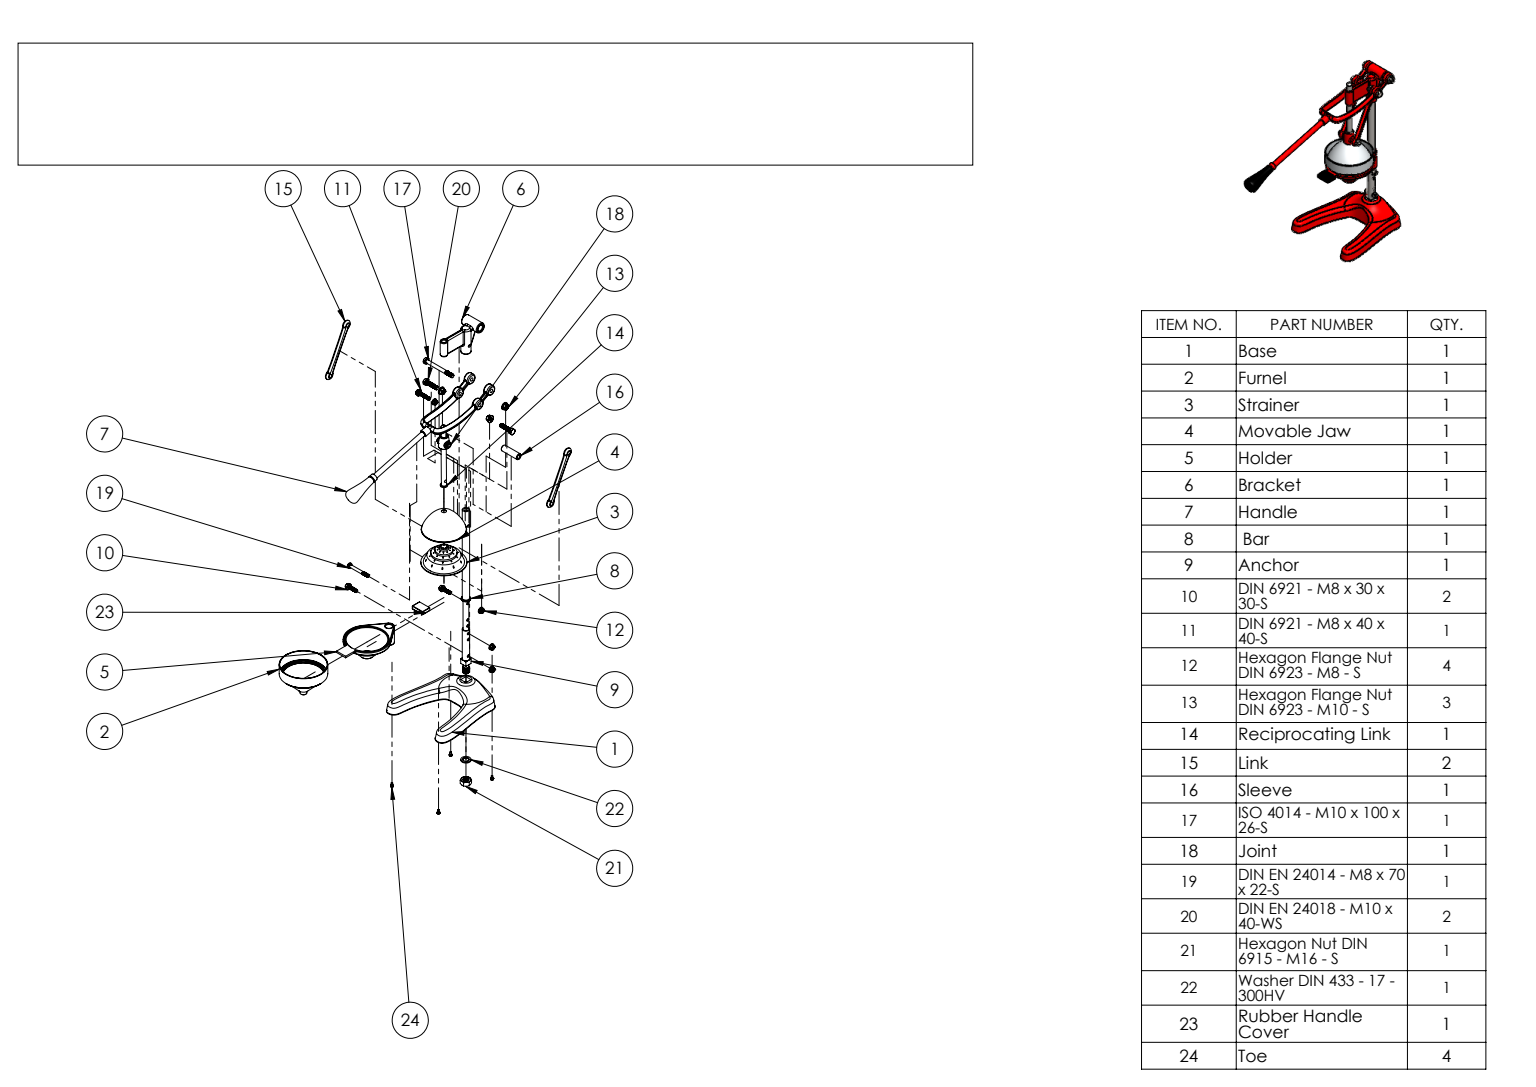
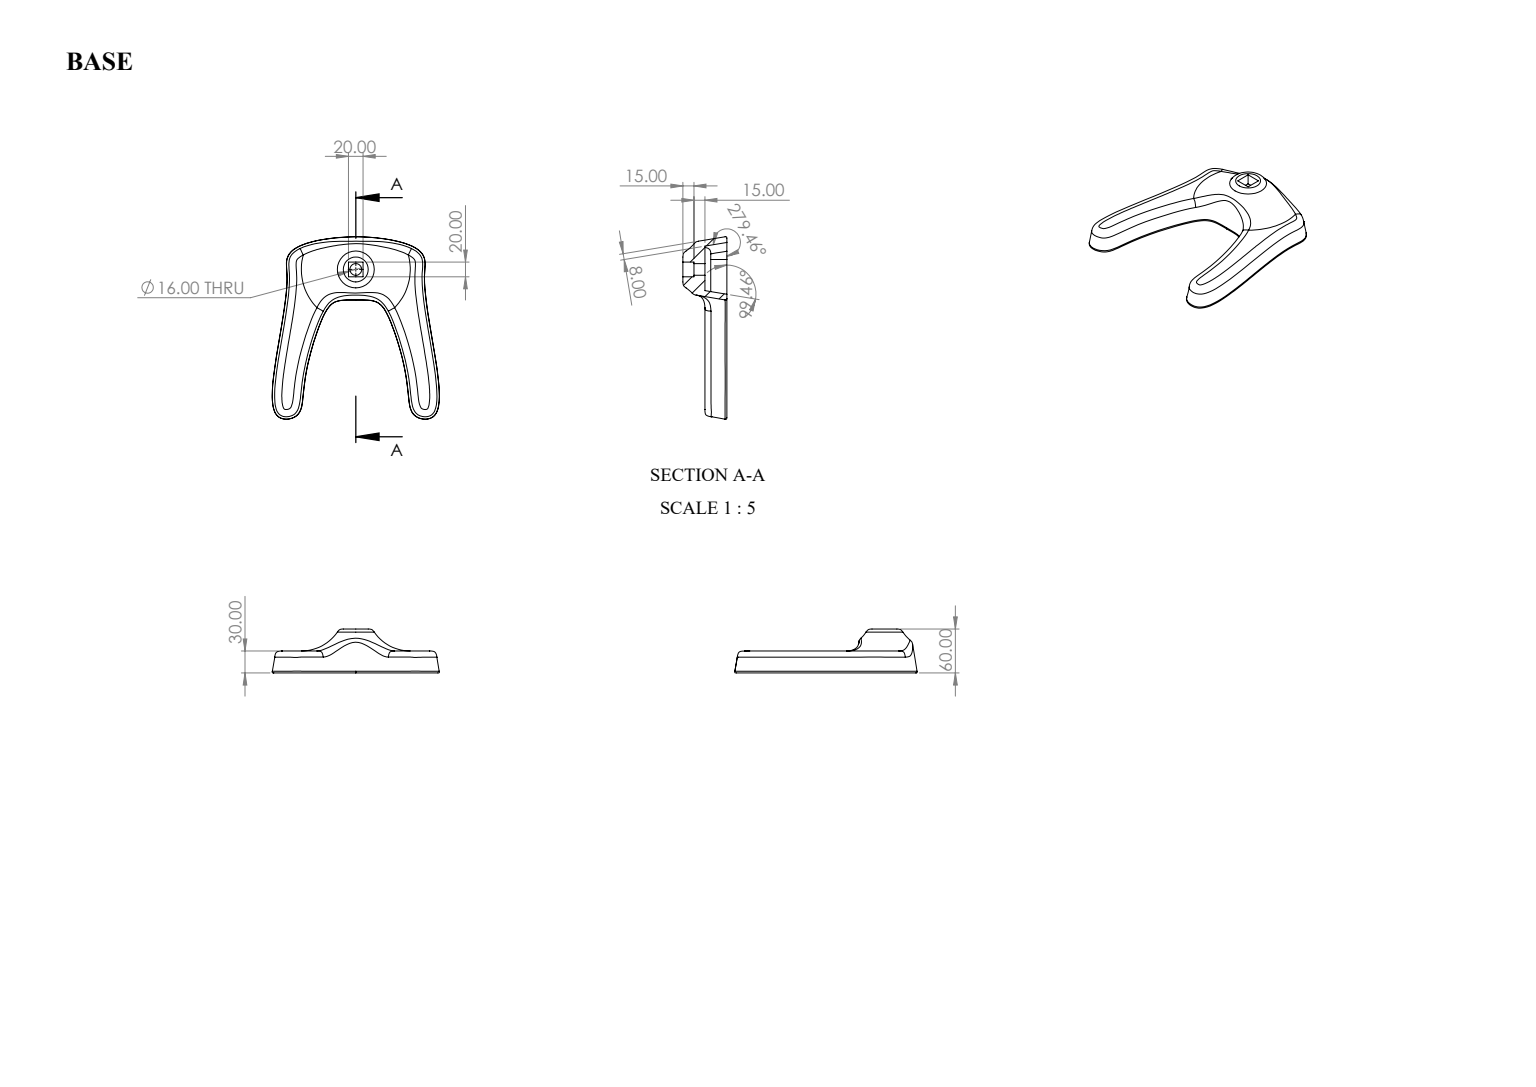
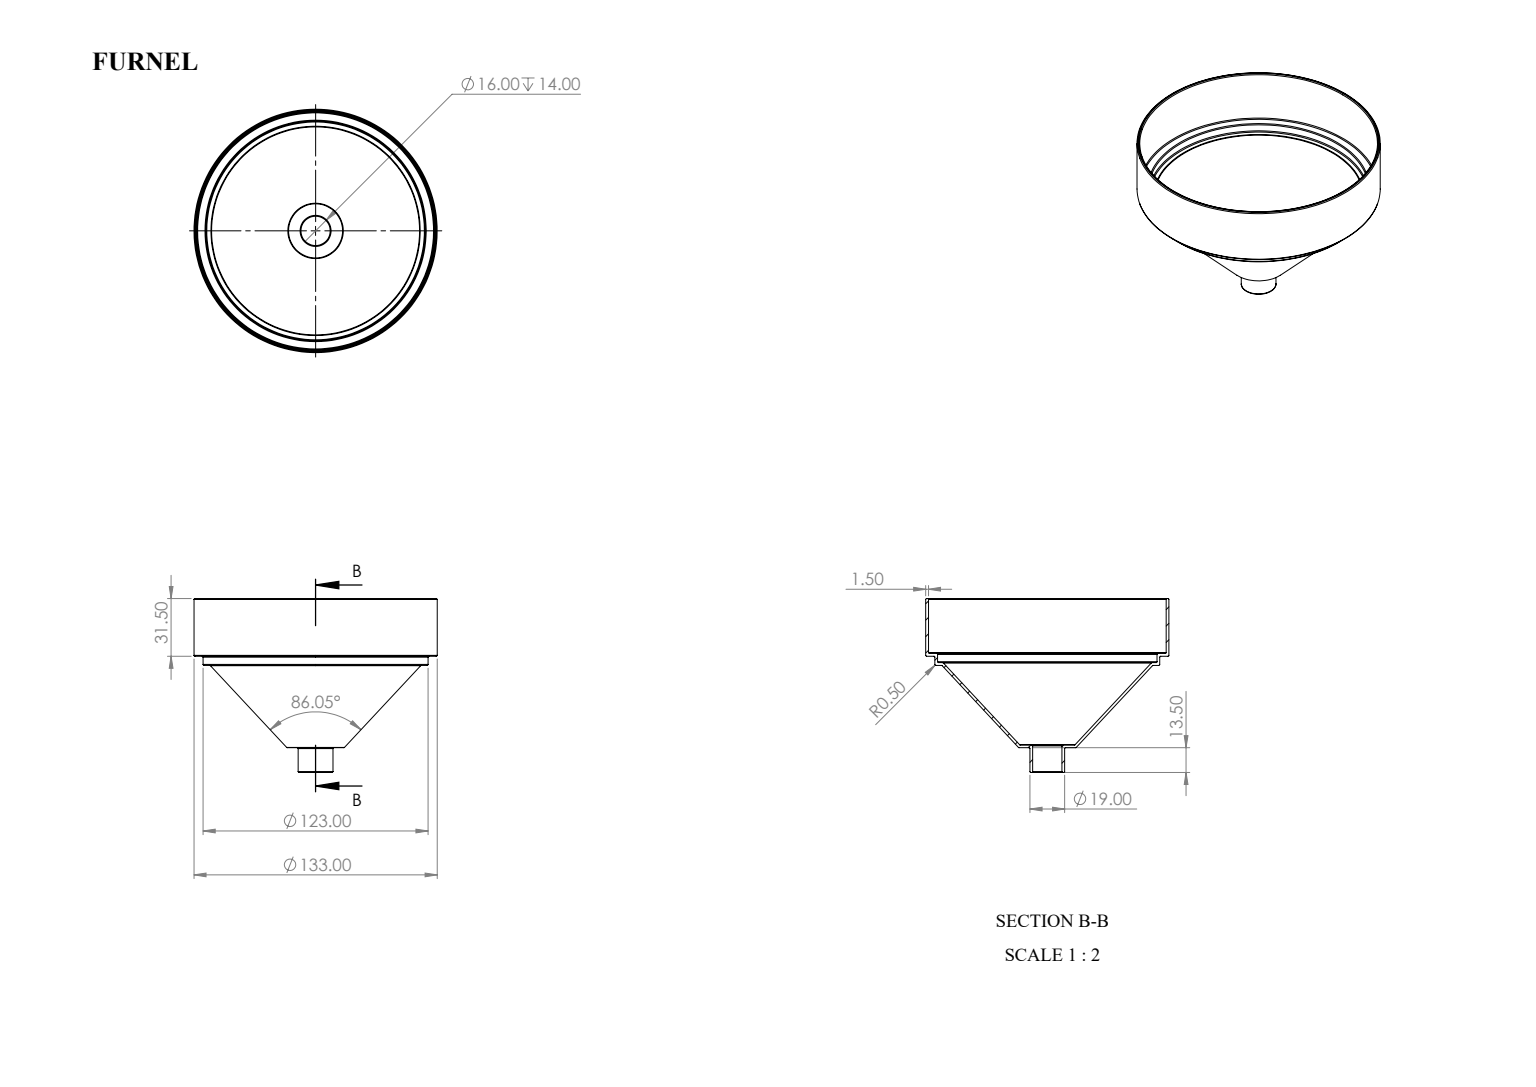
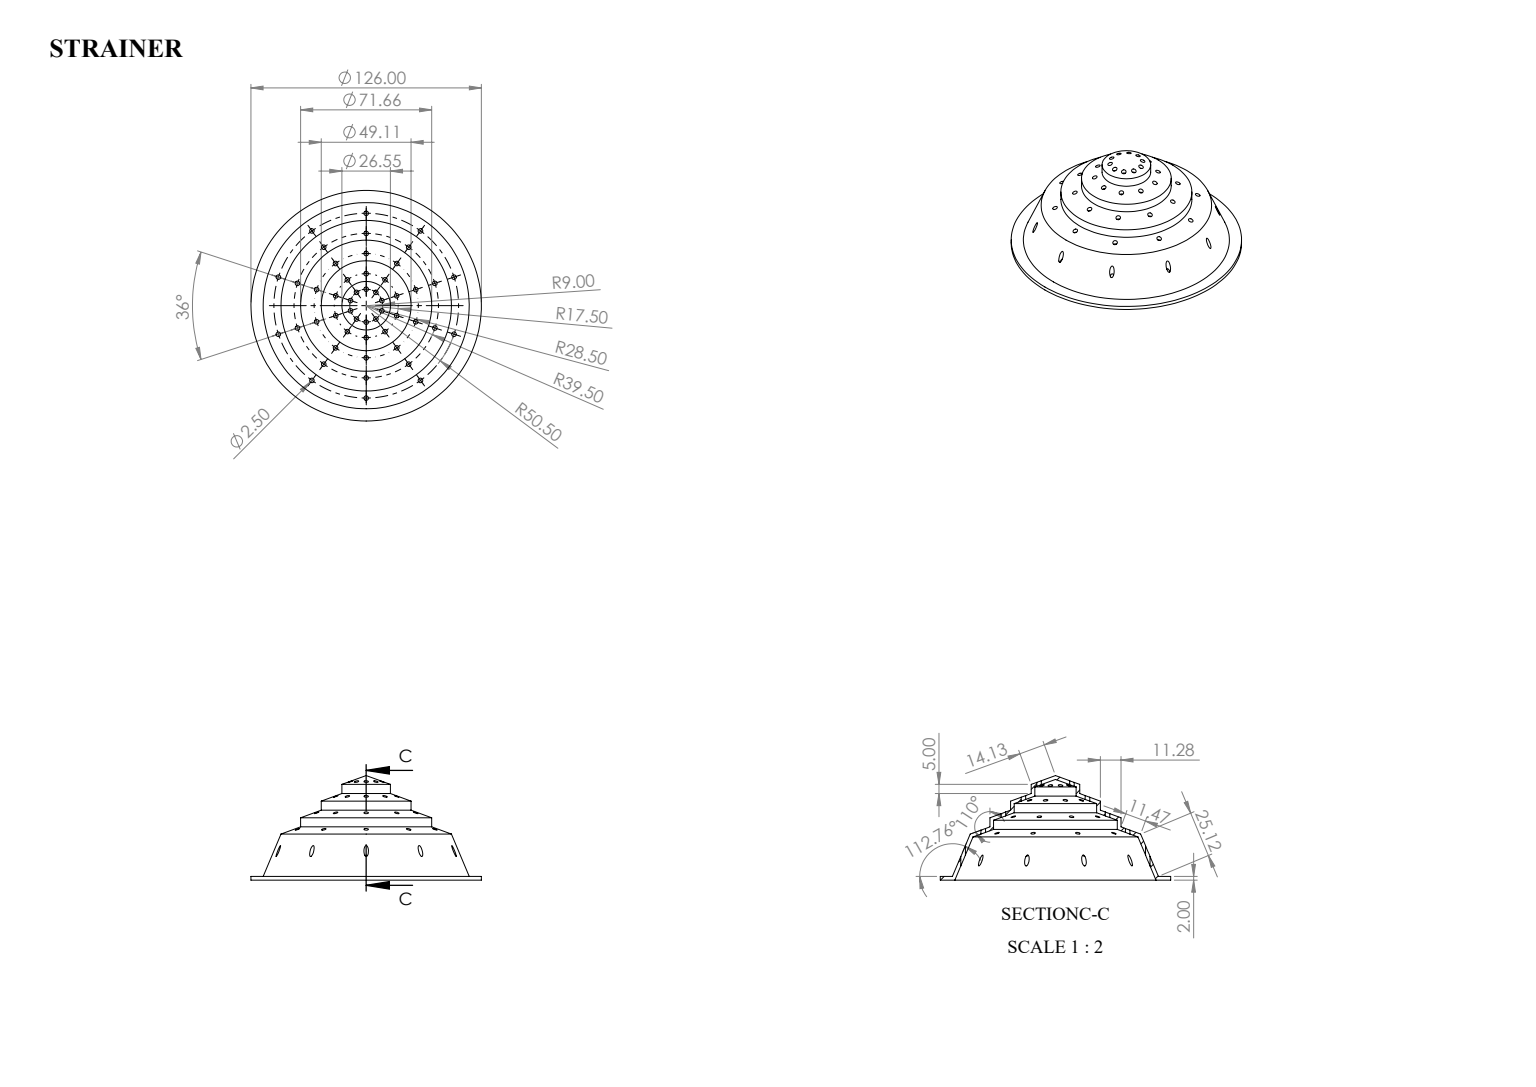
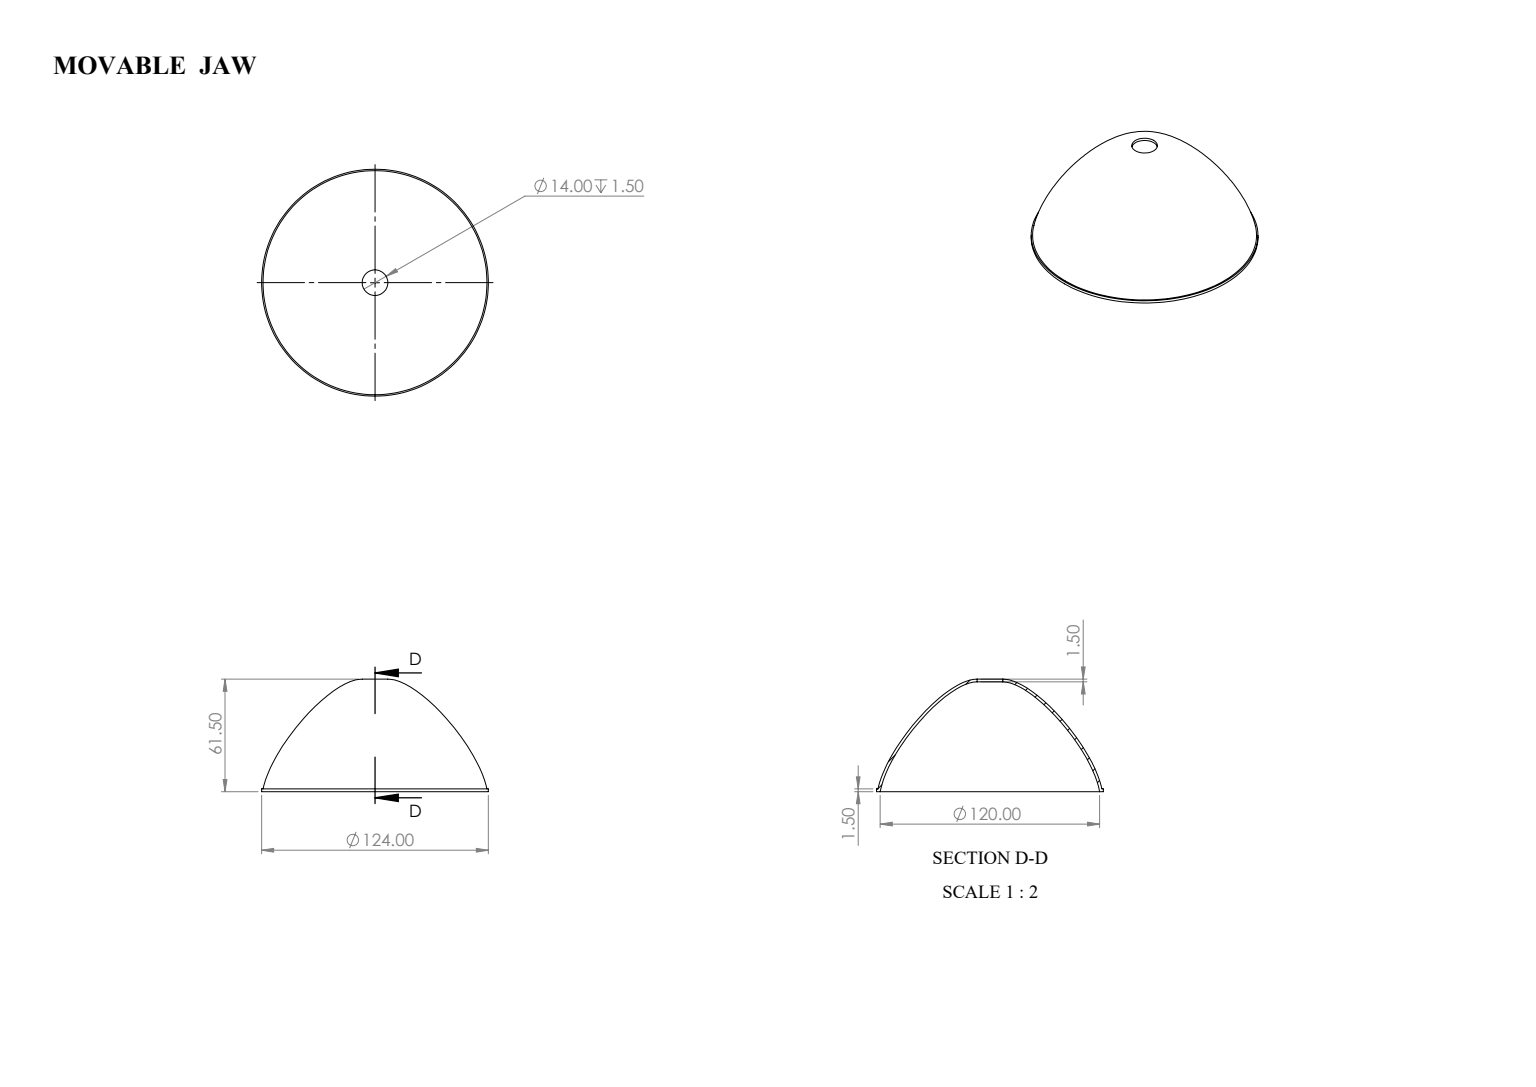
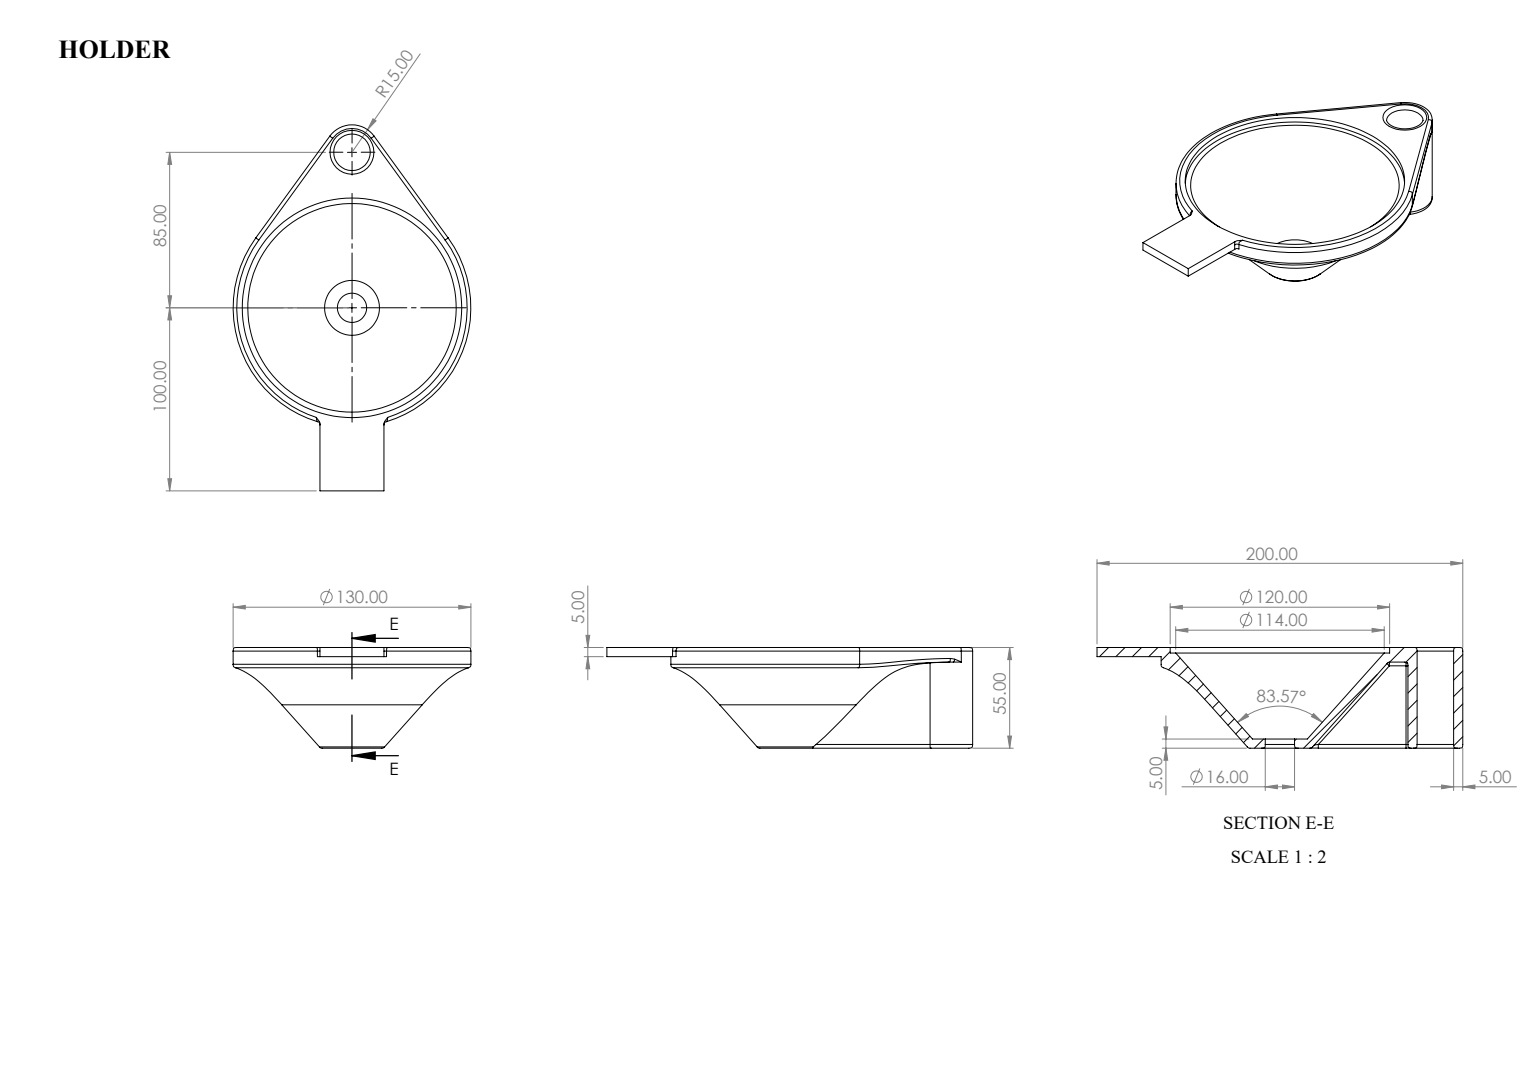
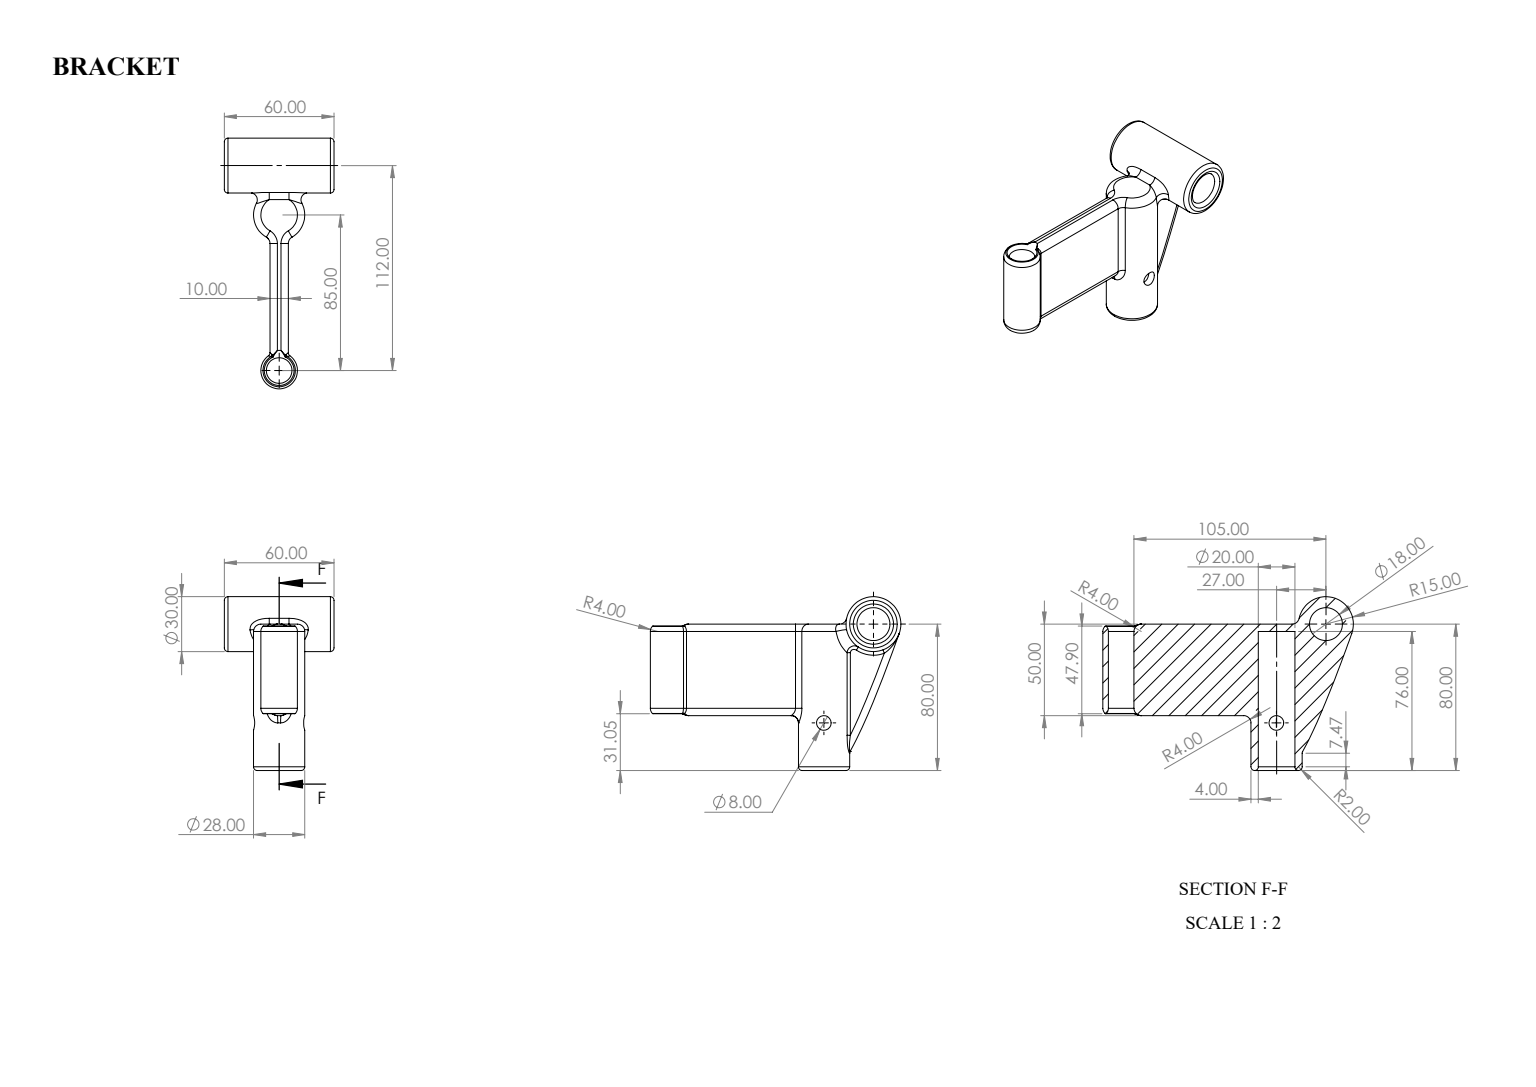
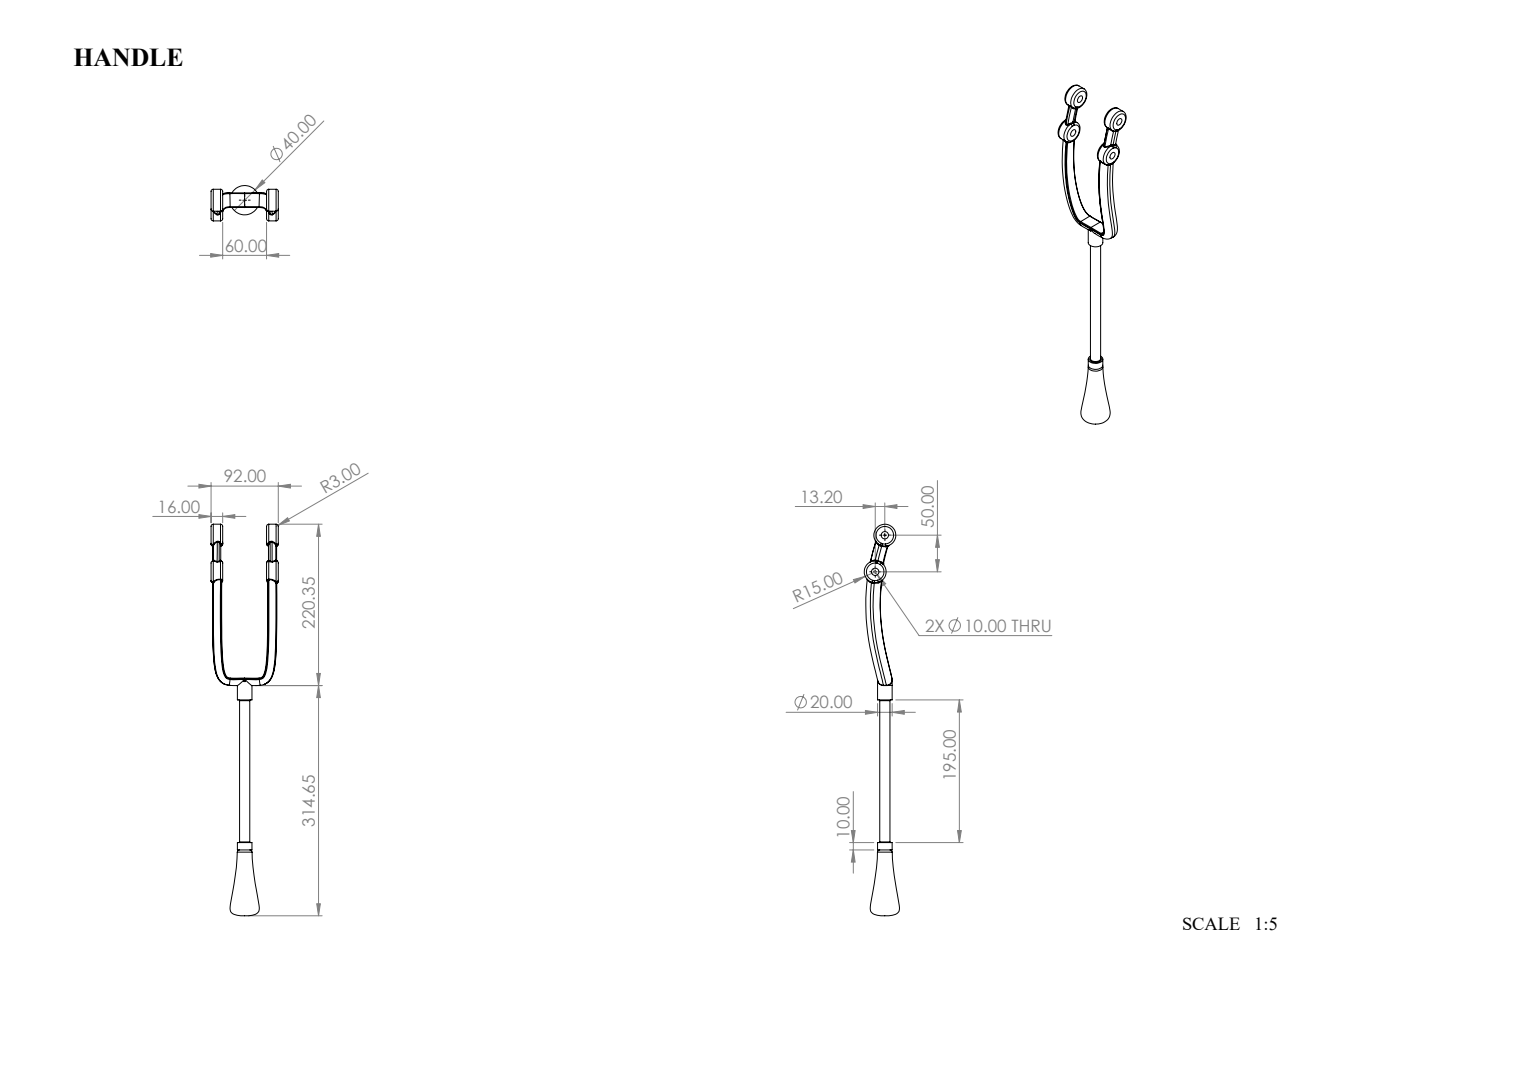
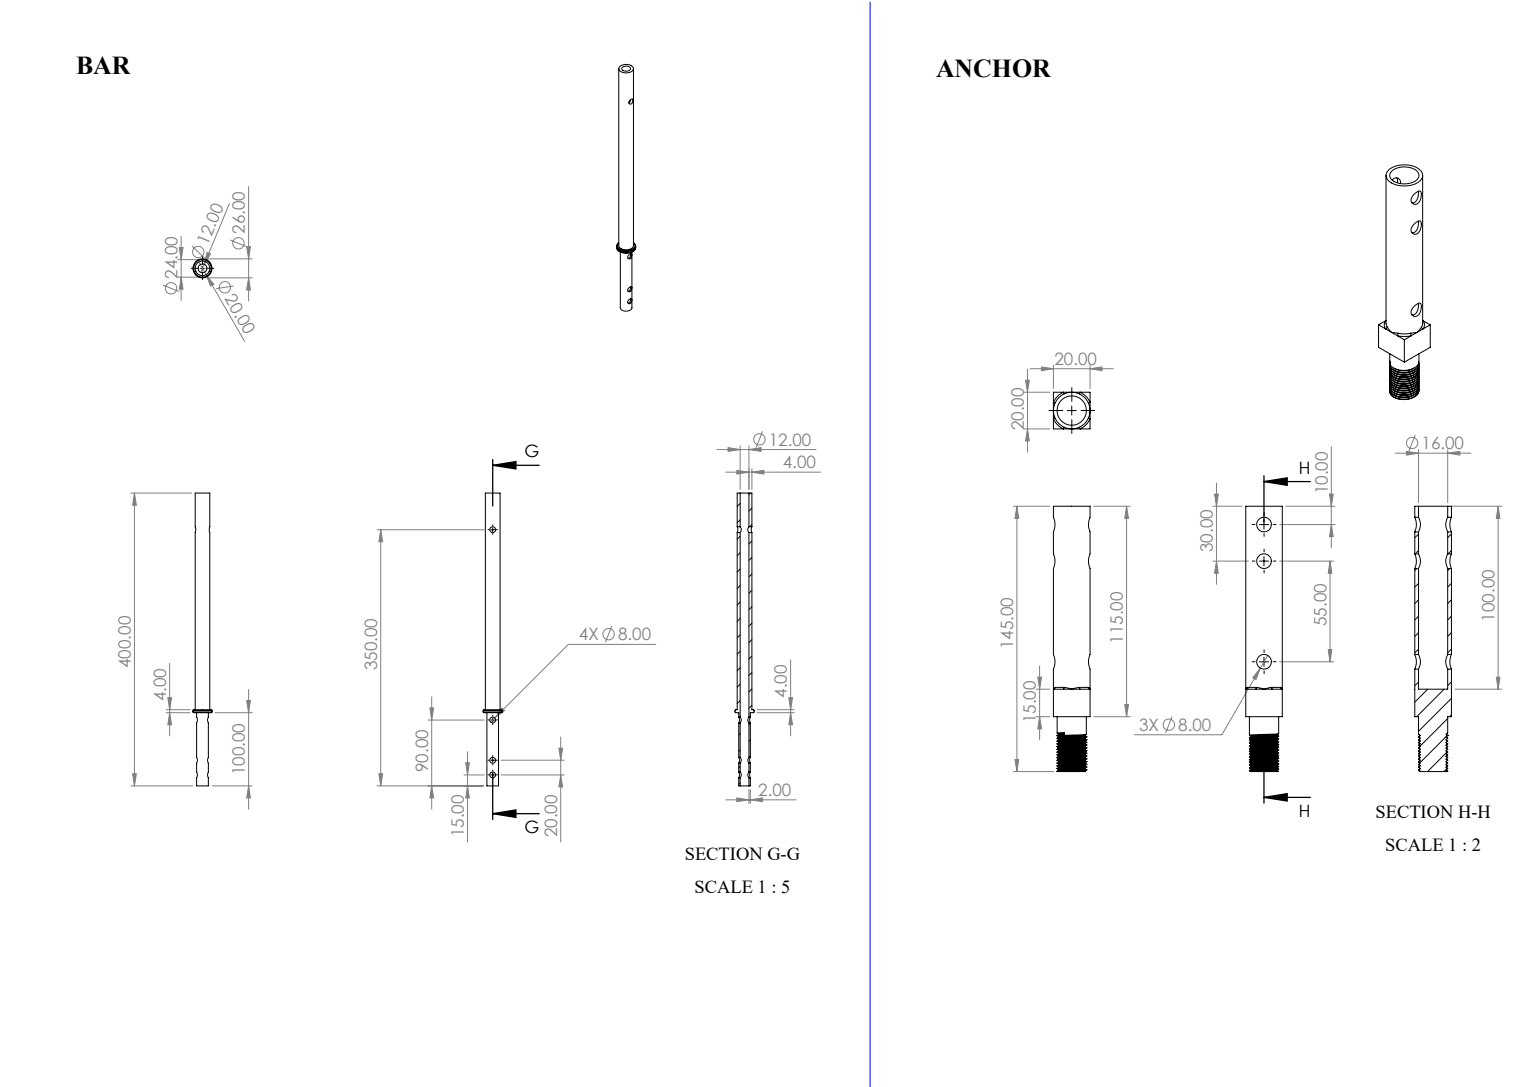
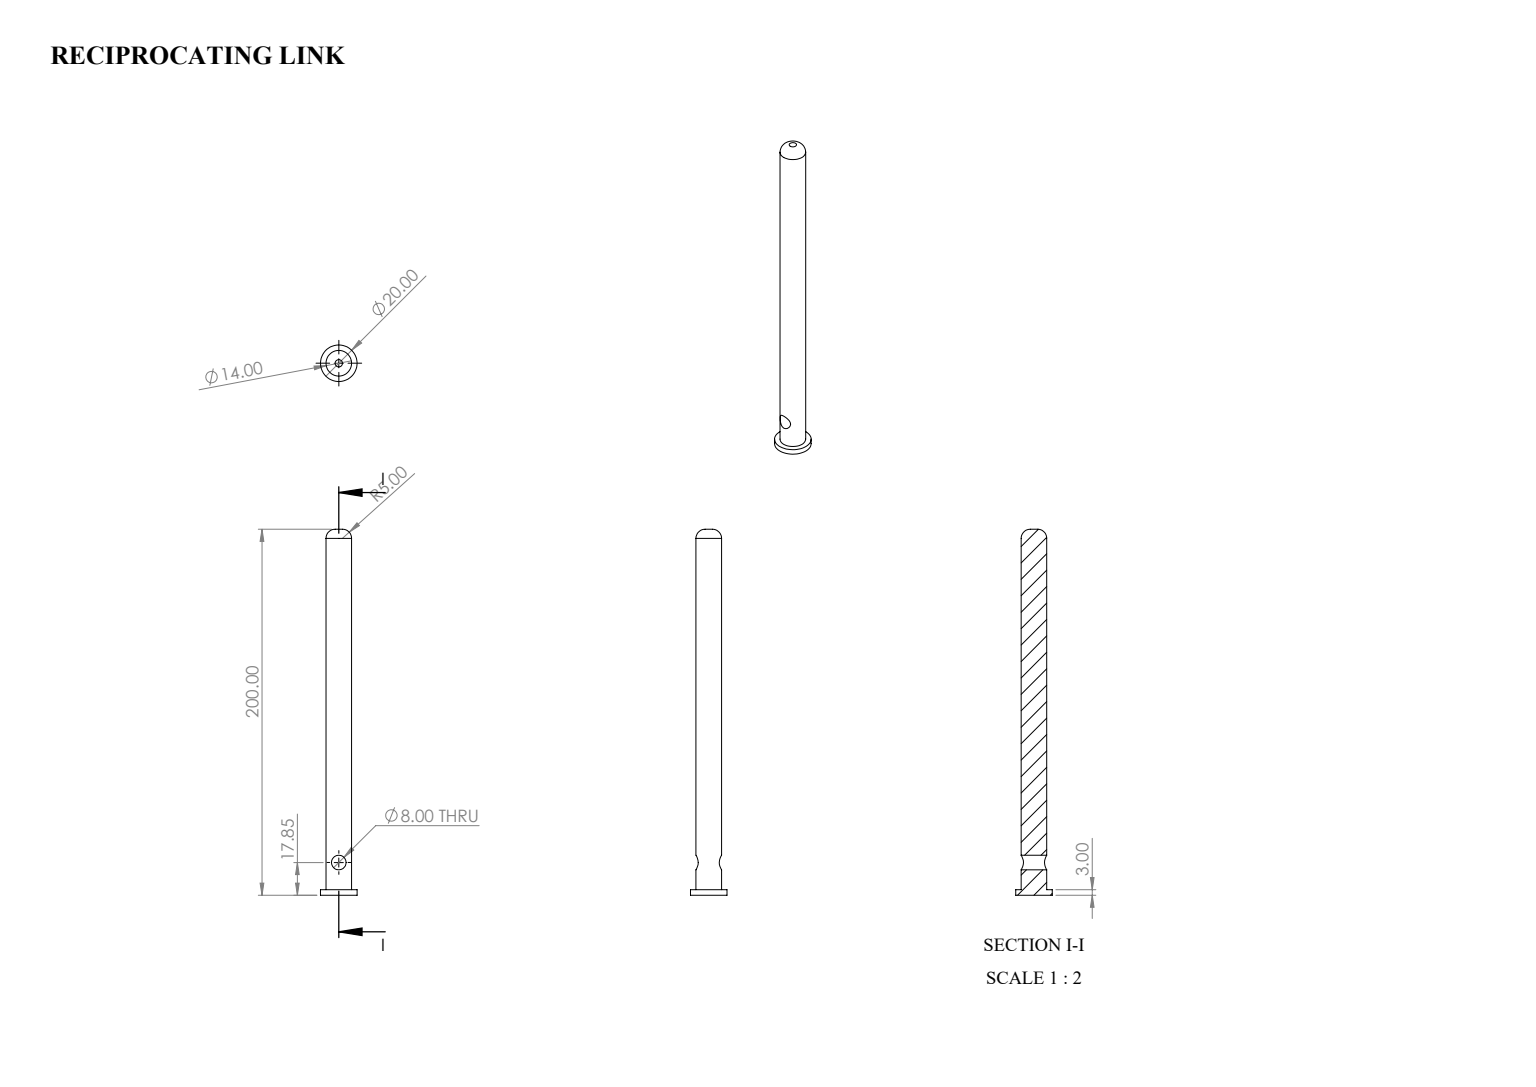
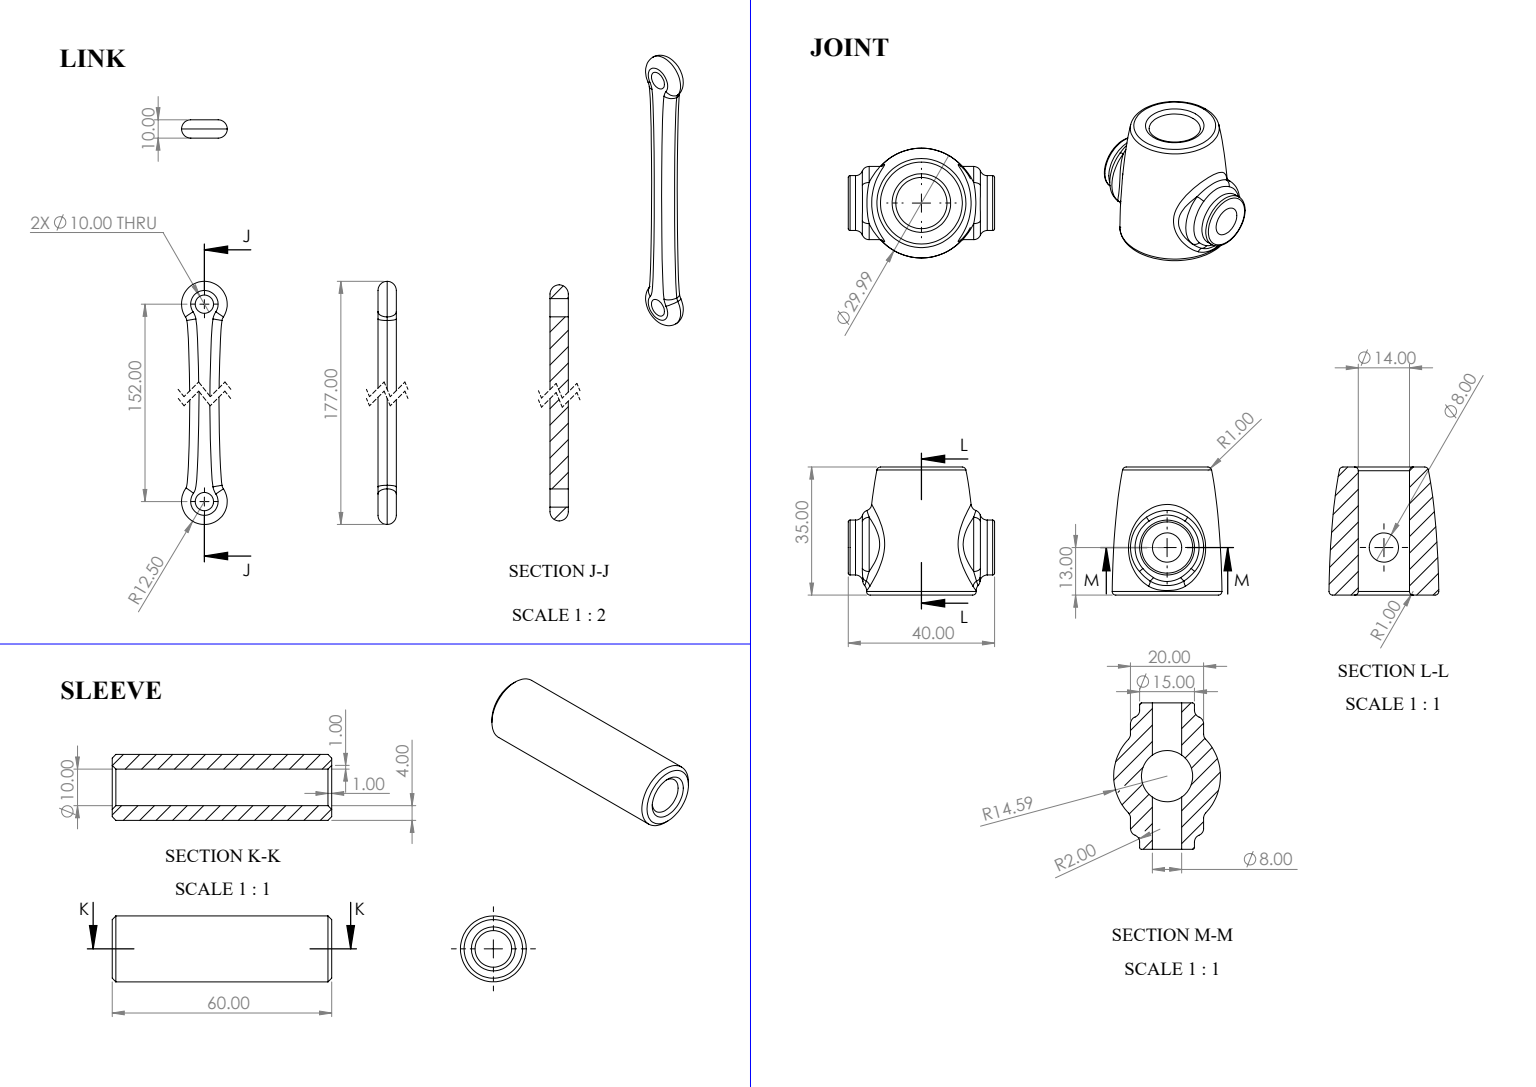
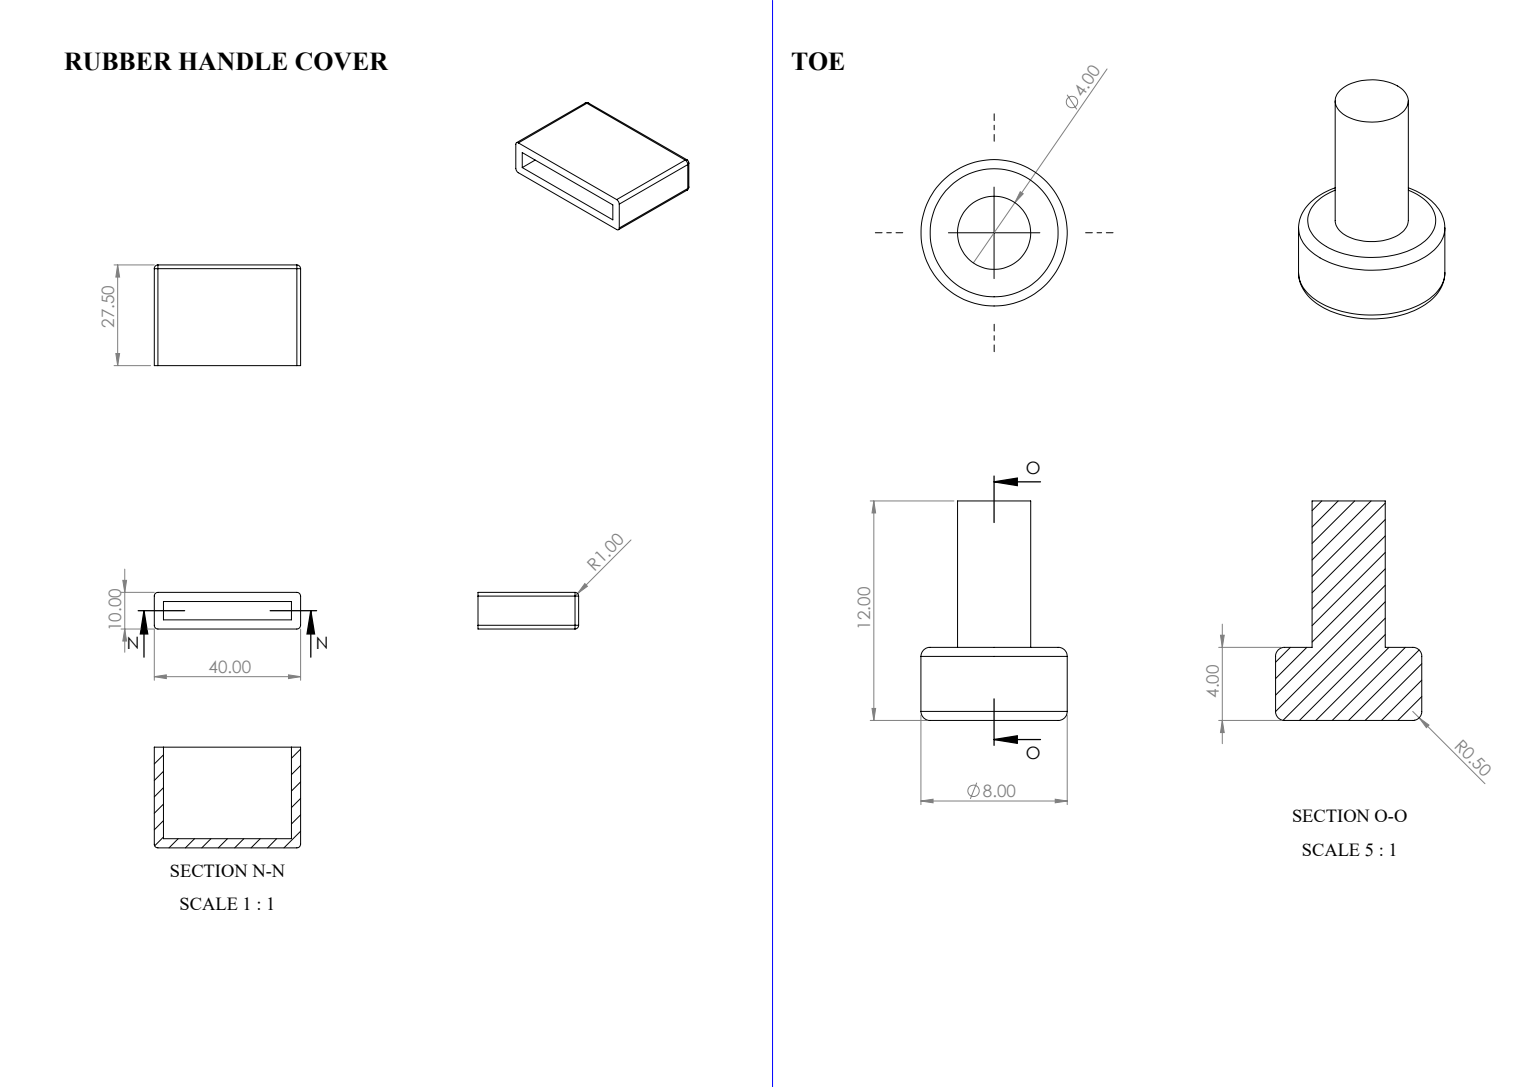
ISO-10303-21;
HEADER;
FILE_DESCRIPTION (('STEP AP214'),
    '1' );
FILE_NAME ('MAS-677',
    '2026-10-09T14:04:53',
    ( '' ),
    ( '' ),
    'SwSTEP 2.0',
    'SolidWorks 2021',
    '' );
FILE_SCHEMA (( 'AUTOMOTIVE_DESIGN' ));
ENDSEC;

DATA;
#1 = VERTEX_POINT ( 'NONE', #17992 ) ;
#2 = B_SPLINE_CURVE_WITH_KNOTS ( 'NONE', 3,
 ( #85581, #66854, #35995, #58769, #77476, #471, #16702, #68867, #91667, #3588, #33983, #17781, #27909, #60775, #99743, #44042, #16163, #93663, #90059, #52119 ),
 .UNSPECIFIED., .F., .F.,
 ( 4, 2, 2, 2, 2, 2, 2, 2, 2, 4 ),
 ( 0.007078851032209184692, 0.007582385810731511952, 0.008085920589253840080, 0.008337687978515005011, 0.008589455367776168207, 0.009092990146298498069, 0.009596524924820827931, 0.01010005970334315779, 0.01060359448186548766, 0.01110712926038781752 ),
 .UNSPECIFIED. ) ;
#3 = FACE_OUTER_BOUND ( 'NONE', #81469, .T. ) ;
#4 = CARTESIAN_POINT ( 'NONE',  ( -5.124871413311637092, 52.11721697291532251, 6.039328222380278888 ) ) ;
#5 = ORIENTED_EDGE ( 'NONE', *, *, #56749, .T. ) ;
#6 = DIRECTION ( 'NONE',  ( -1.000000000000000000, 0.000000000000000000, 0.000000000000000000 ) ) ;
#7 = CARTESIAN_POINT ( 'NONE',  ( -27.61887443722037716, 41.31835651977961987, -69.45683157427789922 ) ) ;
#8 = B_SPLINE_CURVE_WITH_KNOTS ( 'NONE', 3,
 ( #50184, #49649, #7583, #83088, #90116, #41565, #65840, #73380, #17841, #66367, #58829, #99249, #42622, #9178, #75522, #16219, #8125, #82557, #34041, #42089, #34577, #90651, #50690, #83607, #1616, #67451, #23829, #56671, #48578, #41038, #106277, #32440, #98201, #49106, #57729, #82005 ),
 .UNSPECIFIED., .F., .F.,
 ( 4, 2, 2, 2, 2, 2, 2, 2, 2, 2, 2, 2, 2, 2, 2, 2, 2, 4 ),
 ( 0.000000000000000000, 0.0008074604767267243646, 0.001614920953453448729, 0.002422381430180173094, 0.003229841906906897459, 0.004037302383633621823, 0.004844762860360346188, 0.005652223337087070552, 0.006459683813813794917, 0.007267144290540519282, 0.008074604767267243646, 0.008882065243993968878, 0.009689525720720692376, 0.01049698619744741587, 0.01130444667417414110, 0.01211190715090086634, 0.01251563738926422809, 0.01291936762762758983 ),
 .UNSPECIFIED. ) ;
#9 = CARTESIAN_POINT ( 'NONE',  ( -103.2512961873279238, -60.00000000000000711, 100.0497975478645145 ) ) ;
#10 = CARTESIAN_POINT ( 'NONE',  ( 28.43265695612079114, 17.35407036237645073, -40.99228818889015002 ) ) ;
#11 = CARTESIAN_POINT ( 'NONE',  ( 43.35354003336124151, 484.2707123563831715, -0.03226067987456286701 ) ) ;
#12 = DIRECTION ( 'NONE',  ( -1.000000000000000000, -0.000000000000000000, -0.000000000000000000 ) ) ;
#13 = CARTESIAN_POINT ( 'NONE',  ( -32.89862776688973867, 464.9311084009897854, 10.99515925127040283 ) ) ;
#15 = CARTESIAN_POINT ( 'NONE',  ( -6.817720317547426134, 41.26212449704699026, -58.42655649050038136 ) ) ;
#14 = CARTESIAN_POINT ( 'NONE',  ( -7.996668422911731078, -5.000000000000002665, -78.85453279917058467 ) ) ;
#16 = B_SPLINE_CURVE_WITH_KNOTS ( 'NONE', 3,
 ( #64877, #39563, #87576, #48148, #14717, #38505, #13662, #30413, #7160, #64366, #23384, #79992, #104270, #5579, #72952, #15794, #23929, #97239, #56222, #73482, #72438, #47616 ),
 .UNSPECIFIED., .F., .F.,
 ( 4, 2, 2, 2, 2, 2, 2, 2, 2, 2, 4 ),
 ( 0.007103997321553806935, 0.007607990259598500921, 0.008111983197643194907, 0.008363979666665547971, 0.008615976135687899301, 0.009119969073732612369, 0.009371965542754968903, 0.009623962011777323702, 0.01012795494982202810, 0.01063194788786673249, 0.01113594082591143689 ),
 .UNSPECIFIED. ) ;
#17 = CARTESIAN_POINT ( 'NONE',  ( -83.71287190118881938, -39.46305555311884916, 176.1778646026642150 ) ) ;
#18 = VERTEX_POINT ( 'NONE', #35795 ) ;
#19 = FILL_AREA_STYLE ('',( #15706 ) ) ;
#20 = VERTEX_POINT ( 'NONE', #83759 ) ;
#21 = EDGE_LOOP ( 'NONE', ( #101675, #98426, #15089, #46695 ) ) ;
#22 = CARTESIAN_POINT ( 'NONE',  ( 1.380949872273418154E-15, 45.89575828009193259, -11.27631144943088337 ) ) ;
#23 = CARTESIAN_POINT ( 'NONE',  ( 0.000000000000000000, 0.000000000000000000, -9.226681596905679683 ) ) ;
#24 = ORIENTED_EDGE ( 'NONE', *, *, #26895, .F. ) ;
#25 = VECTOR ( 'NONE', #75300, 1000.000000000000000 ) ;
#26 = CARTESIAN_POINT ( 'NONE',  ( -18.93093043102413375, 304.6959352974943158, 9.903868760122875869 ) ) ;
#27 = CARTESIAN_POINT ( 'NONE',  ( -39.15148982810983824, -57.67118160050520004, -41.75192649668374401 ) ) ;
#28 = CARTESIAN_POINT ( 'NONE',  ( 13.09999999999999787, 1.533819458162526451E-15, 0.000000000000000000 ) ) ;
#29 = CARTESIAN_POINT ( 'NONE',  ( -7.896254658894419798, -61.21070817245801976, 1.307282859663299268 ) ) ;
#30 = DIRECTION ( 'NONE',  ( 0.000000000000000000, 0.000000000000000000, 1.000000000000000000 ) ) ;
#31 = DIRECTION ( 'NONE',  ( 1.000000000000000000, 0.000000000000000000, 0.000000000000000000 ) ) ;
#32 = CARTESIAN_POINT ( 'NONE',  ( 106.8726675771063981, -14.21045842199433729, 167.8793401222494595 ) ) ;
#33 = EDGE_CURVE ( 'NONE', #89169, #22959, #61888, .T. ) ;
#34 = CARTESIAN_POINT ( 'NONE',  ( -114.2389886898993581, -60.00000000000000000, 181.3578213617837491 ) ) ;
#35 = CARTESIAN_POINT ( 'NONE',  ( -63.13573024357239660, -42.96249537661331885, 82.55452416654728154 ) ) ;
#36 = VERTEX_POINT ( 'NONE', #74603 ) ;
#37 = DIRECTION ( 'NONE',  ( -1.000000000000000000, -1.224606353822377258E-16, -0.000000000000000000 ) ) ;
#38 = CARTESIAN_POINT ( 'NONE',  ( 95.01673997733890076, -60.00000000000974865, -3.495082099215109928 ) ) ;
#39 = ORIENTED_EDGE ( 'NONE', *, *, #35413, .T. ) ;
#40 = CARTESIAN_POINT ( 'NONE',  ( 6.086195650940305374E-05, -60.35900081385168647, 33.94948342857766477 ) ) ;
#41 = CARTESIAN_POINT ( 'NONE',  ( 5.082755093536325930, -14.84375000204838457, -5.082755093536325042 ) ) ;
#42 =( LENGTH_UNIT ( ) NAMED_UNIT ( * ) SI_UNIT ( .MILLI., .METRE. ) );
#43 = VERTEX_POINT ( 'NONE', #19085 ) ;
#44 = CARTESIAN_POINT ( 'NONE',  ( 6.653282514704100592, -30.00000000000001066, 2.730950945157442966 ) ) ;
#45 = ORIENTED_EDGE ( 'NONE', *, *, #78057, .F. ) ;
#46 = CARTESIAN_POINT ( 'NONE',  ( -5.978033218201116661, -4.054134411712217556, -0.5602453477493335443 ) ) ;
#47 = CARTESIAN_POINT ( 'NONE',  ( -99.61197666665466954, -60.00000000000001421, 201.9966760002100159 ) ) ;
#48 = CARTESIAN_POINT ( 'NONE',  ( -1.320432766682874540E-15, -21.40625000204838457, 7.188101187500000044 ) ) ;
#49 =( GEOMETRIC_REPRESENTATION_CONTEXT ( 3 ) GLOBAL_UNCERTAINTY_ASSIGNED_CONTEXT ( ( #34894 ) ) GLOBAL_UNIT_ASSIGNED_CONTEXT ( ( #91410, #78925, #30403 ) ) REPRESENTATION_CONTEXT ( 'NONE', 'WORKASPACE' ) );
#50 = CARTESIAN_POINT ( 'NONE',  ( 44.26460937848495547, 463.8319445086722794, 7.881633536479285773 ) ) ;
#51 = CARTESIAN_POINT ( 'NONE',  ( 33.77559172535807619, 464.7834715296606305, 7.192701217093271815 ) ) ;
#52 =( BOUNDED_SURFACE ( )  B_SPLINE_SURFACE ( 3, 2, ( 
 ( #98850, #99925, #16904 ),
 ( #82687, #25559, #17442 ),
 ( #26100, #18510, #24494 ),
 ( #49783, #92359, #8792 ) ),
 .UNSPECIFIED., .F., .F., .F. ) 
 B_SPLINE_SURFACE_WITH_KNOTS ( ( 4, 4 ),
 ( 3, 3 ),
 ( -1.734723475976807094E-18, 0.001998086366838127629 ),
 ( 0.000000000000000000, 1.000000000000000000 ),
 .UNSPECIFIED. ) 
 GEOMETRIC_REPRESENTATION_ITEM ( )  RATIONAL_B_SPLINE_SURFACE ( (
 ( 1.000000000000000000, 0.7996726260853292967, 1.000000000000000000),
 ( 1.000000000000000000, 0.8085378326699110829, 1.000000000000000000),
 ( 1.000000000000000000, 0.8176579674344260917, 1.000000000000000000),
 ( 1.000000000000000000, 0.8258027051676627428, 1.000000000000000000) ) ) 
 REPRESENTATION_ITEM ( '' )  SURFACE ( )  );
#53 = CARTESIAN_POINT ( 'NONE',  ( -11.45206486516558009, 14.70585775886807056, 9.862607668232977076 ) ) ;
#54 = CARTESIAN_POINT ( 'NONE',  ( 1.000000000000000000, -32.16482459199326627, -4.060956965557648957 ) ) ;
#55 = AXIS2_PLACEMENT_3D ( 'NONE', #91909, #202, #25075 ) ;
#56 = CARTESIAN_POINT ( 'NONE',  ( 5.290067270632322405, 53.47475093287481940, 8.531152949374478212 ) ) ;
#57 = CARTESIAN_POINT ( 'NONE',  ( 12.30686711561308577, -4.727852861241523819, 20.32466816526829234 ) ) ;
#58 = CARTESIAN_POINT ( 'NONE',  ( -23.84378987347019674, 27.93349636785021772, 30.86234801138808947 ) ) ;
#59 = CARTESIAN_POINT ( 'NONE',  ( 0.000000000000000000, 0.000000000000000000, 8.000000000000000000 ) ) ;
#60 = CARTESIAN_POINT ( 'NONE',  ( -31.41997332126805631, -18.66943872641200741, 29.82631662943089523 ) ) ;
#61 = AXIS2_PLACEMENT_3D ( 'NONE', #48576, #41034, #67447 ) ;
#62 = CARTESIAN_POINT ( 'NONE',  ( -2.120783755322036335, -49.78473794080423431, 102.5525762030298722 ) ) ;
#63 = CARTESIAN_POINT ( 'NONE',  ( 39.22965285208312736, -18.76749908013844248, 33.52532150400537603 ) ) ;
#64 = DIRECTION ( 'NONE',  ( -1.000000000000000000, -1.224606353822377258E-16, -0.000000000000000000 ) ) ;
#65 = EDGE_LOOP ( 'NONE', ( #73939, #52655, #97069, #25713 ) ) ;
#66 = CARTESIAN_POINT ( 'NONE',  ( -7.934883677559675164, 88.86839177937550005, 1.051380792122690311 ) ) ;
#67 = EDGE_CURVE ( 'NONE', #4657, #43097, #41719, .T. ) ;
#68 = VECTOR ( 'NONE', #490, 1000.000000000000000 ) ;
#69 = CARTESIAN_POINT ( 'NONE',  ( -79.89526249746191411, -38.77347676181469183, 192.8024975868495687 ) ) ;
#70 = EDGE_LOOP ( 'NONE', ( #14398, #103627, #81786, #35183, #67385, #53899 ) ) ;
#72 = CARTESIAN_POINT ( 'NONE',  ( -42.64669454907780732, 435.7301117833579838, 8.366116403065163354 ) ) ;
#71 = DIRECTION ( 'NONE',  ( 0.000000000000000000, 1.000000000000000000, 0.000000000000000000 ) ) ;
#73 = CARTESIAN_POINT ( 'NONE',  ( -10.88549210619159346, 9.040369729539051491, -10.02153587380511190 ) ) ;
#74 = CARTESIAN_POINT ( 'NONE',  ( -49.27082696441096488, 7.795205586015203636, -15.75806003941715083 ) ) ;
#75 = CARTESIAN_POINT ( 'NONE',  ( -6.784953749642196108, 41.67963440881483450, -59.00226708758491156 ) ) ;
#76 = CARTESIAN_POINT ( 'NONE',  ( 6.804948497510390659, 41.03925918793141392, -70.91872537021917822 ) ) ;
#78 = B_SPLINE_CURVE_WITH_KNOTS ( 'NONE', 3,
 ( #67643, #99991, #99446, #58484, #91388, #59018, #76777, #77852, #37962, #2880 ),
 .UNSPECIFIED., .F., .F.,
 ( 4, 2, 2, 2, 4 ),
 ( 0.000000000000000000, 0.002305503304226490333, 0.004611006608452981534, 0.006916509912679472301, 0.009222013216905964803 ),
 .UNSPECIFIED. ) ;
#77 = CARTESIAN_POINT ( 'NONE',  ( 9.250997389131581983, 1.340359594676612611E-15, 0.000000000000000000 ) ) ;
#79 = CARTESIAN_POINT ( 'NONE',  ( 4.595881407952572495, -86.06625433201324427, -3.857520671226066789 ) ) ;
#80 = CARTESIAN_POINT ( 'NONE',  ( 60.14984002819952025, -1.232595164407830946E-29, 4.000000000000007105 ) ) ;
#81 = EDGE_CURVE ( 'NONE', #25883, #24620, #13982, .T. ) ;
#82 = CARTESIAN_POINT ( 'NONE',  ( 102.1624392737155205, -60.00000000000001421, 93.69283045337873261 ) ) ;
#83 = FACE_OUTER_BOUND ( 'NONE', #95892, .T. ) ;
#84 = CARTESIAN_POINT ( 'NONE',  ( -5.000000000000000000, 0.000000000000000000, -8.553285714285713937 ) ) ;
#85 = ORIENTED_EDGE ( 'NONE', *, *, #25518, .T. ) ;
#86 = B_SPLINE_CURVE_WITH_KNOTS ( 'NONE', 3,
 ( #103983, #94324, #70033, #102937, #94862, #53843 ),
 .UNSPECIFIED., .F., .F.,
 ( 4, 2, 4 ),
 ( 2.475503369200647279E-07, 0.002222330217055633675, 0.004444412883774348857 ),
 .UNSPECIFIED. ) ;
#87 = CARTESIAN_POINT ( 'NONE',  ( -97.97749490832038077, -30.00000000000004619, 190.5538380573200925 ) ) ;
#88 = ORIENTED_EDGE ( 'NONE', *, *, #84349, .T. ) ;
#89 = DIRECTION ( 'NONE',  ( 0.000000000000000000, 1.000000000000000000, 0.000000000000000000 ) ) ;
#90 = CARTESIAN_POINT ( 'NONE',  ( -43.00000000000000000, 450.0000000000002274, 13.20242257375370976 ) ) ;
#91 = CARTESIAN_POINT ( 'NONE',  ( 9.439578326262994423, 141.9252321839387037, 5.000000000000000000 ) ) ;
#92 = DIRECTION ( 'NONE',  ( 0.000000000000000000, -1.000000000000000000, 0.000000000000000000 ) ) ;
#93 = CARTESIAN_POINT ( 'NONE',  ( -22.66566284726399516, 27.53292244466712546, -33.08065323819745629 ) ) ;
#94 = CARTESIAN_POINT ( 'NONE',  ( -1.320432766682874540E-15, -24.40625000204838813, 7.188101187500000044 ) ) ;
#95 = AXIS2_PLACEMENT_3D ( 'NONE', #87472, #13552, #46470 ) ;
#96 = CARTESIAN_POINT ( 'NONE',  ( 7.084743714275938409, 40.92373723548720221, -70.77066346801599650 ) ) ;
#97 = ORIENTED_EDGE ( 'NONE', *, *, #94758, .T. ) ;
#98 = TOROIDAL_SURFACE ( 'NONE', #91385, 12.00000000000001066, 3.000000000000000000 ) ;
#99 = PRODUCT_RELATED_PRODUCT_CATEGORY ( 'part', '', ( #69145 ) ) ;
#101 = VERTEX_POINT ( 'NONE', #42239 ) ;
#100 = DIRECTION ( 'NONE',  ( 0.000000000000000000, -1.000000000000000000, 0.000000000000000000 ) ) ;
#102 = CARTESIAN_POINT ( 'NONE',  ( 79.44807355516962843, -49.90302049612382973, 154.1158519667677069 ) ) ;
#103 = CARTESIAN_POINT ( 'NONE',  ( -55.63518754872630012, 38.95383793071890466, 32.06611684419585373 ) ) ;
#104 =( LENGTH_UNIT ( ) NAMED_UNIT ( * ) SI_UNIT ( .MILLI., .METRE. ) );
#105 = ORIENTED_EDGE ( 'NONE', *, *, #85457, .F. ) ;
#106 = CARTESIAN_POINT ( 'NONE',  ( 2.607260012660386551E-19, 12.91535575337012354, -51.75000000000000711 ) ) ;
#107 = CARTESIAN_POINT ( 'NONE',  ( -7.188101187500002709, -10.81250000204838457, 2.977408999572647819 ) ) ;
#108 = CARTESIAN_POINT ( 'NONE',  ( 7.344505440741524005, 27.55381072701297285, -3.175463080953007999 ) ) ;
#109 = CARTESIAN_POINT ( 'NONE',  ( -49.97608103696126136, -60.00000000000002132, -32.05360424975566502 ) ) ;
#110 = CARTESIAN_POINT ( 'NONE',  ( 11.27248856952046729, 45.76231435389448876, 13.37350896801524058 ) ) ;
#111 = FILL_AREA_STYLE_COLOUR ( '', #88260 ) ;
#112 = VERTEX_POINT ( 'NONE', #1772 ) ;
#113 = AXIS2_PLACEMENT_3D ( 'NONE', #85690, #35566, #67375 ) ;
#114 =( LENGTH_UNIT ( ) NAMED_UNIT ( * ) SI_UNIT ( .MILLI., .METRE. ) );
#115 = CIRCLE ( 'NONE', #15617, 7.500000000001509015 ) ;
#116 = LINE ( 'NONE', #82122, #11300 ) ;
#117 = CARTESIAN_POINT ( 'NONE',  ( 7.341136360785455395, 41.28570779223741738, -59.23704358728311092 ) ) ;
#118 = CARTESIAN_POINT ( 'NONE',  ( 86.75557114459695640, -46.46500150678768648, 190.6000161368287138 ) ) ;
#119 = EDGE_CURVE ( 'NONE', #62895, #77549, #30853, .T. ) ;
#120 = CARTESIAN_POINT ( 'NONE',  ( 2.985641311035224431E-22, 35.08181111624585213, -27.25000000000000000 ) ) ;
#121 = CARTESIAN_POINT ( 'NONE',  ( -5.082755093536326818, -28.71875000204838813, 5.082755093536325042 ) ) ;
#122 = CARTESIAN_POINT ( 'NONE',  ( 28.31057169221128333, -31.30877727696230295, 39.66972444408808229 ) ) ;
#123 = CARTESIAN_POINT ( 'NONE',  ( -40.46354120900181073, 490.2757239658857884, 11.42275260667292791 ) ) ;
#124 = CARTESIAN_POINT ( 'NONE',  ( 4.284822031654965890, -1.092833614412281218, 104.4267991316945086 ) ) ;
#125 = CARTESIAN_POINT ( 'NONE',  ( 40.31016602574527496, 437.2133713289363754, 22.20736800721878978 ) ) ;
#126 = APPLICATION_PROTOCOL_DEFINITION ( 'draft international standard', 'automotive_design', 1998, #16230 ) ;
#127 = CARTESIAN_POINT ( 'NONE',  ( 48.59958381656775117, 10.21806572665720658, 14.48686862603841519 ) ) ;
#128 = ORIENTED_EDGE ( 'NONE', *, *, #62777, .F. ) ;
#129 = AXIS2_PLACEMENT_3D ( 'NONE', #36140, #18887, #77080 ) ;
#130 = CYLINDRICAL_SURFACE ( 'NONE', #47470, 15.00000000000000000 ) ;
#131 = EDGE_CURVE ( 'NONE', #70327, #36785, #1175, .T. ) ;
#132 = CARTESIAN_POINT ( 'NONE',  ( 16.14595037822613932, 12.99999999999999467, 8.749999999999944933 ) ) ;
#133 = AXIS2_PLACEMENT_3D ( 'NONE', #79588, #64998, #88226 ) ;
#134 = SURFACE_SIDE_STYLE ('',( #74048 ) ) ;
#135 = EDGE_CURVE ( 'NONE', #78511, #45219, #29192, .T. ) ;
#136 = PRESENTATION_STYLE_ASSIGNMENT (( #15825 ) ) ;
#137 = EDGE_LOOP ( 'NONE', ( #79684, #47625 ) ) ;
#138 = AXIS2_PLACEMENT_3D ( 'NONE', #88409, #103516, #29670 ) ;
#139 = CARTESIAN_POINT ( 'NONE',  ( -7.500000000000004441, -5.250000000000005329, -71.71180648257555390 ) ) ;
#140 = CARTESIAN_POINT ( 'NONE',  ( 107.5126338499654253, -57.67122577595705479, 113.4697314741770526 ) ) ;
#141 = COLOUR_RGB ( '', 0.09019608, 0.27058824, 0.51372549) ;
#142 = SURFACE_SIDE_STYLE ('',( #56810 ) ) ;
#143 = CARTESIAN_POINT ( 'NONE',  ( 0.5376128474930174095, 13.88012476438581544, 6.984229002090723171 ) ) ;
#144 = CARTESIAN_POINT ( 'NONE',  ( 6.999999999999995559, -46.00000000000000000, 39.12435565298213902 ) ) ;
#145 = CARTESIAN_POINT ( 'NONE',  ( 37.24841108779522614, 25.58895219176176283, 13.42546066398215210 ) ) ;
#146 = CARTESIAN_POINT ( 'NONE',  ( -77.21030068849461259, -59.99999999999998579, 191.0276050645643693 ) ) ;
#147 = CARTESIAN_POINT ( 'NONE',  ( -33.56345473223404241, 299.9083031499212666, -8.874823776838020706 ) ) ;
#148 =( LENGTH_UNIT ( ) NAMED_UNIT ( * ) SI_UNIT ( .MILLI., .METRE. ) );
#149 = CARTESIAN_POINT ( 'NONE',  ( -63.25915952246064222, 50.00000000000000000, 0.7870165385200997843 ) ) ;
#150 = CARTESIAN_POINT ( 'NONE',  ( -85.33812798373763542, -39.31465026836636412, 184.9304593203771105 ) ) ;
#151 = ORIENTED_EDGE ( 'NONE', *, *, #28634, .T. ) ;
#152 = CARTESIAN_POINT ( 'NONE',  ( 27.09085371571751466, 307.6936400730292576, -8.364846265266118408 ) ) ;
#153 = ORIENTED_EDGE ( 'NONE', *, *, #75458, .T. ) ;
#154 = CARTESIAN_POINT ( 'NONE',  ( 14.90155535905845952, 42.58002643001236720, -90.01374837836192455 ) ) ;
#155 = CARTESIAN_POINT ( 'NONE',  ( -5.308064226573042887, 41.67430808342687243, -70.56675994572434263 ) ) ;
#156 = CARTESIAN_POINT ( 'NONE',  ( -84.48871104503169249, -45.26950317026464177, -6.202404481629068655 ) ) ;
#157 = CIRCLE ( 'NONE', #101825, 3.309500000000001663 ) ;
#158 = CARTESIAN_POINT ( 'NONE',  ( 50.94745919686198476, 50.00000000000000000, -37.05882352941176094 ) ) ;
#159 = DIRECTION ( 'NONE',  ( 0.2276554125578255927, 0.04124382533949764312, 0.9728679047046888684 ) ) ;
#160 = VERTEX_POINT ( 'NONE', #69724 ) ;
#161 = AXIS2_PLACEMENT_3D ( 'NONE', #28600, #84677, #76566 ) ;
#162 = CARTESIAN_POINT ( 'NONE',  ( -32.70293721669443698, 464.5899875799652818, 16.75272535705724053 ) ) ;
#163 = CARTESIAN_POINT ( 'NONE',  ( 6.716227136310304324, 41.28548593599064986, -58.40644136812132103 ) ) ;
#164 = CARTESIAN_POINT ( 'NONE',  ( 13.60704923275002010, -1.734723475976807094E-15, -10.45706415777842935 ) ) ;
#165 = CARTESIAN_POINT ( 'NONE',  ( -34.47678062873980309, 437.1474145881088589, 5.468662283310430361 ) ) ;
#166 = EDGE_CURVE ( 'NONE', #36397, #86892, #67028, .T. ) ;
#167 = CARTESIAN_POINT ( 'NONE',  ( -49.63234380517151578, -59.99999999999993605, -40.41886796471348475 ) ) ;
#168 = CONICAL_SURFACE ( 'NONE', #3618, 4.172000000000001485, 0.9599310885968750373 ) ;
#169 = CARTESIAN_POINT ( 'NONE',  ( -79.92941718139617535, -25.61975873786342106, 131.8724341985731314 ) ) ;
#170 = VERTEX_POINT ( 'NONE', #86462 ) ;
#171 = CARTESIAN_POINT ( 'NONE',  ( 78.26152162121309175, -14.21045842199439946, 161.8191806974193696 ) ) ;
#172 = CARTESIAN_POINT ( 'NONE',  ( 84.15356149169568312, 5.000000000000023093, 6.123233995736781074E-16 ) ) ;
#173 = CARTESIAN_POINT ( 'NONE',  ( 99.06310009222487167, -57.67128884157320101, 63.13715724456057643 ) ) ;
#174 = ORIENTED_EDGE ( 'NONE', *, *, #30556, .F. ) ;
#175 = DIRECTION ( 'NONE',  ( -1.000000000000000000, -1.224606353822377258E-16, -0.000000000000000000 ) ) ;
#176 = CARTESIAN_POINT ( 'NONE',  ( -46.00000000000000000, 450.0000000000002274, 13.20242257375370976 ) ) ;
#177 = EDGE_LOOP ( 'NONE', ( #37832, #56366 ) ) ;
#178 = CARTESIAN_POINT ( 'NONE',  ( 2.022166183945757645, 14.39193082815908831, -6.705330260831378730 ) ) ;
#179 = SURFACE_STYLE_USAGE ( .BOTH. , #33144 ) ;
#180 = DIRECTION ( 'NONE',  ( 0.000000000000000000, 0.000000000000000000, 1.000000000000000000 ) ) ;
#181 = CARTESIAN_POINT ( 'NONE',  ( 7.188101187500000044, -19.15625000204838457, 0.000000000000000000 ) ) ;
#182 = CARTESIAN_POINT ( 'NONE',  ( 44.26720285007096578, 485.4142925135624296, 2.510465450173711144 ) ) ;
#183 = CARTESIAN_POINT ( 'NONE',  ( 9.333892298909262308, 83.21724268374964595, -3.590295303293451923 ) ) ;
#184 = CARTESIAN_POINT ( 'NONE',  ( 0.000000000000000000, 0.000000000000000000, 0.000000000000000000 ) ) ;
#185 = ADVANCED_FACE ( 'NONE', ( #78858 ), #30718, .T. ) ;
#186 = CARTESIAN_POINT ( 'NONE',  ( -7.500000000000000000, -3.948305025207548002, -7.349903712355482455 ) ) ;
#187 = CARTESIAN_POINT ( 'NONE',  ( -7.855360403618689702, 48.00000000000000711, -97.83275449052109707 ) ) ;
#188 = AXIS2_PLACEMENT_3D ( 'NONE', #4644, #61834, #45635 ) ;
#189 = B_SPLINE_CURVE_WITH_KNOTS ( 'NONE', 3,
 ( #47704, #5149, #104909, #71456, #31568, #72522, #105428, #62864, #30501, #97856 ),
 .UNSPECIFIED., .F., .F.,
 ( 4, 2, 2, 2, 4 ),
 ( 0.000000000000000000, 0.1250000000000000000, 0.2500000000000000000, 0.5000000000000000000, 1.000000000000000000 ),
 .UNSPECIFIED. ) ;
#190 = ORIENTED_EDGE ( 'NONE', *, *, #68395, .T. ) ;
#191 = CARTESIAN_POINT ( 'NONE',  ( -7.245482512374693762, 40.92674694571729788, -70.53853366045179030 ) ) ;
#193 = CARTESIAN_POINT ( 'NONE',  ( 30.74548990976421337, -46.43177832593983112, 34.64018936480751165 ) ) ;
#192 = CARTESIAN_POINT ( 'NONE',  ( -3.604576940039468269, -48.95215848635412215, 104.3731177596929314 ) ) ;
#194 = CARTESIAN_POINT ( 'NONE',  ( 35.45036406932566564, 436.3203772529585649, 5.179456583034234285 ) ) ;
#195 = ORIENTED_EDGE ( 'NONE', *, *, #39067, .F. ) ;
#196 = DIRECTION ( 'NONE',  ( 0.000000000000000000, 0.000000000000000000, 1.000000000000000000 ) ) ;
#197 = ORIENTED_EDGE ( 'NONE', *, *, #28937, .F. ) ;
#198 = CARTESIAN_POINT ( 'NONE',  ( 0.4988340113754564098, 3.871605243940360097, 7.999999999999996447 ) ) ;
#199 = CARTESIAN_POINT ( 'NONE',  ( 20.49977525862259142, 302.8459220885798686, -10.00124997875687427 ) ) ;
#200 = CARTESIAN_POINT ( 'NONE',  ( 37.40949999999997289, 0.000000000000000000, 0.000000000000000000 ) ) ;
#201 = CARTESIAN_POINT ( 'NONE',  ( 0.000000000000000000, 0.000000000000000000, -10.00000000000000000 ) ) ;
#202 = DIRECTION ( 'NONE',  ( -0.000000000000000000, -1.000000000000000000, -0.000000000000000000 ) ) ;
#203 = CARTESIAN_POINT ( 'NONE',  ( -37.22405814379114730, 463.3230035706858416, 20.09439497145941900 ) ) ;
#204 = ORIENTED_EDGE ( 'NONE', *, *, #17500, .T. ) ;
#205 = ADVANCED_FACE ( 'NONE', ( #45454 ), #41693, .T. ) ;
#206 = CARTESIAN_POINT ( 'NONE',  ( 92.56567127985995569, -60.00000000000000000, -10.67295280362520593 ) ) ;
#207 = CARTESIAN_POINT ( 'NONE',  ( -46.00000000000000000, 500.0000000000002274, 15.00000000000000711 ) ) ;
#208 = VECTOR ( 'NONE', #3737, 1000.000000000000000 ) ;
#209 = STYLED_ITEM ( 'NONE', ( #32664 ), #50486 ) ;
#210 = ADVANCED_FACE ( 'NONE', ( #73405 ), #48071, .F. ) ;
#211 = CARTESIAN_POINT ( 'NONE',  ( 48.02835407290503866, 11.61227450977245468, -14.35535821593549954 ) ) ;
#212 = ORIENTED_EDGE ( 'NONE', *, *, #24427, .T. ) ;
#213 = DIRECTION ( 'NONE',  ( 0.000000000000000000, 0.000000000000000000, -1.000000000000000000 ) ) ;
#214 = VERTEX_POINT ( 'NONE', #23851 ) ;
#215 = ORIENTED_EDGE ( 'NONE', *, *, #91369, .F. ) ;
#216 = CARTESIAN_POINT ( 'NONE',  ( 1.013561713383841045, 53.56087209037478658, 9.749829111538236504 ) ) ;
#217 = FACE_OUTER_BOUND ( 'NONE', #93796, .T. ) ;
#218 = CARTESIAN_POINT ( 'NONE',  ( 20.70154941269364812, 302.9148302143801175, 9.950696617737659011 ) ) ;
#219 = CARTESIAN_POINT ( 'NONE',  ( 84.37161269647305062, -45.28772981460180347, -2.916092811979204225 ) ) ;
#221 = MECHANICAL_DESIGN_GEOMETRIC_PRESENTATION_REPRESENTATION (  '', ( #3741 ), #8876 ) ;
#220 = CARTESIAN_POINT ( 'NONE',  ( -37.59043012194430844, 369.8415162678004435, 4.161255642873434191 ) ) ;
#222 = CARTESIAN_POINT ( 'NONE',  ( -3.833028914485100636, -68.60312449208545615, 13.52676978846691469 ) ) ;
#223 = CARTESIAN_POINT ( 'NONE',  ( 12.50000000000000178, 35.75035848856805387, -55.58311287890759189 ) ) ;
#224 = EDGE_LOOP ( 'NONE', ( #40162, #29975, #24462, #52322, #2837 ) ) ;
#225 = CARTESIAN_POINT ( 'NONE',  ( -9.957476778176042487, 44.05467513874048535, 12.94893335343420482 ) ) ;
#226 = AXIS2_PLACEMENT_3D ( 'NONE', #49892, #10498, #83857 ) ;
#227 = ORIENTED_EDGE ( 'NONE', *, *, #17235, .T. ) ;
#228 = DIRECTION ( 'NONE',  ( 0.000000000000000000, -1.000000000000000000, 0.000000000000000000 ) ) ;
#229 = DIRECTION ( 'NONE',  ( -1.000000000000000000, 0.000000000000000000, 0.000000000000000000 ) ) ;
#231 = VERTEX_POINT ( 'NONE', #96649 ) ;
#230 = CARTESIAN_POINT ( 'NONE',  ( -43.74360349336041054, -60.00000000000002842, 47.43859567335308469 ) ) ;
#232 = CARTESIAN_POINT ( 'NONE',  ( 64.25703057368325233, -46.43406019868007917, 87.64572675471643493 ) ) ;
#233 = EDGE_CURVE ( 'NONE', #104211, #1, #64264, .T. ) ;
#234 = VERTEX_POINT ( 'NONE', #27047 ) ;
#235 = CARTESIAN_POINT ( 'NONE',  ( 7.188101187500000933, -29.56250000204838813, -2.977408999572650483 ) ) ;
#236 = CARTESIAN_POINT ( 'NONE',  ( -101.8692865417259696, -57.67122770170253432, 80.25822756173465677 ) ) ;
#237 = EDGE_LOOP ( 'NONE', ( #11496, #69196 ) ) ;
#238 = CIRCLE ( 'NONE', #77810, 0.4000000000000001887 ) ;
#239 = CARTESIAN_POINT ( 'NONE',  ( 5.290067270632322405, -1.200000000000000030E-05, 8.531152949374478212 ) ) ;
#240 = VECTOR ( 'NONE', #96144, 1000.000000000000114 ) ;
#241 = CARTESIAN_POINT ( 'NONE',  ( 6.529018613599237852, 51.53955942784660493, -6.914392934962513948 ) ) ;
#242 = AXIS2_PLACEMENT_3D ( 'NONE', #2910, #93547, #94618 ) ;
#243 = LINE ( 'NONE', #66079, #65315 ) ;
#244 = CARTESIAN_POINT ( 'NONE',  ( -5.656854249492379694, -21.12500000409676915, -5.656854249492380582 ) ) ;
#245 = CARTESIAN_POINT ( 'NONE',  ( -4.175893272574851878, -3.000000000000000000, 7.137815226409915503 ) ) ;
#246 = CARTESIAN_POINT ( 'NONE',  ( 9.333555687487635311, 248.2189730339102027, 3.591168747312695420 ) ) ;
#247 = CARTESIAN_POINT ( 'NONE',  ( -43.43869229197126458, 464.9661605157749591, 13.42065392471462637 ) ) ;
#248 = CARTESIAN_POINT ( 'NONE',  ( -5.901355035747913647, 4.636240438707916134, 5.000000000000000000 ) ) ;
#249 = CARTESIAN_POINT ( 'NONE',  ( -13.82057366821712030, 304.5462546222179299, 9.872053150317878334 ) ) ;
#250 = ORIENTED_EDGE ( 'NONE', *, *, #71544, .T. ) ;
#251 = DIRECTION ( 'NONE',  ( 0.000000000000000000, -1.000000000000000000, 0.000000000000000000 ) ) ;
#252 = DIRECTION ( 'NONE',  ( 0.000000000000000000, -1.000000000000000000, 0.000000000000000000 ) ) ;
#253 = DIRECTION ( 'NONE',  ( 0.000000000000000000, 0.000000000000000000, -1.000000000000000000 ) ) ;
#254 = CARTESIAN_POINT ( 'NONE',  ( -98.86384284808873701, -30.00000000000000000, 189.1376879781174694 ) ) ;
#255 = EDGE_CURVE ( 'NONE', #38940, #72492, #94463, .T. ) ;
#256 = CARTESIAN_POINT ( 'NONE',  ( 0.000000000000000000, 0.000000000000000000, 0.000000000000000000 ) ) ;
#257 = CARTESIAN_POINT ( 'NONE',  ( 70.33310829152424049, -57.68251784491140199, 156.7550977623263861 ) ) ;
#258 = EDGE_CURVE ( 'NONE', #42466, #63078, #68595, .T. ) ;
#260 = CARTESIAN_POINT ( 'NONE',  ( -6.617290780772931313, 5.039644235285652307, 4.935407925509285754 ) ) ;
#259 = CARTESIAN_POINT ( 'NONE',  ( 15.95426957152705860, -2.597798534188847874, 14.77606491407465406 ) ) ;
#261 = CARTESIAN_POINT ( 'NONE',  ( 15.09152706886165340, -24.11201641507069482, -38.52986768641943627 ) ) ;
#262 = FILL_AREA_STYLE_COLOUR ( '', #16845 ) ;
#263 = CARTESIAN_POINT ( 'NONE',  ( -43.52531999574927113, -60.00000000000001421, 57.80899546987902227 ) ) ;
#264 = CARTESIAN_POINT ( 'NONE',  ( 34.83349330513379982, -4.000000000000000000, 4.898587196589415787E-16 ) ) ;
#265 = LINE ( 'NONE', #48842, #82040 ) ;
#266 = CARTESIAN_POINT ( 'NONE',  ( -86.58262807044705767, -46.48364591595048267, 190.3714820317854617 ) ) ;
#267 = VECTOR ( 'NONE', #35746, 1000.000000000000000 ) ;
#268 = EDGE_LOOP ( 'NONE', ( #80563, #62495, #21493, #73817, #21490 ) ) ;
#269 = CARTESIAN_POINT ( 'NONE',  ( 19.49736279435683173, 49.99988902982553896, 59.96655211255940543 ) ) ;
#270 = CARTESIAN_POINT ( 'NONE',  ( 30.42269336643044397, 12.90989212739758685, 41.86604079465131889 ) ) ;
#271 = CARTESIAN_POINT ( 'NONE',  ( -8.111617385471721065, -32.51280704258433474, 29.30143946630584040 ) ) ;
#272 = CARTESIAN_POINT ( 'NONE',  ( 0.2573354458087858676, -4.368923434677200568, -5.432802636760778903 ) ) ;
#274 = CARTESIAN_POINT ( 'NONE',  ( 2.923709067210019441, -69.56508743643901482, 13.30482931429384585 ) ) ;
#273 = CARTESIAN_POINT ( 'NONE',  ( 4.444974277457670375, -4.939246403834011367, -5.720331885005380812 ) ) ;
#275 = ORIENTED_EDGE ( 'NONE', *, *, #52695, .F. ) ;
#276 = CARTESIAN_POINT ( 'NONE',  ( -46.00000000000000000, 488.5496196030049418, 3.680746121982443775 ) ) ;
#277 = CARTESIAN_POINT ( 'NONE',  ( -6.615712822709019392, -4.357054607612187880, -16.81429077417682549 ) ) ;
#278 = CARTESIAN_POINT ( 'NONE',  ( -7.211357414135266986, 32.01146539934441648, 3.467230644691326802 ) ) ;
#279 = CONICAL_SURFACE ( 'NONE', #70939, 3.309500000000001663, 0.9599310885968770357 ) ;
#280 = CARTESIAN_POINT ( 'NONE',  ( 31.26362620848352947, 298.2545286346129387, -9.251380759131620835 ) ) ;
#281 = CYLINDRICAL_SURFACE ( 'NONE', #32950, 7.000000000000000000 ) ;
#282 = AXIS2_PLACEMENT_3D ( 'NONE', #75371, #11159, #84548 ) ;
#283 = CARTESIAN_POINT ( 'NONE',  ( -7.344133061198927948, -82.55505607319420847, 3.176267128233875248 ) ) ;
#284 = CARTESIAN_POINT ( 'NONE',  ( 36.08349330513379982, 1.593028355512270962E-15, 0.000000000000000000 ) ) ;
#285 = EDGE_CURVE ( 'NONE', #95564, #63670, #35892, .T. ) ;
#286 = CARTESIAN_POINT ( 'NONE',  ( 109.5675852999991662, -29.99999999999999645, 170.1819856699497961 ) ) ;
#287 = CARTESIAN_POINT ( 'NONE',  ( -35.57955382936916067, 363.3973965622570859, 2.919629247011395368 ) ) ;
#288 = VERTEX_POINT ( 'NONE', #8688 ) ;
#289 = CARTESIAN_POINT ( 'NONE',  ( 0.000000000000000000, 0.000000000000000000, -11.12471428571428689 ) ) ;
#290 = CARTESIAN_POINT ( 'NONE',  ( -9.699189539447148789, 253.1769222824670180, -2.444343703917194688 ) ) ;
#291 = SURFACE_STYLE_USAGE ( .BOTH. , #18137 ) ;
#292 = CARTESIAN_POINT ( 'NONE',  ( -3.280815508853482498, -7.221948645665456468, -7.591546097228406786 ) ) ;
#293 = CARTESIAN_POINT ( 'NONE',  ( 3.021254343616667892, 47.67943487759343668, -5.000000000000000000 ) ) ;
#294 = ADVANCED_FACE ( 'NONE', ( #51802 ), #85848, .T. ) ;
#295 = CARTESIAN_POINT ( 'NONE',  ( 0.000000000000000000, 55.00000000000000000, 0.000000000000000000 ) ) ;
#296 = ORIENTED_EDGE ( 'NONE', *, *, #75581, .T. ) ;
#297 = CARTESIAN_POINT ( 'NONE',  ( -3.313708498984817119, -22.53124999999998934, -7.999999999999941380 ) ) ;
#298 = ORIENTED_EDGE ( 'NONE', *, *, #77843, .T. ) ;
#299 = CARTESIAN_POINT ( 'NONE',  ( 38.47428897412589066, 485.7788508071993760, -4.770630528148340765 ) ) ;
#300 = CARTESIAN_POINT ( 'NONE',  ( 32.15310320217080431, 439.7024266304582056, 23.94087012106557211 ) ) ;
#301 = CARTESIAN_POINT ( 'NONE',  ( 9.045746190732545600, 45.90313006749667579, 14.51680462862703891 ) ) ;
#303 = ADVANCED_FACE ( 'NONE', ( #91748 ), #25570, .T. ) ;
#302 = EDGE_LOOP ( 'NONE', ( #4266, #95495, #92686, #39494, #82857, #4404 ) ) ;
#304 = CARTESIAN_POINT ( 'NONE',  ( -5.957442974701830707, 48.00000000000000000, 65.00000000000000000 ) ) ;
#305 = CARTESIAN_POINT ( 'NONE',  ( 5.000000000000000000, -15.25461064037142833, 12.58690023576579620 ) ) ;
#307 = CARTESIAN_POINT ( 'NONE',  ( -29.44801773522681643, -60.00000000000494538, 45.39224945972397052 ) ) ;
#306 = MECHANICAL_DESIGN_GEOMETRIC_PRESENTATION_REPRESENTATION (  '', ( #93377 ), #55528 ) ;
#308 = DIRECTION ( 'NONE',  ( -0.5735764363510512664, 0.8191520442889881348, 1.003171929053520309E-16 ) ) ;
#309 = ORIENTED_EDGE ( 'NONE', *, *, #20951, .F. ) ;
#310 = CARTESIAN_POINT ( 'NONE',  ( 107.0172663714162553, -60.00000000000002132, 197.1060892900004546 ) ) ;
#311 = CIRCLE ( 'NONE', #55388, 4.000000000000007105 ) ;
#313 = CARTESIAN_POINT ( 'NONE',  ( 18.09412890605399227, -49.91541348027277536, 32.54674071594174478 ) ) ;
#312 = CARTESIAN_POINT ( 'NONE',  ( -109.2896413415886485, -29.99999999999996092, 180.5615511752786233 ) ) ;
#314 = UNCERTAINTY_MEASURE_WITH_UNIT (LENGTH_MEASURE( 1.000000000000000082E-05 ), #86417, 'distance_accuracy_value', 'NONE');
#315 = CARTESIAN_POINT ( 'NONE',  ( 1.218045234088034112, 53.93925255856578360, -8.677002990697831208 ) ) ;
#316 = CARTESIAN_POINT ( 'NONE',  ( -41.05697111444229819, -36.06893584801743202, 38.79370462227291227 ) ) ;
#317 =( GEOMETRIC_REPRESENTATION_CONTEXT ( 3 ) GLOBAL_UNCERTAINTY_ASSIGNED_CONTEXT ( ( #48311 ) ) GLOBAL_UNIT_ASSIGNED_CONTEXT ( ( #53769, #12768, #45689 ) ) REPRESENTATION_CONTEXT ( 'NONE', 'WORKASPACE' ) );
#318 = CARTESIAN_POINT ( 'NONE',  ( -14.62309622336928783, 18.64284798593354964, -35.53993507408184627 ) ) ;
#319 = ORIENTED_EDGE ( 'NONE', *, *, #87246, .F. ) ;
#320 = PRESENTATION_STYLE_ASSIGNMENT (( #72655 ) ) ;
#321 = CARTESIAN_POINT ( 'NONE',  ( 98.59800593614012598, -5.000000000000020428, 0.000000000000000000 ) ) ;
#322 = CARTESIAN_POINT ( 'NONE',  ( 25.95507789760542039, 309.1386286255022924, 10.94030088463808070 ) ) ;
#323 = SURFACE_STYLE_FILL_AREA ( #74247 ) ;
#324 = DIRECTION ( 'NONE',  ( -1.000000000000000000, -0.000000000000000000, -0.000000000000000000 ) ) ;
#325 = CARTESIAN_POINT ( 'NONE',  ( -37.27001300466930900, 460.4716935085137948, 2.455202772530845401 ) ) ;
#326 = ORIENTED_EDGE ( 'NONE', *, *, #60102, .F. ) ;
#327 = CARTESIAN_POINT ( 'NONE',  ( 4.586789253316146286, -47.77528324151398209, 102.5764008378948091 ) ) ;
#328 = EDGE_LOOP ( 'NONE', ( #41587, #87018 ) ) ;
#329 = CARTESIAN_POINT ( 'NONE',  ( 76.44072697005394446, -30.00000000006936318, 169.7891841772097052 ) ) ;
#330 = CARTESIAN_POINT ( 'NONE',  ( -1.544427540536530316E-15, -4.285714285714290916, 25.22241582816893057 ) ) ;
#331 = DIRECTION ( 'NONE',  ( -1.000000000000000000, -1.224606353822377258E-16, -0.000000000000000000 ) ) ;
#332 = DIRECTION ( 'NONE',  ( -1.000000000000000000, -1.224606353822377258E-16, -0.000000000000000000 ) ) ;
#333 = CARTESIAN_POINT ( 'NONE',  ( 90.70948918873676803, -30.00000000000000000, 92.63632137647867637 ) ) ;
#334 = EDGE_CURVE ( 'NONE', #34125, #93985, #84713, .T. ) ;
#335 = CARTESIAN_POINT ( 'NONE',  ( 7.999912353029506207, 101.0001752939690647, -0.2691822806795024503 ) ) ;
#336 = ORIENTED_EDGE ( 'NONE', *, *, #86962, .T. ) ;
#337 = VERTEX_POINT ( 'NONE', #16789 ) ;
#338 = ORIENTED_EDGE ( 'NONE', *, *, #17693, .T. ) ;
#339 = DIRECTION ( 'NONE',  ( -1.000000000000000000, -1.224606353822377258E-16, -0.000000000000000000 ) ) ;
#340 = CARTESIAN_POINT ( 'NONE',  ( -5.413519594459913264, -11.02779875410785237, -10.18303460993699971 ) ) ;
#341 = CARTESIAN_POINT ( 'NONE',  ( -41.16035149709456675, 464.6079056639530904, 16.67014335653854218 ) ) ;
#342 = EDGE_CURVE ( 'NONE', #9727, #28736, #74562, .T. ) ;
#343 = CARTESIAN_POINT ( 'NONE',  ( -30.47452941428689144, 336.9182531266175715, 16.65730915348260410 ) ) ;
#344 = FILL_AREA_STYLE ('',( #10074 ) ) ;
#345 = ORIENTED_EDGE ( 'NONE', *, *, #51668, .F. ) ;
#346 = SURFACE_SIDE_STYLE ('',( #64603 ) ) ;
#347 = VERTEX_POINT ( 'NONE', #103552 ) ;
#348 = CARTESIAN_POINT ( 'NONE',  ( 33.16497501405928716, 438.9508968883829425, 23.91452439716892187 ) ) ;
#349 = CARTESIAN_POINT ( 'NONE',  ( 78.80651474684775337, -38.66927030591594416, 190.4702765846127477 ) ) ;
#350 = LINE ( 'NONE', #100679, #26605 ) ;
#351 = CARTESIAN_POINT ( 'NONE',  ( 30.36308363480350536, 298.1723161944738081, 2.669529410806691150 ) ) ;
#352 = FILL_AREA_STYLE ('',( #57023 ) ) ;
#353 = CARTESIAN_POINT ( 'NONE',  ( 5.581309233574441675E-23, 43.17555810750860701, -18.75000000000000355 ) ) ;
#355 = EDGE_CURVE ( 'NONE', #17308, #71961, #69604, .T. ) ;
#354 = AXIS2_PLACEMENT_3D ( 'NONE', #30290, #103624, #54514 ) ;
#356 = CARTESIAN_POINT ( 'NONE',  ( -28.08625202345140792, 34.36930134029169892, -8.015757243435880142 ) ) ;
#357 = CIRCLE ( 'NONE', #7239, 15.00000000000000711 ) ;
#358 = DIRECTION ( 'NONE',  ( 0.000000000000000000, 1.000000000000000000, 0.000000000000000000 ) ) ;
#359 = DIRECTION ( 'NONE',  ( -1.000000000000000000, 0.000000000000000000, 0.000000000000000000 ) ) ;
#360 = DIRECTION ( 'NONE',  ( -1.000000000000000000, -1.224606353822377258E-16, -0.000000000000000000 ) ) ;
#361 = EDGE_LOOP ( 'NONE', ( #69773, #97426, #67085, #73591, #21283 ) ) ;
#363 = CARTESIAN_POINT ( 'NONE',  ( -23.85731009206051567, 303.8684408157198504, 10.15848730775081599 ) ) ;
#362 = SURFACE_STYLE_USAGE ( .BOTH. , #70999 ) ;
#364 = FACE_OUTER_BOUND ( 'NONE', #54905, .T. ) ;
#365 = FILL_AREA_STYLE ('',( #52142 ) ) ;
#366 = CARTESIAN_POINT ( 'NONE',  ( -5.656854249492381470, -10.06249999999999112, 5.656854249492379694 ) ) ;
#367 = DIRECTION ( 'NONE',  ( 0.2281669654646126255, 0.2206132685146504901, 0.9482982767178022021 ) ) ;
#368 = CIRCLE ( 'NONE', #53762, 4.000000000000000888 ) ;
#369 = B_SPLINE_CURVE_WITH_KNOTS ( 'NONE', 3,
 ( #79357, #70214, #86946, #54006 ),
 .UNSPECIFIED., .F., .F.,
 ( 4, 4 ),
 ( 0.000000000000000000, 0.002179261451102595427 ),
 .UNSPECIFIED. ) ;
#370 = DIRECTION ( 'NONE',  ( 0.000000000000000000, -1.000000000000000000, 0.000000000000000000 ) ) ;
#371 = CYLINDRICAL_SURFACE ( 'NONE', #34798, 3.400000000000000355 ) ;
#372 = CARTESIAN_POINT ( 'NONE',  ( 85.94098261277883921, -35.59794438537343808, 185.2097674715711833 ) ) ;
#373 = CYLINDRICAL_SURFACE ( 'NONE', #62496, 4.000000000000000000 ) ;
#374 = ORIENTED_EDGE ( 'NONE', *, *, #93282, .F. ) ;
#375 = CARTESIAN_POINT ( 'NONE',  ( 87.67975675995961637, -57.66951933457082191, -24.82267382768696251 ) ) ;
#376 = CARTESIAN_POINT ( 'NONE',  ( 0.000000000000000000, 0.000000000000000000, 27.00000000000000000 ) ) ;
#377 = CARTESIAN_POINT ( 'NONE',  ( 30.00000000000000000, 0.000000000000000000, 15.00000000000000000 ) ) ;
#378 =( BOUNDED_CURVE ( )  B_SPLINE_CURVE ( 2, ( #76091, #61000, #11891, #101964, #28124, #35141, #100895, #50737, #44819 ),
 .UNSPECIFIED., .F., .F. ) 
 B_SPLINE_CURVE_WITH_KNOTS ( ( 3, 2, 2, 2, 3 ),
 ( 0.5735294117647058432, 0.5808823529411765163, 0.5882352941176470784, 0.5955882352941176405, 0.6029411764705882026 ),
 .UNSPECIFIED. ) 
 CURVE ( )  GEOMETRIC_REPRESENTATION_ITEM ( )  RATIONAL_B_SPLINE_CURVE ( ( 1.000000000000000000, 0.9238795325112867385, 1.000000000000000000, 0.9238795325112867385, 1.000000000000000000, 0.9238795325112867385, 1.000000000000000000, 0.9238795325112867385, 1.000000000000000000 ) ) 
 REPRESENTATION_ITEM ( '' )  );
#379 = MECHANICAL_DESIGN_GEOMETRIC_PRESENTATION_REPRESENTATION (  '', ( #26349 ), #84892 ) ;
#380 = CARTESIAN_POINT ( 'NONE',  ( -81.08062976773315711, -30.00000000000001421, 2.674856533068522779 ) ) ;
#381 = EDGE_CURVE ( 'NONE', #74067, #18, #102497, .T. ) ;
#382 = B_SPLINE_CURVE_WITH_KNOTS ( 'NONE', 3,
 ( #64122, #81847, #38263, #71124 ),
 .UNSPECIFIED., .F., .F.,
 ( 4, 4 ),
 ( 0.0009348627901856346525, 0.02189385877134459105 ),
 .UNSPECIFIED. ) ;
#383 = CARTESIAN_POINT ( 'NONE',  ( 28.58272191126957651, 16.23375075743845031, 41.45992959583530535 ) ) ;
#384 = DIRECTION ( 'NONE',  ( -1.000000000000000000, 0.000000000000000000, 0.000000000000000000 ) ) ;
#385 = CARTESIAN_POINT ( 'NONE',  ( 14.27307692307692299, -4.171999999999999709, 0.000000000000000000 ) ) ;
#386 = ADVANCED_FACE ( 'NONE', ( #53417 ), #96135, .T. ) ;
#388 = CARTESIAN_POINT ( 'NONE',  ( 23.58349330513380337, 1.593028355512270962E-15, 0.000000000000000000 ) ) ;
#387 = CARTESIAN_POINT ( 'NONE',  ( 0.5805565836007605673, 3.752776749732565253, 6.499999999999997335 ) ) ;
#389 = DIRECTION ( 'NONE',  ( 0.000000000000000000, -1.000000000000000000, 0.000000000000000000 ) ) ;
#390 = CARTESIAN_POINT ( 'NONE',  ( -29.68315524076956535, 13.47185074185901499, 42.10535821593508388 ) ) ;
#391 = SURFACE_STYLE_USAGE ( .BOTH. , #82418 ) ;
#392 = CARTESIAN_POINT ( 'NONE',  ( 4.472135954999578722, -84.72588149001676072, -4.000000000000003553 ) ) ;
#393 = CARTESIAN_POINT ( 'NONE',  ( -22.13658770490400229, 25.65638329602028733, 32.60403273639936117 ) ) ;
#394 = DIRECTION ( 'NONE',  ( 0.000000000000000000, 0.5000000000000009992, 0.8660254037844380415 ) ) ;
#395 = AXIS2_PLACEMENT_3D ( 'NONE', #92986, #43904, #76792 ) ;
#396 = CARTESIAN_POINT ( 'NONE',  ( -100.1961331157895785, -37.99999999999996447, 190.2810200694672744 ) ) ;
#397 = EDGE_LOOP ( 'NONE', ( #26477, #74616, #27189, #53326 ) ) ;
#398 = CARTESIAN_POINT ( 'NONE',  ( -6.928203230275510549, 29.99999999999999645, -4.000000000000000000 ) ) ;
#399 = DIRECTION ( 'NONE',  ( 0.000000000000000000, 1.000000000000000000, 0.000000000000000000 ) ) ;
#400 = CARTESIAN_POINT ( 'NONE',  ( 28.99999999999999645, 6.123233995736765296E-16, -4.999999999999999112 ) ) ;
#401 = CARTESIAN_POINT ( 'NONE',  ( -58.10004709386434740, -28.99893100057961703, -25.62387168749792465 ) ) ;
#403 = FACE_OUTER_BOUND ( 'NONE', #11304, .T. ) ;
#402 = CARTESIAN_POINT ( 'NONE',  ( 102.0666666666666629, 1.023464760207051730E-14, 0.000000000000000000 ) ) ;
#404 = EDGE_CURVE ( 'NONE', #3901, #1310, #12401, .T. ) ;
#405 = ORIENTED_EDGE ( 'NONE', *, *, #80496, .T. ) ;
#406 = ORIENTED_EDGE ( 'NONE', *, *, #769, .T. ) ;
#407 = CARTESIAN_POINT ( 'NONE',  ( -26.78494459259576033, 34.86751637306745977, 7.587752381711101890 ) ) ;
#408 = DIRECTION ( 'NONE',  ( 0.000000000000000000, 0.000000000000000000, -1.000000000000000000 ) ) ;
#409 =( NAMED_UNIT ( * ) PLANE_ANGLE_UNIT ( ) SI_UNIT ( $, .RADIAN. ) );
#410 = CARTESIAN_POINT ( 'NONE',  ( -90.00834054549592622, -60.00000000000000711, -18.84511867618155634 ) ) ;
#411 = ORIENTED_EDGE ( 'NONE', *, *, #79860, .T. ) ;
#412 = CARTESIAN_POINT ( 'NONE',  ( 18.45432732700360390, -25.80688170520882352, -30.46384464344198406 ) ) ;
#413 = CARTESIAN_POINT ( 'NONE',  ( 67.96666666666666856, -3.309500000000000774, 4.475777889183797681E-16 ) ) ;
#414 = CARTESIAN_POINT ( 'NONE',  ( 101.1404883722410517, -52.73811232283483008, 193.2266567730409292 ) ) ;
#416 = CARTESIAN_POINT ( 'NONE',  ( -16.80263806300990481, 45.55013935554968185, 6.657797401561873940 ) ) ;
#415 = CARTESIAN_POINT ( 'NONE',  ( 3.816988791951658744, -18.99760367465201938, 27.04954382783872546 ) ) ;
#417 = ORIENTED_EDGE ( 'NONE', *, *, #61734, .F. ) ;
#418 = MECHANICAL_DESIGN_GEOMETRIC_PRESENTATION_REPRESENTATION (  '', ( #43583 ), #41807 ) ;
#419 = EDGE_LOOP ( 'NONE', ( #2090, #86427, #72217, #95516, #41988, #25906 ) ) ;
#420 =( GEOMETRIC_REPRESENTATION_CONTEXT ( 3 ) GLOBAL_UNCERTAINTY_ASSIGNED_CONTEXT ( ( #22603 ) ) GLOBAL_UNIT_ASSIGNED_CONTEXT ( ( #87873, #23154, #22635 ) ) REPRESENTATION_CONTEXT ( 'NONE', 'WORKASPACE' ) );
#421 = ORIENTED_EDGE ( 'NONE', *, *, #82408, .T. ) ;
#422 = CARTESIAN_POINT ( 'NONE',  ( 30.61824294310940076, 339.8033301911921171, 17.27473575236878389 ) ) ;
#423 = CARTESIAN_POINT ( 'NONE',  ( -6.081241251370744116, -12.38970427209902425, 12.35256966254870115 ) ) ;
#424 = CARTESIAN_POINT ( 'NONE',  ( 9.810831326706606959, 53.41083018302243346, 2.841840335636323989 ) ) ;
#426 = EDGE_CURVE ( 'NONE', #9363, #29639, #83534, .T. ) ;
#425 = ORIENTED_EDGE ( 'NONE', *, *, #39572, .T. ) ;
#427 = CARTESIAN_POINT ( 'NONE',  ( 16.48303619537878006, 45.94111582078985379, -4.157797401561770911 ) ) ;
#428 = CARTESIAN_POINT ( 'NONE',  ( -7.125691916582565177, 41.67430808341742932, -69.26730091582949456 ) ) ;
#429 = DIRECTION ( 'NONE',  ( 1.000000000000000000, -0.000000000000000000, -0.000000000000000000 ) ) ;
#430 = CARTESIAN_POINT ( 'NONE',  ( -14.02841258157142690, -57.67128452586098319, 41.71853563109401364 ) ) ;
#431 = CARTESIAN_POINT ( 'NONE',  ( 7.188101187500001821, -34.06250000204839523, -2.977408999572650483 ) ) ;
#432 = CARTESIAN_POINT ( 'NONE',  ( -30.55667715332060297, 16.37467338430767683, 39.95293003182839442 ) ) ;
#433 = CARTESIAN_POINT ( 'NONE',  ( -21.23684446602550935, 304.9566545053270943, -9.977713076987674512 ) ) ;
#434 = FACE_OUTER_BOUND ( 'NONE', #87709, .T. ) ;
#435 = CARTESIAN_POINT ( 'NONE',  ( 8.555192725956649369, -60.00000000000006395, -44.87746236044966253 ) ) ;
#436 = CARTESIAN_POINT ( 'NONE',  ( -17.10644827616429708, -60.00000000000001421, 42.25319189086976479 ) ) ;
#437 = CARTESIAN_POINT ( 'NONE',  ( -51.13187347197568755, -25.65488839008201438, 47.91772828370423554 ) ) ;
#438 = CARTESIAN_POINT ( 'NONE',  ( 0.2708782075111812460, 21.85270131633358304, -7.000000000000008882 ) ) ;
#439 = ORIENTED_EDGE ( 'NONE', *, *, #77485, .F. ) ;
#440 = CARTESIAN_POINT ( 'NONE',  ( -99.38087883715134296, -60.32317553465453841, 196.1180290444751222 ) ) ;
#441 =( REPRESENTATION_RELATIONSHIP ('NONE','NONE', #69581, #74292 ) REPRESENTATION_RELATIONSHIP_WITH_TRANSFORMATION ( #103638 )SHAPE_REPRESENTATION_RELATIONSHIP( ) );
#442 = CARTESIAN_POINT ( 'NONE',  ( -2.295593195902894124, 298.7070635967813246, -10.00347380708980261 ) ) ;
#443 = CARTESIAN_POINT ( 'NONE',  ( 12.37144696128341792, -4.000000000000002665, 20.44658103856077602 ) ) ;
#444 = VERTEX_POINT ( 'NONE', #60986 ) ;
#445 = CARTESIAN_POINT ( 'NONE',  ( -16.96103378808793138, 43.64123910865905032, 4.188553803742784076 ) ) ;
#446 = CARTESIAN_POINT ( 'NONE',  ( 89.04072021948540794, -38.53165156231079891, 200.3084838905402592 ) ) ;
#447 = CARTESIAN_POINT ( 'NONE',  ( 29.34999999999999787, 1.533819458162526451E-15, 0.000000000000000000 ) ) ;
#448 = FACE_OUTER_BOUND ( 'NONE', #50951, .T. ) ;
#449 = CARTESIAN_POINT ( 'NONE',  ( -20.15810180139540364, 294.7575509362039838, 1.916965569035420369 ) ) ;
#450 = CARTESIAN_POINT ( 'NONE',  ( 72.41885610122542971, 42.00000000000000000, -55.65414010180089832 ) ) ;
#451 = CARTESIAN_POINT ( 'NONE',  ( 85.77043248607724024, -30.00000000000001066, 176.9767547045051685 ) ) ;
#452 = CARTESIAN_POINT ( 'NONE',  ( 37.50059943756071590, 490.7879993827834255, 12.38039871356642507 ) ) ;
#453 = FACE_OUTER_BOUND ( 'NONE', #37066, .T. ) ;
#454 = ADVANCED_FACE ( 'NONE', ( #62064 ), #49615, .T. ) ;
#455 = CARTESIAN_POINT ( 'NONE',  ( 27.33349330513380693, -4.000000000000000888, 4.898587196589416773E-16 ) ) ;
#456 = B_SPLINE_CURVE_WITH_KNOTS ( 'NONE', 3,
 ( #78501, #3568, #102254, #28404 ),
 .UNSPECIFIED., .F., .F.,
 ( 4, 4 ),
 ( 0.008938635547386365732, 0.01006686641814317357 ),
 .UNSPECIFIED. ) ;
#457 = VERTEX_POINT ( 'NONE', #94953 ) ;
#458 = ORIENTED_EDGE ( 'NONE', *, *, #93604, .T. ) ;
#459 = CARTESIAN_POINT ( 'NONE',  ( 52.85568683939615653, -25.63927253738310341, 50.79666856344920234 ) ) ;
#460 = CONICAL_SURFACE ( 'NONE', #53864, 3.309500000000007880, 0.9599310885968770357 ) ;
#461 = CARTESIAN_POINT ( 'NONE',  ( -4.691018660002292506, 301.0267645919033157, -10.01286726553616191 ) ) ;
#462 = CARTESIAN_POINT ( 'NONE',  ( 9.781067317119404692, 51.26646010159761602, 3.095465610852687899 ) ) ;
#463 = ADVANCED_FACE ( 'NONE', ( #21088 ), #52709, .F. ) ;
#464 = ORIENTED_EDGE ( 'NONE', *, *, #17873, .F. ) ;
#465 = CARTESIAN_POINT ( 'NONE',  ( -92.64914355384837563, -38.35495843336040878, 40.51828768684245574 ) ) ;
#466 = ORIENTED_EDGE ( 'NONE', *, *, #57229, .F. ) ;
#467 =( NAMED_UNIT ( * ) SI_UNIT ( $, .STERADIAN. ) SOLID_ANGLE_UNIT ( ) );
#468 = CARTESIAN_POINT ( 'NONE',  ( 98.81766897887224843, -38.35584203838750739, 81.49447246300090342 ) ) ;
#469 = CARTESIAN_POINT ( 'NONE',  ( 13.30905003209610982, 22.18330274843690475, 4.016012902930523154 ) ) ;
#470 = CARTESIAN_POINT ( 'NONE',  ( 87.19055186570717808, -60.14788264809187979, 31.77688151689448404 ) ) ;
#471 = CARTESIAN_POINT ( 'NONE',  ( -17.58486903827841275, 43.20934354716421666, -6.234446319141409454 ) ) ;
#472 = CARTESIAN_POINT ( 'NONE',  ( 4.905843853654985764, -4.999999999999999112, -16.52456679617690938 ) ) ;
#473 = CARTESIAN_POINT ( 'NONE',  ( -29.63900401201415136, 311.2735914789724916, -7.504590757657062738 ) ) ;
#474 = DIRECTION ( 'NONE',  ( 1.000000000000000000, 0.000000000000000000, 0.000000000000000000 ) ) ;
#475 = CARTESIAN_POINT ( 'NONE',  ( 75.45569487463558289, -60.00000000000000711, 184.2290690944641369 ) ) ;
#476 = EDGE_CURVE ( 'NONE', #67441, #75440, #73711, .T. ) ;
#477 = CARTESIAN_POINT ( 'NONE',  ( 18.14701115887386607, 45.00000000000001421, 62.47877254244827583 ) ) ;
#478 = VERTEX_POINT ( 'NONE', #19497 ) ;
#479 = CARTESIAN_POINT ( 'NONE',  ( 59.37731412860715352, -46.43601160270981154, 73.85368140583713625 ) ) ;
#480 = CARTESIAN_POINT ( 'NONE',  ( -28.47508235818447986, 296.9186349479344926, -1.549936504308094598 ) ) ;
#481 = CARTESIAN_POINT ( 'NONE',  ( 9.113097280746998763, -53.73680858635314905, 31.11721482942555639 ) ) ;
#482 = DIRECTION ( 'NONE',  ( -1.000000000000000000, -0.000000000000000000, -0.000000000000000000 ) ) ;
#484 = CARTESIAN_POINT ( 'NONE',  ( -33.00000000000004263, 485.0303364503728289, 0.9535057477319844876 ) ) ;
#483 = CARTESIAN_POINT ( 'NONE',  ( -66.20132703361541360, -30.00000000008030909, 112.2256356094896432 ) ) ;
#485 = CARTESIAN_POINT ( 'NONE',  ( -39.41908235148878958, 328.0183126189934342, 18.00525811984569913 ) ) ;
#486 = CARTESIAN_POINT ( 'NONE',  ( -38.18724015216890422, 25.28177589261053271, -13.30327295121670694 ) ) ;
#487 = DIRECTION ( 'NONE',  ( -0.8191520442889881348, 1.003171929053520186E-16, 0.5735764363510513775 ) ) ;
#488 = CARTESIAN_POINT ( 'NONE',  ( 8.000000000000000000, -28.90624999999999645, -3.313708498984761608 ) ) ;
#489 = CARTESIAN_POINT ( 'NONE',  ( -2.617478844990611897, -3.000000000000002665, -75.26027323389583046 ) ) ;
#490 = DIRECTION ( 'NONE',  ( -0.000000000000000000, 1.000000000000000000, -0.000000000000000000 ) ) ;
#491 = AXIS2_PLACEMENT_3D ( 'NONE', #31691, #89386, #30635 ) ;
#492 = VERTEX_POINT ( 'NONE', #52334 ) ;
#493 = CARTESIAN_POINT ( 'NONE',  ( 84.47996738200173183, -35.89428493999452030, 177.6417994544143539 ) ) ;
#494 = CARTESIAN_POINT ( 'NONE',  ( 43.50722185568069023, 484.7945611035598290, 4.126806436305178849 ) ) ;
#495 = CARTESIAN_POINT ( 'NONE',  ( -41.99101837128264236, 437.4456563656356138, 21.44456026107220126 ) ) ;
#496 = ORIENTED_EDGE ( 'NONE', *, *, #13109, .T. ) ;
#497 = AXIS2_PLACEMENT_3D ( 'NONE', #11558, #44489, #45027 ) ;
#498 = LINE ( 'NONE', #24845, #77218 ) ;
#499 = CARTESIAN_POINT ( 'NONE',  ( 4.905367688403428517, -5.000000000000055067, -16.52522736516917590 ) ) ;
#500 = CARTESIAN_POINT ( 'NONE',  ( -32.89532852795978357, 465.6911463857132389, 10.83018753746699581 ) ) ;
#501 = CARTESIAN_POINT ( 'NONE',  ( 6.162888688655347558, 7.505553499465140277, 0.000000000000000000 ) ) ;
#502 = CARTESIAN_POINT ( 'NONE',  ( -38.79245513715870430, 42.07398859163519234, -57.16919138223752839 ) ) ;
#503 = VECTOR ( 'NONE', #36456, 1000.000000000000341 ) ;
#504 = CARTESIAN_POINT ( 'NONE',  ( -12.40466434899015447, -3.812810247667897112, 20.50928832961362502 ) ) ;
#505 = ADVANCED_FACE ( 'NONE', ( #4864 ), #70658, .T. ) ;
#506 = CARTESIAN_POINT ( 'NONE',  ( 47.40960664892755005, -60.00000000000000000, 65.69262840591406416 ) ) ;
#507 = STYLED_ITEM ( 'NONE', ( #43636 ), #21377 ) ;
#508 = FACE_OUTER_BOUND ( 'NONE', #74890, .T. ) ;
#509 = CARTESIAN_POINT ( 'NONE',  ( 11.66830085788263105, -14.19238082999582851, 31.80802733702232388 ) ) ;
#510 = EDGE_CURVE ( 'NONE', #30914, #85394, #78873, .T. ) ;
#511 = EDGE_CURVE ( 'NONE', #39124, #34646, #11877, .T. ) ;
#513 = CARTESIAN_POINT ( 'NONE',  ( -15.57949638806330839, 22.99924373907892061, -0.5870217286331953499 ) ) ;
#512 = CARTESIAN_POINT ( 'NONE',  ( -6.915205664888873116, -19.09113298351051569, 35.17258881450032959 ) ) ;
#514 = CARTESIAN_POINT ( 'NONE',  ( -1.320432766682874540E-15, -16.53125000204838813, 7.188101187500000044 ) ) ;
#515 = CARTESIAN_POINT ( 'NONE',  ( 30.50814924115433158, 298.0999724620219240, -1.284670219152425297 ) ) ;
#516 = EDGE_CURVE ( 'NONE', #54910, #26965, #77693, .T. ) ;
#517 = ORIENTED_EDGE ( 'NONE', *, *, #1884, .T. ) ;
#518 = CARTESIAN_POINT ( 'NONE',  ( -17.50000000000280664, 49.91179365273242041, 61.97298340137167116 ) ) ;
#519 = COLOUR_RGB ( '', 0.72549020, 0.75294118, 0.79215686) ;
#520 = CARTESIAN_POINT ( 'NONE',  ( 24.46397269780010930, 25.31587970897912854, 32.08082341745669908 ) ) ;
#521 = FILL_AREA_STYLE ('',( #34037 ) ) ;
#522 = VECTOR ( 'NONE', #46039, 1000.000000000000341 ) ;
#524 = CARTESIAN_POINT ( 'NONE',  ( 51.46559081915259526, -60.22828912016439773, -31.80537533325271937 ) ) ;
#523 = CARTESIAN_POINT ( 'NONE',  ( 4.964745198532805048, 53.54848248096784147, 8.490843834923378353 ) ) ;
#525 = EDGE_CURVE ( 'NONE', #14360, #31711, #89207, .T. ) ;
#526 = STYLED_ITEM ( 'NONE', ( #63722 ), #78240 ) ;
#527 = ORIENTED_EDGE ( 'NONE', *, *, #13782, .T. ) ;
#528 = PRESENTATION_LAYER_ASSIGNMENT (  '', '', ( #72933 ) ) ;
#529 = CARTESIAN_POINT ( 'NONE',  ( 14.13631897826462236, 21.04363150066026478, -5.954641296519788796 ) ) ;
#530 = DIRECTION ( 'NONE',  ( -0.5735764363510512664, 0.8191520442889881348, 1.003171929053520309E-16 ) ) ;
#531 = AXIS2_PLACEMENT_3D ( 'NONE', #35055, #67923, #93265 ) ;
#532 = ORIENTED_EDGE ( 'NONE', *, *, #38834, .T. ) ;
#533 = SHAPE_REPRESENTATION ( '15. Rubber Handle Cover', ( #10728 ), #93743 ) ;
#534 = ADVANCED_FACE ( 'NONE', ( #97043 ), #23790, .T. ) ;
#535 = CARTESIAN_POINT ( 'NONE',  ( 102.0666666666666629, 4.172000000000019249, 0.000000000000000000 ) ) ;
#536 = CARTESIAN_POINT ( 'NONE',  ( -19.50262057251149983, 41.86950174827330073, -80.38433612792447036 ) ) ;
#537 = CARTESIAN_POINT ( 'NONE',  ( -101.1691898682323227, -59.99999999999998579, 87.89072118495219854 ) ) ;
#538 = CYLINDRICAL_SURFACE ( 'NONE', #78993, 7.000000000000000000 ) ;
#539 = CARTESIAN_POINT ( 'NONE',  ( -44.17836536378457168, 435.2619773020560956, 14.65562696767996087 ) ) ;
#540 = CARTESIAN_POINT ( 'NONE',  ( 31.03867016165222026, 468.3124986733989772, 18.90871194958903345 ) ) ;
#541 = CARTESIAN_POINT ( 'NONE',  ( -5.385673916453011856, 3.157894736842104866, 14.66382285868950675 ) ) ;
#543 = CARTESIAN_POINT ( 'NONE',  ( 30.00000000000000355, 488.8442721620239695, 4.433647275927809162 ) ) ;
#542 = CARTESIAN_POINT ( 'NONE',  ( -3.140974613990845210, -5.000000000000002665, -73.31232788067644890 ) ) ;
#544 = CARTESIAN_POINT ( 'NONE',  ( -81.41457456882541521, -53.45414052628666468, 177.1216105972638672 ) ) ;
#545 = ORIENTED_EDGE ( 'NONE', *, *, #45539, .T. ) ;
#546 = CARTESIAN_POINT ( 'NONE',  ( -27.10511071441183262, -1.200000000000000030E-05, 8.806984339686158236 ) ) ;
#547 = ORIENTED_EDGE ( 'NONE', *, *, #27451, .T. ) ;
#548 = ORIENTED_EDGE ( 'NONE', *, *, #97150, .F. ) ;
#549 = CARTESIAN_POINT ( 'NONE',  ( 33.58349330513379982, 4.898587196589405926E-16, -4.000000000000001776 ) ) ;
#550 = VERTEX_POINT ( 'NONE', #55500 ) ;
#551 = DIRECTION ( 'NONE',  ( 0.000000000000000000, -0.000000000000000000, 1.000000000000000000 ) ) ;
#552 = CARTESIAN_POINT ( 'NONE',  ( -21.29975379448946171, 294.8969325209483259, -1.990407376643346327 ) ) ;
#553 = CARTESIAN_POINT ( 'NONE',  ( -7.344133061198929724, -62.55505607319423689, 3.176267128233876136 ) ) ;
#554 = CARTESIAN_POINT ( 'NONE',  ( -30.00000000000000000, 488.6481008951269587, 3.890293910847615333 ) ) ;
#555 = DIRECTION ( 'NONE',  ( -1.000000000000000000, -1.224606353822377258E-16, -0.000000000000000000 ) ) ;
#556 = CARTESIAN_POINT ( 'NONE',  ( -16.75187969033554936, 36.38380281757302015, -24.30698433968596106 ) ) ;
#557 = CARTESIAN_POINT ( 'NONE',  ( 106.6845404271915925, -14.21045842199438525, 180.1433801272770836 ) ) ;
#558 = CARTESIAN_POINT ( 'NONE',  ( -106.4002951517535536, -14.21045842199431242, 159.7122570458138284 ) ) ;
#559 = B_SPLINE_CURVE_WITH_KNOTS ( 'NONE', 3,
 ( #3751, #4273, #36682, #21544, #20521 ),
 .UNSPECIFIED., .F., .F.,
 ( 4, 1, 4 ),
 ( 0.000000000000000000, 0.003752776749732568331, 0.007505553499465136662 ),
 .UNSPECIFIED. ) ;
#560 = CARTESIAN_POINT ( 'NONE',  ( -62.70045667444673398, -49.91596129396690174, 84.84719086326107629 ) ) ;
#561 = ORIENTED_EDGE ( 'NONE', *, *, #23670, .T. ) ;
#562 = CARTESIAN_POINT ( 'NONE',  ( 30.80675973667872114, 38.95360674089970132, 55.79500139137103076 ) ) ;
#563 = CARTESIAN_POINT ( 'NONE',  ( 98.58876825478586170, -59.99999999996099831, 57.54132604300040299 ) ) ;
#564 = EDGE_LOOP ( 'NONE', ( #72953, #38325, #11887, #25764 ) ) ;
#565 = CARTESIAN_POINT ( 'NONE',  ( 8.282570541373461381, -53.39685655951549847, 32.78284559411562071 ) ) ;
#566 = CARTESIAN_POINT ( 'NONE',  ( -101.9291513569354350, -37.82052686412928466, 156.3387055009734752 ) ) ;
#567 = CARTESIAN_POINT ( 'NONE',  ( -1.320432766682874540E-15, -12.40625000204838635, 7.188101187500000044 ) ) ;
#568 = VECTOR ( 'NONE', #12370, 1000.000000000000000 ) ;
#569 = CARTESIAN_POINT ( 'NONE',  ( 8.866506694866188809, -3.851859888774471706E-31, 4.000000000000000888 ) ) ;
#570 = ORIENTED_EDGE ( 'NONE', *, *, #97685, .F. ) ;
#571 = B_SPLINE_CURVE_WITH_KNOTS ( 'NONE', 3,
 ( #27752, #101054, #45501, #20192, #77850, #78371, #12039, #68714, #35290, #43357, #53047, #20734, #85965, #84350, #76242, #36896, #68159, #52494, #69762, #44423 ),
 .UNSPECIFIED., .F., .F.,
 ( 4, 2, 2, 2, 2, 2, 2, 2, 2, 4 ),
 ( 0.003055152949284218288, 0.003559479741444611378, 0.003811643137524814429, 0.004063806533605017479, 0.004568133325765439193, 0.005072460117925860039, 0.006081113702246704333, 0.006585440494407136455, 0.006837603890487358588, 0.007089767286567579853 ),
 .UNSPECIFIED. ) ;
#572 = CARTESIAN_POINT ( 'NONE',  ( 73.59428447264397732, 6.856755485862130937E-15, 0.000000000000000000 ) ) ;
#573 = ORIENTED_EDGE ( 'NONE', *, *, #17362, .F. ) ;
#574 = CARTESIAN_POINT ( 'NONE',  ( -46.00000000000000000, 488.3725375423296668, 3.127739281037489771 ) ) ;
#575 = VECTOR ( 'NONE', #68936, 1000.000000000000000 ) ;
#576 = CARTESIAN_POINT ( 'NONE',  ( -31.79882010337384912, -60.00000000000000000, 44.03261922666757044 ) ) ;
#577 = CARTESIAN_POINT ( 'NONE',  ( 7.188101187500001821, -17.93750000204838457, -2.977408999572650483 ) ) ;
#578 = CARTESIAN_POINT ( 'NONE',  ( 16.33361799548379523, 1.482358050883964840E-15, 0.000000000000000000 ) ) ;
#579 = CARTESIAN_POINT ( 'NONE',  ( 16.80323065652739345, 43.42158355246869661, -6.657797401561860617 ) ) ;
#580 = CIRCLE ( 'NONE', #72902, 8.000000000000000000 ) ;
#581 = CARTESIAN_POINT ( 'NONE',  ( -2.026673642932869779, 21.31079249973476308, -6.703948387959501432 ) ) ;
#582 = CARTESIAN_POINT ( 'NONE',  ( -10.82254083843020531, -4.995738461561603394, -12.56441722558348140 ) ) ;
#583 = CARTESIAN_POINT ( 'NONE',  ( -30.00000000000000355, 461.8887775513398992, 11.55279652844095573 ) ) ;
#584 = CYLINDRICAL_SURFACE ( 'NONE', #102404, 9.000000000000000000 ) ;
#585 = CARTESIAN_POINT ( 'NONE',  ( -26.67480708604283990, 296.1445473584531669, -1.720936451573135129 ) ) ;
#586 = EDGE_CURVE ( 'NONE', #87574, #89053, #59103, .T. ) ;
#587 = CARTESIAN_POINT ( 'NONE',  ( 87.01147726110801273, -59.99999999999995737, -6.889873257858575961 ) ) ;
#588 = CARTESIAN_POINT ( 'NONE',  ( -33.42055755381959159, -49.90302826338683673, 36.47865937243805234 ) ) ;
#589 = FACE_OUTER_BOUND ( 'NONE', #76016, .T. ) ;
#590 = CARTESIAN_POINT ( 'NONE',  ( 45.25892614766976862, -18.78593732984838738, 38.35189378481528877 ) ) ;
#591 = ORIENTED_EDGE ( 'NONE', *, *, #38683, .F. ) ;
#592 = EDGE_CURVE ( 'NONE', #102339, #9659, #46179, .T. ) ;
#593 = CARTESIAN_POINT ( 'NONE',  ( 43.42366826522432177, 435.2488004288791217, 10.12833319149042310 ) ) ;
#594 = EDGE_CURVE ( 'NONE', #99282, #59690, #88439, .T. ) ;
#595 = CARTESIAN_POINT ( 'NONE',  ( -83.62175913889684864, -38.78254028569615741, 197.4759616008079206 ) ) ;
#596 = VERTEX_POINT ( 'NONE', #87383 ) ;
#597 = CARTESIAN_POINT ( 'NONE',  ( 29.50756122520733271, 297.9063904818165724, 10.61050061783298126 ) ) ;
#598 = CARTESIAN_POINT ( 'NONE',  ( -1.727368016638141196E-09, 38.95322581935191408, 63.66965480466880223 ) ) ;
#599 = CARTESIAN_POINT ( 'NONE',  ( 15.50560966020076847, 37.05331456527881784, 22.93063681418749766 ) ) ;
#600 = CARTESIAN_POINT ( 'NONE',  ( 30.00000000000000000, 500.0000000000002274, -12.00000000000000711 ) ) ;
#601 = DIRECTION ( 'NONE',  ( 0.000000000000000000, -1.000000000000000000, 0.000000000000000000 ) ) ;
#602 = FACE_BOUND ( 'NONE', #43188, .T. ) ;
#603 = CARTESIAN_POINT ( 'NONE',  ( -31.38880089262778483, 374.5722431920488589, 22.86451044521289333 ) ) ;
#604 = CARTESIAN_POINT ( 'NONE',  ( 16.72321626032220721, 45.57697876764353140, 6.657797401561558637 ) ) ;
#605 = EDGE_CURVE ( 'NONE', #80946, #83274, #40402, .T. ) ;
#606 = CARTESIAN_POINT ( 'NONE',  ( 101.6859781841139920, -60.00000000000000711, 90.91199205705245845 ) ) ;
#607 = CARTESIAN_POINT ( 'NONE',  ( 0.000000000000000000, -6.928203230275511437, -3.999999999999997335 ) ) ;
#608 =( GEOMETRIC_REPRESENTATION_CONTEXT ( 3 ) GLOBAL_UNCERTAINTY_ASSIGNED_CONTEXT ( ( #68853 ) ) GLOBAL_UNIT_ASSIGNED_CONTEXT ( ( #72048, #79605, #57431 ) ) REPRESENTATION_CONTEXT ( 'NONE', 'WORKASPACE' ) );
#609 = EDGE_CURVE ( 'NONE', #31239, #105636, #64688, .T. ) ;
#610 = SURFACE_SIDE_STYLE ('',( #91280 ) ) ;
#611 = ORIENTED_EDGE ( 'NONE', *, *, #54631, .T. ) ;
#612 = AXIS2_PLACEMENT_3D ( 'NONE', #25378, #80380, #57689 ) ;
#613 = CARTESIAN_POINT ( 'NONE',  ( -98.40393905160468080, -30.00000000000002132, 190.0006876441828751 ) ) ;
#614 = ORIENTED_EDGE ( 'NONE', *, *, #97880, .F. ) ;
#615 = FACE_OUTER_BOUND ( 'NONE', #63502, .T. ) ;
#616 = FACE_OUTER_BOUND ( 'NONE', #76040, .T. ) ;
#617 = CARTESIAN_POINT ( 'NONE',  ( 30.00647014684152580, 322.4127042974290021, 14.51058770105004392 ) ) ;
#618 = CARTESIAN_POINT ( 'NONE',  ( 10.00005432054556920, 25.99986419862086962, 0.2621623937322681286 ) ) ;
#619 = CARTESIAN_POINT ( 'NONE',  ( 7.188101187500001821, -16.43750000204838457, -2.977408999572650483 ) ) ;
#620 =( NAMED_UNIT ( * ) SI_UNIT ( $, .STERADIAN. ) SOLID_ANGLE_UNIT ( ) );
#621 = CARTESIAN_POINT ( 'NONE',  ( 87.62222222222222001, 4.172000000000019249, 0.000000000000000000 ) ) ;
#623 = ORIENTED_EDGE ( 'NONE', *, *, #98570, .T. ) ;
#622 = FACE_OUTER_BOUND ( 'NONE', #19692, .T. ) ;
#624 = CARTESIAN_POINT ( 'NONE',  ( 84.12715833974999668, -25.58911834355439652, 158.2829670055756139 ) ) ;
#625 = CARTESIAN_POINT ( 'NONE',  ( 14.27307692307692299, 4.172000000000003261, 0.000000000000000000 ) ) ;
#626 = CARTESIAN_POINT ( 'NONE',  ( 15.17407431220850533, 1.340359594676612611E-15, 0.000000000000000000 ) ) ;
#627 = ORIENTED_EDGE ( 'NONE', *, *, #74226, .F. ) ;
#628 = SURFACE_STYLE_FILL_AREA ( #82659 ) ;
#629 = CARTESIAN_POINT ( 'NONE',  ( -46.86921974295896121, 18.15560460139520416, 16.08157171274191199 ) ) ;
#630 = CARTESIAN_POINT ( 'NONE',  ( -5.082755093536325042, -9.593750002048384573, -5.082755093536325930 ) ) ;
#631 = CARTESIAN_POINT ( 'NONE',  ( 0.000000000000000000, 0.000000000000000000, 0.000000000000000000 ) ) ;
#632 = CARTESIAN_POINT ( 'NONE',  ( -3.823683356083669160, -59.99999999999998579, -36.85499309513409116 ) ) ;
#633 = CARTESIAN_POINT ( 'NONE',  ( 75.30000000000001137, 4.052968581778165278E-16, -3.309499999999999886 ) ) ;
#634 = B_SPLINE_SURFACE_WITH_KNOTS ( 'NONE', 1, 3, ( 
 ( #106536, #66085, #83328, #9421, #249, #49896, #49357, #42341 ),
 ( #82264, #8376, #15943, #41806, #25126, #98964, #74694, #75227 ) ),
 .UNSPECIFIED., .F., .F., .F.,
 ( 2, 2 ),
 ( 4, 2, 2, 4 ),
 ( 0.000000000000000000, 1.000000000000000000 ),
 ( 0.000000000000000000, 0.04450745600790868145, 0.06676118401186306728, 0.08901491201581737678 ),
 .UNSPECIFIED. ) ;
#635 = CARTESIAN_POINT ( 'NONE',  ( 7.770228158362351145, -1.925929944387235853E-31, 5.000000000000002665 ) ) ;
#636 = ORIENTED_EDGE ( 'NONE', *, *, #30453, .T. ) ;
#637 = ADVANCED_FACE ( 'NONE', ( #97560 ), #104603, .F. ) ;
#638 = COLOUR_RGB ( '', 0.40784314, 0.44705882, 0.49803922) ;
#639 = CARTESIAN_POINT ( 'NONE',  ( -1.176549540017828299, 302.5210282605368661, 9.930800019558532199 ) ) ;
#640 = CARTESIAN_POINT ( 'NONE',  ( 7.436486958462253050, 40.68079685609215801, -59.06589984255106174 ) ) ;
#641 = CARTESIAN_POINT ( 'NONE',  ( 86.90843919687902996, -31.72564875591590905, 187.1486806339965199 ) ) ;
#642 = EDGE_CURVE ( 'NONE', #44079, #54759, #31287, .T. ) ;
#643 = CARTESIAN_POINT ( 'NONE',  ( 0.5678805982759365101, 35.03118002593645741, -27.38332561059753090 ) ) ;
#644 = CARTESIAN_POINT ( 'NONE',  ( -5.082755093536325042, -33.59375000204838813, -5.082755093536325930 ) ) ;
#645 = CARTESIAN_POINT ( 'NONE',  ( 55.00000000000000000, 2.000000000000000000, 0.000000000000000000 ) ) ;
#646 = VECTOR ( 'NONE', #4565, 1000.000000000000000 ) ;
#647 = CARTESIAN_POINT ( 'NONE',  ( -14.58934900096693354, 5.487773041254725648, 6.668063844683933539 ) ) ;
#648 = EDGE_CURVE ( 'NONE', #57839, #9002, #34683, .T. ) ;
#649 = CARTESIAN_POINT ( 'NONE',  ( -19.50000000000000000, 12.99999999999999289, 0.000000000000000000 ) ) ;
#650 = VECTOR ( 'NONE', #38589, 999.9999999999998863 ) ;
#651 = ITEM_DEFINED_TRANSFORMATION ( 'NONE', 'NONE', #50667,  #10728 ) ;
#652 = CARTESIAN_POINT ( 'NONE',  ( 49.26018567526338643, 7.766323692793287492, 15.83099189872057622 ) ) ;
#653 = VERTEX_POINT ( 'NONE', #24257 ) ;
#654 = CARTESIAN_POINT ( 'NONE',  ( 0.6456527140175527535, 44.02049913527396541, 16.41655882843762981 ) ) ;
#655 = DIRECTION ( 'NONE',  ( 0.000000000000000000, 0.000000000000000000, 1.000000000000000000 ) ) ;
#656 = FACE_OUTER_BOUND ( 'NONE', #105852, .T. ) ;
#657 = ORIENTED_EDGE ( 'NONE', *, *, #20920, .F. ) ;
#658 = FACE_OUTER_BOUND ( 'NONE', #92742, .T. ) ;
#659 = FACE_OUTER_BOUND ( 'NONE', #11091, .T. ) ;
#660 = CARTESIAN_POINT ( 'NONE',  ( 111.8874950267952499, -57.67106131057807517, 191.6777584699202635 ) ) ;
#661 = EDGE_CURVE ( 'NONE', #96379, #38000, #97654, .T. ) ;
#662 = CARTESIAN_POINT ( 'NONE',  ( 35.05476482818301776, 463.5208552852830053, 19.69826870374934558 ) ) ;
#663 = CARTESIAN_POINT ( 'NONE',  ( 2.025576785233600852, 14.39373949114980178, 6.704368252951605989 ) ) ;
#664 = DIRECTION ( 'NONE',  ( 0.000000000000000000, 1.000000000000000000, 0.000000000000000000 ) ) ;
#665 = CARTESIAN_POINT ( 'NONE',  ( 16.04675029026778788, 302.5605073873273341, 9.875078446694708134 ) ) ;
#666 = CARTESIAN_POINT ( 'NONE',  ( -85.92822421211859307, -60.00000000000001421, 200.5408493071717544 ) ) ;
#667 = FACE_OUTER_BOUND ( 'NONE', #72152, .T. ) ;
#668 = SURFACE_STYLE_USAGE ( .BOTH. , #81606 ) ;
#669 = ADVANCED_FACE ( 'NONE', ( #964 ), #72098, .T. ) ;
#670 = CARTESIAN_POINT ( 'NONE',  ( -40.77380256327629837, 468.8478597483947965, 21.13608272249925690 ) ) ;
#671 = CARTESIAN_POINT ( 'NONE',  ( -86.40833561382129346, -17.71286793965802886, 176.2748628663870250 ) ) ;
#673 = VERTEX_POINT ( 'NONE', #17212 ) ;
#672 = STYLED_ITEM ( 'NONE', ( #57049 ), #18131 ) ;
#674 = CARTESIAN_POINT ( 'NONE',  ( 25.11756370350098422, 305.1043195247783615, -9.727872587232992529 ) ) ;
#675 =( BOUNDED_CURVE ( )  B_SPLINE_CURVE ( 2, ( #7646, #83148, #8722 ),
 .UNSPECIFIED., .F., .F. ) 
 B_SPLINE_CURVE_WITH_KNOTS ( ( 3, 3 ),
 ( 0.000000000000000000, 1.000000000000000000 ),
 .UNSPECIFIED. ) 
 CURVE ( )  GEOMETRIC_REPRESENTATION_ITEM ( )  RATIONAL_B_SPLINE_CURVE ( ( 1.000000000000000000, 1.857142857142858317, 1.000000000000000000 ) ) 
 REPRESENTATION_ITEM ( '' )  );
#676 = CIRCLE ( 'NONE', #59253, 0.5000000000000004441 ) ;
#677 = ORIENTED_EDGE ( 'NONE', *, *, #91818, .T. ) ;
#678 = CARTESIAN_POINT ( 'NONE',  ( 16.05785784214672773, 4.775831776474238843, 3.710403933782425057 ) ) ;
#679 =( LENGTH_UNIT ( ) NAMED_UNIT ( * ) SI_UNIT ( .MILLI., .METRE. ) );
#680 = COLOUR_RGB ( '', 0.09019608, 0.27058824, 0.51372549) ;
#681 = MECHANICAL_DESIGN_GEOMETRIC_PRESENTATION_REPRESENTATION (  '', ( #33473 ), #83255 ) ;
#682 = CARTESIAN_POINT ( 'NONE',  ( -83.23302758787693278, -37.79703903699630985, -5.212852745124933129 ) ) ;
#683 = CARTESIAN_POINT ( 'NONE',  ( -5.169066395376114897, -13.70246774098932541, -6.130298896215165882 ) ) ;
#684 = CARTESIAN_POINT ( 'NONE',  ( -15.72023223728087693, 43.84211828279115508, 6.254247239864763941 ) ) ;
#685 = DIRECTION ( 'NONE',  ( 1.000000000000000000, 1.224606353822377258E-16, 0.000000000000000000 ) ) ;
#686 = CARTESIAN_POINT ( 'NONE',  ( -33.85195725564126690, 465.2464970902066739, 17.18122764674263081 ) ) ;
#687 = CARTESIAN_POINT ( 'NONE',  ( 7.000000000000000000, -15.93202192939576634, -5.930487099830196840 ) ) ;
#688 = CARTESIAN_POINT ( 'NONE',  ( -43.02621584241282449, 434.6128289108255558, 16.97888786059002086 ) ) ;
#689 = CARTESIAN_POINT ( 'NONE',  ( -36.64823341582351901, 437.5392299810053487, 4.281405873620243163 ) ) ;
#690 = CARTESIAN_POINT ( 'NONE',  ( -47.47011933289886088, -14.21045842199439946, -33.05967481147064291 ) ) ;
#691 = CARTESIAN_POINT ( 'NONE',  ( -75.77454316836929138, -42.96621770076318825, 126.5407752095937326 ) ) ;
#692 = EDGE_LOOP ( 'NONE', ( #73594, #52506, #89356, #104672, #50248 ) ) ;
#693 = CARTESIAN_POINT ( 'NONE',  ( 67.17255777190595722, -60.00000000000001421, 138.9727001947898941 ) ) ;
#694 = DIRECTION ( 'NONE',  ( -1.000000000000000000, -1.224606353822377258E-16, -0.000000000000000000 ) ) ;
#695 = CARTESIAN_POINT ( 'NONE',  ( 114.0253014678331596, -57.67114145616815080, 179.0545312471846557 ) ) ;
#696 = VERTEX_POINT ( 'NONE', #75960 ) ;
#697 = CARTESIAN_POINT ( 'NONE',  ( 8.181629489174529368, -12.25161225291834377, 8.655449601632003720 ) ) ;
#698 = FACE_BOUND ( 'NONE', #50405, .T. ) ;
#699 = VERTEX_POINT ( 'NONE', #90019 ) ;
#700 = CARTESIAN_POINT ( 'NONE',  ( -29.68315524076956891, -1.200000000000000030E-05, 40.85535821593508388 ) ) ;
#701 = SURFACE_STYLE_FILL_AREA ( #18011 ) ;
#702 = FACE_OUTER_BOUND ( 'NONE', #86765, .T. ) ;
#703 = CARTESIAN_POINT ( 'NONE',  ( 7.188101187499999156, -10.25000000204838813, 2.977408999572654924 ) ) ;
#704 = DIRECTION ( 'NONE',  ( -0.02876443885984900778, -0.9995862179207344322, 0.000000000000000000 ) ) ;
#705 = DIRECTION ( 'NONE',  ( 0.000000000000000000, 0.000000000000000000, 1.000000000000000000 ) ) ;
#706 = CARTESIAN_POINT ( 'NONE',  ( 6.643884894376897776, 3.901062859471661870, -6.756839076126022192 ) ) ;
#707 = LINE ( 'NONE', #50883, #95053 ) ;
#708 = CARTESIAN_POINT ( 'NONE',  ( -7.897827455343210623, -1.533134349199915647, -7.633632140068263183 ) ) ;
#709 =( LENGTH_UNIT ( ) NAMED_UNIT ( * ) SI_UNIT ( .MILLI., .METRE. ) );
#710 = EDGE_CURVE ( 'NONE', #67680, #74647, #10178, .T. ) ;
#711 = AXIS2_PLACEMENT_3D ( 'NONE', #65376, #24423, #49168 ) ;
#712 = VERTEX_POINT ( 'NONE', #58176 ) ;
#713 = CARTESIAN_POINT ( 'NONE',  ( -6.930184079356135562, 41.27136532024966442, -70.62329956115780760 ) ) ;
#715 = CARTESIAN_POINT ( 'NONE',  ( 29.11974998906863377, -25.58802340656078655, 30.36905162638436906 ) ) ;
#714 =( LENGTH_UNIT ( ) NAMED_UNIT ( * ) SI_UNIT ( .MILLI., .METRE. ) );
#716 = CARTESIAN_POINT ( 'NONE',  ( -5.290067270632269114, 51.34639538792298907, -8.531152949374520844 ) ) ;
#717 = VERTEX_POINT ( 'NONE', #24779 ) ;
#718 = EDGE_CURVE ( 'NONE', #102768, #42192, #99703, .T. ) ;
#719 = PRESENTATION_STYLE_ASSIGNMENT (( #26673 ) ) ;
#720 = EDGE_CURVE ( 'NONE', #58013, #63799, #70749, .T. ) ;
#721 = ORIENTED_EDGE ( 'NONE', *, *, #58191, .T. ) ;
#723 = CARTESIAN_POINT ( 'NONE',  ( -2.583889972062225482, -5.000000000000000000, -9.742892617411701650 ) ) ;
#722 = DIRECTION ( 'NONE',  ( 0.8191520442889881348, 0.000000000000000000, 0.5735764363510513775 ) ) ;
#724 = CARTESIAN_POINT ( 'NONE',  ( -4.871453668401689791E-08, -12.57758911513053413, 32.18678843846154081 ) ) ;
#725 = DIRECTION ( 'NONE',  ( 0.000000000000000000, 0.000000000000000000, 1.000000000000000000 ) ) ;
#726 = AXIS2_PLACEMENT_3D ( 'NONE', #94977, #36763, #4887 ) ;
#727 = CIRCLE ( 'NONE', #54110, 10.00000000000000000 ) ;
#728 = CARTESIAN_POINT ( 'NONE',  ( -5.079411765174640436, 41.99999999999998579, -70.14437560653188086 ) ) ;
#729 = CARTESIAN_POINT ( 'NONE',  ( 0.6415787021996353090, 46.14597056523812313, 16.42407206998221980 ) ) ;
#730 = CARTESIAN_POINT ( 'NONE',  ( -35.63058582597223278, 464.1921406587270553, 19.33089630041828855 ) ) ;
#731 = EDGE_LOOP ( 'NONE', ( #16688, #7338, #6417, #75018, #97240 ) ) ;
#732 = CARTESIAN_POINT ( 'NONE',  ( 92.74300446008587073, -59.99999999999999289, -7.104999719762539634 ) ) ;
#733 = CARTESIAN_POINT ( 'NONE',  ( -11.54075930460758670, 45.44590361214168439, -14.27956357151539102 ) ) ;
#734 = CIRCLE ( 'NONE', #59380, 5.000000000000001776 ) ;
#735 = CARTESIAN_POINT ( 'NONE',  ( 30.00000000000000355, 462.0097303356241127, 12.67201001740816579 ) ) ;
#736 = EDGE_CURVE ( 'NONE', #77337, #18, #99663, .T. ) ;
#737 = CARTESIAN_POINT ( 'NONE',  ( 13.76424046522695122, 304.5457540960956067, -10.06505265514019243 ) ) ;
#738 = CARTESIAN_POINT ( 'NONE',  ( -47.24255575150520059, 16.92138162734892148, -16.58509488952817179 ) ) ;
#739 = ORIENTED_EDGE ( 'NONE', *, *, #66044, .F. ) ;
#740 = DIRECTION ( 'NONE',  ( 1.000000000000000000, 1.224606353822377258E-16, 0.000000000000000000 ) ) ;
#741 = VERTEX_POINT ( 'NONE', #18284 ) ;
#742 = ORIENTED_EDGE ( 'NONE', *, *, #53663, .T. ) ;
#743 = CARTESIAN_POINT ( 'NONE',  ( 33.72905809600513294, 464.0430918388264558, 18.49991514059003705 ) ) ;
#744 = CARTESIAN_POINT ( 'NONE',  ( 0.1061556211655322601, 4.836380039389416297, -4.623144047065555817 ) ) ;
#745 = SURFACE_STYLE_FILL_AREA ( #27776 ) ;
#746 = CARTESIAN_POINT ( 'NONE',  ( 84.47252406500750510, -45.28770036745071081, -5.144395108280352069 ) ) ;
#747 = CARTESIAN_POINT ( 'NONE',  ( -39.13914184472998414, 311.4509987364423864, 1.958682826505325325 ) ) ;
#748 = CARTESIAN_POINT ( 'NONE',  ( -20.21880305278364887, 304.8280059657581091, -9.005058168222342729 ) ) ;
#749 = DIRECTION ( 'NONE',  ( 0.000000000000000000, 0.000000000000000000, 1.000000000000000000 ) ) ;
#750 = ORIENTED_EDGE ( 'NONE', *, *, #45410, .T. ) ;
#751 = CARTESIAN_POINT ( 'NONE',  ( 29.77184624873680718, 12.99572234387825276, 39.60535821593452255 ) ) ;
#752 = ORIENTED_EDGE ( 'NONE', *, *, #96773, .F. ) ;
#753 = CARTESIAN_POINT ( 'NONE',  ( 6.936184427528457874, 1.053834543709838281E-15, 8.605212085995399107 ) ) ;
#755 = ORIENTED_EDGE ( 'NONE', *, *, #93443, .F. ) ;
#754 = CARTESIAN_POINT ( 'NONE',  ( 5.911454136186996777, 51.88613318027746857, 6.184812069074881791 ) ) ;
#756 = CARTESIAN_POINT ( 'NONE',  ( 66.93286271214273597, -25.57999363339980192, 84.51815215314977081 ) ) ;
#757 = COLOUR_RGB ( '', 0.09019608, 0.27058824, 0.51372549) ;
#758 = ORIENTED_EDGE ( 'NONE', *, *, #923, .T. ) ;
#759 = CARTESIAN_POINT ( 'NONE',  ( 62.01418705507710172, 38.95383793061004951, -16.66584972139569487 ) ) ;
#760 = CARTESIAN_POINT ( 'NONE',  ( -7.188101187500002709, -22.81250000204838813, 2.977408999572647819 ) ) ;
#761 = AXIS2_PLACEMENT_3D ( 'NONE', #98178, #38386, #104146 ) ;
#762 = CARTESIAN_POINT ( 'NONE',  ( -113.9839795500101332, -57.67115229137139210, 179.6907882865009185 ) ) ;
#763 = STYLED_ITEM ( 'NONE', ( #7839 ), #82029 ) ;
#765 = ORIENTED_EDGE ( 'NONE', *, *, #69858, .F. ) ;
#764 = COLOUR_RGB ( '', 0.31764706, 0.68627451, 0.89019608) ;
#766 = CARTESIAN_POINT ( 'NONE',  ( 6.683837171061809634, -7.911893696991943337, -3.558927330633863411E-17 ) ) ;
#767 = CARTESIAN_POINT ( 'NONE',  ( 106.5260298931462160, -60.15149297030401243, 172.9218580926358584 ) ) ;
#768 = CARTESIAN_POINT ( 'NONE',  ( 5.290067270632160756, 52.08006895350504806, -6.031152949374595451 ) ) ;
#769 = EDGE_CURVE ( 'NONE', #67191, #31789, #46307, .T. ) ;
#770 = CARTESIAN_POINT ( 'NONE',  ( -10.00000000000000178, 15.00000000000000000, 1.734723475976807489E-15 ) ) ;
#771 = CARTESIAN_POINT ( 'NONE',  ( 5.656854249492380582, -23.00000000409677270, -5.656854249492379694 ) ) ;
#772 = LINE ( 'NONE', #67688, #12340 ) ;
#773 = CARTESIAN_POINT ( 'NONE',  ( 33.67444716837086105, 489.3309112354449439, 10.55021651976763586 ) ) ;
#774 = DIRECTION ( 'NONE',  ( -0.000000000000000000, -0.000000000000000000, -1.000000000000000000 ) ) ;
#775 = CARTESIAN_POINT ( 'NONE',  ( 9.646032546913145822, 33.01280328474367565, 2.644051433538245011 ) ) ;
#776 = DIRECTION ( 'NONE',  ( 0.000000000000000000, 0.000000000000000000, 1.000000000000000000 ) ) ;
#777 = DIRECTION ( 'NONE',  ( 0.000000000000000000, 0.2649831162830741382, 0.9642530518929723904 ) ) ;
#778 = CARTESIAN_POINT ( 'NONE',  ( -3.420980250011399715, -30.00000000000000355, -7.222355033959453330 ) ) ;
#779 = ORIENTED_EDGE ( 'NONE', *, *, #7201, .F. ) ;
#780 = DIRECTION ( 'NONE',  ( 0.5735764363510554853, 0.8191520442889852482, 0.000000000000000000 ) ) ;
#781 = CARTESIAN_POINT ( 'NONE',  ( 8.568842943812819968, -60.00000000000002132, 39.63676292489870434 ) ) ;
#782 = CARTESIAN_POINT ( 'NONE',  ( -95.46185265749743110, -30.00000000000000000, 191.3287857896271191 ) ) ;
#783 = EDGE_CURVE ( 'NONE', #2324, #36626, #35973, .T. ) ;
#784 = CIRCLE ( 'NONE', #57622, 5.000000000000000000 ) ;
#785 = ORIENTED_EDGE ( 'NONE', *, *, #53839, .F. ) ;
#786 = LINE ( 'NONE', #100056, #81311 ) ;
#787 = CARTESIAN_POINT ( 'NONE',  ( 66.29758781432747128, -57.68034428469994879, 132.1174182233373813 ) ) ;
#788 = CARTESIAN_POINT ( 'NONE',  ( -8.628857352971980532, 6.504966632935141213, 3.765103137054122584 ) ) ;
#789 = CARTESIAN_POINT ( 'NONE',  ( 6.955314659475122951, -21.96029575818983304, -38.54528801990171161 ) ) ;
#790 = STYLED_ITEM ( 'NONE', ( #43828 ), #87638 ) ;
#791 = CARTESIAN_POINT ( 'NONE',  ( -43.74985542820358830, 435.5770091380367717, 16.96136490515571182 ) ) ;
#792 = CARTESIAN_POINT ( 'NONE',  ( -41.32172643392373601, -59.99999999999997868, 54.07094069856850638 ) ) ;
#793 = CIRCLE ( 'NONE', #40490, 2.000000000000000000 ) ;
#794 = AXIS2_PLACEMENT_3D ( 'NONE', #54164, #55232, #13714 ) ;
#795 = CONICAL_SURFACE ( 'NONE', #45601, 4.000000000000001776, 0.9599310885968808105 ) ;
#796 = CARTESIAN_POINT ( 'NONE',  ( 42.09158233638500235, 465.7816406625409513, 14.79318349170030089 ) ) ;
#797 = EDGE_CURVE ( 'NONE', #94943, #52640, #39408, .T. ) ;
#798 = CARTESIAN_POINT ( 'NONE',  ( 36.53813723230013011, 463.3027015936760336, 20.13340496300989813 ) ) ;
#799 = CIRCLE ( 'NONE', #38817, 5.000000000000010658 ) ;
#800 = CARTESIAN_POINT ( 'NONE',  ( -86.86786266847680338, -50.11060889839860977, 191.7888452930998255 ) ) ;
#801 = ORIENTED_EDGE ( 'NONE', *, *, #81569, .F. ) ;
#802 = CARTESIAN_POINT ( 'NONE',  ( 3.313708498984762496, -12.78124999999999467, 7.999999999999998224 ) ) ;
#803 = CARTESIAN_POINT ( 'NONE',  ( -10.33879959434646700, -46.43938644275853278, 31.64223682635364199 ) ) ;
#804 = AXIS2_PLACEMENT_3D ( 'NONE', #25250, #74290, #100690 ) ;
#805 = CARTESIAN_POINT ( 'NONE',  ( -5.902962327514317487, 41.87327319969161010, -59.02279321040224147 ) ) ;
#806 = CARTESIAN_POINT ( 'NONE',  ( 42.20041562234358423, 435.2369744135583574, 7.788607701745475786 ) ) ;
#807 = EDGE_CURVE ( 'NONE', #32720, #23780, #96223, .T. ) ;
#809 = CARTESIAN_POINT ( 'NONE',  ( 4.254610347505312973, -66.83165319588984232, 13.14363822686244099 ) ) ;
#808 = DIRECTION ( 'NONE',  ( -1.000000000000000000, 0.000000000000000000, 0.000000000000000000 ) ) ;
#810 = ORIENTED_EDGE ( 'NONE', *, *, #86547, .F. ) ;
#811 = FACE_BOUND ( 'NONE', #67326, .T. ) ;
#812 = CARTESIAN_POINT ( 'NONE',  ( -6.797507374398395363, -5.000000000000177636, -15.30989363317748619 ) ) ;
#813 = CARTESIAN_POINT ( 'NONE',  ( -6.943482370013978944, 30.52848370260725019, 3.973876482044365499 ) ) ;
#814 = CARTESIAN_POINT ( 'NONE',  ( 34.70677891788760405, 301.1180127857406887, -8.590837488028862268 ) ) ;
#815 = DIRECTION ( 'NONE',  ( 0.000000000000000000, 0.000000000000000000, 1.000000000000000000 ) ) ;
#816 = SURFACE_STYLE_USAGE ( .BOTH. , #48859 ) ;
#817 = SURFACE_STYLE_USAGE ( .BOTH. , #99003 ) ;
#818 = CARTESIAN_POINT ( 'NONE',  ( 109.5811936024938120, -29.99999999999993250, 174.3369879458943217 ) ) ;
#819 = EDGE_LOOP ( 'NONE', ( #7919, #30918, #47841, #33303 ) ) ;
#820 = DIRECTION ( 'NONE',  ( 1.000000000000000000, 0.000000000000000000, 0.000000000000000000 ) ) ;
#821 = CARTESIAN_POINT ( 'NONE',  ( -9.482993638194566088, 252.4434872025367440, -3.177441187500450681 ) ) ;
#822 = CARTESIAN_POINT ( 'NONE',  ( -3.313708498984726969, -20.65625000409677625, 8.000000000000039080 ) ) ;
#823 = CARTESIAN_POINT ( 'NONE',  ( -5.274401269815139237, -6.074457022762095093, -7.633824513837116577 ) ) ;
#824 = CARTESIAN_POINT ( 'NONE',  ( 37.71418762737119579, 397.5201552014418667, 6.419224431681028520 ) ) ;
#825 = DIRECTION ( 'NONE',  ( -1.000000000000000000, 0.000000000000000000, 0.000000000000000000 ) ) ;
#826 = VERTEX_POINT ( 'NONE', #2592 ) ;
#827 = UNCERTAINTY_MEASURE_WITH_UNIT (LENGTH_MEASURE( 1.000000000000000082E-05 ), #38778, 'distance_accuracy_value', 'NONE');
#828 = FACE_OUTER_BOUND ( 'NONE', #105672, .T. ) ;
#829 = EDGE_LOOP ( 'NONE', ( #39657, #74387, #10029, #30615 ) ) ;
#830 = CARTESIAN_POINT ( 'NONE',  ( 3.400000000000000355, 0.000000000000000000, -2.716724522925831220 ) ) ;
#831 = CIRCLE ( 'NONE', #81768, 5.000000000000002665 ) ;
#832 = CARTESIAN_POINT ( 'NONE',  ( 9.067083174484489305, 46.09712060844260151, 13.87005886985717673 ) ) ;
#833 = PRODUCT_DEFINITION_FORMATION_WITH_SPECIFIED_SOURCE ( 'ANY', '', #3601, .NOT_KNOWN. ) ;
#834 = CARTESIAN_POINT ( 'NONE',  ( -62.59524157943269529, 48.00000000000000000, 18.50207713769755102 ) ) ;
#835 = CARTESIAN_POINT ( 'NONE',  ( 5.000000000000000888, -15.62228920881127081, 13.86359191440427807 ) ) ;
#836 = CARTESIAN_POINT ( 'NONE',  ( 44.33486631614394469, 435.2047139628968466, 12.56860447607852294 ) ) ;
#837 = ORIENTED_EDGE ( 'NONE', *, *, #76816, .T. ) ;
#838 = CARTESIAN_POINT ( 'NONE',  ( 104.5071319395805176, -60.00000000000001421, 199.6225049996390055 ) ) ;
#840 = CARTESIAN_POINT ( 'NONE',  ( 19.17772706616747769, -46.43459562844415700, 32.07223590092135623 ) ) ;
#839 = CARTESIAN_POINT ( 'NONE',  ( -91.09862910994078788, -14.21045842199425380, 197.8399937059591309 ) ) ;
#841 = CARTESIAN_POINT ( 'NONE',  ( 35.03266379445575751, 463.2767948149638073, 4.632316356192585971 ) ) ;
#842 = CARTESIAN_POINT ( 'NONE',  ( 37.71426591916371507, 395.7719197107890068, 6.364421788594514240 ) ) ;
#843 = CARTESIAN_POINT ( 'NONE',  ( -41.58646596321217004, -49.89193559009187595, 42.49270283408452542 ) ) ;
#844 = CARTESIAN_POINT ( 'NONE',  ( -34.12287332558172892, 18.64284798593243409, -17.67912453245623539 ) ) ;
#845 = ORIENTED_EDGE ( 'NONE', *, *, #101069, .T. ) ;
#846 = DIRECTION ( 'NONE',  ( -0.000000000000000000, -1.000000000000000000, -0.000000000000000000 ) ) ;
#847 = CARTESIAN_POINT ( 'NONE',  ( 6.063014363552462704, -12.44085613821209080, 12.46297707981380753 ) ) ;
#848 = DIRECTION ( 'NONE',  ( 0.000000000000000000, 1.000000000000000000, 0.000000000000000000 ) ) ;
#849 = CARTESIAN_POINT ( 'NONE',  ( 6.326592304916277776, 6.579439845142157850, 2.267162479624766025 ) ) ;
#850 = FACE_OUTER_BOUND ( 'NONE', #64159, .T. ) ;
#851 = EDGE_LOOP ( 'NONE', ( #68969, #20502, #6587, #6206, #66955 ) ) ;
#852 =( NAMED_UNIT ( * ) PLANE_ANGLE_UNIT ( ) SI_UNIT ( $, .RADIAN. ) );
#853 = CARTESIAN_POINT ( 'NONE',  ( 0.000000000000000000, 303.8518027762758038, -10.00000000000000355 ) ) ;
#854 = ORIENTED_EDGE ( 'NONE', *, *, #81130, .F. ) ;
#856 = AXIS2_PLACEMENT_3D ( 'NONE', #13280, #12756, #60808 ) ;
#855 = B_SPLINE_CURVE_WITH_KNOTS ( 'NONE', 3,
 ( #24973, #88624, #72434, #57824, #98304, #72948, #40595, #56218, #22856, #16316 ),
 .UNSPECIFIED., .F., .F.,
 ( 4, 2, 2, 2, 4 ),
 ( 0.000000000000000000, 0.2500000000000000000, 0.5000000000000000000, 0.7500000000000000000, 1.000000000000000000 ),
 .UNSPECIFIED. ) ;
#857 = CARTESIAN_POINT ( 'NONE',  ( 75.18194444360641171, -30.00000000000002132, -17.88826170105039992 ) ) ;
#858 = CARTESIAN_POINT ( 'NONE',  ( 18.35767182829701838, 41.91122692137232519, -81.93709609102950253 ) ) ;
#859 = DIRECTION ( 'NONE',  ( -1.000000000000000000, -1.224606353822377258E-16, -0.000000000000000000 ) ) ;
#861 = EDGE_CURVE ( 'NONE', #65010, #9732, #84119, .T. ) ;
#860 = DIRECTION ( 'NONE',  ( -1.000000000000000000, -1.224606353822377258E-16, -0.000000000000000000 ) ) ;
#862 = CARTESIAN_POINT ( 'NONE',  ( 81.15738970259414486, -30.00000000000000000, 23.70005024620699885 ) ) ;
#863 = EDGE_CURVE ( 'NONE', #34518, #96063, #84597, .T. ) ;
#864 = CARTESIAN_POINT ( 'NONE',  ( 7.343637806710344051, 102.5563687809938074, 3.177475076494674866 ) ) ;
#865 = ORIENTED_EDGE ( 'NONE', *, *, #22367, .T. ) ;
#866 = VERTEX_POINT ( 'NONE', #68417 ) ;
#867 = ORIENTED_EDGE ( 'NONE', *, *, #87061, .F. ) ;
#868 = CARTESIAN_POINT ( 'NONE',  ( -33.80022934467059059, 484.1533297400397373, 1.810399503707904589 ) ) ;
#869 = CARTESIAN_POINT ( 'NONE',  ( -6.457005523775564804, 41.52802923939503899, -70.63630686657118929 ) ) ;
#870 = DIRECTION ( 'NONE',  ( 0.000000000000000000, 1.000000000000000000, 0.000000000000000000 ) ) ;
#871 = CONICAL_SURFACE ( 'NONE', #93935, 4.000000000000001776, 0.9599310885968808105 ) ;
#872 = CARTESIAN_POINT ( 'NONE',  ( -40.04067698533295783, 464.2438039439664976, 17.93195299062574932 ) ) ;
#873 = CARTESIAN_POINT ( 'NONE',  ( -30.72334302712536669, 348.3322246599395271, 19.95789250412614990 ) ) ;
#874 = CARTESIAN_POINT ( 'NONE',  ( 55.74444444444444713, 6.915964383211875250E-15, 0.000000000000000000 ) ) ;
#875 = EDGE_LOOP ( 'NONE', ( #30568, #3242, #63435, #105804, #87512, #94154 ) ) ;
#876 = VERTEX_POINT ( 'NONE', #36085 ) ;
#877 = LINE ( 'NONE', #32789, #58739 ) ;
#878 = CARTESIAN_POINT ( 'NONE',  ( 73.95169229206069872, -38.32650620814214903, 159.8841706720717468 ) ) ;
#879 = CARTESIAN_POINT ( 'NONE',  ( 6.585468679846623985, 7.640532685286893333, 0.2337908078075569274 ) ) ;
#880 =( GEOMETRIC_REPRESENTATION_CONTEXT ( 3 ) GLOBAL_UNCERTAINTY_ASSIGNED_CONTEXT ( ( #60618 ) ) GLOBAL_UNIT_ASSIGNED_CONTEXT ( ( #97027, #23168, #81358 ) ) REPRESENTATION_CONTEXT ( 'NONE', 'WORKASPACE' ) );
#881 = CIRCLE ( 'NONE', #32044, 5.000000000000010658 ) ;
#882 = CARTESIAN_POINT ( 'NONE',  ( 25.54696085151078933, 305.0816729924750916, 10.43539182524720843 ) ) ;
#883 = AXIS2_PLACEMENT_3D ( 'NONE', #55097, #96645, #4442 ) ;
#884 = VECTOR ( 'NONE', #9584, 1000.000000000000000 ) ;
#885 = AXIS2_PLACEMENT_3D ( 'NONE', #85043, #45132, #44050 ) ;
#886 = AXIS2_PLACEMENT_3D ( 'NONE', #53992, #45408, #3879 ) ;
#887 = CARTESIAN_POINT ( 'NONE',  ( -40.87544524660236078, 460.0150911311831692, 2.035358705197947149 ) ) ;
#888 = FACE_OUTER_BOUND ( 'NONE', #42515, .T. ) ;
#889 = DIRECTION ( 'NONE',  ( 0.000000000000000000, -1.000000000000000000, 0.000000000000000000 ) ) ;
#890 = FACE_OUTER_BOUND ( 'NONE', #71798, .T. ) ;
#891 = EDGE_LOOP ( 'NONE', ( #92580, #59792, #70176, #70030 ) ) ;
#892 = DIRECTION ( 'NONE',  ( 0.000000000000000000, 0.000000000000000000, 1.000000000000000000 ) ) ;
#893 = FILL_AREA_STYLE ('',( #24711 ) ) ;
#894 = UNCERTAINTY_MEASURE_WITH_UNIT (LENGTH_MEASURE( 1.000000000000000082E-05 ), #12427, 'distance_accuracy_value', 'NONE');
#895 = CARTESIAN_POINT ( 'NONE',  ( -46.00000000000000000, 438.3878896346936358, 16.22878885428542262 ) ) ;
#896 = CARTESIAN_POINT ( 'NONE',  ( 4.898587196589412829E-16, -10.62499999999999289, -8.000000000000000000 ) ) ;
#897 = CARTESIAN_POINT ( 'NONE',  ( 34.13897275414642962, 489.1603865319385704, 11.37941925723742997 ) ) ;
#898 = DIRECTION ( 'NONE',  ( 1.000000000000000000, 1.224606353822377258E-16, 0.000000000000000000 ) ) ;
#899 = EDGE_CURVE ( 'NONE', #9931, #76623, #63269, .T. ) ;
#900 = CARTESIAN_POINT ( 'NONE',  ( 36.84999999999999432, 3.309500000000003439, 4.052968581778167743E-16 ) ) ;
#901 = CARTESIAN_POINT ( 'NONE',  ( 85.35156438166434612, -42.92490405308009827, 186.7151393938520130 ) ) ;
#902 = DIRECTION ( 'NONE',  ( -0.000000000000000000, 1.000000000000000000, -0.000000000000000000 ) ) ;
#903 = DIRECTION ( 'NONE',  ( 0.000000000000000000, 0.000000000000000000, 1.000000000000000000 ) ) ;
#904 = ORIENTED_EDGE ( 'NONE', *, *, #62879, .F. ) ;
#905 = CARTESIAN_POINT ( 'NONE',  ( 93.45479798572706898, -57.65424997624518966, -16.00303676217793836 ) ) ;
#906 = CARTESIAN_POINT ( 'NONE',  ( 28.86650669486618881, 1.474610560812782335E-15, 0.000000000000000000 ) ) ;
#907 = CARTESIAN_POINT ( 'NONE',  ( 15.98683276757948235, 34.48651532721294188, -24.05821932099534521 ) ) ;
#908 = CARTESIAN_POINT ( 'NONE',  ( 0.4033376246892471650, 4.059728990630802947, 5.968343123267131567 ) ) ;
#909 = CARTESIAN_POINT ( 'NONE',  ( -80.98777655177451607, -30.00000000000000000, 4.227689634766996996 ) ) ;
#910 = EDGE_CURVE ( 'NONE', #58651, #47940, #97897, .T. ) ;
#911 = DIRECTION ( 'NONE',  ( 0.000000000000000000, 0.000000000000000000, 1.000000000000000000 ) ) ;
#912 = CARTESIAN_POINT ( 'NONE',  ( -3.313708498984774042, -29.65625000409676559, 7.999999999999988454 ) ) ;
#913 = CARTESIAN_POINT ( 'NONE',  ( -5.112021521198779617, 5.708827036477108763, -7.069802615102034338 ) ) ;
#915 = CARTESIAN_POINT ( 'NONE',  ( 0.4973051450610691537, -3.866309095671421669, -8.000000000000001776 ) ) ;
#914 = CARTESIAN_POINT ( 'NONE',  ( 4.284822031654949015, -48.90716638558772900, 104.4267991316944943 ) ) ;
#916 = CARTESIAN_POINT ( 'NONE',  ( 2.500000000000002220, -8.000000000000000000, -14.79019945774903988 ) ) ;
#917 = CARTESIAN_POINT ( 'NONE',  ( -31.43600694729765976, 438.9210571544146546, 23.14859716537183942 ) ) ;
#918 = CARTESIAN_POINT ( 'NONE',  ( -12.50000000000000711, -3.000000000000000000, -80.60844091781802945 ) ) ;
#919 = CARTESIAN_POINT ( 'NONE',  ( 4.903871675326606727, -82.97914192698505076, -3.461400506969855684 ) ) ;
#920 = CARTESIAN_POINT ( 'NONE',  ( -55.38798599899330810, -36.77553162784465002, -26.88172734773499428 ) ) ;
#921 = FACE_OUTER_BOUND ( 'NONE', #71190, .T. ) ;
#922 = DIRECTION ( 'NONE',  ( -1.000000000000000000, -1.224606353822377258E-16, -0.000000000000000000 ) ) ;
#923 = EDGE_CURVE ( 'NONE', #74471, #5652, #82172, .T. ) ;
#924 = ORIENTED_EDGE ( 'NONE', *, *, #39644, .F. ) ;
#925 = DIRECTION ( 'NONE',  ( 0.5735764363510466035, -0.8191520442889914655, 1.003171929053524500E-16 ) ) ;
#926 = SURFACE_STYLE_FILL_AREA ( #48971 ) ;
#927 = CARTESIAN_POINT ( 'NONE',  ( -7.212994264445058867, 82.98288655659960966, 3.463766307298584035 ) ) ;
#928 = CARTESIAN_POINT ( 'NONE',  ( -47.39373218408801591, -26.88155139983819453, -28.62974718684898434 ) ) ;
#929 = ADVANCED_FACE ( 'NONE', ( #69999, #102900, #43595, #61934, #36611 ), #42767, .F. ) ;
#931 = DIRECTION ( 'NONE',  ( 0.000000000000000000, -1.000000000000000000, 0.000000000000000000 ) ) ;
#930 = DIRECTION ( 'NONE',  ( 0.000000000000000000, 0.000000000000000000, 1.000000000000000000 ) ) ;
#932 = CIRCLE ( 'NONE', #49162, 4.000000000000001776 ) ;
#933 = ORIENTED_EDGE ( 'NONE', *, *, #61001, .T. ) ;
#934 = B_SPLINE_CURVE_WITH_KNOTS ( 'NONE', 3,
 ( #24452, #57285, #25512, #81035, #90207, #31991, #16307, #49199, #58367, #82099, #49739, #41127, #83174, #82648, #74011, #74541, #72940, #618, #15251, #91288, #9272, #64866, #72427, #56212, #64357, #7151, #59997, #100950, #27645, #42179, #43254, #34665, #17930, #44318 ),
 .UNSPECIFIED., .F., .F.,
 ( 4, 2, 2, 2, 2, 2, 2, 2, 2, 2, 2, 2, 2, 2, 2, 2, 4 ),
 ( 0.000000000000000000, 0.0007899309203816044745, 0.001579861840763208949, 0.002369792761144813315, 0.003159723681526417898, 0.003949654601908022047, 0.004739585522289626630, 0.005529516442671232081, 0.006319447363052837531, 0.007109378283434441247, 0.007899309203816045830, 0.008689240124197651280, 0.009479171044579254995, 0.01026910196496085871, 0.01105903288534246416, 0.01184896380572406788, 0.01263889472610567159 ),
 .UNSPECIFIED. ) ;
#935 = FILL_AREA_STYLE ('',( #31397 ) ) ;
#936 = ORIENTED_EDGE ( 'NONE', *, *, #34599, .F. ) ;
#937 = CARTESIAN_POINT ( 'NONE',  ( -26.11140572328752540, 35.05551467058084114, 8.044021159044859814 ) ) ;
#938 = CARTESIAN_POINT ( 'NONE',  ( 40.69624510163547626, 490.1121057833303212, 11.28177269626871571 ) ) ;
#939 = DIRECTION ( 'NONE',  ( 0.000000000000000000, 0.000000000000000000, 1.000000000000000000 ) ) ;
#940 = CIRCLE ( 'NONE', #85382, 8.000000000000000000 ) ;
#941 = CARTESIAN_POINT ( 'NONE',  ( -88.00960923584342765, -60.00000000000001421, -21.57056747520839224 ) ) ;
#942 = VERTEX_POINT ( 'NONE', #37673 ) ;
#943 = CARTESIAN_POINT ( 'NONE',  ( 0.9999999999999956701, -46.00000000000000000, 40.07669683062201926 ) ) ;
#944 = AXIS2_PLACEMENT_3D ( 'NONE', #49176, #25494, #74522 ) ;
#945 = CARTESIAN_POINT ( 'NONE',  ( 15.19395690307707802, 3.423339800906996633, -3.910915912796353311 ) ) ;
#946 = CIRCLE ( 'NONE', #7833, 3.309500000000001663 ) ;
#947 = CARTESIAN_POINT ( 'NONE',  ( 100.6323957723895859, -45.27888482481586152, 191.8799519755351071 ) ) ;
#948 = CIRCLE ( 'NONE', #42338, 5.000000000000010658 ) ;
#950 = CARTESIAN_POINT ( 'NONE',  ( 0.000000000000000000, 81.00000000000000000, -7.000000000000006217 ) ) ;
#949 = CARTESIAN_POINT ( 'NONE',  ( 16.75187969033571989, -1.200000000000000030E-05, 23.05698433968582961 ) ) ;
#951 = ORIENTED_EDGE ( 'NONE', *, *, #67576, .F. ) ;
#952 = ORIENTED_EDGE ( 'NONE', *, *, #4809, .T. ) ;
#953 = AXIS2_PLACEMENT_3D ( 'NONE', #83715, #26602, #27131 ) ;
#954 = ORIENTED_EDGE ( 'NONE', *, *, #59257, .T. ) ;
#955 = CARTESIAN_POINT ( 'NONE',  ( 31.44965036685163540, 392.5242412485162617, 24.22331400455512807 ) ) ;
#956 = CARTESIAN_POINT ( 'NONE',  ( -1.469576158976823947E-15, -27.87499999999999645, 8.000000000000000000 ) ) ;
#957 = CARTESIAN_POINT ( 'NONE',  ( 9.500000000000005329, -5.000000000000000000, -52.94236561372726868 ) ) ;
#958 = VERTEX_POINT ( 'NONE', #86733 ) ;
#959 = CARTESIAN_POINT ( 'NONE',  ( 15.39894322001505955, 46.20524723896237163, -5.264004132386357782 ) ) ;
#960 = CARTESIAN_POINT ( 'NONE',  ( 6.463481858019714643, 4.600809706232196206, 5.711197301637623625 ) ) ;
#961 = DIRECTION ( 'NONE',  ( 0.000000000000000000, -1.000000000000000000, 0.000000000000000000 ) ) ;
#962 = CARTESIAN_POINT ( 'NONE',  ( -2.832419495711385515, -59.99999999997088906, -44.99999822275857753 ) ) ;
#963 = CARTESIAN_POINT ( 'NONE',  ( 2.977408999572650927, -30.87500000204838813, -7.188101187500001821 ) ) ;
#964 = FACE_OUTER_BOUND ( 'NONE', #43504, .T. ) ;
#965 = CARTESIAN_POINT ( 'NONE',  ( -35.69739812508499455, 430.4862580793411553, 4.964222856391316441 ) ) ;
#966 = CARTESIAN_POINT ( 'NONE',  ( -6.674329190760282415, 41.70627400296338294, -58.97405543038894393 ) ) ;
#967 = CARTESIAN_POINT ( 'NONE',  ( -89.52600508066183238, -29.99999999999992539, 22.05060892610427814 ) ) ;
#968 = CARTESIAN_POINT ( 'NONE',  ( -29.53202096672922039, -60.00000000000010658, 45.26681583358117678 ) ) ;
#969 = CARTESIAN_POINT ( 'NONE',  ( -50.44932658885322496, -29.12285630001392178, 48.00120133921549836 ) ) ;
#970 = CARTESIAN_POINT ( 'NONE',  ( -1.734723475976807094E-15, 15.58845726811991383, -13.00000000000000000 ) ) ;
#971 = EDGE_LOOP ( 'NONE', ( #12898, #106488, #53796, #12965, #34148 ) ) ;
#972 = CARTESIAN_POINT ( 'NONE',  ( 35.81629280842074792, 437.2226580096241264, 4.496548509032537666 ) ) ;
#973 = CARTESIAN_POINT ( 'NONE',  ( -4.544092625063217206, 294.7929985550143215, -8.922686206316964075 ) ) ;
#974 = CARTESIAN_POINT ( 'NONE',  ( 15.95167959069860508, -2.669324059294185147, 14.76264669450079126 ) ) ;
#975 = ORIENTED_EDGE ( 'NONE', *, *, #52449, .T. ) ;
#976 = CARTESIAN_POINT ( 'NONE',  ( -17.39377970932413220, 34.16992860090641670, -24.14261105171526012 ) ) ;
#977 = CARTESIAN_POINT ( 'NONE',  ( 77.84046923451541034, -38.55292655321335360, 187.7603890749101083 ) ) ;
#978 = CARTESIAN_POINT ( 'NONE',  ( 49.26518742571373366, 13.24133944402177399, 15.39083778843029648 ) ) ;
#979 = CARTESIAN_POINT ( 'NONE',  ( 17.33349330513380337, 1.593028355512270567E-15, 0.000000000000000000 ) ) ;
#980 = CARTESIAN_POINT ( 'NONE',  ( -27.99999999999999645, 0.000000000000000000, -11.00000000000000000 ) ) ;
#981 = STYLED_ITEM ( 'NONE', ( #5135 ), #100114 ) ;
#982 = CARTESIAN_POINT ( 'NONE',  ( -42.75230560891496623, 485.3312079086282438, -3.156031357562171902 ) ) ;
#984 = CARTESIAN_POINT ( 'NONE',  ( 85.95410577112431838, -30.00000000000000000, 178.2824706394331713 ) ) ;
#983 = UNCERTAINTY_MEASURE_WITH_UNIT (LENGTH_MEASURE( 1.000000000000000082E-05 ), #44724, 'distance_accuracy_value', 'NONE');
#985 = CARTESIAN_POINT ( 'NONE',  ( 35.00874989808714588, 491.4345812359342176, 12.31435046936197786 ) ) ;
#986 = LINE ( 'NONE', #79046, #34231 ) ;
#987 = EDGE_CURVE ( 'NONE', #93305, #36055, #64077, .T. ) ;
#988 = DIRECTION ( 'NONE',  ( 0.000000000000000000, 0.9180702648391438903, -0.3964176948853118110 ) ) ;
#989 = ORIENTED_EDGE ( 'NONE', *, *, #17999, .T. ) ;
#990 = ORIENTED_EDGE ( 'NONE', *, *, #58627, .T. ) ;
#991 = CARTESIAN_POINT ( 'NONE',  ( 53.62918214583260834, -18.70049265220536938, 49.64637026124001551 ) ) ;
#992 = CARTESIAN_POINT ( 'NONE',  ( 6.563169452749920474, 41.73030697269559397, -58.95245962634098902 ) ) ;
#993 = ADVANCED_FACE ( 'NONE', ( #78604 ), #85825, .T. ) ;
#994 = CARTESIAN_POINT ( 'NONE',  ( 8.718468385534640319, 51.50404178009831924, 4.031152949374445349 ) ) ;
#995 = ORIENTED_EDGE ( 'NONE', *, *, #54153, .T. ) ;
#996 = CARTESIAN_POINT ( 'NONE',  ( -108.7293852557766058, -38.35617175010320068, 143.3098564186624628 ) ) ;
#997 = ORIENTED_EDGE ( 'NONE', *, *, #16088, .F. ) ;
#998 = CARTESIAN_POINT ( 'NONE',  ( 108.2472851096807318, -38.35600094170354168, 139.5562851490066976 ) ) ;
#999 = CARTESIAN_POINT ( 'NONE',  ( 13.75102621199263098, 22.92510964053082390, 1.258367125183780466 ) ) ;
#1000 = CARTESIAN_POINT ( 'NONE',  ( 93.38248521992973394, -60.15121612030061726, 76.38266335057042511 ) ) ;
#1001 = CARTESIAN_POINT ( 'NONE',  ( -30.98504375482477968, 439.0255438726403554, 22.25332216733684021 ) ) ;
#1002 = CARTESIAN_POINT ( 'NONE',  ( -3.381870600466846067E-15, 46.21383923812598482, -16.24999999999995026 ) ) ;
#1003 = CARTESIAN_POINT ( 'NONE',  ( -32.13173123836700995, 314.4153265821008176, -7.484038042796930412 ) ) ;
#1004 = CARTESIAN_POINT ( 'NONE',  ( 6.562934840145643101, 7.579717272840336584, -0.5631738335430742648 ) ) ;
#1005 = CARTESIAN_POINT ( 'NONE',  ( 73.94769450610063188, -60.00000000000001421, 171.6900336431731375 ) ) ;
#1006 = CARTESIAN_POINT ( 'NONE',  ( -32.99999999999982947, 489.5971041675261972, 10.80646835458724908 ) ) ;
#1007 = CONICAL_SURFACE ( 'NONE', #81951, 4.000000000000001776, 0.9599310885968808105 ) ;
#1008 = CARTESIAN_POINT ( 'NONE',  ( 17.80908660213453132, 45.00000000000000711, 62.71861104723561198 ) ) ;
#1010 = ORIENTED_EDGE ( 'NONE', *, *, #18362, .T. ) ;
#1009 =( BOUNDED_CURVE ( )  B_SPLINE_CURVE ( 2, ( #65512, #39132, #73042, #72532, #104921, #15893, #105953, #40692, #72010 ),
 .UNSPECIFIED., .F., .F. ) 
 B_SPLINE_CURVE_WITH_KNOTS ( ( 3, 2, 2, 2, 3 ),
 ( 0.5441176470588234837, 0.5514705882352941568, 0.5588235294117647189, 0.5661764705882352811, 0.5735294117647058432 ),
 .UNSPECIFIED. ) 
 CURVE ( )  GEOMETRIC_REPRESENTATION_ITEM ( )  RATIONAL_B_SPLINE_CURVE ( ( 1.000000000000000000, 0.9238795325112867385, 1.000000000000000000, 0.9238795325112867385, 1.000000000000000000, 0.9238795325112867385, 1.000000000000000000, 0.9238795325112867385, 1.000000000000000000 ) ) 
 REPRESENTATION_ITEM ( '' )  );
#1011 = CARTESIAN_POINT ( 'NONE',  ( 62.66139505928889974, -39.48355879806769053, 79.44996130265079159 ) ) ;
#1012 = CARTESIAN_POINT ( 'NONE',  ( -29.25279567920904000, 297.1008376191005027, -9.510532046834983433 ) ) ;
#1013 = EDGE_CURVE ( 'NONE', #83206, #68858, #73785, .T. ) ;
#1014 = DIRECTION ( 'NONE',  ( 3.469446951953614189E-16, -1.000000000000000000, 0.000000000000000000 ) ) ;
#1015 = AXIS2_PLACEMENT_3D ( 'NONE', #67823, #84544, #17683 ) ;
#1016 = ADVANCED_BREP_SHAPE_REPRESENTATION ( '', ( #89529, #10728 ), #35180 ) ;
#1017 = DIRECTION ( 'NONE',  ( -1.000000000000000000, -1.224606353822377258E-16, -0.000000000000000000 ) ) ;
#1018 = B_SPLINE_CURVE_WITH_KNOTS ( 'NONE', 3,
 ( #64522, #7320, #40232, #97390, #31640, #82820, #99519, #25143, #49371, #82279, #75243, #789, #58559, #48837, #98976, #97936, #24087, #89329, #41294, #32705, #73647, #15422, #50434, #33762, #74180, #17573, #33228, #83346, #89852, #15957, #57459, #8918, #261, #23552, #81725, #7854, #40758, #9436, #65573, #56392, #57999, #48308, #66636, #98459, #24611, #81204, #41824, #25698, #91457, #106014, #90379, #66102, #90923, #17036, #49911, #74711, #3506, #2426, #34306, #51510, #1343, #19205, #45042, #77392, #36446, #28339, #52039, #101666, #69313, #91973, #84953, #53120, #100592, #35370, #11573, #26751, #68785, #34838, #67183, #93581, #92498, #52568, #93042, #44502, #102192, #50965, #75790, #1885, #9991, #84426, #83877, #26227, #27824, #19732, #61217, #67710, #94103, #43959, #18650, #59088, #20270, #18106, #42896, #11040, #60174, #86038, #12112, #60695, #100061, #85492, #59628, #10517, #43433, #76849, #2955, #35913, #76313, #68238, #101131, #27292, #70889, #53639 ),
 .UNSPECIFIED., .F., .F.,
 ( 4, 2, 2, 2, 1, 1, 1, 2, 2, 2, 2, 1, 1, 1, 1, 2, 1, 1, 1, 2, 2, 1, 1, 2, 2, 1, 1, 2, 2, 1, 1, 1, 2, 2, 1, 2, 2, 1, 1, 2, 2, 2, 1, 2, 2, 1, 1, 1, 1, 1, 2, 2, 2, 2, 1, 1, 2, 2, 2, 2, 2, 1, 1, 1, 2, 2, 2, 2, 2, 2, 2, 2, 2, 1, 2, 2, 4 ),
 ( 0.4975915512072818236, 0.5289920792568175711, 0.5309546122599135831, 0.5314452455106876139, 0.5319358787614616446, 0.5329171452630095951, 0.5368422112692015080, 0.5446923432815854449, 0.5603926073063532076, 0.5623551403094491086, 0.5628457735602231393, 0.5633364068109970590, 0.5643176733125451205, 0.5682427393187369224, 0.5760928713311206373, 0.5917931353558881780, 0.5927744018574361284, 0.5932650351082101592, 0.5935103517335971191, 0.5936330100462905435, 0.5937556683589840789, 0.5957182013620797578, 0.5996432673682712267, 0.6074933993806540533, 0.6231936634054197066, 0.6241749299069676571, 0.6246655631577415768, 0.6249108797831286477, 0.6250335380958220721, 0.6251561964085156076, 0.6271187294116120636, 0.6310437954178048647, 0.6388939274301904669, 0.6545941914549617824, 0.6555754579565099549, 0.6560660912072839857, 0.6563114078326710565, 0.6565567244580581274, 0.6585192574611541394, 0.6624443234673463854, 0.6702944554797307664, 0.6859947195044996393, 0.6869759860060478118, 0.6874666192568217316, 0.6875892775695152670, 0.6877119358822088024, 0.6879572525075958733, 0.6899197855106924404, 0.6938448515168855746, 0.7016949835292720650, 0.7173952475540448237, 0.7487957756035905632, 0.7497770421051389578, 0.7507583086066873523, 0.7527208416097839194, 0.7566459076159772756, 0.7644960396283637660, 0.7801963036531369688, 0.8115968317026831524, 0.8120874649534575163, 0.8125780982042316580, 0.8135593647057801636, 0.8155218977088771748, 0.8194469637150711971, 0.8272970957274592418, 0.8429973597522353312, 0.8743978878017877321, 0.8783229538079817544, 0.8822480198141758878, 0.8900981518265640435, 0.9057984158513401329, 0.9371989439008926448, 0.9411240099070868892, 0.9450490759132811336, 0.9528992079256695114, 0.9685994719504462669, 1.000000000000000000 ),
 .UNSPECIFIED. ) ;
#1020 = CARTESIAN_POINT ( 'NONE',  ( -38.23306958165720459, 485.0121922191594308, -3.940089245333577850 ) ) ;
#1019 = CARTESIAN_POINT ( 'NONE',  ( -83.56878833267877837, -38.35732955512302311, -24.05591699864107014 ) ) ;
#1021 = CARTESIAN_POINT ( 'NONE',  ( -40.92982833529047326, 415.5608250047296792, 27.55013716896922915 ) ) ;
#1022 = CARTESIAN_POINT ( 'NONE',  ( -32.15166163075726047, 486.0589784586663882, 5.199393881401819684 ) ) ;
#1023 = FACE_OUTER_BOUND ( 'NONE', #27594, .T. ) ;
#1024 = CARTESIAN_POINT ( 'NONE',  ( 4.898587196589412829E-16, -28.62499999999999289, -8.000000000000000000 ) ) ;
#1025 = VECTOR ( 'NONE', #69707, 1000.000000000000000 ) ;
#1026 = CARTESIAN_POINT ( 'NONE',  ( 0.000000000000000000, 0.000000000000000000, 0.000000000000000000 ) ) ;
#1027 = ADVANCED_FACE ( 'NONE', ( #79675 ), #26616, .F. ) ;
#1028 = AXIS2_PLACEMENT_3D ( 'NONE', #14538, #72264, #28810 ) ;
#1029 = VECTOR ( 'NONE', #105452, 1000.000000000000000 ) ;
#1030 = CONICAL_SURFACE ( 'NONE', #92299, 6.500000000000000888, 0.8987552595851637793 ) ;
#1031 = CARTESIAN_POINT ( 'NONE',  ( 28.60676286294167880, 48.00000000000000000, 58.59397763554171235 ) ) ;
#1032 = AXIS2_PLACEMENT_3D ( 'NONE', #27039, #92244, #21458 ) ;
#1033 = EDGE_LOOP ( 'NONE', ( #58622, #71478, #91327, #14523 ) ) ;
#1034 = CARTESIAN_POINT ( 'NONE',  ( 86.29990591153305957, -18.16420165869689640, 170.9052643593855407 ) ) ;
#1035 = CARTESIAN_POINT ( 'NONE',  ( 44.12472801210862627, 485.7238370326472818, 3.975897585121170863 ) ) ;
#1036 = DIRECTION ( 'NONE',  ( 0.000000000000000000, 0.000000000000000000, -1.000000000000000000 ) ) ;
#1037 = EDGE_LOOP ( 'NONE', ( #8175, #51723, #94062, #91131, #68624 ) ) ;
#1038 = CARTESIAN_POINT ( 'NONE',  ( 0.000000000000000000, 0.000000000000000000, -25.03750572909317285 ) ) ;
#1039 = CARTESIAN_POINT ( 'NONE',  ( 0.000000000000000000, 3.500000000000000000, -4.000000000000000000 ) ) ;
#1040 = DIRECTION ( 'NONE',  ( -1.000000000000000000, -1.224606353822377258E-16, -0.000000000000000000 ) ) ;
#1041 = DIRECTION ( 'NONE',  ( -0.000000000000000000, 1.000000000000000000, -0.000000000000000000 ) ) ;
#1042 = CARTESIAN_POINT ( 'NONE',  ( 12.57956330987153848, -3.000000000000002665, -93.28077019087170640 ) ) ;
#1043 = CONICAL_SURFACE ( 'NONE', #28691, 4.000000000000007105, 0.9599310885968835860 ) ;
#1044 = CARTESIAN_POINT ( 'NONE',  ( -13.85649155559951673, -23.71556875437013190, -38.53520488289465362 ) ) ;
#1045 = CARTESIAN_POINT ( 'NONE',  ( -11.16486260932954444, -1.276900883929068975, 20.44370595537206370 ) ) ;
#1046 = EDGE_CURVE ( 'NONE', #86797, #45061, #95974, .T. ) ;
#1048 = VECTOR ( 'NONE', #46311, 1000.000000000000000 ) ;
#1047 = CARTESIAN_POINT ( 'NONE',  ( 54.43804780095958762, -60.00000000000001421, 83.66271491324665988 ) ) ;
#1049 = CARTESIAN_POINT ( 'NONE',  ( 46.00000000000000000, 488.5496196030049418, 3.680746121983992314 ) ) ;
#1050 = CARTESIAN_POINT ( 'NONE',  ( 16.25118221408220265, -15.62697450488209228, 31.58037248904192040 ) ) ;
#1052 = CARTESIAN_POINT ( 'NONE',  ( -13.79622750027070488, 22.99942056476660213, -0.5183817344751221468 ) ) ;
#1051 = CARTESIAN_POINT ( 'NONE',  ( -15.58516397110831520, -23.01955332296469692, 36.01882826759725020 ) ) ;
#1053 = CARTESIAN_POINT ( 'NONE',  ( -3.999995229665001428, -8.688226215992830959, 6.928205984420947594 ) ) ;
#1054 = CARTESIAN_POINT ( 'NONE',  ( -2.977408999572654480, -10.62500000204838813, 7.188101187499999156 ) ) ;
#1055 = DIRECTION ( 'NONE',  ( 0.000000000000000000, 0.000000000000000000, 1.000000000000000000 ) ) ;
#1056 = CARTESIAN_POINT ( 'NONE',  ( 4.302752950498871520, -1.102340297636630106, 104.4121132197325181 ) ) ;
#1057 = ORIENTED_EDGE ( 'NONE', *, *, #67703, .T. ) ;
#1058 = STYLED_ITEM ( 'NONE', ( #103909 ), #28353 ) ;
#1059 = B_SPLINE_CURVE_WITH_KNOTS ( 'NONE', 3,
 ( #76944, #85592, #59182, #69402, #18750, #91551, #9537, #93135, #28431, #42448, #27386, #75338, #17659, #50522, #11127, #42994, #1440, #34402, #44055, #67277, #93674, #76400, #34928, #100156, #36006, #26322, #92061, #2514, #19826, #18203, #67795, #100681, #68879, #101753, #35462, #26848 ),
 .UNSPECIFIED., .F., .F.,
 ( 4, 2, 2, 2, 2, 2, 2, 2, 2, 2, 2, 2, 2, 2, 2, 2, 2, 4 ),
 ( 0.000000000000000000, 0.0008074604767267251236, 0.001614920953453450247, 0.002422381430180175262, 0.003229841906906900494, 0.004037302383633626160, 0.004844762860360350525, 0.005652223337087076624, 0.006459683813813802723, 0.007267144290540529690, 0.008074604767267254055, 0.008882065243993981021, 0.009689525720720704519, 0.01049698619744742975, 0.01130444667417415498, 0.01211190715090088021, 0.01251563738926424196, 0.01291936762762760545 ),
 .UNSPECIFIED. ) ;
#1060 = CARTESIAN_POINT ( 'NONE',  ( -17.50000000000073186, 50.01371676753186080, 60.25403804533437579 ) ) ;
#1061 = DIRECTION ( 'NONE',  ( -0.5735764363510497121, 0.8191520442889892450, 1.003171929053521665E-16 ) ) ;
#1062 = CARTESIAN_POINT ( 'NONE',  ( 37.62251730745836653, 437.3427388312645121, 4.535622330043116435 ) ) ;
#1063 = EDGE_CURVE ( 'NONE', #63010, #81483, #29576, .T. ) ;
#1065 = CARTESIAN_POINT ( 'NONE',  ( 18.69608613214362336, -21.77036281612506485, -29.76801956564477081 ) ) ;
#1064 = CARTESIAN_POINT ( 'NONE',  ( 9.250997389131581983, 1.340359594676612611E-15, 0.000000000000000000 ) ) ;
#1066 = EDGE_LOOP ( 'NONE', ( #69695, #66571, #74398, #89106 ) ) ;
#1067 = CARTESIAN_POINT ( 'NONE',  ( 51.01037695545453232, 450.0000000000002274, 8.202422573753707979 ) ) ;
#1068 = CARTESIAN_POINT ( 'NONE',  ( -5.207264114973761515, 51.36227786629242331, 8.531152949374574135 ) ) ;
#1069 = ORIENTED_EDGE ( 'NONE', *, *, #67018, .F. ) ;
#1070 = EDGE_CURVE ( 'NONE', #86142, #96901, #21475, .T. ) ;
#1071 = CARTESIAN_POINT ( 'NONE',  ( -6.232496158895186156, 41.83455024993975968, -59.02481301687200244 ) ) ;
#1072 = CARTESIAN_POINT ( 'NONE',  ( -24.40731547348265096, 41.58993316039871502, -73.75804528573827668 ) ) ;
#1073 = CARTESIAN_POINT ( 'NONE',  ( -102.3034211283397354, -60.00000000000000000, 94.51454494009686869 ) ) ;
#1074 = DIRECTION ( 'NONE',  ( 0.000000000000000000, 1.000000000000000000, -0.000000000000000000 ) ) ;
#1075 = CARTESIAN_POINT ( 'NONE',  ( -18.54415329739355300, 304.6135272573319526, -9.050647025036806070 ) ) ;
#1076 = DIRECTION ( 'NONE',  ( 0.000000000000000000, 1.000000000000000000, 0.000000000000000000 ) ) ;
#1078 = CARTESIAN_POINT ( 'NONE',  ( -4.551587301587291634, -48.79941684889506348, 104.4018401814738013 ) ) ;
#1077 = APPLICATION_CONTEXT ( 'automotive_design' ) ;
#1079 = CIRCLE ( 'NONE', #61436, 1.000000000000000000 ) ;
#1081 = DIRECTION ( 'NONE',  ( 0.000000000000000000, -1.000000000000000000, 0.000000000000000000 ) ) ;
#1080 = FACE_OUTER_BOUND ( 'NONE', #43817, .T. ) ;
#1082 = CARTESIAN_POINT ( 'NONE',  ( -84.21860900825973317, -32.47513773243782964, 170.3689398041517506 ) ) ;
#1083 = MECHANICAL_DESIGN_GEOMETRIC_PRESENTATION_REPRESENTATION (  '', ( #80331 ), #71707 ) ;
#1084 = VERTEX_POINT ( 'NONE', #98506 ) ;
#1085 = DIRECTION ( 'NONE',  ( -0.7071067811865460184, 8.659560562354953812E-17, -0.7071067811865490160 ) ) ;
#1086 = EDGE_CURVE ( 'NONE', #79581, #6418, #65173, .T. ) ;
#1087 = ORIENTED_EDGE ( 'NONE', *, *, #4626, .T. ) ;
#1088 = ORIENTED_EDGE ( 'NONE', *, *, #51547, .T. ) ;
#1089 = DIRECTION ( 'NONE',  ( 1.000000000000000000, -0.000000000000000000, -0.000000000000000000 ) ) ;
#1091 = FACE_OUTER_BOUND ( 'NONE', #64944, .T. ) ;
#1090 = AXIS2_PLACEMENT_3D ( 'NONE', #64514, #23542, #89844 ) ;
#1092 = EDGE_LOOP ( 'NONE', ( #12741, #98908, #96303, #87577, #9713 ) ) ;
#1093 = CARTESIAN_POINT ( 'NONE',  ( 31.99924010301233324, 487.3002804477013683, 7.702477312236240437 ) ) ;
#1094 = DIRECTION ( 'NONE',  ( -1.000000000000000000, 0.000000000000000000, 0.000000000000000000 ) ) ;
#1095 = DIRECTION ( 'NONE',  ( 0.000000000000000000, 0.000000000000000000, -1.000000000000000000 ) ) ;
#1096 = CARTESIAN_POINT ( 'NONE',  ( -3.172455242975765533, 15.40272630234914253, 6.241991285340878548 ) ) ;
#1097 = AXIS2_PLACEMENT_3D ( 'NONE', #81472, #40508, #41042 ) ;
#1098 = CARTESIAN_POINT ( 'NONE',  ( -0.08431525725544751493, 53.39766064372322774, 10.24999999999997335 ) ) ;
#1099 = DIRECTION ( 'NONE',  ( 0.000000000000000000, -1.000000000000000000, 0.000000000000000000 ) ) ;
#1100 = PRESENTATION_LAYER_ASSIGNMENT (  '', '', ( #52878 ) ) ;
#1101 = CARTESIAN_POINT ( 'NONE',  ( 6.800000000000000711, 0.000000000000000000, -5.400000000000001243 ) ) ;
#1102 = CARTESIAN_POINT ( 'NONE',  ( 109.2895958250431931, -30.00000000000001776, 180.5620058458624442 ) ) ;
#1103 = CARTESIAN_POINT ( 'NONE',  ( -114.5103415054848170, -60.00000000000004263, 177.0886483751272351 ) ) ;
#1104 = CARTESIAN_POINT ( 'NONE',  ( -60.10583360727262914, -46.44061193372358787, 75.82408097508675837 ) ) ;
#1105 = VERTEX_POINT ( 'NONE', #16006 ) ;
#1106 = CARTESIAN_POINT ( 'NONE',  ( 94.24355000539094362, -59.99999999999023714, 9.059983527071823417 ) ) ;
#1107 = ORIENTED_EDGE ( 'NONE', *, *, #6750, .F. ) ;
#1108 = CARTESIAN_POINT ( 'NONE',  ( 5.103942930757551899, -46.43457032225082770, 31.61858307196456508 ) ) ;
#1109 = AXIS2_PLACEMENT_3D ( 'NONE', #32248, #98025, #22039 ) ;
#1110 = CARTESIAN_POINT ( 'NONE',  ( -103.8570207266811849, -45.26542059613050384, 165.7338815625408870 ) ) ;
#1112 = AXIS2_PLACEMENT_3D ( 'NONE', #11999, #77816, #58981 ) ;
#1111 = CARTESIAN_POINT ( 'NONE',  ( -1.320432766682874540E-15, -15.40625000204838635, 7.188101187500000044 ) ) ;
#1113 = EDGE_CURVE ( 'NONE', #66070, #72821, #25654, .T. ) ;
#1114 = CARTESIAN_POINT ( 'NONE',  ( -13.50000000000000178, -1.317096457811611332, 9.791700870259711920E-16 ) ) ;
#1115 = LINE ( 'NONE', #90159, #104394 ) ;
#1116 = ORIENTED_EDGE ( 'NONE', *, *, #2297, .F. ) ;
#1117 = CARTESIAN_POINT ( 'NONE',  ( -5.441945782601306014, -4.363644636964944645, -0.3576316571898500163 ) ) ;
#1119 = CIRCLE ( 'NONE', #87324, 5.000000000000010658 ) ;
#1118 = CARTESIAN_POINT ( 'NONE',  ( -24.62151441998206991, -60.00000000000002842, 41.06435363319492637 ) ) ;
#1120 = CARTESIAN_POINT ( 'NONE',  ( 9.378402013738298848, -55.78449074848818157, 23.52762072402763849 ) ) ;
#1121 = CARTESIAN_POINT ( 'NONE',  ( 2.977408999572651815, -18.31250000204838457, 7.188101187500000933 ) ) ;
#1122 = DIRECTION ( 'NONE',  ( 0.000000000000000000, -1.000000000000000000, 0.000000000000000000 ) ) ;
#1123 = DIRECTION ( 'NONE',  ( -1.000000000000000000, -1.224606353822377258E-16, -0.000000000000000000 ) ) ;
#1124 = CARTESIAN_POINT ( 'NONE',  ( 17.33349330513380693, 4.898587196589411843E-16, -4.000000000000001776 ) ) ;
#1125 = CARTESIAN_POINT ( 'NONE',  ( 1.000000000000000000, -10.14931581696268026, -12.32157755740822402 ) ) ;
#1126 = CARTESIAN_POINT ( 'NONE',  ( 32.84088564781247044, 464.9638558180851078, 11.24476942535891588 ) ) ;
#1127 = DIRECTION ( 'NONE',  ( -1.000000000000000000, -1.224606353822377258E-16, -0.000000000000000000 ) ) ;
#1128 = CARTESIAN_POINT ( 'NONE',  ( -23.61948937802356951, 28.00997096501932759, 30.76980700055176499 ) ) ;
#1129 = ADVANCED_FACE ( 'NONE', ( #74756 ), #71942, .T. ) ;
#1130 = CARTESIAN_POINT ( 'NONE',  ( 101.3080640753006350, -60.00000000000000711, 123.4091116514592414 ) ) ;
#1131 = CARTESIAN_POINT ( 'NONE',  ( -28.95202798812907830, -22.11406365714871924, 29.69911553587598974 ) ) ;
#1132 = CARTESIAN_POINT ( 'NONE',  ( 2.083846472846741813E-15, -8.673617379884035472E-16, 17.01589776168603407 ) ) ;
#1133 = CARTESIAN_POINT ( 'NONE',  ( 46.31338397479791524, -42.98337749828782250, 46.26860352693638845 ) ) ;
#1134 = CARTESIAN_POINT ( 'NONE',  ( 0.000000000000000000, 0.000000000000000000, 0.000000000000000000 ) ) ;
#1135 = ORIENTED_EDGE ( 'NONE', *, *, #16738, .T. ) ;
#1136 = EDGE_CURVE ( 'NONE', #26511, #53379, #48882, .T. ) ;
#1137 = CARTESIAN_POINT ( 'NONE',  ( -7.151217271224854066, 86.78749400445715878, -3.587901469523282927 ) ) ;
#1138 = CARTESIAN_POINT ( 'NONE',  ( -76.05157118273700689, -38.38104278720037144, 178.7388989767962926 ) ) ;
#1139 = EDGE_LOOP ( 'NONE', ( #15242, #12006 ) ) ;
#1140 = CARTESIAN_POINT ( 'NONE',  ( 2.499999999999997335, -17.18733286780618386, 25.31895441490158660 ) ) ;
#1141 = CARTESIAN_POINT ( 'NONE',  ( 54.39905599971908146, -60.00000000000002132, 67.33650783362674019 ) ) ;
#1142 = CARTESIAN_POINT ( 'NONE',  ( -48.02835407290533709, 9.771516447483559631, -16.85535821593460426 ) ) ;
#1143 = CARTESIAN_POINT ( 'NONE',  ( -43.19180182214383024, 464.9217280168089133, 10.90460934093050582 ) ) ;
#1144 = FACE_OUTER_BOUND ( 'NONE', #89371, .T. ) ;
#1145 = CARTESIAN_POINT ( 'NONE',  ( 0.000000000000000000, -100.0000000000000000, 0.000000000000000000 ) ) ;
#1146 = CARTESIAN_POINT ( 'NONE',  ( 5.649205854336970312, -88.45354532811518311, -2.034449005107560549 ) ) ;
#1147 = CARTESIAN_POINT ( 'NONE',  ( 16.96000587140905225, 45.76999459631175426, 4.188133835394149074 ) ) ;
#1148 = CIRCLE ( 'NONE', #70087, 4.000000000000000888 ) ;
#1149 = CARTESIAN_POINT ( 'NONE',  ( 108.9289463635939939, -60.00000000000000711, 135.4717115545318507 ) ) ;
#1150 = DIRECTION ( 'NONE',  ( 0.000000000000000000, -1.000000000000000000, 0.000000000000000000 ) ) ;
#1151 = AXIS2_PLACEMENT_3D ( 'NONE', #56465, #98526, #74774 ) ;
#1152 = CARTESIAN_POINT ( 'NONE',  ( -33.73990888107731223, 486.9635486473591186, 1.197400340714733780 ) ) ;
#1153 = ORIENTED_EDGE ( 'NONE', *, *, #98100, .T. ) ;
#1154 = CARTESIAN_POINT ( 'NONE',  ( -88.74229694790767553, -29.99999999999991473, 188.3111048629079676 ) ) ;
#1155 = VERTEX_POINT ( 'NONE', #58600 ) ;
#1156 = CARTESIAN_POINT ( 'NONE',  ( -3.430943074671103599, -4.332661967060490227, -17.58450835315055372 ) ) ;
#1157 = SURFACE_SIDE_STYLE ('',( #35186 ) ) ;
#1158 = CARTESIAN_POINT ( 'NONE',  ( 21.65154485178137378, 304.1284227431553404, 9.996232502259760011 ) ) ;
#1159 = DIRECTION ( 'NONE',  ( -0.000000000000000000, 1.000000000000000000, -0.000000000000000000 ) ) ;
#1160 = CARTESIAN_POINT ( 'NONE',  ( -5.082755093536326818, -21.59375000204838457, 5.082755093536325042 ) ) ;
#1161 = CARTESIAN_POINT ( 'NONE',  ( 0.000000000000000000, 34.00000000000000711, 0.000000000000000000 ) ) ;
#1162 = DIRECTION ( 'NONE',  ( 0.000000000000000000, 1.000000000000000000, 0.000000000000000000 ) ) ;
#1164 = ORIENTED_EDGE ( 'NONE', *, *, #63234, .T. ) ;
#1163 = CARTESIAN_POINT ( 'NONE',  ( -41.47568486386963116, 477.4114866153279308, -1.106491860746871669 ) ) ;
#1165 = CARTESIAN_POINT ( 'NONE',  ( 80.43333148890700102, -60.41558019800816481, 179.0669228154336281 ) ) ;
#1166 = DIRECTION ( 'NONE',  ( -0.000000000000000000, 0.000000000000000000, -1.000000000000000000 ) ) ;
#1167 = CIRCLE ( 'NONE', #61511, 8.000000000000000000 ) ;
#1168 = DIRECTION ( 'NONE',  ( 0.000000000000000000, 0.000000000000000000, 1.000000000000000000 ) ) ;
#1169 = ORIENTED_EDGE ( 'NONE', *, *, #74805, .F. ) ;
#1170 = CARTESIAN_POINT ( 'NONE',  ( -0.6177861184392186011, 18.48477677756791593, -49.40942936560928445 ) ) ;
#1171 = DIRECTION ( 'NONE',  ( -1.000000000000000000, -0.000000000000000000, -0.000000000000000000 ) ) ;
#1172 = FACE_OUTER_BOUND ( 'NONE', #64148, .T. ) ;
#1173 = CARTESIAN_POINT ( 'NONE',  ( -4.472135954999578722, 249.9999999999999432, 4.000000000000002665 ) ) ;
#1174 = CARTESIAN_POINT ( 'NONE',  ( -26.78010304687303034, 306.6307806999158743, 10.80426651792510739 ) ) ;
#1175 = B_SPLINE_CURVE_WITH_KNOTS ( 'NONE', 3,
 ( #75129, #68117, #101015, #76730, #90813, #1225, #34192, #2843, #27169, #60060, #16928, #8814, #49805, #82711, #26123, #66528, #58979, #45979, #3391, #101554, #102616, #77813, #61653, #29819, #3924, #103151, #93993, #54035, #27710, #95589, #44929, #94543, #54567, #61105, #62697, #20153, #13049, #37389, #12521, #53533, #86979, #21205, #11458, #85925 ),
 .UNSPECIFIED., .F., .F.,
 ( 4, 2, 2, 2, 2, 2, 2, 2, 2, 2, 2, 2, 2, 2, 2, 2, 2, 2, 2, 2, 2, 4 ),
 ( 0.000000000000000000, 0.0005557066357529374858, 0.001111413271505874972, 0.002222826543011752545, 0.003334239814517629685, 0.004445653086023509427, 0.006668479629035269779, 0.008891306172047029263, 0.01333695925807055517, 0.01778261234409407934, 0.02667391851614113810, 0.03556522468818819338, 0.05334783703228231089, 0.07113044937637644227, 0.08891306172047055978, 0.1066956740645646912, 0.1155869802366117499, 0.1244782864086588087, 0.1333695925807058813, 0.1378152456667294246, 0.1400380722097411823, 0.1422608987527529401 ),
 .UNSPECIFIED. ) ;
#1176 = CARTESIAN_POINT ( 'NONE',  ( -32.15702871317409972, 435.6533017138530681, 19.42106620642798376 ) ) ;
#1177 = ORIENTED_EDGE ( 'NONE', *, *, #63865, .F. ) ;
#1178 = CIRCLE ( 'NONE', #61525, 8.500000000000000000 ) ;
#1179 = VECTOR ( 'NONE', #23307, 1000.000000000000000 ) ;
#1180 = CARTESIAN_POINT ( 'NONE',  ( 6.898406705472277429E-15, 1.999999999999998224, 56.32976553137783782 ) ) ;
#1182 = CARTESIAN_POINT ( 'NONE',  ( -5.000000000000000000, -61.57181732616183467, 13.02933472593649533 ) ) ;
#1181 =( BOUNDED_SURFACE ( )  B_SPLINE_SURFACE ( 3, 2, ( 
 ( #5338, #103493, #29642 ),
 ( #47890, #55972, #96475 ),
 ( #105606, #38772, #47369 ),
 ( #46324, #80259, #87850 ) ),
 .UNSPECIFIED., .F., .F., .F. ) 
 B_SPLINE_SURFACE_WITH_KNOTS ( ( 4, 4 ),
 ( 3, 3 ),
 ( 1.626303258728256651E-18, 0.0009823161607561291166 ),
 ( 0.000000000000000000, 1.000000000000000000 ),
 .UNSPECIFIED. ) 
 GEOMETRIC_REPRESENTATION_ITEM ( )  RATIONAL_B_SPLINE_SURFACE ( (
 ( 1.000000000000000000, 0.9359444767143315635, 1.000000000000000000),
 ( 1.000000000000000000, 0.9457608441872460414, 1.000000000000000000),
 ( 1.000000000000000000, 0.9551386542018357462, 1.000000000000000000),
 ( 1.000000000000000000, 0.9603284238771496728, 1.000000000000000000) ) ) 
 REPRESENTATION_ITEM ( '' )  SURFACE ( )  );
#1183 = CARTESIAN_POINT ( 'NONE',  ( 87.17785765982114299, -39.07126277053915686, 189.3859673183815175 ) ) ;
#1184 = CARTESIAN_POINT ( 'NONE',  ( 0.3379004368769049083, 35.06844978857020578, -27.28504174633816959 ) ) ;
#1185 = CARTESIAN_POINT ( 'NONE',  ( -2.977408999572650039, -30.68750000204839168, -7.188101187500001821 ) ) ;
#1186 = CIRCLE ( 'NONE', #92529, 0.9999999999999971134 ) ;
#1187 = LINE ( 'NONE', #2266, #66386 ) ;
#1188 = CONICAL_SURFACE ( 'NONE', #11533, 13.50000000000000178, 1.047197551196596077 ) ;
#1189 = DIRECTION ( 'NONE',  ( -0.000000000000000000, 1.000000000000000000, -0.000000000000000000 ) ) ;
#1190 = B_SPLINE_CURVE_WITH_KNOTS ( 'NONE', 3,
 ( #28714, #11947, #21678, #87456, #13537, #46453, #79342, #5462, #12470, #38385, #44333, #71247, #104145, #61596, #30288, #19573, #11408, #77227, #94491, #3342 ),
 .UNSPECIFIED., .F., .F.,
 ( 4, 2, 2, 2, 2, 2, 2, 2, 2, 4 ),
 ( 0.001455504135240683061, 0.001707392234674408663, 0.001959280334108134264, 0.002463056532975591104, 0.002966832731843047945, 0.003470608930710504785, 0.003974385129577961626, 0.004478161328445418032, 0.004981937527312874439, 0.005485713726180331713 ),
 .UNSPECIFIED. ) ;
#1191 = DIRECTION ( 'NONE',  ( 0.000000000000000000, -1.000000000000000000, 0.000000000000000000 ) ) ;
#1192 = ITEM_DEFINED_TRANSFORMATION ( 'NONE', 'NONE', #100666,  #10728 ) ;
#1193 = ORIENTED_EDGE ( 'NONE', *, *, #9570, .T. ) ;
#1194 = CARTESIAN_POINT ( 'NONE',  ( -36.73887825314407252, 438.2333816059634160, 3.899276075025503996 ) ) ;
#1195 =( NAMED_UNIT ( * ) PLANE_ANGLE_UNIT ( ) SI_UNIT ( $, .RADIAN. ) );
#1196 = CARTESIAN_POINT ( 'NONE',  ( -10.03463480799100438, 7.450536368003699117, 0.000000000000000000 ) ) ;
#1197 = CARTESIAN_POINT ( 'NONE',  ( 30.00000000000000000, 0.000000000000000000, 0.000000000000000000 ) ) ;
#1198 = EDGE_CURVE ( 'NONE', #1084, #96013, #16742, .T. ) ;
#1199 = ORIENTED_EDGE ( 'NONE', *, *, #79459, .F. ) ;
#1200 = B_SPLINE_CURVE_WITH_KNOTS ( 'NONE', 3,
 ( #21077, #70646, #103540, #87370, #46370, #79260 ),
 .UNSPECIFIED., .F., .F.,
 ( 4, 2, 4 ),
 ( 8.673617379884035472E-19, 0.0003352299596267557021, 0.0006704599192535105369 ),
 .UNSPECIFIED. ) ;
#1201 = CARTESIAN_POINT ( 'NONE',  ( -4.852941176470593199, 41.41666666666666430, -70.80672828634229177 ) ) ;
#1202 = CARTESIAN_POINT ( 'NONE',  ( 111.1322596926232791, -57.67055516791452874, 193.7673871897310960 ) ) ;
#1203 = ORIENTED_EDGE ( 'NONE', *, *, #98674, .F. ) ;
#1204 = EDGE_CURVE ( 'NONE', #27751, #76782, #1387, .T. ) ;
#1205 = CARTESIAN_POINT ( 'NONE',  ( 31.35596682365932608, 438.0939828603627575, 22.55458131663555221 ) ) ;
#1206 = DIRECTION ( 'NONE',  ( 0.000000000000000000, -1.000000000000000000, 0.000000000000000000 ) ) ;
#1207 = CARTESIAN_POINT ( 'NONE',  ( 0.000000000000000000, -945.0000000000000000, 0.000000000000000000 ) ) ;
#1208 = FACE_OUTER_BOUND ( 'NONE', #105262, .T. ) ;
#1209 = CARTESIAN_POINT ( 'NONE',  ( -86.47079280586432048, -60.00000000000000000, 200.7835212895751908 ) ) ;
#1210 = EDGE_CURVE ( 'NONE', #77725, #102376, #18713, .T. ) ;
#1211 = CARTESIAN_POINT ( 'NONE',  ( 9.500496464815300968, 44.08937475915367088, -13.17128768611811296 ) ) ;
#1212 = CARTESIAN_POINT ( 'NONE',  ( 4.699999999999999289, 7.505553499465139389, 0.000000000000000000 ) ) ;
#1213 = CARTESIAN_POINT ( 'NONE',  ( -43.63899620156477965, 434.3182181978404515, 14.37213632273176422 ) ) ;
#1214 = CONICAL_SURFACE ( 'NONE', #70171, 4.000000000000001776, 0.9599310885968774798 ) ;
#1215 = CARTESIAN_POINT ( 'NONE',  ( -85.04835365382125190, -35.79626639874415872, 181.2982241859634769 ) ) ;
#1216 = ORIENTED_EDGE ( 'NONE', *, *, #7066, .T. ) ;
#1217 =( LENGTH_UNIT ( ) NAMED_UNIT ( * ) SI_UNIT ( .MILLI., .METRE. ) );
#1218 = EDGE_CURVE ( 'NONE', #87052, #73679, #22173, .T. ) ;
#1219 = CIRCLE ( 'NONE', #23690, 60.00000000000000000 ) ;
#1220 = ORIENTED_EDGE ( 'NONE', *, *, #17572, .F. ) ;
#1221 = CARTESIAN_POINT ( 'NONE',  ( -7.999912353029502654, -13.99982470603094065, -0.2691822806795001188 ) ) ;
#1222 = CARTESIAN_POINT ( 'NONE',  ( -6.057904167604424295, 41.61856606222242760, -70.65344123333893833 ) ) ;
#1223 = CARTESIAN_POINT ( 'NONE',  ( -85.33191461124319233, -52.75079290529370724, -11.76315019629209502 ) ) ;
#1224 = CARTESIAN_POINT ( 'NONE',  ( -6.934100574218754254, -13.60622170956001398, -6.341742298311178416 ) ) ;
#1225 = CARTESIAN_POINT ( 'NONE',  ( -5.249407336941563251, 5.831820959896639067, -5.000000000000000000 ) ) ;
#1226 = CARTESIAN_POINT ( 'NONE',  ( 34.98833365448072641, 302.4475715112917555, -0.2687722403786184100 ) ) ;
#1227 = DIRECTION ( 'NONE',  ( -1.000000000000000000, -1.224606353822377258E-16, -0.000000000000000000 ) ) ;
#1228 = CARTESIAN_POINT ( 'NONE',  ( -51.76085035125569789, 42.00000000008225953, 29.83308852628617203 ) ) ;
#1230 = STYLED_ITEM ( 'NONE', ( #95479 ), #1826 ) ;
#1229 = CARTESIAN_POINT ( 'NONE',  ( -22.10841373170487856, 28.16423242622105860, 31.35595207099942172 ) ) ;
#1231 = CARTESIAN_POINT ( 'NONE',  ( 31.98199460507809277, -29.99999999999994316, 41.00477363309762779 ) ) ;
#1232 = CARTESIAN_POINT ( 'NONE',  ( -36.29541806397919856, 438.2518625957745826, 3.876047449288457347 ) ) ;
#1233 = CARTESIAN_POINT ( 'NONE',  ( -41.39220545275658480, -29.99999999999999289, -36.78659115423995729 ) ) ;
#1234 = CARTESIAN_POINT ( 'NONE',  ( -67.53808867432213958, -36.01100032359511971, 91.97886330798218069 ) ) ;
#1235 = ORIENTED_EDGE ( 'NONE', *, *, #9863, .T. ) ;
#1236 = CARTESIAN_POINT ( 'NONE',  ( 72.40119513776858184, -29.99999999999997868, 139.7542682952119719 ) ) ;
#1237 = DIRECTION ( 'NONE',  ( 1.734723475976807094E-16, 0.000000000000000000, 1.000000000000000000 ) ) ;
#1238 = CARTESIAN_POINT ( 'NONE',  ( 95.90504079892977529, -57.67160311991111143, 40.96731908205725148 ) ) ;
#1239 = ORIENTED_EDGE ( 'NONE', *, *, #17517, .F. ) ;
#1240 = CARTESIAN_POINT ( 'NONE',  ( 15.02532841153920806, 41.95741965229949955, -84.73629853939195300 ) ) ;
#1241 = DIRECTION ( 'NONE',  ( -1.000000000000000000, -1.224606353822377258E-16, -0.000000000000000000 ) ) ;
#1242 = ORIENTED_EDGE ( 'NONE', *, *, #17766, .F. ) ;
#1243 = AXIS2_PLACEMENT_3D ( 'NONE', #40069, #39022, #100 ) ;
#1244 = CARTESIAN_POINT ( 'NONE',  ( 16.08349330513380337, 1.593028355512270567E-15, 0.000000000000000000 ) ) ;
#1245 = DIRECTION ( 'NONE',  ( -0.000000000000000000, -0.000000000000000000, 1.000000000000000000 ) ) ;
#1246 = DIRECTION ( 'NONE',  ( 0.000000000000000000, 0.000000000000000000, 1.000000000000000000 ) ) ;
#1247 = CARTESIAN_POINT ( 'NONE',  ( 2.977408999572650927, -12.87500000204838280, -7.188101187500001821 ) ) ;
#1248 = CARTESIAN_POINT ( 'NONE',  ( -48.28140683493110430, 14.38570471689504338, 16.83761797438776142 ) ) ;
#1249 = CARTESIAN_POINT ( 'NONE',  ( 25.22241582816893057, -4.285714285714296246, 1.650803255657552482 ) ) ;
#1250 = LINE ( 'NONE', #64569, #70140 ) ;
#1251 = CARTESIAN_POINT ( 'NONE',  ( 1.890187507280920418E-15, -1.000000000000000000, -15.43455230191221261 ) ) ;
#1252 = DIRECTION ( 'NONE',  ( 0.000000000000000000, -0.000000000000000000, 1.000000000000000000 ) ) ;
#1253 = EDGE_CURVE ( 'NONE', #84621, #81027, #106601, .T. ) ;
#1254 = VERTEX_POINT ( 'NONE', #49424 ) ;
#1255 = CARTESIAN_POINT ( 'NONE',  ( -7.428752412959402918, 40.00000000001743672, -70.23138725920588854 ) ) ;
#1256 = AXIS2_PLACEMENT_3D ( 'NONE', #83241, #12397, #59515 ) ;
#1257 = CIRCLE ( 'NONE', #20291, 4.000000000000001776 ) ;
#1259 = CARTESIAN_POINT ( 'NONE',  ( 31.45708034808273368, -36.01777946066211911, 33.04625429053564289 ) ) ;
#1258 = CARTESIAN_POINT ( 'NONE',  ( -3.769311339735803124, -48.92514534113568203, 104.1674216685380969 ) ) ;
#1260 = CARTESIAN_POINT ( 'NONE',  ( -32.68253575351214124, 486.6530702916673476, 8.413834116590887646 ) ) ;
#1261 = ORIENTED_EDGE ( 'NONE', *, *, #74125, .F. ) ;
#1262 = EDGE_CURVE ( 'NONE', #44273, #68006, #58320, .T. ) ;
#1263 = ADVANCED_FACE ( 'NONE', ( #66145 ), #27342, .F. ) ;
#1264 = DIRECTION ( 'NONE',  ( 1.000000000000000000, 0.000000000000000000, 0.000000000000000000 ) ) ;
#1265 = ORIENTED_EDGE ( 'NONE', *, *, #91724, .F. ) ;
#1266 = CIRCLE ( 'NONE', #102861, 8.000000000000000000 ) ;
#1268 = CARTESIAN_POINT ( 'NONE',  ( -9.999872502480485537, -5.000000000000000000, -1.308371270542921794 ) ) ;
#1267 = DIRECTION ( 'NONE',  ( 0.000000000000000000, 1.000000000000000000, 0.000000000000000000 ) ) ;
#1269 = AXIS2_PLACEMENT_3D ( 'NONE', #64012, #96889, #7855 ) ;
#1270 = CARTESIAN_POINT ( 'NONE',  ( 2.727751707655953116E-05, -39.99999999999999289, 30.55631662626905154 ) ) ;
#1271 = CARTESIAN_POINT ( 'NONE',  ( -6.499999999999999112, -3.752776749732587902, -8.000000000000000000 ) ) ;
#1272 =( GEOMETRIC_REPRESENTATION_CONTEXT ( 3 ) GLOBAL_UNCERTAINTY_ASSIGNED_CONTEXT ( ( #22151 ) ) GLOBAL_UNIT_ASSIGNED_CONTEXT ( ( #20564, #2162, #100342 ) ) REPRESENTATION_CONTEXT ( 'NONE', 'WORKASPACE' ) );
#1273 = COLOUR_RGB ( '', 0.40784314, 0.44705882, 0.49803922) ;
#1274 = DIRECTION ( 'NONE',  ( -1.000000000000000000, -1.224606353822377258E-16, -0.000000000000000000 ) ) ;
#1275 = FACE_OUTER_BOUND ( 'NONE', #82360, .T. ) ;
#1276 = CARTESIAN_POINT ( 'NONE',  ( 0.2960973004666590525, 12.99320615743570251, -51.71653671273871566 ) ) ;
#1277 = ORIENTED_EDGE ( 'NONE', *, *, #16474, .F. ) ;
#1278 = CARTESIAN_POINT ( 'NONE',  ( 92.74240834403246936, -60.00000000000001421, -6.770989331620668850 ) ) ;
#1279 = CARTESIAN_POINT ( 'NONE',  ( 22.57772903360667982, 26.07719920855362972, -30.87900892229609440 ) ) ;
#1280 = CARTESIAN_POINT ( 'NONE',  ( 11.82165952410163356, 294.5900423753296309, -10.05563889079273387 ) ) ;
#1281 = VECTOR ( 'NONE', #20460, 1000.000000000000000 ) ;
#1282 = DIRECTION ( 'NONE',  ( 0.000000000000000000, -1.000000000000000000, 0.000000000000000000 ) ) ;
#1283 = ORIENTED_EDGE ( 'NONE', *, *, #100237, .T. ) ;
#1284 = EDGE_CURVE ( 'NONE', #77091, #40703, #51379, .T. ) ;
#1285 = DIRECTION ( 'NONE',  ( 0.000000000000000000, -1.000000000000000000, 0.000000000000000000 ) ) ;
#1286 = ORIENTED_EDGE ( 'NONE', *, *, #100714, .F. ) ;
#1287 = VERTEX_POINT ( 'NONE', #53687 ) ;
#1288 = CARTESIAN_POINT ( 'NONE',  ( -4.573977915173229720E-15, 5.469921996229796690, -3.525817189091416282 ) ) ;
#1289 = CARTESIAN_POINT ( 'NONE',  ( 38.51502786939295930, 460.6916007118329617, 1.299075388252284080 ) ) ;
#1290 = CARTESIAN_POINT ( 'NONE',  ( 85.75148193301690469, -52.74700210787339216, -7.196367400198823816 ) ) ;
#1291 = CARTESIAN_POINT ( 'NONE',  ( -33.08716774766348578, 314.1783826430524300, -7.302587774995415337 ) ) ;
#1292 = FACE_OUTER_BOUND ( 'NONE', #5334, .T. ) ;
#1293 = CARTESIAN_POINT ( 'NONE',  ( 12.50000000000000711, 34.81126633643881974, -54.09195137927829933 ) ) ;
#1294 = ORIENTED_EDGE ( 'NONE', *, *, #89470, .F. ) ;
#1295 = ADVANCED_FACE ( 'NONE', ( #85541 ), #13506, .F. ) ;
#1296 = CARTESIAN_POINT ( 'NONE',  ( 6.499999999999996447, 1.286902272306400308, -0.09436334093185852478 ) ) ;
#1297 = ORIENTED_EDGE ( 'NONE', *, *, #96152, .T. ) ;
#1298 = VECTOR ( 'NONE', #77870, 1000.000000000000000 ) ;
#1299 = CARTESIAN_POINT ( 'NONE',  ( -7.500000000000007105, -3.000000000000000000, -68.91429205785459544 ) ) ;
#1300 = FACE_OUTER_BOUND ( 'NONE', #36868, .T. ) ;
#1301 = EDGE_CURVE ( 'NONE', #72256, #53057, #78955, .T. ) ;
#1302 = MECHANICAL_DESIGN_GEOMETRIC_PRESENTATION_REPRESENTATION (  '', ( #87494 ), #101275 ) ;
#1304 = ORIENTED_EDGE ( 'NONE', *, *, #24647, .T. ) ;
#1303 = CARTESIAN_POINT ( 'NONE',  ( 5.398220238549152228, 41.68867471179443385, -58.74408635829322378 ) ) ;
#1305 = CARTESIAN_POINT ( 'NONE',  ( 73.95717139486286840, -53.37645863163115934, 126.4388429052782641 ) ) ;
#1306 = ORIENTED_EDGE ( 'NONE', *, *, #69525, .T. ) ;
#1307 = AXIS2_PLACEMENT_3D ( 'NONE', #37456, #37990, #86531 ) ;
#1308 = CARTESIAN_POINT ( 'NONE',  ( 2.977408999572650927, -27.87500000204838457, -7.188101187500000933 ) ) ;
#1309 = CARTESIAN_POINT ( 'NONE',  ( -94.41342216801938036, -57.67108681604360498, -0.2751897739404595700 ) ) ;
#1310 = VERTEX_POINT ( 'NONE', #61264 ) ;
#1311 = PRESENTATION_STYLE_ASSIGNMENT (( #82794 ) ) ;
#1312 = CARTESIAN_POINT ( 'NONE',  ( 34.16642289233210050, 463.8422268500519863, 18.98106911353328385 ) ) ;
#1313 = AXIS2_PLACEMENT_3D ( 'NONE', #34707, #83734, #100461 ) ;
#1314 = CARTESIAN_POINT ( 'NONE',  ( 105.4036389870676373, -60.15118156600056665, 186.0926753555523021 ) ) ;
#1315 = VECTOR ( 'NONE', #44030, 1000.000000000000000 ) ;
#1316 = FACE_OUTER_BOUND ( 'NONE', #66260, .T. ) ;
#1317 = FACE_OUTER_BOUND ( 'NONE', #95853, .T. ) ;
#1318 = B_SPLINE_CURVE_WITH_KNOTS ( 'NONE', 3,
 ( #56388, #73642, #55336, #81200, #104427, #15952, #32700, #65033, #23017, #82273, #56922, #23547, #47771, #89323, #49365, #47250 ),
 .UNSPECIFIED., .F., .F.,
 ( 4, 2, 2, 2, 2, 2, 2, 4 ),
 ( 7.439477314509340780E-15, 0.0007609940918443174962, 0.001141491137762725176, 0.001521988183681132530, 0.001902485229599540102, 0.002282982275517947673, 0.002663479321436355244, 0.003043976367354762382 ),
 .UNSPECIFIED. ) ;
#1319 = CARTESIAN_POINT ( 'NONE',  ( -5.656854249492379694, -25.62500000409677270, -5.656854249492380582 ) ) ;
#1320 = CARTESIAN_POINT ( 'NONE',  ( 0.01372220897661855475, 5.948365447239585713, 2.697128823393877273 ) ) ;
#1321 = CARTESIAN_POINT ( 'NONE',  ( 9.165151389911699198, 249.9999999999999432, -4.000000000000002665 ) ) ;
#1322 = DIRECTION ( 'NONE',  ( 1.000000000000000000, -0.000000000000000000, -0.000000000000000000 ) ) ;
#1323 = CARTESIAN_POINT ( 'NONE',  ( 36.36650669486618881, 0.000000000000000000, 4.000000000000000888 ) ) ;
#1324 = LINE ( 'NONE', #34288, #96412 ) ;
#1325 = DIRECTION ( 'NONE',  ( 1.000000000000000000, 0.000000000000000000, 0.000000000000000000 ) ) ;
#1326 = SURFACE_SIDE_STYLE ('',( #75229 ) ) ;
#1327 = CARTESIAN_POINT ( 'NONE',  ( 2.499999999999999556, -7.216878364870337847, -7.063244554130006847 ) ) ;
#1328 = DIRECTION ( 'NONE',  ( 0.000000000000000000, -1.000000000000000000, 0.000000000000000000 ) ) ;
#1330 = CARTESIAN_POINT ( 'NONE',  ( 8.612678335079275271, -60.00000000000001421, 39.63706026226171986 ) ) ;
#1329 =( BOUNDED_SURFACE ( )  B_SPLINE_SURFACE ( 2, 3, ( 
 ( #7055, #79884, #38919, #90642, #9705, #34034, #66907, #1608, #65831, #16751, #50175, #74970, #42615, #17832, #83080, #16212, #81998, #16353, #32961, #82550, #81460, #50683, #8651, #49641, #75514, #99792, #25963, #34570, #98710, #41557 ),
 ( #67443, #83600, #9169, #49098, #8117, #24864, #57719, #74440, #7575, #100319, #518, #41030, #98194, #33483, #26479, #66359, #42082, #17304, #73911, #1060, #58822, #89587, #99241, #15680, #32434, #57191, #90106, #24348, #91713, #48570 ),
 ( #25410, #58270, #91195, #40496, #73371, #106271, #65306, #43681, #79631, #44766, #35093, #10765, #27010, #38667, #69565, #11835, #102456, #77656, #84680, #76570, #3770, #101916, #44225, #77115, #28604, #18372, #92218, #51223, #52297, #60945 ) ),
 .UNSPECIFIED., .F., .F., .F. ) 
 B_SPLINE_SURFACE_WITH_KNOTS ( ( 3, 3 ),
 ( 4, 2, 2, 2, 2, 2, 2, 2, 2, 2, 2, 2, 2, 2, 4 ),
 ( 0.000000000000000000, 1.000000000000000000 ),
 ( 0.000000000000000000, 0.0008794597212716800472, 0.001758919442543360094, 0.002638379163815040250, 0.003078109024450880436, 0.003517838885086720189, 0.003957568745722559941, 0.004397298606358400128, 0.005276758327630080500, 0.006156218048901760873, 0.006595947909537601059, 0.006650914142117081082, 0.006705880374696561105, 0.006815812839855521152, 0.007035677770173440378 ),
 .UNSPECIFIED. ) 
 GEOMETRIC_REPRESENTATION_ITEM ( )  RATIONAL_B_SPLINE_SURFACE ( (
 ( 1.000000000000000000, 1.000000000000000000, 1.000000000000000000, 1.000000000000000000, 1.000000000000000000, 1.000000000000000000, 1.000000000000000000, 1.000000000000000000, 1.000000000000000000, 1.000000000000000000, 1.000000000000000000, 1.000000000000000000, 1.000000000000000000, 1.000000000000000000, 1.000000000000000000, 1.000000000000000000, 1.000000000000000000, 1.000000000000000000, 1.000000000000000000, 1.000000000000000000, 1.000000000000000000, 1.000000000000000000, 1.000000000000000000, 1.000000000000000000, 1.000000000000000000, 1.000000000000000000, 1.000000000000000000, 1.000000000000000000, 1.000000000000000000, 1.000000000000000000),
 ( 1.857142857142858317, 1.857142857142858317, 1.857142857142860093, 1.857142857142860093, 1.857142857142858317, 1.857142857142858317, 1.857142857142858317, 1.857142857142858317, 1.857142857142858317, 1.857142857142858317, 1.857142857142858317, 1.857142857142858317, 1.857142857142858317, 1.857142857142858317, 1.857142857142858317, 1.857142857142858317, 1.857142857142858317, 1.857142857142858317, 1.857142857142858317, 1.857142857142858317, 1.857142857142858317, 1.857142857142858317, 1.857142857142858317, 1.857142857142858317, 1.857142857142858317, 1.857142857142858317, 1.857142857142858317, 1.857142857142858317, 1.857142857142858317, 1.857142857142858317),
 ( 1.000000000000000000, 1.000000000000000000, 1.000000000000000000, 1.000000000000000000, 1.000000000000000000, 1.000000000000000000, 1.000000000000000000, 1.000000000000000000, 1.000000000000000000, 1.000000000000000000, 1.000000000000000000, 1.000000000000000000, 1.000000000000000000, 1.000000000000000000, 1.000000000000000000, 1.000000000000000000, 1.000000000000000000, 1.000000000000000000, 1.000000000000000000, 1.000000000000000000, 1.000000000000000000, 1.000000000000000000, 1.000000000000000000, 1.000000000000000000, 1.000000000000000000, 1.000000000000000000, 1.000000000000000000, 1.000000000000000000, 1.000000000000000000, 1.000000000000000000) ) ) 
 REPRESENTATION_ITEM ( '' )  SURFACE ( )  );
#1331 = CARTESIAN_POINT ( 'NONE',  ( -89.07735706832592371, -30.00000000000000355, 188.8167402104235180 ) ) ;
#1332 = EDGE_CURVE ( 'NONE', #15839, #4914, #2467, .T. ) ;
#1333 = ORIENTED_EDGE ( 'NONE', *, *, #88212, .F. ) ;
#1334 = CONICAL_SURFACE ( 'NONE', #70289, 4.172000000000001485, 0.9599310885968750373 ) ;
#1335 = CARTESIAN_POINT ( 'NONE',  ( 3.039836064073310862, -49.44988477872288968, 44.27385412736651205 ) ) ;
#1336 = CONICAL_SURFACE ( 'NONE', #85774, 3.309500000000001663, 0.9599310885968770357 ) ;
#1337 = CARTESIAN_POINT ( 'NONE',  ( 72.47680246399455939, -57.66589478774676536, 176.7310626288513902 ) ) ;
#1338 = VECTOR ( 'NONE', #17309, 1000.000000000000000 ) ;
#1340 = CARTESIAN_POINT ( 'NONE',  ( 23.86650669486618881, -3.851859888774471706E-31, 4.000000000000000888 ) ) ;
#1339 = CARTESIAN_POINT ( 'NONE',  ( -14.84237598262832769, 1.406801708887335245, -2.172554589303035577 ) ) ;
#1341 = ADVANCED_FACE ( 'NONE', ( #26797 ), #44552, .F. ) ;
#1342 = EDGE_CURVE ( 'NONE', #27470, #31549, #77439, .T. ) ;
#1343 = CARTESIAN_POINT ( 'NONE',  ( 26.08484759583986090, -28.11660871352809821, -38.33721129155797769 ) ) ;
#1344 = CARTESIAN_POINT ( 'NONE',  ( 27.33349330513380337, 1.593028355512270567E-15, 0.000000000000000000 ) ) ;
#1345 = PRESENTATION_STYLE_ASSIGNMENT (( #91460 ) ) ;
#1346 = CARTESIAN_POINT ( 'NONE',  ( -38.90638701791922216, -60.00000000000000000, 50.62404636354061438 ) ) ;
#1347 = STYLED_ITEM ( 'NONE', ( #52437 ), #59058 ) ;
#1348 = AXIS2_PLACEMENT_3D ( 'NONE', #8861, #84364, #26692 ) ;
#1349 = DIRECTION ( 'NONE',  ( 0.000000000000000000, -1.000000000000000000, 0.000000000000000000 ) ) ;
#1350 = CARTESIAN_POINT ( 'NONE',  ( 5.930156825389887310, 53.39845306454675011, 8.358120849896316429 ) ) ;
#1351 = CARTESIAN_POINT ( 'NONE',  ( -86.43059533877344336, -24.51652298365282689, 183.3697959701796094 ) ) ;
#1352 = VERTEX_POINT ( 'NONE', #11622 ) ;
#1353 = CARTESIAN_POINT ( 'NONE',  ( 30.10055902053774801, 13.03130292445773719, 42.03558690210214621 ) ) ;
#1354 = CARTESIAN_POINT ( 'NONE',  ( -7.205479452658297035, -49.92090683998103628, 32.20013795827138381 ) ) ;
#1355 = EDGE_CURVE ( 'NONE', #7599, #17049, #34025, .T. ) ;
#1356 =( NAMED_UNIT ( * ) SI_UNIT ( $, .STERADIAN. ) SOLID_ANGLE_UNIT ( ) );
#1357 = CARTESIAN_POINT ( 'NONE',  ( -42.59877899174541938, 471.6663479800946561, 11.88906521140567918 ) ) ;
#1359 = CARTESIAN_POINT ( 'NONE',  ( 4.457938013472972472, -66.14659025852527918, 13.13206513276273313 ) ) ;
#1358 = CARTESIAN_POINT ( 'NONE',  ( 0.000000000000000000, 0.000000000000000000, -1.161000000000000032 ) ) ;
#1360 = ORIENTED_EDGE ( 'NONE', *, *, #58649, .F. ) ;
#1361 = CARTESIAN_POINT ( 'NONE',  ( -46.00000000000000000, 488.9831568219305495, 4.757012338623842318 ) ) ;
#1362 = DIRECTION ( 'NONE',  ( 0.000000000000000000, -1.000000000000000000, 0.000000000000000000 ) ) ;
#1363 = CARTESIAN_POINT ( 'NONE',  ( 32.99999999999999289, 434.0826380246135727, 11.57835738278531323 ) ) ;
#1364 = CARTESIAN_POINT ( 'NONE',  ( 29.09372310509538551, 297.2342953755526196, -1.479845727618128715 ) ) ;
#1365 = CARTESIAN_POINT ( 'NONE',  ( 32.11411341898570981, 317.7919323371296514, -6.873671351699469412 ) ) ;
#1366 = DIRECTION ( 'NONE',  ( -1.000000000000000000, 1.224646799147354686E-16, 0.000000000000000000 ) ) ;
#1367 = CARTESIAN_POINT ( 'NONE',  ( -14.29190075645216318, 6.456385560668112866, -7.561819230143454362 ) ) ;
#1368 = CARTESIAN_POINT ( 'NONE',  ( 108.5047413589249032, -30.00000000000003197, 153.5997199437166785 ) ) ;
#1369 = CARTESIAN_POINT ( 'NONE',  ( -80.21561207987609521, -49.91266703426506979, 160.3608070185047723 ) ) ;
#1370 = ORIENTED_EDGE ( 'NONE', *, *, #98570, .F. ) ;
#1371 = CARTESIAN_POINT ( 'NONE',  ( 10.00000000000000000, 0.000000000000000000, 10.00000000000000000 ) ) ;
#1372 = CARTESIAN_POINT ( 'NONE',  ( -8.252218488625017898E-15, -6.732211846623387785, 4.339467034331188522 ) ) ;
#1373 = FILL_AREA_STYLE_COLOUR ( '', #73048 ) ;
#1374 = LINE ( 'NONE', #95210, #95947 ) ;
#1376 = VECTOR ( 'NONE', #72788, 1000.000000000000000 ) ;
#1375 = CARTESIAN_POINT ( 'NONE',  ( 4.258999010316228073, 11.59408722316739038, -5.000000000000002665 ) ) ;
#1377 = CARTESIAN_POINT ( 'NONE',  ( 6.562934840145643101, -7.579717272840337472, 0.5631738335430738207 ) ) ;
#1378 = VERTEX_POINT ( 'NONE', #60219 ) ;
#1379 = CARTESIAN_POINT ( 'NONE',  ( -22.67189858315301265, 304.4443818766867480, 10.06497620991740760 ) ) ;
#1380 = ORIENTED_EDGE ( 'NONE', *, *, #50736, .F. ) ;
#1381 = CARTESIAN_POINT ( 'NONE',  ( 36.69747761309537992, 484.6510752690958839, -2.871877106304832061 ) ) ;
#1382 = CARTESIAN_POINT ( 'NONE',  ( -11.28351131189990220, 9.073918974790291969, -12.46553453015540924 ) ) ;
#1383 = CARTESIAN_POINT ( 'NONE',  ( 32.65915130203010364, 487.2382554987875665, 8.056573295094644038 ) ) ;
#1384 = CARTESIAN_POINT ( 'NONE',  ( 57.09426686933954898, 50.00000000000000000, -27.25041924768392576 ) ) ;
#1385 = CARTESIAN_POINT ( 'NONE',  ( 5.000000000000000000, -14.24437098773438315, 11.98245615812517784 ) ) ;
#1387 = LINE ( 'NONE', #83925, #53182 ) ;
#1386 = VECTOR ( 'NONE', #70885, 1000.000000000000000 ) ;
#1388 = ORIENTED_EDGE ( 'NONE', *, *, #43399, .F. ) ;
#1389 = CARTESIAN_POINT ( 'NONE',  ( 108.1486474569906591, -60.00000000000001421, 129.9490626958306052 ) ) ;
#1391 = CARTESIAN_POINT ( 'NONE',  ( 19.73958029447546281, -22.07186201797325964, 28.03297876132052835 ) ) ;
#1390 = CARTESIAN_POINT ( 'NONE',  ( -70.85198506086598513, -59.99999999999993605, 164.3657034848495186 ) ) ;
#1393 = CARTESIAN_POINT ( 'NONE',  ( 82.92278159110408353, -38.00000000000002132, -11.29934189521478416 ) ) ;
#1392 = PRODUCT_DEFINITION_CONTEXT ( 'detailed design', #6631, 'design' ) ;
#1394 = CARTESIAN_POINT ( 'NONE',  ( 16.64348903516524203, 43.75610143575153188, 4.157797401561407646 ) ) ;
#1395 = AXIS2_PLACEMENT_3D ( 'NONE', #72416, #22310, #39003 ) ;
#1396 = EDGE_CURVE ( 'NONE', #75387, #97120, #56369, .T. ) ;
#1397 = CARTESIAN_POINT ( 'NONE',  ( -39.55842790402597586, -25.68830429364345136, 35.29869333941604026 ) ) ;
#1398 = CARTESIAN_POINT ( 'NONE',  ( 47.33349330513379982, -7.703719777548943412E-31, 4.000000000000001776 ) ) ;
#1399 = UNCERTAINTY_MEASURE_WITH_UNIT (LENGTH_MEASURE( 1.000000000000000082E-05 ), #35187, 'distance_accuracy_value', 'NONE');
#1400 = ORIENTED_EDGE ( 'NONE', *, *, #19466, .F. ) ;
#1401 = CARTESIAN_POINT ( 'NONE',  ( 8.099999999999999645, 1.041268927496807532E-15, -8.400000000000000355 ) ) ;
#1402 = CARTESIAN_POINT ( 'NONE',  ( -43.22624402988198256, 434.6924416827911841, 9.644670084742074323 ) ) ;
#1403 = CARTESIAN_POINT ( 'NONE',  ( 31.19792890532719198, 414.2215770364159084, 25.44228638033458623 ) ) ;
#1404 = VECTOR ( 'NONE', #20579, 1000.000000000000114 ) ;
#1405 = CARTESIAN_POINT ( 'NONE',  ( 27.02022815836235026, 5.000000000000004441, 6.123233995736770227E-16 ) ) ;
#1406 = CARTESIAN_POINT ( 'NONE',  ( 16.97163447634728328, 303.5650180578880963, -10.06095676631376534 ) ) ;
#1407 = CARTESIAN_POINT ( 'NONE',  ( 6.898673495379865628, -0.02001816142087574704, 19.00543362303419670 ) ) ;
#1408 = ORIENTED_EDGE ( 'NONE', *, *, #104014, .T. ) ;
#1409 = CARTESIAN_POINT ( 'NONE',  ( -16.58616928888070419, 36.42044334926446680, -24.29863715439297067 ) ) ;
#1410 = COLOUR_RGB ( '', 0.08235294, 0.09019608, 0.10196078) ;
#1411 = EDGE_LOOP ( 'NONE', ( #4506, #106407, #66047, #25112 ) ) ;
#1412 = B_SPLINE_CURVE_WITH_KNOTS ( 'NONE', 3,
 ( #39421, #57162, #56631, #89552 ),
 .UNSPECIFIED., .F., .F.,
 ( 4, 4 ),
 ( 0.000000000000000000, 0.001851782051266449803 ),
 .UNSPECIFIED. ) ;
#1413 = CARTESIAN_POINT ( 'NONE',  ( 51.82200911525481501, -29.99999999993400834, 69.17902143724853659 ) ) ;
#1414 = CARTESIAN_POINT ( 'NONE',  ( 46.97231841192020596, 12.59348177918415956, 16.28806988207259110 ) ) ;
#1415 = CARTESIAN_POINT ( 'NONE',  ( -33.00000000000000000, 485.0303364503728289, 0.9535057477320436625 ) ) ;
#1416 = FACE_OUTER_BOUND ( 'NONE', #84705, .T. ) ;
#1417 = CARTESIAN_POINT ( 'NONE',  ( 81.07391525874288618, -30.00000000000001066, 22.29763315622286868 ) ) ;
#1418 = SURFACE_STYLE_USAGE ( .BOTH. , #50506 ) ;
#1419 = ORIENTED_EDGE ( 'NONE', *, *, #69551, .F. ) ;
#1420 = VERTEX_POINT ( 'NONE', #3554 ) ;
#1421 = ORIENTED_EDGE ( 'NONE', *, *, #89266, .F. ) ;
#1422 = AXIS2_PLACEMENT_3D ( 'NONE', #95336, #54307, #87253 ) ;
#1423 = DIRECTION ( 'NONE',  ( 0.000000000000000000, 0.000000000000000000, 1.000000000000000000 ) ) ;
#1424 = VECTOR ( 'NONE', #7236, 1000.000000000000000 ) ;
#1425 = DIRECTION ( 'NONE',  ( -0.000000000000000000, -1.000000000000000000, -0.000000000000000000 ) ) ;
#1426 = CARTESIAN_POINT ( 'NONE',  ( 7.999999999999998224, -15.59374999999999289, 3.313708498984766049 ) ) ;
#1427 = AXIS2_PLACEMENT_3D ( 'NONE', #11060, #73010, #21864 ) ;
#1428 = CARTESIAN_POINT ( 'NONE',  ( 40.54867362617589777, 438.3503844673198842, 22.65705215920161919 ) ) ;
#1430 = AXIS2_PLACEMENT_3D ( 'NONE', #49604, #72807, #41516 ) ;
#1429 = CARTESIAN_POINT ( 'NONE',  ( -32.01725138626208178, 362.9172354553742821, 22.63265723493709203 ) ) ;
#1431 = CARTESIAN_POINT ( 'NONE',  ( 56.48317336153285595, 6.856755485862130937E-15, 0.000000000000000000 ) ) ;
#1432 = ORIENTED_EDGE ( 'NONE', *, *, #71720, .T. ) ;
#1433 = CARTESIAN_POINT ( 'NONE',  ( -11.68767211932355465, 50.00000000000000000, -88.14097461399492772 ) ) ;
#1434 = ORIENTED_EDGE ( 'NONE', *, *, #1046, .T. ) ;
#1435 = CARTESIAN_POINT ( 'NONE',  ( 101.4868948250290259, 1.016364837396684119E-14, 0.000000000000000000 ) ) ;
#1436 = CARTESIAN_POINT ( 'NONE',  ( 63.48417968370426223, -38.33937475606958145, 107.9424513483785688 ) ) ;
#1437 = CYLINDRICAL_SURFACE ( 'NONE', #33669, 2.000000000000000444 ) ;
#1438 = CARTESIAN_POINT ( 'NONE',  ( 33.82934323895533169, 302.9354609585176945, 11.80188247845831917 ) ) ;
#1439 = ADVANCED_FACE ( 'NONE', ( #19781 ), #39171, .T. ) ;
#1440 = CARTESIAN_POINT ( 'NONE',  ( -5.999511540169428336, 246.0007326911455721, -0.2833228702578324265 ) ) ;
#1441 = ORIENTED_EDGE ( 'NONE', *, *, #60385, .T. ) ;
#1442 = DIRECTION ( 'NONE',  ( 0.000000000000000000, 0.000000000000000000, 1.000000000000000000 ) ) ;
#1443 = DIRECTION ( 'NONE',  ( -1.000000000000000000, -1.224606353822377258E-16, -0.000000000000000000 ) ) ;
#1444 = DIRECTION ( 'NONE',  ( -0.000000000000000000, -1.000000000000000000, -0.000000000000000000 ) ) ;
#1445 = CARTESIAN_POINT ( 'NONE',  ( 14.98982670280988039, 2.030473042282394225, 0.4147640935944429397 ) ) ;
#1446 = ORIENTED_EDGE ( 'NONE', *, *, #35977, .F. ) ;
#1447 = STYLED_ITEM ( 'NONE', ( #79901 ), #44605 ) ;
#1449 = CARTESIAN_POINT ( 'NONE',  ( -24.23834595003092574, 304.0759229526369154, 10.20476466122759085 ) ) ;
#1448 = SHAPE_REPRESENTATION_RELATIONSHIP ( 'NONE' , 'NONE' ,  #38413, #89702 ) ;
#1450 = CARTESIAN_POINT ( 'NONE',  ( 7.321407651878572231, 54.25251164017154082, -2.971923534686649049 ) ) ;
#1451 = DIRECTION ( 'NONE',  ( 0.000000000000000000, 0.000000000000000000, -1.000000000000000000 ) ) ;
#1452 = CARTESIAN_POINT ( 'NONE',  ( -8.000000000000000000, -10.34374999999999289, -3.313708498984762496 ) ) ;
#1453 = CARTESIAN_POINT ( 'NONE',  ( 0.000000000000000000, 50.00000000000000000, 0.000000000000000000 ) ) ;
#1454 = VECTOR ( 'NONE', #92157, 1000.000000000000000 ) ;
#1455 = CARTESIAN_POINT ( 'NONE',  ( 1.697392215626793099, 301.6957921518827561, 9.856842546290842222 ) ) ;
#1456 = AXIS2_PLACEMENT_3D ( 'NONE', #15897, #40696, #88208 ) ;
#1457 = PRODUCT_RELATED_PRODUCT_CATEGORY ( 'part', '', ( #19103 ) ) ;
#1458 = CARTESIAN_POINT ( 'NONE',  ( 3.400000000000000355, 0.000000000000000000, -3.852324522925831385 ) ) ;
#1459 = CARTESIAN_POINT ( 'NONE',  ( 84.15625878038136420, -57.42679397882895387, 190.9228678296396708 ) ) ;
#1460 = AXIS2_PLACEMENT_3D ( 'NONE', #96325, #38110, #20886 ) ;
#1461 = CARTESIAN_POINT ( 'NONE',  ( 17.07643158642794390, 37.03581886162301373, -21.84712036628289056 ) ) ;
#1462 = CARTESIAN_POINT ( 'NONE',  ( -3.067650313623253577, 44.37499570395408455, 5.000000000000000000 ) ) ;
#1463 = EDGE_LOOP ( 'NONE', ( #93051, #42549 ) ) ;
#1464 = CARTESIAN_POINT ( 'NONE',  ( 92.25064720835594301, -57.65936633065353334, -18.85860424735002994 ) ) ;
#1465 = CARTESIAN_POINT ( 'NONE',  ( 41.47644909359268439, 477.1147368610181161, -1.041749719072760261 ) ) ;
#1466 = CARTESIAN_POINT ( 'NONE',  ( 15.52523732965139125, 34.97072044547751091, -22.76566327259062206 ) ) ;
#1467 = DIRECTION ( 'NONE',  ( 0.000000000000000000, 0.000000000000000000, 1.000000000000000000 ) ) ;
#1468 = CARTESIAN_POINT ( 'NONE',  ( -91.50145128248362880, -30.00000000000000000, 97.27245082254961517 ) ) ;
#1469 = MECHANICAL_DESIGN_GEOMETRIC_PRESENTATION_REPRESENTATION (  '', ( #84110 ), #61812 ) ;
#1470 = CARTESIAN_POINT ( 'NONE',  ( 0.000000000000000000, -5.000000000000000000, -14.14213562373095101 ) ) ;
#1471 = CARTESIAN_POINT ( 'NONE',  ( -5.656854249492381470, -29.75000000409677270, 5.656854249492379694 ) ) ;
#1472 = CARTESIAN_POINT ( 'NONE',  ( -7.112481253774054935, 4.553861071371609448, -7.781689322729132385 ) ) ;
#1474 = DIRECTION ( 'NONE',  ( -0.000000000000000000, -0.1492727218618779272, -0.9887960631535436251 ) ) ;
#1473 = CARTESIAN_POINT ( 'NONE',  ( 35.88361968365485666, 490.8299076634168046, 12.39904854651338972 ) ) ;
#1475 = EDGE_CURVE ( 'NONE', #36646, #93186, #88516, .T. ) ;
#1476 = FACE_OUTER_BOUND ( 'NONE', #103523, .T. ) ;
#1477 = CARTESIAN_POINT ( 'NONE',  ( -29.68315524076957246, 18.29184282782463455, 39.60535821593508388 ) ) ;
#1478 = CARTESIAN_POINT ( 'NONE',  ( -35.02595189227570671, 491.4435019764551953, 12.32055256812894228 ) ) ;
#1479 = CARTESIAN_POINT ( 'NONE',  ( 5.855777637195783925, -81.21893503241551571, -1.331220292256681592 ) ) ;
#1480 = CARTESIAN_POINT ( 'NONE',  ( -43.95063711303794207, 484.1591904870579697, -1.189330446659679241 ) ) ;
#1481 = DIRECTION ( 'NONE',  ( 0.000000000000000000, 1.000000000000000000, 0.000000000000000000 ) ) ;
#1482 = CARTESIAN_POINT ( 'NONE',  ( 44.68310115566336549, -26.19546418128159360, -29.27681102373194832 ) ) ;
#1483 = COLOUR_RGB ( '', 0.09019608, 0.27058824, 0.51372549) ;
#1484 = CARTESIAN_POINT ( 'NONE',  ( -21.59838042582818574, -49.91976248583917908, 32.92827807905565862 ) ) ;
#1485 = VERTEX_POINT ( 'NONE', #106327 ) ;
#1486 = CARTESIAN_POINT ( 'NONE',  ( 6.705159343100833169, 9.539515232900985353, 2.022944797798714944 ) ) ;
#1487 = CARTESIAN_POINT ( 'NONE',  ( -7.619135598915499408, 81.82694632215323338, 2.449260492474793161 ) ) ;
#1488 = EDGE_CURVE ( 'NONE', #96068, #80953, #103829, .T. ) ;
#1489 = CARTESIAN_POINT ( 'NONE',  ( -55.65965000038991661, -28.60422584645425914, -26.38104815732392439 ) ) ;
#1490 = EDGE_CURVE ( 'NONE', #80282, #84910, #59881, .T. ) ;
#1492 = CARTESIAN_POINT ( 'NONE',  ( -73.91452718666039345, -47.40888132954707856, -22.31150090410597642 ) ) ;
#1491 = CARTESIAN_POINT ( 'NONE',  ( 0.000000000000000000, 0.000000000000000000, 0.000000000000000000 ) ) ;
#1493 = VERTEX_POINT ( 'NONE', #51 ) ;
#1494 = DIRECTION ( 'NONE',  ( 0.000000000000000000, 0.000000000000000000, 1.000000000000000000 ) ) ;
#1495 = ORIENTED_EDGE ( 'NONE', *, *, #35490, .T. ) ;
#1496 = CARTESIAN_POINT ( 'NONE',  ( -26.34287197489002352, 35.00042356184812320, 7.802188285690729863 ) ) ;
#1497 = STYLED_ITEM ( 'NONE', ( #106107 ), #89707 ) ;
#1498 = LINE ( 'NONE', #3117, #83897 ) ;
#1499 = CARTESIAN_POINT ( 'NONE',  ( -43.30146564658384278, -60.00000000000000711, -39.13498028926473893 ) ) ;
#1500 = ORIENTED_EDGE ( 'NONE', *, *, #15313, .F. ) ;
#1501 = CARTESIAN_POINT ( 'NONE',  ( 0.000000000000000000, 34.00000000000000000, 0.000000000000000000 ) ) ;
#1502 = CARTESIAN_POINT ( 'NONE',  ( -5.144603409922094528, 294.7784803138362690, -8.579809241137068554 ) ) ;
#1503 = CARTESIAN_POINT ( 'NONE',  ( 100.5526317174083886, -45.27816195441151592, 191.9872936527002594 ) ) ;
#1505 = CARTESIAN_POINT ( 'NONE',  ( -3.668277386370349280, -1.103629945923298106, 104.6014336420241051 ) ) ;
#1504 = CARTESIAN_POINT ( 'NONE',  ( 6.752393983348615514, 294.7360562376221651, -7.398233510975328109 ) ) ;
#1506 = ORIENTED_EDGE ( 'NONE', *, *, #47518, .F. ) ;
#1507 = VERTEX_POINT ( 'NONE', #87137 ) ;
#1508 = EDGE_LOOP ( 'NONE', ( #97538, #59106, #779, #30356 ) ) ;
#1509 = CARTESIAN_POINT ( 'NONE',  ( 31.20657268416513475, 410.2456177201033825, 25.45174340587148265 ) ) ;
#1510 = CARTESIAN_POINT ( 'NONE',  ( 0.000000000000000000, 0.000000000000000000, -10.00000000000000000 ) ) ;
#1511 = CARTESIAN_POINT ( 'NONE',  ( 9.768787396428281866, 53.46522389469076586, 2.424760876876827176 ) ) ;
#1512 = ORIENTED_EDGE ( 'NONE', *, *, #55924, .F. ) ;
#1513 = CARTESIAN_POINT ( 'NONE',  ( 15.39205472978306233, 46.19766366449148620, -5.347876573122199773 ) ) ;
#1514 = CARTESIAN_POINT ( 'NONE',  ( -32.22503847990287795, 485.9064490506194716, 4.829857536089223302 ) ) ;
#1515 = COLOUR_RGB ( '', 0.08235294, 0.09019608, 0.10196078) ;
#1516 = LINE ( 'NONE', #59261, #27205 ) ;
#1517 = CARTESIAN_POINT ( 'NONE',  ( -65.18805258578451856, -57.67964089302213893, 127.3758707571902846 ) ) ;
#1518 = CARTESIAN_POINT ( 'NONE',  ( -30.77329953031004450, 15.53171713056513603, 40.23250653748785766 ) ) ;
#1519 = AXIS2_PLACEMENT_3D ( 'NONE', #92753, #35621, #18911 ) ;
#1520 = CARTESIAN_POINT ( 'NONE',  ( -31.00389226642222340, 485.8187364282109115, 14.27494812388583512 ) ) ;
#1521 = DIRECTION ( 'NONE',  ( -0.000000000000000000, 0.000000000000000000, -1.000000000000000000 ) ) ;
#1522 = CARTESIAN_POINT ( 'NONE',  ( -87.61621634008581339, -14.21045842199436571, -10.69165924380367372 ) ) ;
#1523 = ADVANCED_FACE ( 'NONE', ( #46142 ), #49156, .F. ) ;
#1524 = CARTESIAN_POINT ( 'NONE',  ( -51.33256727740138103, -39.51242535013955859, 53.05575148282086673 ) ) ;
#1525 = AXIS2_PLACEMENT_3D ( 'NONE', #82681, #15823, #655 ) ;
#1526 = DIRECTION ( 'NONE',  ( 0.000000000000000000, -1.000000000000000000, 0.000000000000000000 ) ) ;
#1527 = VERTEX_POINT ( 'NONE', #32493 ) ;
#1528 = LINE ( 'NONE', #2066, #52976 ) ;
#1529 = CARTESIAN_POINT ( 'NONE',  ( -8.890893604471449052, 294.6744728344740452, -4.583208782182904173 ) ) ;
#1530 = AXIS2_PLACEMENT_3D ( 'NONE', #103824, #70931, #88185 ) ;
#1531 = CARTESIAN_POINT ( 'NONE',  ( 9.886129545901154003, -3.298559501015256856, 15.11875162840864739 ) ) ;
#1532 = VERTEX_POINT ( 'NONE', #48626 ) ;
#1533 =( LENGTH_UNIT ( ) NAMED_UNIT ( * ) SI_UNIT ( .MILLI., .METRE. ) );
#1534 = STYLED_ITEM ( 'NONE', ( #23767 ), #12836 ) ;
#1535 = CARTESIAN_POINT ( 'NONE',  ( 83.71607977213993479, -38.77881177540385949, 197.5599962973940364 ) ) ;
#1536 = CARTESIAN_POINT ( 'NONE',  ( 49.03408319953887684, 14.13974658789363836, 14.85990013744586591 ) ) ;
#1537 = CARTESIAN_POINT ( 'NONE',  ( -5.371856143885752388, 52.06043921290445553, -6.031152949374585681 ) ) ;
#1538 = CARTESIAN_POINT ( 'NONE',  ( -17.49999999999997513, 47.00000000000000000, 64.09953197959339377 ) ) ;
#1539 = CARTESIAN_POINT ( 'NONE',  ( -79.13121736037263076, 42.00000000000000000, -45.60838156032659185 ) ) ;
#1540 = CARTESIAN_POINT ( 'NONE',  ( 89.35610039075180566, -30.00000000000000355, 189.1959864005116003 ) ) ;
#1541 = CARTESIAN_POINT ( 'NONE',  ( 43.63899620156487202, 434.3182181978403946, 14.37213632273145336 ) ) ;
#1542 = EDGE_CURVE ( 'NONE', #84380, #59429, #35822, .T. ) ;
#1543 = DIRECTION ( 'NONE',  ( 1.000000000000000000, 1.224606353822377258E-16, 0.000000000000000000 ) ) ;
#1544 = FACE_OUTER_BOUND ( 'NONE', #57409, .T. ) ;
#1545 = AXIS2_PLACEMENT_3D ( 'NONE', #26592, #28178, #18475 ) ;
#1546 = ORIENTED_EDGE ( 'NONE', *, *, #12871, .F. ) ;
#1547 = VERTEX_POINT ( 'NONE', #62331 ) ;
#1548 = CARTESIAN_POINT ( 'NONE',  ( 50.83651537935279663, -56.83343471464645091, 58.27782394269261346 ) ) ;
#1550 = PRESENTATION_LAYER_ASSIGNMENT (  '', '', ( #53244 ) ) ;
#1549 = FACE_OUTER_BOUND ( 'NONE', #26116, .T. ) ;
#1551 = ORIENTED_EDGE ( 'NONE', *, *, #14177, .F. ) ;
#1552 = CARTESIAN_POINT ( 'NONE',  ( -90.66125720047617165, -38.34385643748635886, 8.951488509635131763 ) ) ;
#1553 = ORIENTED_EDGE ( 'NONE', *, *, #58689, .T. ) ;
#1554 = FACE_OUTER_BOUND ( 'NONE', #56896, .T. ) ;
#1555 = CARTESIAN_POINT ( 'NONE',  ( 110.3663729943234273, -38.35605026316035548, 158.8586429886188967 ) ) ;
#1556 = CARTESIAN_POINT ( 'NONE',  ( 13.58541053222488060, 24.75820122212995500, 0.5865258224344345184 ) ) ;
#1557 = CARTESIAN_POINT ( 'NONE',  ( 86.28824347430642661, -52.71555702371639285, 35.16861034268297459 ) ) ;
#1559 = AXIS2_PLACEMENT_3D ( 'NONE', #13097, #27758, #28820 ) ;
#1558 = CARTESIAN_POINT ( 'NONE',  ( -0.1681987345962790426, 45.30391365246044444, -18.75000000000000355 ) ) ;
#1560 = CARTESIAN_POINT ( 'NONE',  ( -27.22372400652621849, 306.4093034055409817, -9.433020069181509371 ) ) ;
#1561 = CARTESIAN_POINT ( 'NONE',  ( 3.208180356140310163, -10.20788741807700717, -11.61546768905490445 ) ) ;
#1562 = EDGE_CURVE ( 'NONE', #68982, #59035, #69233, .T. ) ;
#1563 = VECTOR ( 'NONE', #93447, 1000.000000000000000 ) ;
#1564 = DIRECTION ( 'NONE',  ( -1.000000000000000000, -0.000000000000000000, -0.000000000000000000 ) ) ;
#1565 = CARTESIAN_POINT ( 'NONE',  ( 18.30269215000137351, 45.00000000000000000, 62.40549835204959805 ) ) ;
#1566 = VERTEX_POINT ( 'NONE', #33544 ) ;
#1567 = CARTESIAN_POINT ( 'NONE',  ( 59.78093605258602139, -25.59731411256743527, 65.24099791815997662 ) ) ;
#1568 = ADVANCED_FACE ( 'NONE', ( #9765 ), #3048, .T. ) ;
#1569 = CARTESIAN_POINT ( 'NONE',  ( 0.8394321637725764562, 37.08900195433652414, 27.57017630837880517 ) ) ;
#1570 = DIRECTION ( 'NONE',  ( -1.000000000000000000, -1.224606353822377258E-16, -0.000000000000000000 ) ) ;
#1571 = CARTESIAN_POINT ( 'NONE',  ( -34.28792013165121233, 484.9850795199450886, 0.1048768172220471973 ) ) ;
#1572 = CARTESIAN_POINT ( 'NONE',  ( -32.46302019025186780, 342.3532878214976449, 19.26406215151588341 ) ) ;
#1573 = CARTESIAN_POINT ( 'NONE',  ( -38.56699491466429208, 25.18982931514603507, -12.97440760532226456 ) ) ;
#1574 = FACE_BOUND ( 'NONE', #45713, .T. ) ;
#1575 = CARTESIAN_POINT ( 'NONE',  ( 3.313708498984762496, -26.28124999999999645, 7.999999999999998224 ) ) ;
#1576 = EDGE_CURVE ( 'NONE', #43900, #49621, #104578, .T. ) ;
#1577 = MECHANICAL_DESIGN_GEOMETRIC_PRESENTATION_REPRESENTATION (  '', ( #5070 ), #92830 ) ;
#1578 = CONICAL_SURFACE ( 'NONE', #5076, 4.000000000000001776, 0.9599310885968774798 ) ;
#1579 = STYLED_ITEM ( 'NONE', ( #94435 ), #102410 ) ;
#1580 = CARTESIAN_POINT ( 'NONE',  ( 16.02905770043921763, 43.70337463170952930, -6.507967097231396103 ) ) ;
#1581 = VERTEX_POINT ( 'NONE', #17361 ) ;
#1582 = CARTESIAN_POINT ( 'NONE',  ( 84.05033357701425700, -42.97894289604104046, 182.1071465539960172 ) ) ;
#1583 = FACE_OUTER_BOUND ( 'NONE', #33137, .T. ) ;
#1584 = CARTESIAN_POINT ( 'NONE',  ( -3.313708498984722528, -9.218750004096770923, -8.000000000000040856 ) ) ;
#1585 = ORIENTED_EDGE ( 'NONE', *, *, #7579, .T. ) ;
#1586 = DIRECTION ( 'NONE',  ( 0.000000000000000000, 0.000000000000000000, 1.000000000000000000 ) ) ;
#1587 = EDGE_CURVE ( 'NONE', #80603, #84468, #68497, .T. ) ;
#1588 = CARTESIAN_POINT ( 'NONE',  ( 43.04469050570425992, 434.7734435962918269, 9.248231035222774565 ) ) ;
#1589 = FILL_AREA_STYLE_COLOUR ( '', #61034 ) ;
#1590 = CARTESIAN_POINT ( 'NONE',  ( -1.347801180114141628, -3.000000000000002665, -99.99999999999927525 ) ) ;
#1591 = CARTESIAN_POINT ( 'NONE',  ( -27.10508918418226898, -28.49923914006959080, -38.30058658043027719 ) ) ;
#1592 = LINE ( 'NONE', #34553, #4317 ) ;
#1593 = VECTOR ( 'NONE', #4066, 1000.000000000000000 ) ;
#1594 = CARTESIAN_POINT ( 'NONE',  ( 43.73109350357475478, -60.00000000000000711, 58.18588980859811244 ) ) ;
#1595 = CIRCLE ( 'NONE', #82536, 4.000000000000001776 ) ;
#1596 = CARTESIAN_POINT ( 'NONE',  ( 7.896254658894418021, 108.7892918275420016, 1.307282859663298158 ) ) ;
#1597 = CARTESIAN_POINT ( 'NONE',  ( 13.32650251567469724, -14.66737781475426416, 31.72147017887533949 ) ) ;
#1600 = AXIS2_PLACEMENT_3D ( 'NONE', #2844, #83238, #34731 ) ;
#1599 = CARTESIAN_POINT ( 'NONE',  ( -15.26425464274176491, 22.59372108562831016, -2.835904228628532309 ) ) ;
#1598 = CARTESIAN_POINT ( 'NONE',  ( -44.47534256803313468, -38.31161230092084224, 57.00189278798902137 ) ) ;
#1601 = CARTESIAN_POINT ( 'NONE',  ( -9.798380800342664898, 88.46800654315505597, -2.010350564680321472 ) ) ;
#1602 = FACE_OUTER_BOUND ( 'NONE', #92437, .T. ) ;
#1603 = DIRECTION ( 'NONE',  ( 0.000000000000000000, -0.000000000000000000, 1.000000000000000000 ) ) ;
#1604 = DIRECTION ( 'NONE',  ( 0.000000000000000000, -0.000000000000000000, 1.000000000000000000 ) ) ;
#1605 = CIRCLE ( 'NONE', #75690, 3.309499999999999886 ) ;
#1606 = ORIENTED_EDGE ( 'NONE', *, *, #52137, .F. ) ;
#1607 = CARTESIAN_POINT ( 'NONE',  ( -40.04958995022020929, -32.98584746607007645, -37.46495261379590858 ) ) ;
#1608 = CARTESIAN_POINT ( 'NONE',  ( -19.01558148378874691, 49.54233067771259869, 61.88543008401511258 ) ) ;
#1609 = DIRECTION ( 'NONE',  ( -1.000000000000000000, -1.224606353822377258E-16, -0.000000000000000000 ) ) ;
#1610 = CARTESIAN_POINT ( 'NONE',  ( -39.43526690229246867, 464.6969442309963938, 18.30945923499460903 ) ) ;
#1611 = ADVANCED_FACE ( 'NONE', ( #43741 ), #18978, .F. ) ;
#1613 = CARTESIAN_POINT ( 'NONE',  ( 40.94348386959299546, -34.58951997928637212, -29.39300229961106581 ) ) ;
#1612 = CARTESIAN_POINT ( 'NONE',  ( 30.00000000000000000, 488.8442721620239126, 4.433647275927487641 ) ) ;
#1614 = ORIENTED_EDGE ( 'NONE', *, *, #70657, .F. ) ;
#1615 = AXIS2_PLACEMENT_3D ( 'NONE', #32685, #33207, #100568 ) ;
#1616 = CARTESIAN_POINT ( 'NONE',  ( -5.384233811324310892, -88.00217091344775611, 2.655407383564611923 ) ) ;
#1617 =( NAMED_UNIT ( * ) SI_UNIT ( $, .STERADIAN. ) SOLID_ANGLE_UNIT ( ) );
#1618 = VERTEX_POINT ( 'NONE', #100378 ) ;
#1619 = ADVANCED_FACE ( 'NONE', ( #74503 ), #18535, .T. ) ;
#1620 = CARTESIAN_POINT ( 'NONE',  ( 0.000000000000000000, 4.898587196589412829E-16, -4.000000000000000000 ) ) ;
#1621 = CARTESIAN_POINT ( 'NONE',  ( 30.93163070004071358, 9.246556120444319404, -40.70059110212535103 ) ) ;
#1622 = AXIS2_PLACEMENT_3D ( 'NONE', #22279, #78353, #70278 ) ;
#1623 = DIRECTION ( 'NONE',  ( 0.000000000000000000, 1.000000000000000000, 0.000000000000000000 ) ) ;
#1624 = CARTESIAN_POINT ( 'NONE',  ( -103.9547180768905008, -60.00000000000000000, 104.1795586391435791 ) ) ;
#1625 = CARTESIAN_POINT ( 'NONE',  ( 6.231493956936416723, 147.8264543773111654, -5.000000000000000000 ) ) ;
#1626 = CARTESIAN_POINT ( 'NONE',  ( 61.85555555555556140, 6.915964383211875250E-15, 0.000000000000000000 ) ) ;
#1627 = DIRECTION ( 'NONE',  ( 1.000000000000000000, 0.000000000000000000, 0.000000000000000000 ) ) ;
#1628 = CARTESIAN_POINT ( 'NONE',  ( 40.76154164607566344, 460.9888869747084073, 2.282783108351458701 ) ) ;
#1629 = B_SPLINE_CURVE_WITH_KNOTS ( 'NONE', 3,
 ( #13810, #21418, #95819, #38652, #46205, #71519, #55328, #39707, #88255, #72582, #96871, #105485, #45676, #13277, #64511, #79091, #23538, #86682, #12753, #78556, #4686, #37619, #70482, #103377, #57443, #17558, #32692, #16477, #91444, #65559, #97919, #66619, #17021, #106000 ),
 .UNSPECIFIED., .F., .F.,
 ( 4, 2, 2, 2, 2, 2, 2, 2, 2, 2, 2, 2, 2, 2, 2, 2, 4 ),
 ( 1.734723475976807094E-18, 0.0007951492273476417835, 0.001590298454695281832, 0.002385447682042921881, 0.003180596909390559762, 0.003975746136738197642, 0.004770895364085835089, 0.005566044591433473403, 0.006361193818781110849, 0.007156343046128746561, 0.007951492273476384876, 0.008746641500824020588, 0.009541790728171659769, 0.01033693995551929548, 0.01113208918286693293, 0.01192723841021457037, 0.01272238763756220782 ),
 .UNSPECIFIED. ) ;
#1631 = CARTESIAN_POINT ( 'NONE',  ( 0.000000000000000000, 0.000000000000000000, -0.9215586320570148260 ) ) ;
#1630 = CARTESIAN_POINT ( 'NONE',  ( -1.308996937483428491, -5.000000000000002665, -75.00000000000001421 ) ) ;
#1632 = CONICAL_SURFACE ( 'NONE', #70583, 3.309500000000001663, 0.9599310885968770357 ) ;
#1633 = CARTESIAN_POINT ( 'NONE',  ( -83.58190473302030910, -35.99179951698813085, 169.8173457906621877 ) ) ;
#1634 = ORIENTED_EDGE ( 'NONE', *, *, #54089, .T. ) ;
#1635 =( NAMED_UNIT ( * ) SI_UNIT ( $, .STERADIAN. ) SOLID_ANGLE_UNIT ( ) );
#1636 = VERTEX_POINT ( 'NONE', #27608 ) ;
#1637 =( BOUNDED_SURFACE ( )  B_SPLINE_SURFACE ( 3, 2, ( 
 ( #12824, #20989, #61951 ),
 ( #94844, #37694, #53822 ),
 ( #11763, #68435, #45744 ),
 ( #43611, #18850, #51695 ),
 ( #26940, #93232, #86754 ),
 ( #93768, #61413, #86229 ),
 ( #94305, #60878, #84612 ),
 ( #78621, #4755, #3703 ),
 ( #69495, #20468, #10697 ),
 ( #2612, #19394, #52226 ),
 ( #85137, #11229, #44154 ),
 ( #77043, #3159, #45228 ) ),
 .UNSPECIFIED., .F., .F., .T. ) 
 B_SPLINE_SURFACE_WITH_KNOTS ( ( 4, 2, 2, 2, 2, 4 ),
 ( 3, 3 ),
 ( 0.000000000000000000, 0.0007735885786023083931, 0.001547177157204616786, 0.001933971446505770983, 0.002320765735806925179, 0.003094354314409233572 ),
 ( 0.000000000000000000, 1.000000000000000000 ),
 .UNSPECIFIED. ) 
 GEOMETRIC_REPRESENTATION_ITEM ( )  RATIONAL_B_SPLINE_SURFACE ( (
 ( 1.000000000000000000, 0.9603284238771501169, 1.000000000000000000),
 ( 1.000000000000000000, 0.9628724889917420482, 1.000000000000000000),
 ( 1.000000000000000000, 0.9663306537743326929, 1.000000000000000000),
 ( 1.000000000000000000, 0.9744563874115806934, 1.000000000000000000),
 ( 1.000000000000000000, 0.9789903143386278206, 1.000000000000000000),
 ( 1.000000000000000000, 0.9855527733005997604, 1.000000000000000000),
 ( 1.000000000000000000, 0.9877025284828834240, 1.000000000000000000),
 ( 1.000000000000000000, 0.9916277982505393718, 1.000000000000000000),
 ( 1.000000000000000000, 0.9934221110297505319, 1.000000000000000000),
 ( 1.000000000000000000, 0.9980179737617284053, 1.000000000000000000),
 ( 1.000000000000000000, 1.000016370385679254, 1.000000000000000000),
 ( 1.000000000000000000, 1.000000000000000000, 1.000000000000000000) ) ) 
 REPRESENTATION_ITEM ( '' )  SURFACE ( )  );
#1638 = VERTEX_POINT ( 'NONE', #16817 ) ;
#1639 = DIRECTION ( 'NONE',  ( -0.000000000000000000, 1.000000000000000000, -0.000000000000000000 ) ) ;
#1640 = EDGE_CURVE ( 'NONE', #57615, #33722, #26541, .T. ) ;
#1641 = DIRECTION ( 'NONE',  ( -1.000000000000000000, 0.000000000000000000, 0.000000000000000000 ) ) ;
#1642 = ORIENTED_EDGE ( 'NONE', *, *, #96728, .F. ) ;
#1643 = CARTESIAN_POINT ( 'NONE',  ( -5.420469775605654128, 41.88321586335170821, -59.04137891894603030 ) ) ;
#1644 = DIRECTION ( 'NONE',  ( -0.000000000000000000, -1.000000000000000000, -0.000000000000000000 ) ) ;
#1645 = CARTESIAN_POINT ( 'NONE',  ( 100.0424503805845831, 1.016364837396684119E-14, 0.000000000000000000 ) ) ;
#1646 = CARTESIAN_POINT ( 'NONE',  ( -2.649051870092321792, 14.84475683689757908, 6.482396460464982191 ) ) ;
#1647 = CARTESIAN_POINT ( 'NONE',  ( -1.102159017229340288, 53.60731710284914442, 9.611294474598382820 ) ) ;
#1648 = CARTESIAN_POINT ( 'NONE',  ( -7.500000000000007105, -3.000000000000000000, -68.91429205785459544 ) ) ;
#1649 = CARTESIAN_POINT ( 'NONE',  ( 4.699999999999999289, 3.752776749732569694, 6.499999999999997335 ) ) ;
#1650 = AXIS2_PLACEMENT_3D ( 'NONE', #82261, #57440, #81191 ) ;
#1651 = CARTESIAN_POINT ( 'NONE',  ( 95.23263947746859515, -60.00000000000000000, 30.92889862699057701 ) ) ;
#1652 = CARTESIAN_POINT ( 'NONE',  ( -96.06797501213969781, -14.21045842199444564, 198.0637310406154938 ) ) ;
#1653 = EDGE_CURVE ( 'NONE', #101821, #58545, #98801, .T. ) ;
#1654 = CARTESIAN_POINT ( 'NONE',  ( -57.59724535810557455, -36.02309701339866166, 64.66795058115701522 ) ) ;
#1655 = ORIENTED_EDGE ( 'NONE', *, *, #106374, .F. ) ;
#1656 = CARTESIAN_POINT ( 'NONE',  ( 6.322210203194782885, 15.64510924972225681, 3.011395388464980005 ) ) ;
#1657 = CARTESIAN_POINT ( 'NONE',  ( 14.02564712579228434, -60.00000000000000000, -44.59530358871077027 ) ) ;
#1658 = ORIENTED_EDGE ( 'NONE', *, *, #78441, .T. ) ;
#1659 = CARTESIAN_POINT ( 'NONE',  ( 7.080836988906568763, -32.51043656205519028, 29.29839389023845087 ) ) ;
#1661 = CARTESIAN_POINT ( 'NONE',  ( -102.7591849661067585, -37.82055285979338777, 174.7714434000731387 ) ) ;
#1660 = CIRCLE ( 'NONE', #84139, 56.85174851683467523 ) ;
#1662 = FACE_OUTER_BOUND ( 'NONE', #43469, .T. ) ;
#1663 = FILL_AREA_STYLE_COLOUR ( '', #80458 ) ;
#1664 = CARTESIAN_POINT ( 'NONE',  ( 16.06569373956322266, 42.44590539575593624, -88.41332270392955195 ) ) ;
#1665 = ORIENTED_EDGE ( 'NONE', *, *, #86180, .T. ) ;
#1666 = CARTESIAN_POINT ( 'NONE',  ( -2.216488688100141324, -14.30876692738957345, -0.5344654698446129615 ) ) ;
#1667 = CARTESIAN_POINT ( 'NONE',  ( -30.55841257715690062, -60.00000000000000000, 43.32489242905028703 ) ) ;
#1668 = CARTESIAN_POINT ( 'NONE',  ( 36.44054363913070205, 26.07465808859272371, -11.65710653164109445 ) ) ;
#1669 = CARTESIAN_POINT ( 'NONE',  ( 7.188101187499999156, -19.62500000204838457, 2.977408999572654924 ) ) ;
#1670 = FACE_OUTER_BOUND ( 'NONE', #60073, .T. ) ;
#1671 = DIRECTION ( 'NONE',  ( 0.000000000000000000, 0.000000000000000000, 1.000000000000000000 ) ) ;
#1672 = CARTESIAN_POINT ( 'NONE',  ( 6.943926999490791729, -84.46699007373852908, -3.973092371898547803 ) ) ;
#1673 = CARTESIAN_POINT ( 'NONE',  ( -27.57151080649627417, 314.0751515626058676, 12.18133379269485239 ) ) ;
#1674 = CARTESIAN_POINT ( 'NONE',  ( 27.97565635352651015, 315.9216507687758053, 12.64980990155120999 ) ) ;
#1675 =( BOUNDED_SURFACE ( )  B_SPLINE_SURFACE ( 3, 2, ( 
 ( #57212, #90131, #543 ),
 ( #82570, #32983, #58291 ),
 ( #98215, #42104, #16233 ),
 ( #41050, #9723, #66380 ),
 ( #56686, #89609, #8675 ),
 ( #17854, #49118, #40515 ),
 ( #98732, #91735, #82018 ),
 ( #16774, #7597, #41577 ) ),
 .UNSPECIFIED., .F., .F., .F. ) 
 B_SPLINE_SURFACE_WITH_KNOTS ( ( 4, 2, 2, 4 ),
 ( 3, 3 ),
 ( 0.006812271038101246068, 0.007673844606678349028, 0.008535418175255451989, 0.01025856531240965618 ),
 ( 0.1554254205220907958, 1.000000000000000000 ),
 .UNSPECIFIED. ) 
 GEOMETRIC_REPRESENTATION_ITEM ( )  RATIONAL_B_SPLINE_SURFACE ( (
 ( 0.9279458904032336086, 0.7682035880786783899, 1.000000000000000000),
 ( 0.9304043519111940830, 0.7761124021571679243, 1.000000000000000000),
 ( 0.9321886790048431459, 0.7818525413430721382, 1.000000000000000000),
 ( 0.9342334009477870627, 0.7884303647649926194, 1.000000000000000000),
 ( 0.9344904078379445700, 0.7892571500144520691, 1.000000000000000000),
 ( 0.9330319136750675479, 0.7845652078663214457, 1.000000000000000000),
 ( 0.9290861136362296158, 0.7718716599718282723, 1.000000000000000000),
 ( 0.9231047755039956115, 0.7526298328880023369, 1.000000000000000000) ) ) 
 REPRESENTATION_ITEM ( '' )  SURFACE ( )  );
#1676 = CARTESIAN_POINT ( 'NONE',  ( -9.647567108638854805, 44.08445422138064629, -13.07998335409894253 ) ) ;
#1677 = EDGE_CURVE ( 'NONE', #46768, #83885, #76100, .T. ) ;
#1678 = FILL_AREA_STYLE ('',( #40557 ) ) ;
#1679 = CARTESIAN_POINT ( 'NONE',  ( 86.88755769280966490, -60.00000000000002132, -3.487599879275609105 ) ) ;
#1680 = UNCERTAINTY_MEASURE_WITH_UNIT (LENGTH_MEASURE( 1.000000000000000082E-05 ), #104797, 'distance_accuracy_value', 'NONE');
#1681 = CARTESIAN_POINT ( 'NONE',  ( -30.23497050974513201, -36.01572923412079774, 32.58813699357081362 ) ) ;
#1682 = AXIS2_PLACEMENT_3D ( 'NONE', #84062, #77570, #2597 ) ;
#1683 = CARTESIAN_POINT ( 'NONE',  ( 32.82691535583474973, 485.1045372766795367, 1.724905475515037701 ) ) ;
#1684 = CARTESIAN_POINT ( 'NONE',  ( 44.36345712709423594, -18.78927584261837680, 37.46452360639921864 ) ) ;
#1685 = CARTESIAN_POINT ( 'NONE',  ( 8.000000000000000000, -13.90624999999999289, -3.313708498984761164 ) ) ;
#1686 = VERTEX_POINT ( 'NONE', #17893 ) ;
#1687 = CARTESIAN_POINT ( 'NONE',  ( 43.79395675348460060, 434.3550296691302037, 12.19643612484853001 ) ) ;
#1688 = MECHANICAL_DESIGN_GEOMETRIC_PRESENTATION_REPRESENTATION (  '', ( #24143 ), #101559 ) ;
#1689 = CARTESIAN_POINT ( 'NONE',  ( -79.44558119418380215, -38.73421251888159844, 191.9379437533855821 ) ) ;
#1690 = ORIENTED_EDGE ( 'NONE', *, *, #35369, .F. ) ;
#1692 = CARTESIAN_POINT ( 'NONE',  ( 14.54015256618498775, 9.738273119607207207, 0.000000000000000000 ) ) ;
#1691 = CARTESIAN_POINT ( 'NONE',  ( 0.000000000000000000, 0.1588408748199928722, 0.000000000000000000 ) ) ;
#1693 = CARTESIAN_POINT ( 'NONE',  ( 71.97178132980937448, -59.99999999999997868, 122.5137839838858866 ) ) ;
#1694 = CYLINDRICAL_SURFACE ( 'NONE', #944, 4.000000000000002665 ) ;
#1695 = CARTESIAN_POINT ( 'NONE',  ( -7.439139359426217624, 41.00331351352566145, -59.84461297751296627 ) ) ;
#1696 = CARTESIAN_POINT ( 'NONE',  ( -2.500000000000002220, 1.714505518806294638E-15, -14.00000000000000000 ) ) ;
#1697 = DIRECTION ( 'NONE',  ( 0.000000000000000000, -1.000000000000000000, 0.000000000000000000 ) ) ;
#1698 = CARTESIAN_POINT ( 'NONE',  ( -27.21876204780540220, 312.2794116683786569, 10.72559560151416669 ) ) ;
#1699 = CARTESIAN_POINT ( 'NONE',  ( 17.88790647107491694, 45.31130133375065583, 5.552611910812898621 ) ) ;
#1700 = CONICAL_SURFACE ( 'NONE', #53145, 5.000000000000010658, 0.9599310885968697082 ) ;
#1701 = CARTESIAN_POINT ( 'NONE',  ( 109.9795466629233118, -59.99999999999998579, 143.2892139239177425 ) ) ;
#1702 = CARTESIAN_POINT ( 'NONE',  ( 38.58349330513380693, 1.593028355512270567E-15, 0.000000000000000000 ) ) ;
#1703 = COLOUR_RGB ( '', 0.66274510, 0.83137255, 0.94901961) ;
#1704 = EDGE_LOOP ( 'NONE', ( #80984, #96917, #80755, #5682 ) ) ;
#1705 = EDGE_CURVE ( 'NONE', #20613, #71082, #8712, .T. ) ;
#1706 = CARTESIAN_POINT ( 'NONE',  ( -88.09576673204246333, -30.00000000000004619, 187.0129754708849816 ) ) ;
#1707 = EDGE_LOOP ( 'NONE', ( #12150, #104339, #21184, #103283, #98378 ) ) ;
#1708 = CIRCLE ( 'NONE', #68888, 4.000000000000007105 ) ;
#1709 = LINE ( 'NONE', #51860, #59701 ) ;
#1710 = CARTESIAN_POINT ( 'NONE',  ( 43.03265099500004709, 484.2747968070555089, -0.8099405866658345721 ) ) ;
#1711 = CARTESIAN_POINT ( 'NONE',  ( 29.60994972707265305, 319.5812630551522489, 13.80934071871660151 ) ) ;
#1712 = CARTESIAN_POINT ( 'NONE',  ( 35.11650669486618170, 0.000000000000000000, 4.000000000000000888 ) ) ;
#1713 = CARTESIAN_POINT ( 'NONE',  ( -7.188101187500001821, -18.87500000204838457, -2.977408999572651371 ) ) ;
#1714 = ADVANCED_FACE ( 'NONE', ( #83651 ), #83964, .T. ) ;
#1715 = CARTESIAN_POINT ( 'NONE',  ( -10.48543666094594862, -5.000000000000002665, -91.04342776276726568 ) ) ;
#1716 = EDGE_CURVE ( 'NONE', #56185, #45991, #15032, .T. ) ;
#1717 = TOROIDAL_SURFACE ( 'NONE', #91292, 8.331345277524542681, 0.6186547224754556096 ) ;
#1718 = UNCERTAINTY_MEASURE_WITH_UNIT (LENGTH_MEASURE( 1.000000000000000082E-05 ), #26069, 'distance_accuracy_value', 'NONE');
#1719 = CARTESIAN_POINT ( 'NONE',  ( -43.51084452654468748, 465.2903130129606666, 9.421687747985890482 ) ) ;
#1721 = ORIENTED_EDGE ( 'NONE', *, *, #73541, .F. ) ;
#1720 = CARTESIAN_POINT ( 'NONE',  ( -40.34377797254171583, 485.2472197438310104, -4.812374094186917084 ) ) ;
#1722 = CARTESIAN_POINT ( 'NONE',  ( 81.94408366797206611, -39.49612657794242665, 160.0900498601838819 ) ) ;
#1723 = AXIS2_PLACEMENT_3D ( 'NONE', #90274, #56829, #76068 ) ;
#1724 = CARTESIAN_POINT ( 'NONE',  ( -46.00000000000000000, 460.6862940191606981, 7.630022560101465068 ) ) ;
#1725 = VERTEX_POINT ( 'NONE', #11351 ) ;
#1726 = CARTESIAN_POINT ( 'NONE',  ( -0.07733840395782722033, 18.87382441218279894, -49.24999999999998579 ) ) ;
#1727 = FACE_OUTER_BOUND ( 'NONE', #56464, .T. ) ;
#1728 = CARTESIAN_POINT ( 'NONE',  ( 30.00000000000184031, 486.6562833505878416, 5.030808486058892193 ) ) ;
#1729 =( LENGTH_UNIT ( ) NAMED_UNIT ( * ) SI_UNIT ( .MILLI., .METRE. ) );
#1730 = CARTESIAN_POINT ( 'NONE',  ( -32.53853074909311971, 344.3203851192521370, 19.65648080016363508 ) ) ;
#1731 = CARTESIAN_POINT ( 'NONE',  ( 99.17777777777777715, 1.023464760207051730E-14, 0.000000000000000000 ) ) ;
#1732 = ORIENTED_EDGE ( 'NONE', *, *, #22739, .T. ) ;
#1733 = UNCERTAINTY_MEASURE_WITH_UNIT (LENGTH_MEASURE( 1.000000000000000082E-05 ), #70336, 'distance_accuracy_value', 'NONE');
#1734 = CARTESIAN_POINT ( 'NONE',  ( -6.500000000000000888, 0.000000000000000000, 1.734723475976807094E-15 ) ) ;
#1735 = CARTESIAN_POINT ( 'NONE',  ( -1.000000000000000000, -70.02685735654881682, 13.01550610203317682 ) ) ;
#1736 = CARTESIAN_POINT ( 'NONE',  ( 86.98622367796362198, -24.32005973283799705, 186.4277034656624039 ) ) ;
#1737 = B_SPLINE_CURVE_WITH_KNOTS ( 'NONE', 3,
 ( #77779, #21176, #103636, #78821 ),
 .UNSPECIFIED., .F., .F.,
 ( 4, 4 ),
 ( 0.000000000000000000, 0.0005776816123952190898 ),
 .UNSPECIFIED. ) ;
#1738 = CARTESIAN_POINT ( 'NONE',  ( -6.249999999999997335, 5.051814855409221927, -7.198902722707427593 ) ) ;
#1739 = CARTESIAN_POINT ( 'NONE',  ( -8.000000000000001776, -8.843750004096769146, 3.313708498984758943 ) ) ;
#1740 = CARTESIAN_POINT ( 'NONE',  ( 13.63088759365579428, 294.5432864296589628, -2.065629630185572552 ) ) ;
#1741 = CARTESIAN_POINT ( 'NONE',  ( -14.29190075645648683, 6.456385560661901835, 7.561819230138081771 ) ) ;
#1742 = CARTESIAN_POINT ( 'NONE',  ( 14.29190075645216673, 6.456385560668102208, 7.561819230143447257 ) ) ;
#1743 = VERTEX_POINT ( 'NONE', #86357 ) ;
#1744 = CARTESIAN_POINT ( 'NONE',  ( 2.848917157793759055E-13, 44.08548369317517768, 16.24999999999732836 ) ) ;
#1745 = CARTESIAN_POINT ( 'NONE',  ( 56.96666666666666856, -3.309500000000000774, 0.000000000000000000 ) ) ;
#1746 = CARTESIAN_POINT ( 'NONE',  ( -9.999806008763298948, 7.500277120283445953, -4.999999999999999112 ) ) ;
#1747 = EDGE_CURVE ( 'NONE', #103314, #69385, #75329, .T. ) ;
#1748 = ORIENTED_EDGE ( 'NONE', *, *, #17744, .T. ) ;
#1749 = CARTESIAN_POINT ( 'NONE',  ( 1.224646799147353256E-15, -80.00000000000000000, 17.00000000000000000 ) ) ;
#1750 = FILL_AREA_STYLE_COLOUR ( '', #27264 ) ;
#1751 = EDGE_LOOP ( 'NONE', ( #16896, #102287, #65721, #16262 ) ) ;
#1752 = ADVANCED_FACE ( 'NONE', ( #101972 ), #90896, .T. ) ;
#1753 = CARTESIAN_POINT ( 'NONE',  ( 31.88318484955206955, 435.8726686874541656, 17.58993604645352349 ) ) ;
#1754 = CARTESIAN_POINT ( 'NONE',  ( -1.168005587324537631, 9.591777280503173131, -50.96219972952603428 ) ) ;
#1755 = CARTESIAN_POINT ( 'NONE',  ( 1.448103213439550618, -5.000000000000000888, -72.00403106213767046 ) ) ;
#1756 = CARTESIAN_POINT ( 'NONE',  ( 4.269533675236951709, 302.8261475636076625, 9.931633460720737716 ) ) ;
#1757 = CARTESIAN_POINT ( 'NONE',  ( -90.88092632026551598, -60.00000000000000711, 202.1567407304452502 ) ) ;
#1758 = CARTESIAN_POINT ( 'NONE',  ( 9.658290426964626363, 43.42980812226979026, -15.25060361923008045 ) ) ;
#1759 = CARTESIAN_POINT ( 'NONE',  ( 67.96666666666666856, 6.915964383211875250E-15, 0.000000000000000000 ) ) ;
#1760 = FACE_OUTER_BOUND ( 'NONE', #32612, .T. ) ;
#1761 = CARTESIAN_POINT ( 'NONE',  ( -86.20286142257957351, -21.32224752070146323, 177.4588804251129375 ) ) ;
#1762 = ORIENTED_EDGE ( 'NONE', *, *, #53785, .F. ) ;
#1763 = PRESENTATION_STYLE_ASSIGNMENT (( #102066 ) ) ;
#1764 = AXIS2_PLACEMENT_3D ( 'NONE', #100011, #42843, #84374 ) ;
#1765 = CIRCLE ( 'NONE', #84495, 4.000000000000001776 ) ;
#1766 = VERTEX_POINT ( 'NONE', #37282 ) ;
#1767 = FACE_OUTER_BOUND ( 'NONE', #16568, .T. ) ;
#1768 = EDGE_CURVE ( 'NONE', #52464, #53278, #44388, .T. ) ;
#1769 = CARTESIAN_POINT ( 'NONE',  ( -86.97516054069694746, -60.21813631295302827, -9.169555333803231179 ) ) ;
#1770 = B_SPLINE_CURVE_WITH_KNOTS ( 'NONE', 3,
 ( #61089, #13033, #85908, #11982, #45960, #78842, #70760, #103656, #29805, #3376, #36841, #69708, #102601, #28753, #76715, #93458, #19606, #61636, #62681, #2826, #19070, #35782, #94527, #68660 ),
 .UNSPECIFIED., .F., .F.,
 ( 4, 2, 2, 2, 2, 2, 2, 2, 2, 2, 2, 4 ),
 ( 0.004982501964703170937, 0.005234564667989256501, 0.005486627371275342065, 0.005990752777847506254, 0.006494878184419670443, 0.006999003590991834632, 0.007251066294277914992, 0.007503128997563995352, 0.008007254404136160408, 0.008511379810708322863, 0.008763442513994400621, 0.009015505217280478378 ),
 .UNSPECIFIED. ) ;
#1771 = CIRCLE ( 'NONE', #8639, 3.309500000000001663 ) ;
#1772 = CARTESIAN_POINT ( 'NONE',  ( -4.000000000000000000, 0.000000000000000000, -4.567799999999999194 ) ) ;
#1773 = CARTESIAN_POINT ( 'NONE',  ( -15.90614609307868399, -3.157894736842107530, 14.66382285868950675 ) ) ;
#1774 = CARTESIAN_POINT ( 'NONE',  ( 28.08444336946503483, 36.49846905662621310, -8.013953787025748454 ) ) ;
#1775 = CARTESIAN_POINT ( 'NONE',  ( 90.56128410203886858, 42.00000000000000000, -11.85444436786857558 ) ) ;
#1776 = CARTESIAN_POINT ( 'NONE',  ( 29.34999999999999787, 1.533819458162526451E-15, 0.000000000000000000 ) ) ;
#1777 = CARTESIAN_POINT ( 'NONE',  ( 68.01663869669266660, -29.99999999999994316, 119.4502877181080862 ) ) ;
#1778 = CARTESIAN_POINT ( 'NONE',  ( -36.59119455513882713, 438.2489652597741383, 3.879698295689448351 ) ) ;
#1779 = AXIS2_PLACEMENT_3D ( 'NONE', #25073, #81145, #33164 ) ;
#1780 = CARTESIAN_POINT ( 'NONE',  ( -94.55497525217361954, -59.99999999999993605, 22.39874202688834615 ) ) ;
#1781 = CARTESIAN_POINT ( 'NONE',  ( -75.39866320161442559, -36.02139133080472533, 119.8324419168973378 ) ) ;
#1782 = ORIENTED_EDGE ( 'NONE', *, *, #40887, .T. ) ;
#1783 = CARTESIAN_POINT ( 'NONE',  ( 74.04755006654457361, -14.21045842199432307, 133.5027151116648838 ) ) ;
#1784 = CARTESIAN_POINT ( 'NONE',  ( 59.27219564965441378, 40.83785294361205587, 26.84540320310011197 ) ) ;
#1785 = CARTESIAN_POINT ( 'NONE',  ( 42.88790708626195425, -60.00000000000487432, 61.60924055822990653 ) ) ;
#1786 = EDGE_LOOP ( 'NONE', ( #101838, #61211, #49411, #867 ) ) ;
#1787 = CARTESIAN_POINT ( 'NONE',  ( 23.73746414932995208, 1.482358050883964840E-15, 0.000000000000000000 ) ) ;
#1788 = CARTESIAN_POINT ( 'NONE',  ( -1.320432766682874540E-15, -25.90625000204838813, 7.188101187500000044 ) ) ;
#1789 = CONICAL_SURFACE ( 'NONE', #101672, 4.000000000000001776, 0.9599310885968808105 ) ;
#1790 = FACE_OUTER_BOUND ( 'NONE', #50901, .T. ) ;
#1791 = ORIENTED_EDGE ( 'NONE', *, *, #20378, .T. ) ;
#1792 = FILL_AREA_STYLE ('',( #77832 ) ) ;
#1793 = CARTESIAN_POINT ( 'NONE',  ( 3.585532980576127571, 16.06055535235176635, -6.013159465609652088 ) ) ;
#1794 = CARTESIAN_POINT ( 'NONE',  ( -28.99999999999998934, 1.102182119232617714E-15, 9.000000000000000000 ) ) ;
#1795 = CARTESIAN_POINT ( 'NONE',  ( 26.33485479066055746, 305.7717630634953707, -9.578373927320027903 ) ) ;
#1796 = CARTESIAN_POINT ( 'NONE',  ( -1.320432766682874540E-15, -15.03125000204838457, 7.188101187500000044 ) ) ;
#1797 = DIRECTION ( 'NONE',  ( 8.673617379884035472E-17, 0.000000000000000000, 1.000000000000000000 ) ) ;
#1798 = DIRECTION ( 'NONE',  ( -1.000000000000000000, -0.000000000000000000, -0.000000000000000000 ) ) ;
#1799 = CARTESIAN_POINT ( 'NONE',  ( 0.000000000000000000, 4.898587196589413815E-16, -4.000000000000000888 ) ) ;
#1800 = CARTESIAN_POINT ( 'NONE',  ( 4.898587196589412829E-16, -15.12499999999999289, -8.000000000000000000 ) ) ;
#1801 = CARTESIAN_POINT ( 'NONE',  ( 4.644559862127829675, 48.00000000000000711, -99.31133601631377417 ) ) ;
#1802 = VERTEX_POINT ( 'NONE', #20599 ) ;
#1803 = CARTESIAN_POINT ( 'NONE',  ( -7.499934961134938405, 40.55407393519936221, -69.64904099334012244 ) ) ;
#1804 = CARTESIAN_POINT ( 'NONE',  ( 32.43724909693664671, -42.96036988411042046, 34.72672468598132411 ) ) ;
#1805 = COLOUR_RGB ( '', 0.09019608, 0.27058824, 0.51372549) ;
#1806 = CARTESIAN_POINT ( 'NONE',  ( 35.19894401196863498, 355.5759600829595684, 2.569406999161085281 ) ) ;
#1807 = ORIENTED_EDGE ( 'NONE', *, *, #14201, .F. ) ;
#1808 = CARTESIAN_POINT ( 'NONE',  ( -0.8435576335715310181, 13.67164987635283246, 51.42579297825043483 ) ) ;
#1809 = AXIS2_PLACEMENT_3D ( 'NONE', #3719, #4238, #38229 ) ;
#1810 = ORIENTED_EDGE ( 'NONE', *, *, #86807, .F. ) ;
#1812 = CARTESIAN_POINT ( 'NONE',  ( 18.00000000000000355, 12.99999999999999289, 0.000000000000000000 ) ) ;
#1811 = DIRECTION ( 'NONE',  ( -0.000000000000000000, -1.000000000000000000, -0.000000000000000000 ) ) ;
#1813 = CARTESIAN_POINT ( 'NONE',  ( 43.00000000000000000, 485.2629658518202405, -2.796394914059364911 ) ) ;
#1814 = CARTESIAN_POINT ( 'NONE',  ( -33.13462985527915805, 435.1334760212066044, 11.13098077912248307 ) ) ;
#1815 = FACE_OUTER_BOUND ( 'NONE', #62603, .T. ) ;
#1816 = CARTESIAN_POINT ( 'NONE',  ( 32.68851106861551159, 465.0799323318228176, 13.83425062237051151 ) ) ;
#1817 = CARTESIAN_POINT ( 'NONE',  ( 1.160281544699517831, 17.00865987995647544, -50.01912393708035154 ) ) ;
#1818 = ORIENTED_EDGE ( 'NONE', *, *, #44327, .T. ) ;
#1819 = CARTESIAN_POINT ( 'NONE',  ( 81.10482683381307822, -59.99999999999998579, -27.27273203502905119 ) ) ;
#1820 = FACE_OUTER_BOUND ( 'NONE', #14130, .T. ) ;
#1821 = CARTESIAN_POINT ( 'NONE',  ( 5.947762761376478302, -4.378239541354659536, 5.416666666666666075 ) ) ;
#1822 = CARTESIAN_POINT ( 'NONE',  ( 13.09999999999999787, 1.533819458162526451E-15, 0.000000000000000000 ) ) ;
#1823 = DIRECTION ( 'NONE',  ( -1.000000000000000000, -1.224606353822377258E-16, -0.000000000000000000 ) ) ;
#1824 = EDGE_LOOP ( 'NONE', ( #9401, #76936, #1087, #43914, #53407 ) ) ;
#1825 = EDGE_CURVE ( 'NONE', #84857, #42272, #85672, .T. ) ;
#1826 = ADVANCED_FACE ( 'NONE', ( #21110 ), #60489, .F. ) ;
#1827 = CARTESIAN_POINT ( 'NONE',  ( 37.06438722625302518, 1.482358050883964840E-15, 0.000000000000000000 ) ) ;
#1828 = ORIENTED_EDGE ( 'NONE', *, *, #21149, .T. ) ;
#1829 = ORIENTED_EDGE ( 'NONE', *, *, #76927, .F. ) ;
#1830 = VECTOR ( 'NONE', #98914, 1000.000000000000114 ) ;
#1831 = CARTESIAN_POINT ( 'NONE',  ( 7.046289519167722837, 83.69408180055623347, -3.789821819998813623 ) ) ;
#1832 = CARTESIAN_POINT ( 'NONE',  ( 6.169949891408690767, -4.949864754179921889, -4.426582755168041672 ) ) ;
#1833 = CARTESIAN_POINT ( 'NONE',  ( 0.2578475836320682779, 4.367703157927327773, -5.434916218090833695 ) ) ;
#1834 = DIRECTION ( 'NONE',  ( -0.000000000000000000, -0.000000000000000000, -1.000000000000000000 ) ) ;
#1835 = CARTESIAN_POINT ( 'NONE',  ( 86.89782702116733049, -60.22147714030394638, -10.09549994484113888 ) ) ;
#1836 = CARTESIAN_POINT ( 'NONE',  ( -30.99573784467934345, 309.3902544572148372, -8.491104135219801563 ) ) ;
#1837 = CARTESIAN_POINT ( 'NONE',  ( -20.24579557674103825, 304.8297271373346575, -10.00469232190999413 ) ) ;
#1838 = CARTESIAN_POINT ( 'NONE',  ( 12.50000000000000355, 27.37863077022358027, -44.93064604781708482 ) ) ;
#1839 = VERTEX_POINT ( 'NONE', #53941 ) ;
#1841 = EDGE_CURVE ( 'NONE', #99399, #47564, #36229, .T. ) ;
#1840 = CARTESIAN_POINT ( 'NONE',  ( -43.50377727019364471, 435.9167426301696082, 18.24083946424745761 ) ) ;
#1842 = ORIENTED_EDGE ( 'NONE', *, *, #18459, .F. ) ;
#1843 = LINE ( 'NONE', #42852, #91545 ) ;
#1844 = CYLINDRICAL_SURFACE ( 'NONE', #52417, 1.250000000000000222 ) ;
#1846 = VERTEX_POINT ( 'NONE', #93368 ) ;
#1845 = CARTESIAN_POINT ( 'NONE',  ( 5.290067270632321517, 52.08006895350504095, 6.031152949374479100 ) ) ;
#1847 = CARTESIAN_POINT ( 'NONE',  ( 75.40505029639432166, -56.84436558962719488, 136.0568600359671905 ) ) ;
#1848 = ORIENTED_EDGE ( 'NONE', *, *, #36708, .T. ) ;
#1849 = ADVANCED_FACE ( 'NONE', ( #36760 ), #102980, .T. ) ;
#1850 = CARTESIAN_POINT ( 'NONE',  ( 3.473244378093581108, -49.24695708051920207, 40.73076878102696696 ) ) ;
#1851 = PLANE ( 'NONE',  #78548 ) ;
#1852 = CARTESIAN_POINT ( 'NONE',  ( -2.977408999572654480, -25.62500000204838813, 7.188101187499999156 ) ) ;
#1853 = PRESENTATION_LAYER_ASSIGNMENT (  '', '', ( #105192 ) ) ;
#1854 = CARTESIAN_POINT ( 'NONE',  ( -93.98392372475152001, -57.65316015971099972, -14.13389826495936141 ) ) ;
#1855 = ORIENTED_EDGE ( 'NONE', *, *, #100383, .F. ) ;
#1856 = CIRCLE ( 'NONE', #32845, 4.000000000000000888 ) ;
#1857 = DIRECTION ( 'NONE',  ( 8.673617379884035472E-17, 0.000000000000000000, 1.000000000000000000 ) ) ;
#1859 = CARTESIAN_POINT ( 'NONE',  ( 102.7627937065603732, -45.28273124251436599, 186.5622291220291231 ) ) ;
#1858 = AXIS2_PLACEMENT_3D ( 'NONE', #74347, #24771, #17731 ) ;
#1860 = CARTESIAN_POINT ( 'NONE',  ( -37.24781850355250867, 27.71755434321492118, -13.42510649394979438 ) ) ;
#1861 = CIRCLE ( 'NONE', #29497, 5.000000000000010658 ) ;
#1862 = CARTESIAN_POINT ( 'NONE',  ( 0.000000000000000000, 0.000000000000000000, -11.82492182392400437 ) ) ;
#1863 = CARTESIAN_POINT ( 'NONE',  ( 8.000000000000000000, -26.18750000409677270, 0.000000000000000000 ) ) ;
#1864 = CARTESIAN_POINT ( 'NONE',  ( 11.08349330513380160, 1.593028355512270567E-15, 0.000000000000000000 ) ) ;
#1865 = CARTESIAN_POINT ( 'NONE',  ( -37.56673239365849781, 25.47613764497371136, 13.45617127781066280 ) ) ;
#1866 = CARTESIAN_POINT ( 'NONE',  ( -7.413000813362873309, 41.14546169070921877, -59.83891281791527916 ) ) ;
#1867 = DIRECTION ( 'NONE',  ( -1.000000000000000000, -1.224606353822377258E-16, -0.000000000000000000 ) ) ;
#1868 = CARTESIAN_POINT ( 'NONE',  ( 85.31310517497098544, 6.123233995736568081E-16, -5.000000000000011546 ) ) ;
#1869 = DIRECTION ( 'NONE',  ( 0.000000000000000000, 0.000000000000000000, 1.000000000000000000 ) ) ;
#1870 = FACE_OUTER_BOUND ( 'NONE', #101862, .T. ) ;
#1871 = ORIENTED_EDGE ( 'NONE', *, *, #41470, .F. ) ;
#1872 = CARTESIAN_POINT ( 'NONE',  ( 58.92761780597729881, -1.232595164407830946E-29, 4.000000000000007105 ) ) ;
#1873 = CARTESIAN_POINT ( 'NONE',  ( 13.37207953394533355, 1.482358050883964840E-15, 0.000000000000000000 ) ) ;
#1874 = CARTESIAN_POINT ( 'NONE',  ( -7.500000000000007105, -3.000000000000000000, -68.91429205785459544 ) ) ;
#1875 = CARTESIAN_POINT ( 'NONE',  ( -85.55157992948998924, -29.99999999999999645, 175.2523284361330411 ) ) ;
#1876 = EDGE_CURVE ( 'NONE', #596, #98741, #106344, .T. ) ;
#1877 = VECTOR ( 'NONE', #23294, 999.9999999999998863 ) ;
#1878 = EDGE_LOOP ( 'NONE', ( #32027, #39229, #67122, #48724, #5383, #100745 ) ) ;
#1879 = DIRECTION ( 'NONE',  ( 0.000000000000000000, -1.000000000000000000, 0.000000000000000000 ) ) ;
#1880 = CARTESIAN_POINT ( 'NONE',  ( 71.28015635268077688, -57.68069394656665594, 164.9132661665504145 ) ) ;
#1881 = TOROIDAL_SURFACE ( 'NONE', #63896, 5.400000000000001243, 0.4000000000000000222 ) ;
#1882 = DIRECTION ( 'NONE',  ( 1.734723475976806108E-16, -1.000000000000000000, 0.000000000000000000 ) ) ;
#1883 = EDGE_CURVE ( 'NONE', #14833, #62772, #28132, .T. ) ;
#1884 = EDGE_CURVE ( 'NONE', #38179, #40774, #29720, .T. ) ;
#1885 = CARTESIAN_POINT ( 'NONE',  ( 43.63372982999123195, -33.99649851277516888, -37.05616739551991401 ) ) ;
#1886 =( LENGTH_UNIT ( ) NAMED_UNIT ( * ) SI_UNIT ( .MILLI., .METRE. ) );
#1887 = CARTESIAN_POINT ( 'NONE',  ( -43.40846727561957152, 434.3587631104416005, 15.36753962288952380 ) ) ;
#1888 = CARTESIAN_POINT ( 'NONE',  ( -43.51410555626048904, -60.00000000000003553, 57.78858762630559909 ) ) ;
#1889 = DIRECTION ( 'NONE',  ( -1.619075244245005545E-14, -0.9887960631535431810, 0.1492727218618803420 ) ) ;
#1890 = CARTESIAN_POINT ( 'NONE',  ( -5.957442974701830707, 48.00000000000000000, 65.00000000000000000 ) ) ;
#1891 = CARTESIAN_POINT ( 'NONE',  ( -86.37715061851159248, -28.18947634940464297, 184.3000902350322008 ) ) ;
#1892 = EDGE_LOOP ( 'NONE', ( #55785, #65651, #67466, #82236, #54519 ) ) ;
#1893 = CARTESIAN_POINT ( 'NONE',  ( 0.000000000000000000, -5.629165124598847214, 3.250000000000005329 ) ) ;
#1894 = CARTESIAN_POINT ( 'NONE',  ( -1.003950229922949244, -39.47608679182096125, 30.46899775823919754 ) ) ;
#1895 = CARTESIAN_POINT ( 'NONE',  ( -6.232496158895186156, 41.83455024993975968, -59.02481301687200244 ) ) ;
#1896 = CARTESIAN_POINT ( 'NONE',  ( -41.59976559118467065, 472.6865677842792479, 16.01929606595135880 ) ) ;
#1898 = CARTESIAN_POINT ( 'NONE',  ( 3.387540951686171198, -69.89757699288746551, 13.41458569023665959 ) ) ;
#1897 = CARTESIAN_POINT ( 'NONE',  ( -42.22982424653864797, 347.2022962952978560, 14.15837535828084448 ) ) ;
#1899 = ORIENTED_EDGE ( 'NONE', *, *, #66860, .T. ) ;
#1900 = EDGE_CURVE ( 'NONE', #76623, #55395, #20051, .T. ) ;
#1901 = VECTOR ( 'NONE', #97341, 1000.000000000000000 ) ;
#1902 = CARTESIAN_POINT ( 'NONE',  ( -1.489880555935389612E-15, 34.19642918197134662, -12.16579798332631412 ) ) ;
#1903 = CARTESIAN_POINT ( 'NONE',  ( 4.684273348644264514E-15, 28.20649408426940141, 38.25000000000000000 ) ) ;
#1904 = CARTESIAN_POINT ( 'NONE',  ( 17.61650669486618881, 4.000000000000003553, 4.898587196589414801E-16 ) ) ;
#1905 = CARTESIAN_POINT ( 'NONE',  ( 24.96106100295528663, 303.9424320914693567, -9.763924114932871490 ) ) ;
#1906 = CARTESIAN_POINT ( 'NONE',  ( 21.51569398614858031, 294.9107018935607130, -9.987480606144492512 ) ) ;
#1907 = ADVANCED_FACE ( 'NONE', ( #15610 ), #71948, .T. ) ;
#1908 = DIRECTION ( 'NONE',  ( 1.000000000000000000, 1.224606353822377258E-16, 0.000000000000000000 ) ) ;
#1909 = DIRECTION ( 'NONE',  ( 0.000000000000000000, 1.000000000000000000, 0.000000000000000000 ) ) ;
#1910 = CARTESIAN_POINT ( 'NONE',  ( 114.0746655879125200, -59.99999999999997158, 159.9914145889356121 ) ) ;
#1911 = CARTESIAN_POINT ( 'NONE',  ( -81.44491109756651781, -39.50132863999797195, 155.9728766274752161 ) ) ;
#1912 = ORIENTED_EDGE ( 'NONE', *, *, #68254, .F. ) ;
#1913 = CYLINDRICAL_SURFACE ( 'NONE', #24062, 8.000000000000000000 ) ;
#1914 = CARTESIAN_POINT ( 'NONE',  ( 4.678819457397416670, 143.9212778189090614, -5.000000000000000000 ) ) ;
#1915 =( NAMED_UNIT ( * ) SI_UNIT ( $, .STERADIAN. ) SOLID_ANGLE_UNIT ( ) );
#1916 = CARTESIAN_POINT ( 'NONE',  ( -6.901579824520443829, 4.675625068323812528, -0.7022220667781287062 ) ) ;
#1917 = ADVANCED_FACE ( 'NONE', ( #46915 ), #31338, .T. ) ;
#1918 = CARTESIAN_POINT ( 'NONE',  ( 3.443309072005564797, 27.85918987796394575, -5.000000000000000000 ) ) ;
#1919 = CARTESIAN_POINT ( 'NONE',  ( 44.47534377888507606, -38.31160956920668070, 57.00192013341546016 ) ) ;
#1920 = ORIENTED_EDGE ( 'NONE', *, *, #50012, .T. ) ;
#1921 = UNCERTAINTY_MEASURE_WITH_UNIT (LENGTH_MEASURE( 1.000000000000000082E-05 ), #29795, 'distance_accuracy_value', 'NONE');
#1922 = AXIS2_PLACEMENT_3D ( 'NONE', #72176, #95393, #5838 ) ;
#1923 = FACE_OUTER_BOUND ( 'NONE', #40395, .T. ) ;
#1924 = ORIENTED_EDGE ( 'NONE', *, *, #70173, .F. ) ;
#1925 = AXIS2_PLACEMENT_3D ( 'NONE', #36403, #11524, #44452 ) ;
#1926 = CARTESIAN_POINT ( 'NONE',  ( 0.000000000000000000, 15.00000000000000000, 9.999999999999998224 ) ) ;
#1927 = DIRECTION ( 'NONE',  ( -0.5735764363510459374, -0.8191520442889919096, 0.000000000000000000 ) ) ;
#1928 = CARTESIAN_POINT ( 'NONE',  ( 28.89099332389485042, 49.99999999997997691, 58.53034795348389707 ) ) ;
#1929 = CARTESIAN_POINT ( 'NONE',  ( 5.990115786909115947, -12.91256367767907420, 13.08452859117424616 ) ) ;
#1930 = VECTOR ( 'NONE', #65836, 1000.000000000000000 ) ;
#1931 = SURFACE_SIDE_STYLE ('',( #69881 ) ) ;
#1932 = ORIENTED_EDGE ( 'NONE', *, *, #62858, .F. ) ;
#1933 = CARTESIAN_POINT ( 'NONE',  ( 104.6021310401891782, -60.00000000000001421, 107.7617790675090390 ) ) ;
#1934 = VECTOR ( 'NONE', #1927, 1000.000000000000000 ) ;
#1936 = CARTESIAN_POINT ( 'NONE',  ( 23.35041436762913136, -29.03775181700250840, 29.66908870611247906 ) ) ;
#1935 = CARTESIAN_POINT ( 'NONE',  ( -74.38379737572475392, -29.99999999999997513, 152.0617010018234794 ) ) ;
#1937 = CARTESIAN_POINT ( 'NONE',  ( 81.98192093697382177, -38.00000000001091394, -13.86368299876859567 ) ) ;
#1938 = CARTESIAN_POINT ( 'NONE',  ( 37.64086247411519537, 431.4033951771388615, 5.263547432144151550 ) ) ;
#1939 = CARTESIAN_POINT ( 'NONE',  ( -42.58793732781356312, -53.34669846594655240, 44.38150804302040342 ) ) ;
#1940 = VECTOR ( 'NONE', #12867, 1000.000000000000000 ) ;
#1941 = CARTESIAN_POINT ( 'NONE',  ( -31.82717529008558799, 18.64284798593262593, -21.53956455646148527 ) ) ;
#1942 = UNCERTAINTY_MEASURE_WITH_UNIT (LENGTH_MEASURE( 1.000000000000000082E-05 ), #98006, 'distance_accuracy_value', 'NONE');
#1943 = ORIENTED_EDGE ( 'NONE', *, *, #85149, .T. ) ;
#1944 = CYLINDRICAL_SURFACE ( 'NONE', #70223, 4.000000000000000000 ) ;
#1945 = CARTESIAN_POINT ( 'NONE',  ( -7.000000000000000000, -46.00000000000000000, 39.12435565298213902 ) ) ;
#1946 = CARTESIAN_POINT ( 'NONE',  ( 5.958501008717178138, -13.50719282745116701, 13.62690037880517302 ) ) ;
#1947 = DIRECTION ( 'NONE',  ( 0.000000000000000000, 0.000000000000000000, -1.000000000000000000 ) ) ;
#1948 = CARTESIAN_POINT ( 'NONE',  ( -30.00000000000000000, 488.0703656971138571, 7.691389546088009510 ) ) ;
#1949 = ORIENTED_EDGE ( 'NONE', *, *, #16553, .T. ) ;
#1950 = SURFACE_SIDE_STYLE ('',( #92568 ) ) ;
#1951 = EDGE_LOOP ( 'NONE', ( #7356, #25088, #51858, #40070, #60430, #55409 ) ) ;
#1952 = CARTESIAN_POINT ( 'NONE',  ( 77.69923846652405075, -29.99999999995701572, 180.6369940188211842 ) ) ;
#1953 = DIRECTION ( 'NONE',  ( -1.000000000000000000, -1.224606353822377258E-16, -0.000000000000000000 ) ) ;
#1954 = UNCERTAINTY_MEASURE_WITH_UNIT (LENGTH_MEASURE( 1.000000000000000082E-05 ), #85242, 'distance_accuracy_value', 'NONE');
#1955 = DIRECTION ( 'NONE',  ( 0.000000000000000000, -1.000000000000000000, 0.000000000000000000 ) ) ;
#1956 = CARTESIAN_POINT ( 'NONE',  ( 7.922281120364393914, -4.573931137438281169, -8.047472243342934206 ) ) ;
#1957 = CARTESIAN_POINT ( 'NONE',  ( 86.72630328678319245, -30.00000000000000711, 68.79586718995930994 ) ) ;
#1958 = CARTESIAN_POINT ( 'NONE',  ( -31.36074749248147953, 339.5349300696510682, 18.44790366892796030 ) ) ;
#1959 = ORIENTED_EDGE ( 'NONE', *, *, #31611, .T. ) ;
#1960 = EDGE_CURVE ( 'NONE', #76808, #81667, #46174, .T. ) ;
#1961 = PRESENTATION_LAYER_ASSIGNMENT (  '', '', ( #96680 ) ) ;
#1962 = ORIENTED_EDGE ( 'NONE', *, *, #105947, .T. ) ;
#1963 = ORIENTED_EDGE ( 'NONE', *, *, #53294, .T. ) ;
#1964 = CARTESIAN_POINT ( 'NONE',  ( -32.66787492830678730, 465.0722615638545108, 12.52936269481466525 ) ) ;
#1965 =( NAMED_UNIT ( * ) SI_UNIT ( $, .STERADIAN. ) SOLID_ANGLE_UNIT ( ) );
#1966 = DIRECTION ( 'NONE',  ( 1.000000000000000000, 0.000000000000000000, 0.000000000000000000 ) ) ;
#1967 = CARTESIAN_POINT ( 'NONE',  ( 4.589925132946516939, -11.06526016292516523, 3.864926970398261830 ) ) ;
#1968 = CARTESIAN_POINT ( 'NONE',  ( -31.69622719680273448, 348.2611537118722254, 20.17808803883451318 ) ) ;
#1969 = EDGE_CURVE ( 'NONE', #85296, #41445, #16906, .T. ) ;
#1970 =( LENGTH_UNIT ( ) NAMED_UNIT ( * ) SI_UNIT ( .MILLI., .METRE. ) );
#1971 = EDGE_LOOP ( 'NONE', ( #12366, #18193, #59824, #30066, #41908 ) ) ;
#1973 = EDGE_CURVE ( 'NONE', #102083, #106204, #75445, .T. ) ;
#1972 = CARTESIAN_POINT ( 'NONE',  ( -10.48543666094731464, 50.00000000000000000, -91.04342776276725147 ) ) ;
#1974 = VECTOR ( 'NONE', #25652, 1000.000000000000000 ) ;
#1975 = ORIENTED_EDGE ( 'NONE', *, *, #64833, .F. ) ;
#1976 = DIRECTION ( 'NONE',  ( -1.000000000000000000, -1.224606353822377258E-16, -0.000000000000000000 ) ) ;
#1977 = CARTESIAN_POINT ( 'NONE',  ( 76.23961518655661962, -38.39423639178605185, 180.1051403894379632 ) ) ;
#1978 = DIRECTION ( 'NONE',  ( -1.000000000000000000, -1.224606353822377258E-16, -0.000000000000000000 ) ) ;
#1979 = CARTESIAN_POINT ( 'NONE',  ( 25.69789908786751909, 305.2354844591588972, 10.47141389340269058 ) ) ;
#1980 = EDGE_CURVE ( 'NONE', #45703, #33011, #92308, .T. ) ;
#1981 = CARTESIAN_POINT ( 'NONE',  ( 0.000000000000000000, -6.938893903907228378E-15, 0.000000000000000000 ) ) ;
#1982 = ORIENTED_EDGE ( 'NONE', *, *, #24892, .F. ) ;
#1983 = EDGE_CURVE ( 'NONE', #10582, #79906, #56452, .T. ) ;
#1984 = CARTESIAN_POINT ( 'NONE',  ( 29.83349330513380337, 1.593028355512270567E-15, 0.000000000000000000 ) ) ;
#1985 = DIRECTION ( 'NONE',  ( 0.000000000000000000, 0.000000000000000000, -1.000000000000000000 ) ) ;
#1986 =( BOUNDED_SURFACE ( )  B_SPLINE_SURFACE ( 3, 2, ( 
 ( #49944, #100090, #26260 ),
 ( #83378, #58589, #57491 ),
 ( #9473, #34342, #99554 ),
 ( #59122, #51542, #10023 ),
 ( #17067, #91490, #32738 ),
 ( #41325, #65605, #824 ),
 ( #66671, #33793, #66133 ),
 ( #99011, #84457, #50995 ),
 ( #25176, #41856, #10548 ),
 ( #82850, #43467, #17604 ),
 ( #16519, #98490, #92005 ),
 ( #90416, #42930, #94692 ),
 ( #28376, #61799, #78477 ),
 ( #4603, #53155, #20841 ),
 ( #13198, #102761, #53671 ),
 ( #95212, #35946, #20308 ),
 ( #86605, #43992, #37000 ),
 ( #86072, #70401, #103299 ),
 ( #36479, #76880, #2996 ),
 ( #12144, #37536, #45073 ),
 ( #44536, #68816, #2455 ),
 ( #60727, #29446, #52071 ),
 ( #45602, #62318, #77955 ),
 ( #101167, #19241, #21343 ),
 ( #28926, #27327, #69868 ),
 ( #4070, #61252, #12670 ),
 ( #84986, #54184, #85526 ),
 ( #101699, #87122, #11069 ),
 ( #94137, #46126, #35403 ),
 ( #93615, #27859, #68271 ),
 ( #19770, #60206, #93074 ),
 ( #52599, #11607, #77424 ),
 ( #3540, #102226, #69348 ),
 ( #71981, #6169, #14258 ),
 ( #96797, #64435, #6708 ),
 ( #15332, #48219, #97307 ),
 ( #105411, #104890, #56297 ),
 ( #81122, #79537, #71437 ),
 ( #89237, #7231, #47161 ),
 ( #5131, #96281, #88701 ),
 ( #22406, #62846, #80061 ),
 ( #54715, #39101, #38573 ),
 ( #104336, #87650, #31552 ),
 ( #31030, #39635, #23461 ),
 ( #47689, #55250, #79013 ),
 ( #70921, #38065, #55765 ),
 ( #22929, #103815, #29958 ),
 ( #95733, #13732, #21874 ),
 ( #88174, #5650, #72506 ),
 ( #63911, #46640, #14794 ),
 ( #30485, #80588, #63386 ),
 ( #1226, #17055, #82302 ),
 ( #89872, #83365, #58019 ),
 ( #90945, #99542, #90405 ),
 ( #48332, #49933, #73127 ),
 ( #66121, #32725, #98999 ),
 ( #15979, #50455, #97958 ),
 ( #26247, #25165, #82839 ),
 ( #9464, #814, #56952 ),
 ( #33783, #24108, #48857 ),
 ( #24633, #81225, #81749 ),
 ( #16507, #91992, #7872 ),
 ( #8941, #7344, #8412 ),
 ( #106032, #42375, #74731 ),
 ( #57479, #40252, #40779 ),
 ( #41314, #32178, #41843 ),
 ( #33249, #98480, #65061 ),
 ( #66659, #73671, #25719 ),
 ( #58579, #280, #91478 ),
 ( #106574, #17593, #49393 ),
 ( #65594, #75266, #74202 ),
 ( #1364, #34328, #67205 ),
 ( #100080, #59112, #100612 ),
 ( #2979, #94124, #1905 ),
 ( #35392, #85515, #11594 ),
 ( #35934, #11058, #42918 ),
 ( #101687, #68807, #84974 ),
 ( #19754, #86059, #69335 ),
 ( #36987, #69855, #12133 ),
 ( #44523, #43454, #83898 ),
 ( #93602, #27846, #19229 ),
 ( #76868, #26773, #61240 ),
 ( #75810, #59644, #101152 ),
 ( #60717, #76332, #77945 ),
 ( #68260, #34859, #28912 ),
 ( #52059, #52589, #60196 ) ),
 .UNSPECIFIED., .F., .F., .F. ) 
 B_SPLINE_SURFACE_WITH_KNOTS ( ( 4, 2, 2, 2, 2, 2, 2, 2, 2, 2, 2, 2, 2, 2, 2, 2, 2, 2, 2, 2, 2, 2, 2, 2, 2, 2, 2, 2, 2, 2, 2, 2, 2, 2, 2, 2, 2, 2, 2, 2, 2, 2, 4 ),
 ( 3, 3 ),
 ( 0.06920511848905148977, 0.08726663333270481826, 0.1053281481763581329, 0.1233896630200114614, 0.1324204204418381325, 0.1369357991527514473, 0.1414511778636647898, 0.1595126927073181045, 0.1685434501291447618, 0.1730588288400580765, 0.1753165181955147478, 0.1775742075509714191, 0.1866049649727980764, 0.1888626543282547199, 0.1911203436837113911, 0.1956357223946247337, 0.1962001447334889015, 0.1964823559029209854, 0.1967645670723530693, 0.1978934117500814049, 0.2001511011055380762, 0.2024087904609947475, 0.2025498960457107755, 0.2026910016304268314, 0.2029732127998589153, 0.2035376351387230831, 0.2046664798164514187, 0.2052309021553155866, 0.2053720077400316146, 0.2054425605323896287, 0.2055131133247476705, 0.2057953244941797544, 0.2069241691719080900, 0.2074885915107722578, 0.2077708026802043417, 0.2080530138496364256, 0.2091818585273647613, 0.2103107032050930969, 0.2105929143745251808, 0.2107340199592412366, 0.2108751255439572647, 0.2114395478828214325, 0.2136972372382780760 ),
 ( 0.000000000000000000, 1.000000000000000000 ),
 .UNSPECIFIED. ) 
 GEOMETRIC_REPRESENTATION_ITEM ( )  RATIONAL_B_SPLINE_SURFACE ( (
 ( 1.000000000000000000, 0.7071068666372158917, 1.000000000000000000),
 ( 1.000000000000000000, 0.7071069334655512018, 1.000000000000000000),
 ( 1.000000000000000000, 0.7071067806429638392, 1.000000000000000000),
 ( 1.000000000000000000, 0.7071067806429638392, 1.000000000000000000),
 ( 1.000000000000000000, 0.7071067801986182788, 1.000000000000000000),
 ( 1.000000000000000000, 0.7071067801986182788, 1.000000000000000000),
 ( 1.000000000000000000, 0.7071052001454407598, 1.000000000000000000),
 ( 1.000000000000000000, 0.7071044926390116503, 1.000000000000000000),
 ( 1.000000000000000000, 0.7071050701755247081, 1.000000000000000000),
 ( 1.000000000000000000, 0.7071061918383323430, 1.000000000000000000),
 ( 1.000000000000000000, 0.7071065781433840680, 1.000000000000000000),
 ( 1.000000000000000000, 0.7071068693410902384, 1.000000000000000000),
 ( 1.000000000000000000, 0.7071066685034318455, 1.000000000000000000),
 ( 1.000000000000000000, 0.7071047597315383015, 1.000000000000000000),
 ( 1.000000000000000000, 0.7071038952480431794, 1.000000000000000000),
 ( 1.000000000000000000, 0.7071067879969044068, 1.000000000000000000),
 ( 1.000000000000000000, 0.7071060229798925567, 1.000000000000000000),
 ( 1.000000000000000000, 0.7071045510378535237, 1.000000000000000000),
 ( 1.000000000000000000, 0.7071047759561507329, 1.000000000000000000),
 ( 1.000000000000000000, 0.7071057096469625103, 1.000000000000000000),
 ( 1.000000000000000000, 0.7071060902437995566, 1.000000000000000000),
 ( 1.000000000000000000, 0.7071066634560565500, 1.000000000000000000),
 ( 1.000000000000000000, 0.7071075604197455400, 1.000000000000000000),
 ( 1.000000000000000000, 0.7071021497887993723, 1.000000000000000000),
 ( 1.000000000000000000, 0.7070768753575527032, 1.000000000000000000),
 ( 1.000000000000000000, 0.7070957430991587911, 1.000000000000000000),
 ( 1.000000000000000000, 0.7071005200448091665, 1.000000000000000000),
 ( 1.000000000000000000, 0.7071069032146458655, 1.000000000000000000),
 ( 1.000000000000000000, 0.7071070792554502438, 1.000000000000000000),
 ( 1.000000000000000000, 0.7071020376249698147, 1.000000000000000000),
 ( 1.000000000000000000, 0.7071032367434819665, 1.000000000000000000),
 ( 1.000000000000000000, 0.7071062266188036238, 1.000000000000000000),
 ( 1.000000000000000000, 0.7071064999784369975, 1.000000000000000000),
 ( 1.000000000000000000, 0.7071067279415800266, 1.000000000000000000),
 ( 1.000000000000000000, 0.7071067734869487253, 1.000000000000000000),
 ( 1.000000000000000000, 0.7071067871051068821, 1.000000000000000000),
 ( 1.000000000000000000, 0.7071062041018818523, 1.000000000000000000),
 ( 1.000000000000000000, 0.7070992872384374017, 1.000000000000000000),
 ( 1.000000000000000000, 0.7070832079407209925, 1.000000000000000000),
 ( 1.000000000000000000, 0.7070350815532235877, 1.000000000000000000),
 ( 1.000000000000000000, 0.7070089198012663445, 1.000000000000000000),
 ( 1.000000000000000000, 0.7070369844464885478, 1.000000000000000000),
 ( 1.000000000000000000, 0.7070957717068352411, 1.000000000000000000),
 ( 1.000000000000000000, 0.7071063006734819023, 1.000000000000000000),
 ( 1.000000000000000000, 0.7071066758728855595, 1.000000000000000000),
 ( 1.000000000000000000, 0.7071068482684416123, 1.000000000000000000),
 ( 1.000000000000000000, 0.7071067509067768819, 1.000000000000000000),
 ( 1.000000000000000000, 0.7071064712481558434, 1.000000000000000000),
 ( 1.000000000000000000, 0.7071060929135511985, 1.000000000000000000),
 ( 1.000000000000000000, 0.7071047181370017087, 1.000000000000000000),
 ( 1.000000000000000000, 0.7071035035220220033, 1.000000000000000000),
 ( 1.000000000000000000, 0.7071009480114961443, 1.000000000000000000),
 ( 1.000000000000000000, 0.7071013247174512406, 1.000000000000000000),
 ( 1.000000000000000000, 0.7071045817508229137, 1.000000000000000000),
 ( 1.000000000000000000, 0.7071059709058636900, 1.000000000000000000),
 ( 1.000000000000000000, 0.7071066865108602828, 1.000000000000000000),
 ( 1.000000000000000000, 0.7071067743865847577, 1.000000000000000000),
 ( 1.000000000000000000, 0.7071067840454771103, 1.000000000000000000),
 ( 1.000000000000000000, 0.7071068029700603441, 1.000000000000000000),
 ( 1.000000000000000000, 0.7071068959044196633, 1.000000000000000000),
 ( 1.000000000000000000, 0.7071069647084402554, 1.000000000000000000),
 ( 1.000000000000000000, 0.7071074002998787300, 1.000000000000000000),
 ( 1.000000000000000000, 0.7071080365385555844, 1.000000000000000000),
 ( 1.000000000000000000, 0.7071115864958791297, 1.000000000000000000),
 ( 1.000000000000000000, 0.7071144955833897905, 1.000000000000000000),
 ( 1.000000000000000000, 0.7071126567777766825, 1.000000000000000000),
 ( 1.000000000000000000, 0.7071112265437271560, 1.000000000000000000),
 ( 1.000000000000000000, 0.7071089973616805358, 1.000000000000000000),
 ( 1.000000000000000000, 0.7071082539167721226, 1.000000000000000000),
 ( 1.000000000000000000, 0.7071071327761628833, 1.000000000000000000),
 ( 1.000000000000000000, 0.7071068561964874988, 1.000000000000000000),
 ( 1.000000000000000000, 0.7071064601745752354, 1.000000000000000000),
 ( 1.000000000000000000, 0.7070930974566089766, 1.000000000000000000),
 ( 1.000000000000000000, 0.7070887504644172150, 1.000000000000000000),
 ( 1.000000000000000000, 0.7070959029254426653, 1.000000000000000000),
 ( 1.000000000000000000, 0.7071036569772559677, 1.000000000000000000),
 ( 1.000000000000000000, 0.7071050404321805871, 1.000000000000000000),
 ( 1.000000000000000000, 0.7071063254753164884, 1.000000000000000000),
 ( 1.000000000000000000, 0.7071066210311753863, 1.000000000000000000),
 ( 1.000000000000000000, 0.7071068435589438206, 1.000000000000000000),
 ( 1.000000000000000000, 0.7071067323499335977, 1.000000000000000000),
 ( 1.000000000000000000, 0.7071044733372250368, 1.000000000000000000),
 ( 1.000000000000000000, 0.7070984845377915606, 1.000000000000000000),
 ( 1.000000000000000000, 0.7070731566999163276, 1.000000000000000000),
 ( 1.000000000000000000, 0.7070931432108062964, 1.000000000000000000),
 ( 1.000000000000000000, 0.7071067811865465735, 1.000000000000000000) ) ) 
 REPRESENTATION_ITEM ( '' )  SURFACE ( )  );
#1987 = DIRECTION ( 'NONE',  ( 0.000000000000000000, 0.000000000000000000, -1.000000000000000000 ) ) ;
#1988 = CARTESIAN_POINT ( 'NONE',  ( 14.65167870846204323, 2.576877453026212628, 3.244758155286363799 ) ) ;
#1989 = ORIENTED_EDGE ( 'NONE', *, *, #13590, .F. ) ;
#1990 = CARTESIAN_POINT ( 'NONE',  ( 30.00000000000000000, 461.8423635046865456, 11.25802415799502221 ) ) ;
#1991 = CARTESIAN_POINT ( 'NONE',  ( 0.000000000000000000, 0.000000000000000000, -13.00000000000000000 ) ) ;
#1992 = DIRECTION ( 'NONE',  ( 0.000000000000000000, 0.000000000000000000, -1.000000000000000000 ) ) ;
#1993 = CARTESIAN_POINT ( 'NONE',  ( -5.174575781536625563, -5.672711317432108657, -7.030005583190792606 ) ) ;
#1994 = CARTESIAN_POINT ( 'NONE',  ( 6.379164974645483710, 294.7476919991335080, 1.915027880699541107 ) ) ;
#1995 = B_SPLINE_CURVE_WITH_KNOTS ( 'NONE', 3,
 ( #67727, #45062, #77411, #20292, #27314, #10010, #18674, #3528, #43981, #92520, #36467, #51528, #102215, #93063, #84445, #4057, #28362, #53141, #102750, #61786, #10537, #18128, #50984, #2444, #63897, #37523, #31018, #96786, #22917, #104326, #13185, #86594, #4588, #55754, #21333, #88162, #12658, #55238, #30473, #5639, #46629, #62830, #38563, #94681, #72494, #105399, #53661, #31543, #95721, #21860, #20828, #95200, #13720, #63370, #45588, #54702, #87635, #78467, #88686, #14246, #14781, #70387, #47676, #5120 ),
 .UNSPECIFIED., .F., .F.,
 ( 4, 1, 1, 1, 1, 2, 2, 1, 1, 1, 2, 2, 1, 1, 2, 2, 1, 1, 1, 2, 2, 1, 1, 1, 2, 2, 1, 1, 1, 1, 2, 2, 1, 1, 1, 1, 2, 2, 1, 1, 1, 1, 1, 2, 2, 4 ),
 ( 0.000000000000000000, 0.06250000000002220446, 0.09375000000003327894, 0.1093750000000388162, 0.1171875000000364569, 0.1210937500000405925, 0.1250000000000447142, 0.1875000000000952571, 0.2187500000001203759, 0.2343750000001331713, 0.2421875000001395550, 0.2500000000001459388, 0.3125000000001888489, 0.3437500000002124967, 0.3593750000002264300, 0.3750000000002403633, 0.4062500000002738365, 0.4218750000002892686, 0.4296875000002963740, 0.4335937500002993161, 0.4375000000003022582, 0.4687500000003195777, 0.4843750000003300138, 0.4921875000003336220, 0.4960937500003369527, 0.5000000000003402834, 0.5625000000003637091, 0.5937500000003747003, 0.6093750000003824718, 0.6171875000003853584, 0.6210937500003826939, 0.6250000000003799183, 0.6875000000003140821, 0.7187500000002793321, 0.7343750000002625677, 0.7421875000002535749, 0.7460937500002484679, 0.7500000000002434719, 0.8125000000001709743, 0.8437500000001322276, 0.8593750000001146860, 0.8671875000001059153, 0.8710937500001014744, 0.8730468750001000311, 0.8750000000000984768, 1.000000000000000000 ),
 .UNSPECIFIED. ) ;
#1996 = CARTESIAN_POINT ( 'NONE',  ( 46.00000000000000000, 463.8885932308145357, 10.44912889354677432 ) ) ;
#1997 = CARTESIAN_POINT ( 'NONE',  ( 86.39493283625975550, -17.42247157107316013, 179.1641491230458314 ) ) ;
#1998 = DIRECTION ( 'NONE',  ( 0.000000000000000000, 1.000000000000000000, 0.000000000000000000 ) ) ;
#1999 = CARTESIAN_POINT ( 'NONE',  ( -3.572097512798535046, 127.8538299566993004, 5.000000000000000888 ) ) ;
#2000 = ORIENTED_EDGE ( 'NONE', *, *, #46736, .T. ) ;
#2001 = DIRECTION ( 'NONE',  ( 0.000000000000000000, 1.000000000000000000, -0.000000000000000000 ) ) ;
#2002 = CIRCLE ( 'NONE', #65690, 7.000000000000000000 ) ;
#2003 = VECTOR ( 'NONE', #11800, 1000.000000000000000 ) ;
#2004 = DIRECTION ( 'NONE',  ( -1.000000000000000000, 0.000000000000000000, 0.000000000000000000 ) ) ;
#2005 = CARTESIAN_POINT ( 'NONE',  ( 15.50677046609170162, 34.82766853602287682, -23.25192831108139657 ) ) ;
#2006 = DIRECTION ( 'NONE',  ( 0.000000000000000000, 1.000000000000000000, -0.000000000000000000 ) ) ;
#2007 = AXIS2_PLACEMENT_3D ( 'NONE', #42460, #85062, #66747 ) ;
#2008 = CARTESIAN_POINT ( 'NONE',  ( -81.88499113863680634, -29.99999999999998934, 32.76904490412169935 ) ) ;
#2009 = DIRECTION ( 'NONE',  ( 1.000000000000000000, 0.000000000000000000, 0.000000000000000000 ) ) ;
#2010 = VECTOR ( 'NONE', #8185, 1000.000000000000000 ) ;
#2011 = CARTESIAN_POINT ( 'NONE',  ( 0.000000000000000000, 0.000000000000000000, 4.000000000000000000 ) ) ;
#2012 = FACE_OUTER_BOUND ( 'NONE', #85586, .T. ) ;
#2014 = CARTESIAN_POINT ( 'NONE',  ( 38.86638200451619696, 1.340359594676612611E-15, 0.000000000000000000 ) ) ;
#2013 = CARTESIAN_POINT ( 'NONE',  ( 28.86650669486618881, -3.999999999999998224, 0.000000000000000000 ) ) ;
#2015 = EDGE_CURVE ( 'NONE', #64595, #50361, #25487, .T. ) ;
#2016 = VECTOR ( 'NONE', #91954, 1000.000000000000000 ) ;
#2017 = CARTESIAN_POINT ( 'NONE',  ( 6.737208386734103271, -48.35039989235347946, 39.27323200384739010 ) ) ;
#2018 = DIRECTION ( 'NONE',  ( 0.000000000000000000, 0.000000000000000000, -1.000000000000000000 ) ) ;
#2019 = DIRECTION ( 'NONE',  ( 0.000000000000000000, 0.000000000000000000, -1.000000000000000000 ) ) ;
#2020 = FACE_OUTER_BOUND ( 'NONE', #77003, .T. ) ;
#2021 = FACE_OUTER_BOUND ( 'NONE', #98289, .T. ) ;
#2022 = LINE ( 'NONE', #59222, #39129 ) ;
#2023 = CARTESIAN_POINT ( 'NONE',  ( 47.90406143040812736, -27.00548834118202990, -28.50430916820407390 ) ) ;
#2024 = CARTESIAN_POINT ( 'NONE',  ( -25.00494464352431123, -42.95926918693982799, 32.33779692008577200 ) ) ;
#2025 = VERTEX_POINT ( 'NONE', #42013 ) ;
#2026 = DIRECTION ( 'NONE',  ( 0.000000000000000000, 1.000000000000000000, 0.000000000000000000 ) ) ;
#2027 = CARTESIAN_POINT ( 'NONE',  ( -9.699016383038308931, 108.1763817144834121, 2.444973590251038775 ) ) ;
#2028 = CARTESIAN_POINT ( 'NONE',  ( 7.500000000000000000, -4.330127018922200755, -7.422398894150036064 ) ) ;
#2029 = CARTESIAN_POINT ( 'NONE',  ( -47.33572465232198567, -26.86733324311558846, -28.64391245175660572 ) ) ;
#2031 = CYLINDRICAL_SURFACE ( 'NONE', #65535, 4.000000000000000888 ) ;
#2030 = FACE_OUTER_BOUND ( 'NONE', #68537, .T. ) ;
#2032 = ORIENTED_EDGE ( 'NONE', *, *, #10442, .T. ) ;
#2033 = CIRCLE ( 'NONE', #82965, 0.9999999999999849010 ) ;
#2034 = CARTESIAN_POINT ( 'NONE',  ( 15.11650669486618881, 4.000000000000003553, 4.898587196589414801E-16 ) ) ;
#2035 = EDGE_LOOP ( 'NONE', ( #19354, #16414, #90087, #17768, #101633 ) ) ;
#2036 = CARTESIAN_POINT ( 'NONE',  ( -7.751476769693538493, 50.00000000000000711, -95.64149282985064815 ) ) ;
#2037 = COLOUR_RGB ( '', 0.08235294, 0.09019608, 0.10196078) ;
#2038 = DIRECTION ( 'NONE',  ( 1.000000000000000000, 0.000000000000000000, 0.000000000000000000 ) ) ;
#2039 = DIRECTION ( 'NONE',  ( -0.5735764363510494901, -0.8191520442889894671, 0.000000000000000000 ) ) ;
#2040 = ORIENTED_EDGE ( 'NONE', *, *, #37938, .T. ) ;
#2041 = DIRECTION ( 'NONE',  ( 0.000000000000000000, -1.000000000000000000, 0.000000000000000000 ) ) ;
#2042 = CARTESIAN_POINT ( 'NONE',  ( -7.482235987343121231, 54.13190626386991511, -3.435864714555328270 ) ) ;
#2043 = CARTESIAN_POINT ( 'NONE',  ( 98.90275021636469432, -37.79594797260679684, 191.9678992726249191 ) ) ;
#2045 = CARTESIAN_POINT ( 'NONE',  ( -7.414580834929597408, -7.353437197185189511, 3.010264818013838273 ) ) ;
#2044 = DIRECTION ( 'NONE',  ( 0.000000000000000000, -1.000000000000000000, 0.000000000000000000 ) ) ;
#2047 = EDGE_CURVE ( 'NONE', #21783, #81794, #10699, .T. ) ;
#2046 = B_SPLINE_CURVE_WITH_KNOTS ( 'NONE', 3,
 ( #20307, #53154, #69867, #55764, #23460, #25048, #40140, #88699 ),
 .UNSPECIFIED., .F., .F.,
 ( 4, 2, 2, 4 ),
 ( 0.003797433802554431997, 0.004743183970586230952, 0.005688934138618029906, 0.007580434474681626948 ),
 .UNSPECIFIED. ) ;
#2048 = ORIENTED_EDGE ( 'NONE', *, *, #96195, .T. ) ;
#2049 = ORIENTED_EDGE ( 'NONE', *, *, #21354, .T. ) ;
#2050 = ORIENTED_EDGE ( 'NONE', *, *, #6380, .F. ) ;
#2051 = CARTESIAN_POINT ( 'NONE',  ( 26.75035470498962908, 311.3380438201987772, 11.49138685496244605 ) ) ;
#2052 = DIRECTION ( 'NONE',  ( 0.000000000000000000, -1.000000000000000000, 0.000000000000000000 ) ) ;
#2053 = CARTESIAN_POINT ( 'NONE',  ( 9.500000000000000000, -5.000000000000000000, -20.99851272547260095 ) ) ;
#2054 = ORIENTED_EDGE ( 'NONE', *, *, #72475, .F. ) ;
#2055 = CYLINDRICAL_SURFACE ( 'NONE', #51323, 4.250000000000000000 ) ;
#2056 = CARTESIAN_POINT ( 'NONE',  ( -32.75411547143850299, 465.7435926370450829, 11.50418982276456958 ) ) ;
#2057 = CARTESIAN_POINT ( 'NONE',  ( -72.68483858684419374, -57.66063987133676960, 178.6659478268091163 ) ) ;
#2058 = CARTESIAN_POINT ( 'NONE',  ( 6.944031699373467426, -65.53460654556130294, 3.972913591453824278 ) ) ;
#2059 = CARTESIAN_POINT ( 'NONE',  ( -29.45362385905110969, 325.9253963054578662, 15.14270878922920716 ) ) ;
#2060 = CARTESIAN_POINT ( 'NONE',  ( 38.82095363404105370, 477.1416748918212534, -1.685506013212387133 ) ) ;
#2061 = CARTESIAN_POINT ( 'NONE',  ( -91.01451176774321539, -60.00000000000003553, -21.65129702257078392 ) ) ;
#2062 = CARTESIAN_POINT ( 'NONE',  ( -43.53997681417765619, 465.2530638215212093, 9.299393732150377900 ) ) ;
#2063 = CARTESIAN_POINT ( 'NONE',  ( -48.95121697330014143, -60.29223702220649983, 55.82659700904435596 ) ) ;
#2064 = PLANE ( 'NONE',  #3939 ) ;
#2065 = ORIENTED_EDGE ( 'NONE', *, *, #46622, .F. ) ;
#2066 = CARTESIAN_POINT ( 'NONE',  ( 30.59999999999999787, -3.309499999999999886, 0.000000000000000000 ) ) ;
#2067 = DIRECTION ( 'NONE',  ( 0.000000000000000000, 0.000000000000000000, 1.000000000000000000 ) ) ;
#2068 = CARTESIAN_POINT ( 'NONE',  ( 9.336331243639834909, -2.525205179013640056, 14.78776590177819372 ) ) ;
#2069 = ORIENTED_EDGE ( 'NONE', *, *, #43770, .T. ) ;
#2070 = CARTESIAN_POINT ( 'NONE',  ( 5.092539576892236575, 247.5567653279156843, 3.177249149099067083 ) ) ;
#2071 = CARTESIAN_POINT ( 'NONE',  ( 75.04363187477058261, -38.33897610751563434, 169.9345625973519418 ) ) ;
#2072 = CARTESIAN_POINT ( 'NONE',  ( 49.27079747525518627, 12.96457032161368872, 15.75812555157588335 ) ) ;
#2073 = DIRECTION ( 'NONE',  ( 0.000000000000000000, -1.000000000000000000, 0.000000000000000000 ) ) ;
#2074 = AXIS2_PLACEMENT_3D ( 'NONE', #105346, #64371, #90221 ) ;
#2075 = CARTESIAN_POINT ( 'NONE',  ( -13.50000000000000000, -7.794228634059985339, -11.79422863405993382 ) ) ;
#2076 = CARTESIAN_POINT ( 'NONE',  ( 23.70422451878993186, 42.00000000000000000, 88.20421627933662023 ) ) ;
#2077 = CARTESIAN_POINT ( 'NONE',  ( 93.01758433144732408, -30.00000000000000355, 191.1199583869153287 ) ) ;
#2078 = CARTESIAN_POINT ( 'NONE',  ( 43.81028729233673147, 434.3199584132789255, 12.84475684849125265 ) ) ;
#2079 =( NAMED_UNIT ( * ) PLANE_ANGLE_UNIT ( ) SI_UNIT ( $, .RADIAN. ) );
#2080 = EDGE_CURVE ( 'NONE', #1766, #79700, #61601, .T. ) ;
#2081 = ORIENTED_EDGE ( 'NONE', *, *, #17235, .F. ) ;
#2082 = ORIENTED_EDGE ( 'NONE', *, *, #7579, .F. ) ;
#2083 = CARTESIAN_POINT ( 'NONE',  ( 51.62032401756362532, -29.11406301577443401, 49.91969295013280572 ) ) ;
#2084 = DIRECTION ( 'NONE',  ( -1.000000000000000000, -1.224606353822377258E-16, -0.000000000000000000 ) ) ;
#2085 = CARTESIAN_POINT ( 'NONE',  ( 67.22793774957824553, 6.975173280561618775E-15, 0.000000000000000000 ) ) ;
#2086 = ADVANCED_FACE ( 'NONE', ( #26415 ), #26941, .T. ) ;
#2087 = AXIS2_PLACEMENT_3D ( 'NONE', #68907, #19856, #37626 ) ;
#2088 = ORIENTED_EDGE ( 'NONE', *, *, #81317, .F. ) ;
#2089 = CARTESIAN_POINT ( 'NONE',  ( -87.97618656098680390, -38.37017363619033006, -19.60761191172759155 ) ) ;
#2090 = ORIENTED_EDGE ( 'NONE', *, *, #7883, .F. ) ;
#2091 = CARTESIAN_POINT ( 'NONE',  ( 110.2902390756780733, -38.35602141471932924, 184.0508174503084433 ) ) ;
#2092 = CARTESIAN_POINT ( 'NONE',  ( 13.55263786699659256, 24.70009625497336003, 1.189294995871621685 ) ) ;
#2093 = CARTESIAN_POINT ( 'NONE',  ( 85.58843428916756579, -52.71458237231213673, 27.65246598081628804 ) ) ;
#2094 = CARTESIAN_POINT ( 'NONE',  ( 32.81992448453895150, 465.7192846569213316, 11.17271167765130890 ) ) ;
#2095 = CARTESIAN_POINT ( 'NONE',  ( 0.000000000000000000, 44.50000000000000711, 0.000000000000000000 ) ) ;
#2096 = CARTESIAN_POINT ( 'NONE',  ( 32.04230769230768772, 1.411358822780289120E-15, 0.000000000000000000 ) ) ;
#2097 = CARTESIAN_POINT ( 'NONE',  ( 24.83349330513380337, 1.593028355512270567E-15, 0.000000000000000000 ) ) ;
#2098 = EDGE_CURVE ( 'NONE', #39498, #91936, #92694, .T. ) ;
#2099 = CARTESIAN_POINT ( 'NONE',  ( 19.00000000000001066, -4.000000000000000000, -1.500000000000000000 ) ) ;
#2100 = CARTESIAN_POINT ( 'NONE',  ( 8.830661707197901222, 133.7962572603164801, 8.673617379768678370E-16 ) ) ;
#2101 = ORIENTED_EDGE ( 'NONE', *, *, #75261, .T. ) ;
#2102 = EDGE_CURVE ( 'NONE', #102684, #1527, #89200, .T. ) ;
#2103 = PLANE ( 'NONE',  #91243 ) ;
#2104 = STYLED_ITEM ( 'NONE', ( #41395 ), #14634 ) ;
#2105 = DIRECTION ( 'NONE',  ( -0.5735764363510494901, -0.8191520442889894671, 0.000000000000000000 ) ) ;
#2106 = ORIENTED_EDGE ( 'NONE', *, *, #75155, .T. ) ;
#2107 = CARTESIAN_POINT ( 'NONE',  ( -34.64092164578498512, 485.1226699209325943, -1.978063925740380924 ) ) ;
#2108 = CARTESIAN_POINT ( 'NONE',  ( -42.67513304101517946, 370.1312389253066044, 17.76078588121451318 ) ) ;
#2109 = CARTESIAN_POINT ( 'NONE',  ( -32.13509466278925686, 486.0944799719932803, 5.282526334130711376 ) ) ;
#2110 = CARTESIAN_POINT ( 'NONE',  ( 5.656854249492378806, -24.68749999999999289, 5.656854249492381470 ) ) ;
#2111 = STYLED_ITEM ( 'NONE', ( #20193 ), #93726 ) ;
#2112 = CARTESIAN_POINT ( 'NONE',  ( 41.54461699769327510, -26.98090085330345644, 36.99557725161058386 ) ) ;
#2113 = DIRECTION ( 'NONE',  ( -0.9090909090909092827, 0.000000000000000000, -0.4165977904505306917 ) ) ;
#2114 = MECHANICAL_DESIGN_GEOMETRIC_PRESENTATION_REPRESENTATION (  '', ( #64141 ), #72723 ) ;
#2115 = VERTEX_POINT ( 'NONE', #82480 ) ;
#2116 = CARTESIAN_POINT ( 'NONE',  ( 81.99421977229519598, -57.10237923831468265, 184.9719132876309970 ) ) ;
#2117 = CARTESIAN_POINT ( 'NONE',  ( 0.000000000000000000, 0.000000000000000000, 0.000000000000000000 ) ) ;
#2118 = ORIENTED_EDGE ( 'NONE', *, *, #32107, .F. ) ;
#2119 = DIRECTION ( 'NONE',  ( 0.000000000000000000, 0.000000000000000000, -1.000000000000000000 ) ) ;
#2120 = CARTESIAN_POINT ( 'NONE',  ( 42.64669454893656564, 435.7301117832689101, 8.366116403187898953 ) ) ;
#2121 = DIRECTION ( 'NONE',  ( -1.000000000000000000, -1.224606353822377258E-16, -0.000000000000000000 ) ) ;
#2122 = CARTESIAN_POINT ( 'NONE',  ( 10.19007819943552562, -3.000000000000002665, -96.34610920172687543 ) ) ;
#2123 = CARTESIAN_POINT ( 'NONE',  ( 2.695484166361491685, -3.000000000000002665, -99.81725120020546171 ) ) ;
#2124 = CARTESIAN_POINT ( 'NONE',  ( -43.82550334199506636, -34.04363078587874014, -37.02915632368206644 ) ) ;
#2125 = FILL_AREA_STYLE ('',( #34020 ) ) ;
#2126 = CARTESIAN_POINT ( 'NONE',  ( 55.24550608235244908, -60.00000000000001421, 85.96734175474250605 ) ) ;
#2127 = CARTESIAN_POINT ( 'NONE',  ( 29.65525632516439103, -32.22057144229324166, 40.37876903116406169 ) ) ;
#2128 = CARTESIAN_POINT ( 'NONE',  ( 1.625879232102889042E-15, 47.29617335651134624, -13.27631144943088515 ) ) ;
#2129 = CARTESIAN_POINT ( 'NONE',  ( 25.50276709395012631, -19.53775645589208665, 31.59196450892726915 ) ) ;
#2131 = CARTESIAN_POINT ( 'NONE',  ( -13.30705700582391593, 22.17985797309225759, -4.023645276857861219 ) ) ;
#2130 = CARTESIAN_POINT ( 'NONE',  ( -29.91573279547425557, -32.39459060425171089, 40.52592436092722039 ) ) ;
#2132 = EDGE_CURVE ( 'NONE', #51980, #104099, #97802, .T. ) ;
#2133 = CARTESIAN_POINT ( 'NONE',  ( 4.898587196589412829E-16, -16.62499999999999289, -8.000000000000000000 ) ) ;
#2134 = CARTESIAN_POINT ( 'NONE',  ( 29.50756122520733271, 297.9063904818165724, 10.61050061783298126 ) ) ;
#2135 = FACE_OUTER_BOUND ( 'NONE', #14476, .T. ) ;
#2136 = CARTESIAN_POINT ( 'NONE',  ( -3.288228914120472801, 7.217643567644802971, -7.591235721156638583 ) ) ;
#2137 =( GEOMETRIC_REPRESENTATION_CONTEXT ( 3 ) GLOBAL_UNCERTAINTY_ASSIGNED_CONTEXT ( ( #77264 ) ) GLOBAL_UNIT_ASSIGNED_CONTEXT ( ( #2316, #93484, #26648 ) ) REPRESENTATION_CONTEXT ( 'NONE', 'WORKASPACE' ) );
#2138 = VERTEX_POINT ( 'NONE', #37157 ) ;
#2139 = CARTESIAN_POINT ( 'NONE',  ( 5.290067270632157204, 54.20842449845687838, -6.031152949374584793 ) ) ;
#2140 = CIRCLE ( 'NONE', #65830, 5.000000000000010658 ) ;
#2141 =( NAMED_UNIT ( * ) SI_UNIT ( $, .STERADIAN. ) SOLID_ANGLE_UNIT ( ) );
#2142 = UNCERTAINTY_MEASURE_WITH_UNIT (LENGTH_MEASURE( 1.000000000000000082E-05 ), #89430, 'distance_accuracy_value', 'NONE');
#2143 = FILL_AREA_STYLE_COLOUR ( '', #97854 ) ;
#2144 = COLOUR_RGB ( '', 0.66274510, 0.83137255, 0.94901961) ;
#2145 = DIRECTION ( 'NONE',  ( -0.5735764363510497121, 0.8191520442889892450, 1.003171929053521665E-16 ) ) ;
#2146 = EDGE_CURVE ( 'NONE', #13028, #60867, #101289, .T. ) ;
#2148 = CARTESIAN_POINT ( 'NONE',  ( 44.60714091412001636, -47.40887810288958093, -30.95114210435581725 ) ) ;
#2147 = FACE_OUTER_BOUND ( 'NONE', #44985, .T. ) ;
#2149 = VERTEX_POINT ( 'NONE', #19396 ) ;
#2150 = CARTESIAN_POINT ( 'NONE',  ( 28.08507790984678465, 36.49817779799894879, 8.014648791690131446 ) ) ;
#2151 = CARTESIAN_POINT ( 'NONE',  ( -44.47476153554900691, 485.8001565544831237, -0.4986688628725900463 ) ) ;
#2153 = VERTEX_POINT ( 'NONE', #37695 ) ;
#2152 = AXIS2_PLACEMENT_3D ( 'NONE', #14691, #6080, #81021 ) ;
#2154 = CARTESIAN_POINT ( 'NONE',  ( 20.11650669486618881, -3.851859888774471706E-31, 4.000000000000000888 ) ) ;
#2155 = CARTESIAN_POINT ( 'NONE',  ( 30.82729297445905914, 10.08692072324638822, -40.33672416147567219 ) ) ;
#2156 = DIRECTION ( 'NONE',  ( -1.000000000000000000, -0.000000000000000000, -0.000000000000000000 ) ) ;
#2157 = CARTESIAN_POINT ( 'NONE',  ( -92.03933232207216975, -60.00000000000000711, 19.29454771163106486 ) ) ;
#2158 = FILL_AREA_STYLE ('',( #59910 ) ) ;
#2159 = DIRECTION ( 'NONE',  ( -1.000000000000000000, -1.224606353822377258E-16, -0.000000000000000000 ) ) ;
#2160 = CARTESIAN_POINT ( 'NONE',  ( -5.000000000000000000, 0.000000000000000000, -4.289342857142857568 ) ) ;
#2162 =( NAMED_UNIT ( * ) PLANE_ANGLE_UNIT ( ) SI_UNIT ( $, .RADIAN. ) );
#2161 = CARTESIAN_POINT ( 'NONE',  ( -34.25876023350725319, 436.5729693652305059, 6.423321597049534759 ) ) ;
#2163 = ADVANCED_FACE ( 'NONE', ( #52768, #11764 ), #94845, .F. ) ;
#2164 = CARTESIAN_POINT ( 'NONE',  ( -81.65897383743494231, -53.48041058990561680, 179.0445688183182824 ) ) ;
#2165 = ORIENTED_EDGE ( 'NONE', *, *, #91155, .T. ) ;
#2166 = CARTESIAN_POINT ( 'NONE',  ( 0.000000000000000000, 0.000000000000000000, -7.974599999999995248 ) ) ;
#2167 = ORIENTED_EDGE ( 'NONE', *, *, #61657, .F. ) ;
#2168 = EDGE_LOOP ( 'NONE', ( #16801, #28743, #105035, #93656 ) ) ;
#2169 = DIRECTION ( 'NONE',  ( 0.000000000000000000, 0.000000000000000000, 1.000000000000000000 ) ) ;
#2170 = CARTESIAN_POINT ( 'NONE',  ( 0.000000000000000000, 6.123233995736767268E-16, -5.000000000000000888 ) ) ;
#2171 = AXIS2_PLACEMENT_3D ( 'NONE', #72189, #104547, #31231 ) ;
#2172 = EDGE_CURVE ( 'NONE', #12254, #89611, #106433, .T. ) ;
#2173 = CARTESIAN_POINT ( 'NONE',  ( 0.06682554136337941209, 6.264794173742279426, 2.149058192116896748 ) ) ;
#2174 = ORIENTED_EDGE ( 'NONE', *, *, #60499, .T. ) ;
#2175 = CARTESIAN_POINT ( 'NONE',  ( -19.70764564238368877, 304.7954121406193053, 9.925013215726751881 ) ) ;
#2176 = FILL_AREA_STYLE_COLOUR ( '', #68490 ) ;
#2177 = DIRECTION ( 'NONE',  ( -0.000000000000000000, -0.000000000000000000, -1.000000000000000000 ) ) ;
#2178 = CARTESIAN_POINT ( 'NONE',  ( -7.414580834929595632, -62.35343719718518685, 3.010264818013839161 ) ) ;
#2179 = AXIS2_PLACEMENT_3D ( 'NONE', #4659, #13785, #4125 ) ;
#2180 = CARTESIAN_POINT ( 'NONE',  ( -0.4142654402135939606, 53.41932298510439381, 10.18236585056131460 ) ) ;
#2181 = DIRECTION ( 'NONE',  ( 0.000000000000000000, 0.000000000000000000, 1.000000000000000000 ) ) ;
#2182 = DIRECTION ( 'NONE',  ( 0.000000000000000000, -1.000000000000000000, 0.000000000000000000 ) ) ;
#2183 = CARTESIAN_POINT ( 'NONE',  ( 96.66679845751455957, -59.99999999999993605, 43.68127598107410847 ) ) ;
#2184 = CARTESIAN_POINT ( 'NONE',  ( -109.5584880022855998, -59.99999999999993605, 197.6571416747650574 ) ) ;
#2185 = CARTESIAN_POINT ( 'NONE',  ( -60.91996879675399157, -32.54063067540256782, 71.34513968801962847 ) ) ;
#2186 = ORIENTED_EDGE ( 'NONE', *, *, #49857, .T. ) ;
#2187 = B_SPLINE_CURVE_WITH_KNOTS ( 'NONE', 3,
 ( #50053, #33915, #99672, #91598 ),
 .UNSPECIFIED., .F., .F.,
 ( 4, 4 ),
 ( 0.0005359291086695390635, 0.02814212626749257318 ),
 .UNSPECIFIED. ) ;
#2188 = ORIENTED_EDGE ( 'NONE', *, *, #63395, .F. ) ;
#2189 = CARTESIAN_POINT ( 'NONE',  ( -103.9196169064778985, -60.15914586142672960, 191.0476149618794750 ) ) ;
#2190 = CARTESIAN_POINT ( 'NONE',  ( 109.3513501059324255, -30.00000000000000000, 179.6549720493207190 ) ) ;
#2191 = AXIS2_PLACEMENT_3D ( 'NONE', #12585, #29355, #95652 ) ;
#2192 = FILL_AREA_STYLE ('',( #1663 ) ) ;
#2193 = CARTESIAN_POINT ( 'NONE',  ( 31.84999999999999787, 1.533819458162526451E-15, 0.000000000000000000 ) ) ;
#2194 = ORIENTED_EDGE ( 'NONE', *, *, #43555, .T. ) ;
#2195 = CARTESIAN_POINT ( 'NONE',  ( 7.500000000000001776, -4.999999999999998224, -68.91429205785460965 ) ) ;
#2196 = EDGE_CURVE ( 'NONE', #71103, #717, #66791, .T. ) ;
#2197 = CARTESIAN_POINT ( 'NONE',  ( -52.56211189760216485, -60.00000000000001421, 78.42721256930607865 ) ) ;
#2198 = CARTESIAN_POINT ( 'NONE',  ( -3.350247031700762879, -1.071204144247461576, 104.4269854689273558 ) ) ;
#2199 = CARTESIAN_POINT ( 'NONE',  ( -7.188101187500002709, -18.68750000204838102, 2.977408999572648707 ) ) ;
#2200 = CARTESIAN_POINT ( 'NONE',  ( 89.06666666666666288, -4.171999999999998820, 0.000000000000000000 ) ) ;
#2201 = SURFACE_STYLE_USAGE ( .BOTH. , #41619 ) ;
#2202 = CARTESIAN_POINT ( 'NONE',  ( 102.6464385083043283, 1.030564683017419500E-14, 0.000000000000000000 ) ) ;
#2203 = CARTESIAN_POINT ( 'NONE',  ( -11.44495203399156047, -4.945649015923802239, -12.56974089514457127 ) ) ;
#2204 = CARTESIAN_POINT ( 'NONE',  ( -6.499999999999999112, 3.752776749732556816, -6.064240316920397333 ) ) ;
#2205 = CARTESIAN_POINT ( 'NONE',  ( 9.051760805868392268, -13.60634430745754386, 16.31685301915852548 ) ) ;
#2206 = CARTESIAN_POINT ( 'NONE',  ( -15.43372845131082016, 46.13227632078329776, -5.762758105581760937 ) ) ;
#2207 = CARTESIAN_POINT ( 'NONE',  ( 14.33580413386840213, 42.00000000000000000, -89.41414995614803729 ) ) ;
#2208 = CARTESIAN_POINT ( 'NONE',  ( -29.78904055858565059, -39.48797846605977924, 33.06079419891941029 ) ) ;
#2209 = FILL_AREA_STYLE ('',( #35158 ) ) ;
#2210 = CARTESIAN_POINT ( 'NONE',  ( 45.52105560327908762, -39.52714366401688295, 44.31032762745270759 ) ) ;
#2211 = CARTESIAN_POINT ( 'NONE',  ( 14.85284876471456350, -5.000000000000000000, 6.123233995736768255E-16 ) ) ;
#2212 = CARTESIAN_POINT ( 'NONE',  ( -0.3371335334081437818, 45.31563508470815549, 18.71541435546660637 ) ) ;
#2213 = CARTESIAN_POINT ( 'NONE',  ( -86.93198415347136176, -38.59779612754854128, 199.5132169019792912 ) ) ;
#2214 = EDGE_LOOP ( 'NONE', ( #94723, #68154, #69718, #103687 ) ) ;
#2216 = CARTESIAN_POINT ( 'NONE',  ( -43.11534632275843393, 435.4435433140276928, 9.329549855370979472 ) ) ;
#2215 = CARTESIAN_POINT ( 'NONE',  ( 79.34455092495568351, -38.35611032209237692, -26.90405483085318039 ) ) ;
#2217 = CARTESIAN_POINT ( 'NONE',  ( 20.85090658074709324, -60.00000000000000711, 34.52371470500510497 ) ) ;
#2218 = CARTESIAN_POINT ( 'NONE',  ( -48.91516379432439976, 8.057663746602589327, -16.48802948946170233 ) ) ;
#2219 = CARTESIAN_POINT ( 'NONE',  ( -7.217786764392071674, 41.17942498929775752, -58.69594858756412492 ) ) ;
#2220 = CARTESIAN_POINT ( 'NONE',  ( 6.689297305232898339, 41.36669071814934284, -70.70516774953483718 ) ) ;
#2221 = DIRECTION ( 'NONE',  ( 0.000000000000000000, 0.000000000000000000, -1.000000000000000000 ) ) ;
#2223 = CARTESIAN_POINT ( 'NONE',  ( 43.43869229197125748, 464.9661605157749591, 13.42065392471466900 ) ) ;
#2222 = VECTOR ( 'NONE', #11886, 1000.000000000000000 ) ;
#2224 = CARTESIAN_POINT ( 'NONE',  ( 43.86650669486618881, -3.999999999999998224, 0.000000000000000000 ) ) ;
#2225 = CARTESIAN_POINT ( 'NONE',  ( 110.0463146278414683, -60.00000000000000000, 143.8199656869762464 ) ) ;
#2227 = CARTESIAN_POINT ( 'NONE',  ( 6.692588830498432451, -7.935834885954439422, -0.04058884017440578251 ) ) ;
#2226 = COLOUR_RGB ( '', 0.09019608, 0.27058824, 0.51372549) ;
#2228 = ADVANCED_FACE ( 'NONE', ( #29597 ), #82484, .T. ) ;
#2229 = CIRCLE ( 'NONE', #60849, 1.000000000000000000 ) ;
#2230 = CARTESIAN_POINT ( 'NONE',  ( 0.000000000000000000, 1.500000000000000000, 62.00000000000000000 ) ) ;
#2231 = ORIENTED_EDGE ( 'NONE', *, *, #30179, .F. ) ;
#2232 = EDGE_CURVE ( 'NONE', #73687, #37488, #32403, .T. ) ;
#2233 = CARTESIAN_POINT ( 'NONE',  ( -91.54332115524630353, -30.00000000000000000, 97.26594229145295856 ) ) ;
#2234 = VERTEX_POINT ( 'NONE', #89917 ) ;
#2235 = DIRECTION ( 'NONE',  ( -1.000000000000000000, -0.000000000000000000, -0.000000000000000000 ) ) ;
#2236 = DIRECTION ( 'NONE',  ( -0.000000000000000000, 1.000000000000000000, 0.000000000000000000 ) ) ;
#2237 = FILL_AREA_STYLE ('',( #74540 ) ) ;
#2238 = LINE ( 'NONE', #84243, #5874 ) ;
#2239 = CARTESIAN_POINT ( 'NONE',  ( 4.401442555609581635E-16, -22.15625000204838457, -7.188101187500000044 ) ) ;
#2241 = EDGE_CURVE ( 'NONE', #60237, #86927, #22079, .T. ) ;
#2240 = CARTESIAN_POINT ( 'NONE',  ( 11.68767211932491712, -5.000000000000002665, -88.14097461399492772 ) ) ;
#2242 = CARTESIAN_POINT ( 'NONE',  ( -1.469576158976823947E-15, -11.56250000409677092, 8.000000000000000000 ) ) ;
#2244 = EDGE_LOOP ( 'NONE', ( #77086, #3933, #61631, #24307 ) ) ;
#2243 = CARTESIAN_POINT ( 'NONE',  ( -38.82069281039413511, 477.2384714551109823, -1.705991107642487403 ) ) ;
#2245 = CARTESIAN_POINT ( 'NONE',  ( 80.88940320574509713, -49.91559681877727428, 166.5735459904898619 ) ) ;
#2246 = CARTESIAN_POINT ( 'NONE',  ( 0.000000000000000000, 0.000000000000000000, -5.000000000000000000 ) ) ;
#2247 = CARTESIAN_POINT ( 'NONE',  ( 9.482993638194542996, 87.44348720253677243, -3.177441187500463560 ) ) ;
#2248 = ORIENTED_EDGE ( 'NONE', *, *, #15481, .F. ) ;
#2249 = DIRECTION ( 'NONE',  ( 0.000000000000000000, 0.000000000000000000, 1.000000000000000000 ) ) ;
#2250 = CARTESIAN_POINT ( 'NONE',  ( -47.24423074384419152, 16.91655035847128019, 16.58644287016946706 ) ) ;
#2251 = CARTESIAN_POINT ( 'NONE',  ( 0.000000000000000000, 0.000000000000000000, -10.00000000000000000 ) ) ;
#2252 = CARTESIAN_POINT ( 'NONE',  ( 33.58349330513380693, 4.000000000000002665, 0.000000000000000000 ) ) ;
#2254 = CARTESIAN_POINT ( 'NONE',  ( 11.49350100829463805, 45.59260286365996961, 13.79671030421800104 ) ) ;
#2253 = AXIS2_PLACEMENT_3D ( 'NONE', #13145, #29904, #55199 ) ;
#2255 = LINE ( 'NONE', #28190, #26239 ) ;
#2256 = ORIENTED_EDGE ( 'NONE', *, *, #36061, .F. ) ;
#2257 =( GEOMETRIC_REPRESENTATION_CONTEXT ( 3 ) GLOBAL_UNCERTAINTY_ASSIGNED_CONTEXT ( ( #66150 ) ) GLOBAL_UNIT_ASSIGNED_CONTEXT ( ( #55188, #55705, #106391 ) ) REPRESENTATION_CONTEXT ( 'NONE', 'WORKASPACE' ) );
#2258 = SURFACE_SIDE_STYLE ('',( #34149 ) ) ;
#2259 = VECTOR ( 'NONE', #85723, 1000.000000000000000 ) ;
#2260 = CARTESIAN_POINT ( 'NONE',  ( -33.00000000000000000, 461.8802764867013479, 14.89328939273682195 ) ) ;
#2261 = CARTESIAN_POINT ( 'NONE',  ( -5.000000000000000000, -62.87784732671490673, 13.68732737529383670 ) ) ;
#2262 = CARTESIAN_POINT ( 'NONE',  ( 86.53852868639081919, -17.00621220630052477, 184.4929596998693739 ) ) ;
#2263 = FACE_OUTER_BOUND ( 'NONE', #39040, .T. ) ;
#2264 = EDGE_CURVE ( 'NONE', #37220, #48016, #101302, .T. ) ;
#2265 = CARTESIAN_POINT ( 'NONE',  ( 7.188101187500000044, -26.65625000204838813, 0.000000000000000000 ) ) ;
#2266 = CARTESIAN_POINT ( 'NONE',  ( 14.34999999999999787, 3.309500000000003439, 4.052968581778167743E-16 ) ) ;
#2267 = DIRECTION ( 'NONE',  ( 0.000000000000000000, 0.000000000000000000, -1.000000000000000000 ) ) ;
#2268 = EDGE_CURVE ( 'NONE', #37002, #57955, #84033, .T. ) ;
#2269 = CYLINDRICAL_SURFACE ( 'NONE', #68427, 1.250000000000000222 ) ;
#2270 = CONTEXT_DEPENDENT_SHAPE_REPRESENTATION ( #74185, #63064 ) ;
#2271 = ORIENTED_EDGE ( 'NONE', *, *, #75007, .F. ) ;
#2272 = CARTESIAN_POINT ( 'NONE',  ( -35.76964818834205317, 490.7750452587320069, 12.37427806642345196 ) ) ;
#2273 = CARTESIAN_POINT ( 'NONE',  ( -1.000000000000000888, -50.00000000000000000, 40.07669683062201926 ) ) ;
#2274 = CARTESIAN_POINT ( 'NONE',  ( -6.072471596195612165, 4.391857883210726676, -5.000000000000000000 ) ) ;
#2275 = EDGE_CURVE ( 'NONE', #22430, #60654, #61658, .T. ) ;
#2276 = CARTESIAN_POINT ( 'NONE',  ( 46.85000000000000142, 5.109226446042757607E-16, -4.171999999999999709 ) ) ;
#2277 = ORIENTED_EDGE ( 'NONE', *, *, #96460, .F. ) ;
#2278 = CARTESIAN_POINT ( 'NONE',  ( 3.313708498984800688, -17.28124999999999645, 7.999999999999960032 ) ) ;
#2279 = PLANE ( 'NONE',  #1313 ) ;
#2280 = VERTEX_POINT ( 'NONE', #49445 ) ;
#2281 = DIRECTION ( 'NONE',  ( 1.000000000000000000, 0.000000000000000000, 0.000000000000000000 ) ) ;
#2282 = CARTESIAN_POINT ( 'NONE',  ( -0.7725392102466939193, 13.06347760300539207, -49.51297689002939961 ) ) ;
#2283 = CARTESIAN_POINT ( 'NONE',  ( 32.80436725737454395, 485.2967250516980471, 5.900038805303855938 ) ) ;
#2284 = DIRECTION ( 'NONE',  ( 0.000000000000000000, 0.000000000000000000, 1.000000000000000000 ) ) ;
#2285 = CARTESIAN_POINT ( 'NONE',  ( -76.81430757441975743, -59.99999999999999289, 189.9012580596375699 ) ) ;
#2286 = DIRECTION ( 'NONE',  ( -1.000000000000000000, 0.000000000000000000, 0.000000000000000000 ) ) ;
#2287 = VECTOR ( 'NONE', #3635, 1000.000000000000000 ) ;
#2288 = DIRECTION ( 'NONE',  ( 0.000000000000000000, 0.000000000000000000, 1.000000000000000000 ) ) ;
#2289 = CARTESIAN_POINT ( 'NONE',  ( -43.00000000000000000, 487.9285348210879647, 8.903916466045071587 ) ) ;
#2290 = DIRECTION ( 'NONE',  ( -1.000000000000000000, 0.000000000000000000, 0.000000000000000000 ) ) ;
#2291 = CARTESIAN_POINT ( 'NONE',  ( -85.21415449681325072, -35.76165008134817214, 182.1678819788450880 ) ) ;
#2292 = CIRCLE ( 'NONE', #41891, 1.000000000000000888 ) ;
#2293 = SURFACE_STYLE_USAGE ( .BOTH. , #69195 ) ;
#2294 = CONICAL_SURFACE ( 'NONE', #16094, 5.000000000000001776, 0.9599310885968803664 ) ;
#2295 = ORIENTED_EDGE ( 'NONE', *, *, #82415, .F. ) ;
#2296 = CYLINDRICAL_SURFACE ( 'NONE', #71585, 3.400000000000000355 ) ;
#2297 = EDGE_CURVE ( 'NONE', #100438, #44273, #90998, .T. ) ;
#2298 = CARTESIAN_POINT ( 'NONE',  ( 3.365451957726484977, -0.9314134953375798887, 104.1992105446103096 ) ) ;
#2299 = CARTESIAN_POINT ( 'NONE',  ( -85.54679910649467445, -52.71797009601630890, -1.685581303667236908 ) ) ;
#2300 = CARTESIAN_POINT ( 'NONE',  ( -7.000000000000000000, -14.05766640829038749, -5.232782735144286157 ) ) ;
#2301 = CARTESIAN_POINT ( 'NONE',  ( -26.27902093981875709, 306.9027577142574614, -9.548073367145329726 ) ) ;
#2302 = EDGE_LOOP ( 'NONE', ( #47141, #12270, #97467, #103494, #52732, #80515, #77317, #15258 ) ) ;
#2303 = COLOUR_RGB ( '', 0.66274510, 0.83137255, 0.94901961) ;
#2304 = CARTESIAN_POINT ( 'NONE',  ( -14.73107898043755881, -7.226827713034739809, 13.14759240030440424 ) ) ;
#2305 = CARTESIAN_POINT ( 'NONE',  ( -6.920567593065749534, -12.35473601147217870, 8.513547508574108136 ) ) ;
#2306 = CARTESIAN_POINT ( 'NONE',  ( -88.20421627925426833, 42.00000000000000000, -23.70422451879017345 ) ) ;
#2307 = EDGE_CURVE ( 'NONE', #85900, #31075, #15125, .T. ) ;
#2308 = CARTESIAN_POINT ( 'NONE',  ( -1.446302031375384789E-15, 60.76237703744687479, 11.80995232570204045 ) ) ;
#2309 = CARTESIAN_POINT ( 'NONE',  ( 69.27313422356952799, -59.99999999999999289, 151.6321682696899984 ) ) ;
#2310 = SURFACE_STYLE_FILL_AREA ( #76206 ) ;
#2311 = CARTESIAN_POINT ( 'NONE',  ( -88.92180072262880230, -30.00000000000001421, -15.18793788064705197 ) ) ;
#2312 = EDGE_CURVE ( 'NONE', #5281, #3985, #17106, .T. ) ;
#2313 = CARTESIAN_POINT ( 'NONE',  ( -71.21937153047667834, -36.01495328744242386, 103.8040231744988802 ) ) ;
#2314 = ORIENTED_EDGE ( 'NONE', *, *, #20001, .T. ) ;
#2315 = CARTESIAN_POINT ( 'NONE',  ( 72.11378188144121282, -59.99999999999999289, 177.1381934468311670 ) ) ;
#2316 =( LENGTH_UNIT ( ) NAMED_UNIT ( * ) SI_UNIT ( .MILLI., .METRE. ) );
#2317 = ORIENTED_EDGE ( 'NONE', *, *, #6369, .T. ) ;
#2318 = CARTESIAN_POINT ( 'NONE',  ( 11.20998319195465776, -57.67118707559646396, -44.35019014734187692 ) ) ;
#2319 = EDGE_CURVE ( 'NONE', #8756, #59177, #42694, .T. ) ;
#2320 = ORIENTED_EDGE ( 'NONE', *, *, #103922, .F. ) ;
#2321 = CARTESIAN_POINT ( 'NONE',  ( 7.943457856580265819, 51.78228140934420765, -3.880460080061692629 ) ) ;
#2322 = CARTESIAN_POINT ( 'NONE',  ( -7.188101187500000933, -24.87500000204838813, -2.977408999572651371 ) ) ;
#2323 = CARTESIAN_POINT ( 'NONE',  ( 8.099999999999999645, 7.505553499465140277, -3.755786496842903002E-16 ) ) ;
#2324 = VERTEX_POINT ( 'NONE', #51036 ) ;
#2325 = DIRECTION ( 'NONE',  ( -0.000000000000000000, 1.000000000000000000, -0.000000000000000000 ) ) ;
#2326 = ORIENTED_EDGE ( 'NONE', *, *, #10621, .T. ) ;
#2327 = DIRECTION ( 'NONE',  ( -1.000000000000000000, -1.224606353822377258E-16, -0.000000000000000000 ) ) ;
#2328 = VECTOR ( 'NONE', #32417, 1000.000000000000000 ) ;
#2329 = CARTESIAN_POINT ( 'NONE',  ( 4.699999999999999289, 0.000000000000000000, 0.000000000000000000 ) ) ;
#2330 = CARTESIAN_POINT ( 'NONE',  ( -42.13804600684559887, -59.99999999998057376, 60.14875204916594953 ) ) ;
#2331 = CARTESIAN_POINT ( 'NONE',  ( 20.37278541768183615, 303.8378246129572631, -10.00297115033342266 ) ) ;
#2332 = CARTESIAN_POINT ( 'NONE',  ( -2.977408999572654480, -12.12500000204838990, 7.188101187499999156 ) ) ;
#2333 = CARTESIAN_POINT ( 'NONE',  ( 55.00571552735602410, 4.000000000000014211, 0.000000000000000000 ) ) ;
#2334 = AXIS2_PLACEMENT_3D ( 'NONE', #102678, #94054, #61717 ) ;
#2335 = FACE_OUTER_BOUND ( 'NONE', #100459, .T. ) ;
#2336 = DIRECTION ( 'NONE',  ( 0.000000000000000000, 0.000000000000000000, 1.000000000000000000 ) ) ;
#2337 = CARTESIAN_POINT ( 'NONE',  ( -3.140974613988893882, 50.00000000000000000, -96.68767211932436112 ) ) ;
#2338 = CARTESIAN_POINT ( 'NONE',  ( -3.313708498984726969, -14.46874999999999112, 8.000000000000039080 ) ) ;
#2339 = LINE ( 'NONE', #61687, #89177 ) ;
#2340 = UNCERTAINTY_MEASURE_WITH_UNIT (LENGTH_MEASURE( 1.000000000000000082E-05 ), #36595, 'distance_accuracy_value', 'NONE');
#2341 = STYLED_ITEM ( 'NONE', ( #80001 ), #51084 ) ;
#2342 = MECHANICAL_DESIGN_GEOMETRIC_PRESENTATION_REPRESENTATION (  '', ( #81542 ), #38557 ) ;
#2343 = VERTEX_POINT ( 'NONE', #8462 ) ;
#2344 = CARTESIAN_POINT ( 'NONE',  ( 5.374793246923871948, -2.224716758540632888, 104.0614974883207537 ) ) ;
#2345 = PRESENTATION_LAYER_ASSIGNMENT (  '', '', ( #52080 ) ) ;
#2347 = CARTESIAN_POINT ( 'NONE',  ( 33.64991883386763050, -60.30412654068202727, 38.51323943821249429 ) ) ;
#2346 = FILL_AREA_STYLE ('',( #16958 ) ) ;
#2348 = CARTESIAN_POINT ( 'NONE',  ( 20.16952962162617879, -4.285714285716217375, 15.50035291838605467 ) ) ;
#2349 = ORIENTED_EDGE ( 'NONE', *, *, #84634, .T. ) ;
#2350 = CARTESIAN_POINT ( 'NONE',  ( 36.23446467943824700, 484.5294442010003877, -2.438443429321658140 ) ) ;
#2351 = ORIENTED_EDGE ( 'NONE', *, *, #65543, .T. ) ;
#2353 = CARTESIAN_POINT ( 'NONE',  ( -0.08421528330799921136, 44.08548369317413318, -16.25000000000000355 ) ) ;
#2352 = CARTESIAN_POINT ( 'NONE',  ( -26.35543691165159430, 34.76319968196727217, -9.819974411512054857 ) ) ;
#2354 = CARTESIAN_POINT ( 'NONE',  ( 19.62651309133643451, 302.7443318707399840, -10.02279753415084329 ) ) ;
#2355 = CARTESIAN_POINT ( 'NONE',  ( -43.65809794933295507, 484.6141936383213533, 3.261896584726788451 ) ) ;
#2356 = DIRECTION ( 'NONE',  ( 0.000000000000000000, 1.000000000000000000, 0.000000000000000000 ) ) ;
#2357 = DIRECTION ( 'NONE',  ( -0.000000000000000000, -1.000000000000000000, -0.000000000000000000 ) ) ;
#2358 = CARTESIAN_POINT ( 'NONE',  ( -7.500000000000000888, -1.443375672974072543, -7.063244554130002406 ) ) ;
#2359 = ORIENTED_EDGE ( 'NONE', *, *, #9804, .T. ) ;
#2360 = CARTESIAN_POINT ( 'NONE',  ( 91.76855862128167018, -60.00000000000000000, -14.78760871838603741 ) ) ;
#2361 = SURFACE_SIDE_STYLE ('',( #43368 ) ) ;
#2362 = CARTESIAN_POINT ( 'NONE',  ( 40.04008949875137802, 489.2273486934136031, 11.31296313617416338 ) ) ;
#2363 = CARTESIAN_POINT ( 'NONE',  ( -46.79790428518977308, 18.85533329945891978, -15.37169442865915236 ) ) ;
#2364 = ORIENTED_EDGE ( 'NONE', *, *, #44524, .F. ) ;
#2365 = EDGE_CURVE ( 'NONE', #24844, #100880, #18174, .T. ) ;
#2366 = CONICAL_SURFACE ( 'NONE', #93703, 3.400000000000000355, 0.9599310885968748153 ) ;
#2367 = CARTESIAN_POINT ( 'NONE',  ( -80.67925139857744909, -29.99999999998416200, 191.9698402685723977 ) ) ;
#2368 = ORIENTED_EDGE ( 'NONE', *, *, #91354, .F. ) ;
#2369 = ORIENTED_EDGE ( 'NONE', *, *, #104134, .F. ) ;
#2370 = CARTESIAN_POINT ( 'NONE',  ( 7.986452802927059835, 81.02690242308116808, 0.5332468218996382348 ) ) ;
#2371 = CARTESIAN_POINT ( 'NONE',  ( 37.56673239365870387, 27.60449318992555945, 13.45617127780999134 ) ) ;
#2372 = CARTESIAN_POINT ( 'NONE',  ( 40.02592568779148507, 5.000000000000002665, 0.000000000000000000 ) ) ;
#2373 = DIRECTION ( 'NONE',  ( 0.000000000000000000, -1.000000000000000000, 0.000000000000000000 ) ) ;
#2374 = CARTESIAN_POINT ( 'NONE',  ( 83.39873523156931867, -45.27648495923967431, -13.67455449466119966 ) ) ;
#2375 = CARTESIAN_POINT ( 'NONE',  ( -42.44954169440552505, 319.4024488318097497, -4.056765102163490511 ) ) ;
#2376 = CARTESIAN_POINT ( 'NONE',  ( -16.94033034664163395, 304.5648766887006218, -9.060986148973602994 ) ) ;
#2378 = EDGE_CURVE ( 'NONE', #88738, #41320, #80775, .T. ) ;
#2377 = CARTESIAN_POINT ( 'NONE',  ( -17.49999999999997158, 45.00000000000000000, 63.96297035378971430 ) ) ;
#2379 = CARTESIAN_POINT ( 'NONE',  ( 20.59999999999999787, 3.309500000000003439, 4.052968581778167743E-16 ) ) ;
#2380 = ORIENTED_EDGE ( 'NONE', *, *, #101889, .T. ) ;
#2381 = CARTESIAN_POINT ( 'NONE',  ( -6.500000000000000000, -4.014037567183547317, -6.470355840301009742 ) ) ;
#2382 = EDGE_LOOP ( 'NONE', ( #85674, #102561, #70360 ) ) ;
#2383 = CARTESIAN_POINT ( 'NONE',  ( 48.60240570037284158, 10.21057620019136003, -14.48840219382827321 ) ) ;
#2384 = CARTESIAN_POINT ( 'NONE',  ( 6.936184427528457874, 0.000000000000000000, -8.605212085995399107 ) ) ;
#2385 = AXIS2_PLACEMENT_3D ( 'NONE', #20676, #104174, #78839 ) ;
#2387 = ORIENTED_EDGE ( 'NONE', *, *, #58333, .T. ) ;
#2386 = CARTESIAN_POINT ( 'NONE',  ( 5.371796735821363633, 52.06045347113851562, 6.031152949374357419 ) ) ;
#2388 = CARTESIAN_POINT ( 'NONE',  ( 76.97083215510561160, -29.07873089524411725, 121.1780571378874640 ) ) ;
#2389 = ORIENTED_EDGE ( 'NONE', *, *, #58737, .F. ) ;
#2390 = CARTESIAN_POINT ( 'NONE',  ( 4.136210027783189247, -48.58433892124558184, 40.56527332860810020 ) ) ;
#2391 = DIRECTION ( 'NONE',  ( 0.000000000000000000, 0.000000000000000000, 1.000000000000000000 ) ) ;
#2392 = AXIS2_PLACEMENT_3D ( 'NONE', #60995, #43727, #42125 ) ;
#2393 = CARTESIAN_POINT ( 'NONE',  ( 4.401442555609581635E-16, -27.78125000204838457, -7.188101187500000044 ) ) ;
#2394 = CARTESIAN_POINT ( 'NONE',  ( -93.89173215636174064, -57.65323629495627245, -14.51111636511549996 ) ) ;
#2395 = EDGE_CURVE ( 'NONE', #21935, #99732, #40999, .T. ) ;
#2396 = EDGE_LOOP ( 'NONE', ( #64019, #88196 ) ) ;
#2397 = FILL_AREA_STYLE_COLOUR ( '', #74565 ) ;
#2398 = B_SPLINE_CURVE_WITH_KNOTS ( 'NONE', 3,
 ( #27469, #59271, #100239, #68965 ),
 .UNSPECIFIED., .F., .F.,
 ( 4, 4 ),
 ( 0.000000000000000000, 1.000000000000000000 ),
 .UNSPECIFIED. ) ;
#2399 = CARTESIAN_POINT ( 'NONE',  ( 33.07276483573664905, 438.9325140356084489, 23.89537236861388081 ) ) ;
#2400 = CARTESIAN_POINT ( 'NONE',  ( 106.0465130611873974, -60.15137259862576968, 181.9139942087800534 ) ) ;
#2401 = DIRECTION ( 'NONE',  ( -1.000000000000000000, -1.224606353822377258E-16, -0.000000000000000000 ) ) ;
#2402 = CARTESIAN_POINT ( 'NONE',  ( 49.18736646279173641, 13.60337276043470389, -15.12866845614532352 ) ) ;
#2403 = EDGE_CURVE ( 'NONE', #26186, #57765, #8261, .T. ) ;
#2404 = CARTESIAN_POINT ( 'NONE',  ( 8.000000000000000000, -15.68750000409677092, 0.000000000000000000 ) ) ;
#2405 = DIRECTION ( 'NONE',  ( 0.000000000000000000, 1.000000000000000000, 0.000000000000000000 ) ) ;
#2406 = CARTESIAN_POINT ( 'NONE',  ( 9.482993638194562536, 247.5565127974631423, -3.177441187500463116 ) ) ;
#2407 = CARTESIAN_POINT ( 'NONE',  ( 12.50000000000000000, 1.530808498934191521E-15, 0.000000000000000000 ) ) ;
#2408 = CARTESIAN_POINT ( 'NONE',  ( 96.81745522565726958, -37.99999999999980815, 192.8977754549547967 ) ) ;
#2410 = VECTOR ( 'NONE', #80931, 999.9999999999998863 ) ;
#2409 = DIRECTION ( 'NONE',  ( 0.000000000000000000, 0.000000000000000000, 1.000000000000000000 ) ) ;
#2411 = CARTESIAN_POINT ( 'NONE',  ( 0.000000000000000000, 0.000000000000000000, 0.000000000000000000 ) ) ;
#2412 = ORIENTED_EDGE ( 'NONE', *, *, #29212, .F. ) ;
#2413 = CARTESIAN_POINT ( 'NONE',  ( 44.17836536378433010, 435.2619773020561524, 14.65562696768152939 ) ) ;
#2414 = CARTESIAN_POINT ( 'NONE',  ( 81.84444444444444855, 1.023464760207051730E-14, 0.000000000000000000 ) ) ;
#2415 = CARTESIAN_POINT ( 'NONE',  ( -7.500000000000000888, -3.000671055698259870, -20.99923901233272971 ) ) ;
#2416 = COLOUR_RGB ( '', 0.09019608, 0.27058824, 0.51372549) ;
#2417 = CARTESIAN_POINT ( 'NONE',  ( -85.27768309077019637, -30.00000000000000711, 172.8990738933071327 ) ) ;
#2418 = EDGE_CURVE ( 'NONE', #37530, #17654, #17641, .T. ) ;
#2419 = VECTOR ( 'NONE', #1159, 1000.000000000000000 ) ;
#2420 = ORIENTED_EDGE ( 'NONE', *, *, #5467, .F. ) ;
#2421 = CARTESIAN_POINT ( 'NONE',  ( 4.457519228156027857, -48.07754600148881252, 43.17321295657507818 ) ) ;
#2422 = CARTESIAN_POINT ( 'NONE',  ( 78.99859466470238090, -57.50609917691477335, 197.8297617738492704 ) ) ;
#2424 = CARTESIAN_POINT ( 'NONE',  ( 46.00000000000000000, 437.9690125970928989, 14.09127711025711527 ) ) ;
#2423 = CARTESIAN_POINT ( 'NONE',  ( -15.47565679866127653, 2.746345986930186278, -1.655435732240887026 ) ) ;
#2425 = ORIENTED_EDGE ( 'NONE', *, *, #15135, .F. ) ;
#2426 = CARTESIAN_POINT ( 'NONE',  ( 24.48579885659522404, -27.51483317846157206, -38.38701603259436013 ) ) ;
#2427 = CARTESIAN_POINT ( 'NONE',  ( -5.385673916453011856, 4.000000000000000000, 18.57417562100670949 ) ) ;
#2428 = CARTESIAN_POINT ( 'NONE',  ( -40.70962269998187821, -59.99999999999999289, 53.12857981522989803 ) ) ;
#2429 = CARTESIAN_POINT ( 'NONE',  ( -31.01497228917065740, 439.2907934540658630, 22.60551266133744264 ) ) ;
#2430 = SURFACE_STYLE_FILL_AREA ( #3512 ) ;
#2431 = CARTESIAN_POINT ( 'NONE',  ( -86.11174981640101578, -53.81160830264160211, 192.0627294854906211 ) ) ;
#2432 = ORIENTED_EDGE ( 'NONE', *, *, #64318, .F. ) ;
#2433 = CARTESIAN_POINT ( 'NONE',  ( 29.68315524077034340, 18.29184282782460969, 39.60535821593451544 ) ) ;
#2434 = CARTESIAN_POINT ( 'NONE',  ( -3.040491613002718196, -42.95758431452577497, 31.04430139814011724 ) ) ;
#2435 = CARTESIAN_POINT ( 'NONE',  ( -3.279721309033237109, -49.29419538185737792, 103.5044183211188198 ) ) ;
#2437 = CARTESIAN_POINT ( 'NONE',  ( -7.369762991775258065, 54.30878687387412640, 2.388529231885675674 ) ) ;
#2436 = CARTESIAN_POINT ( 'NONE',  ( -31.56403572835066740, 299.1279782509382130, 2.888934931175894061 ) ) ;
#2438 = EDGE_CURVE ( 'NONE', #23524, #39236, #72034, .T. ) ;
#2439 = VERTEX_POINT ( 'NONE', #1415 ) ;
#2441 = CARTESIAN_POINT ( 'NONE',  ( -1.722054852581828306E-15, 24.73290587908618932, -14.06164498842270483 ) ) ;
#2440 = AXIS2_PLACEMENT_3D ( 'NONE', #99860, #26032, #16283 ) ;
#2442 = DIRECTION ( 'NONE',  ( -1.000000000000000000, -1.224606353822377258E-16, -0.000000000000000000 ) ) ;
#2443 = DIRECTION ( 'NONE',  ( 0.000000000000000000, 0.000000000000000000, -1.000000000000000000 ) ) ;
#2444 = CARTESIAN_POINT ( 'NONE',  ( 17.86116378879217947, 50.00000000000001421, 62.08262986194836941 ) ) ;
#2445 = CARTESIAN_POINT ( 'NONE',  ( 34.06332199976886699, 330.0526646846329299, -3.810096259360388427 ) ) ;
#2446 = EDGE_CURVE ( 'NONE', #46570, #11369, #59159, .T. ) ;
#2447 = DIRECTION ( 'NONE',  ( 1.224646799147353207E-16, 1.000000000000000000, 0.000000000000000000 ) ) ;
#2448 = CARTESIAN_POINT ( 'NONE',  ( 9.096683260177623964, 53.76343451018224329, -1.649683610281133417 ) ) ;
#2449 = CARTESIAN_POINT ( 'NONE',  ( 95.99465422657044655, -14.21045842199428222, 88.91344185009528189 ) ) ;
#2450 = CARTESIAN_POINT ( 'NONE',  ( -78.67339649595623996, -56.84650683190278642, 157.0027717221539660 ) ) ;
#2451 = ORIENTED_EDGE ( 'NONE', *, *, #8287, .F. ) ;
#2452 = CARTESIAN_POINT ( 'NONE',  ( 80.00000000000000000, -60.00000000000000000, -21.09707704303352926 ) ) ;
#2453 = CARTESIAN_POINT ( 'NONE',  ( 5.650483388624512493, 253.4556659685037801, 2.031129859422152073 ) ) ;
#2454 = CARTESIAN_POINT ( 'NONE',  ( 7.000000000000000000, -15.62228920881129390, 12.61250543006183378 ) ) ;
#2455 = CARTESIAN_POINT ( 'NONE',  ( 36.52123894458239306, 336.4625677502544363, -1.853260623619672254 ) ) ;
#2456 = CARTESIAN_POINT ( 'NONE',  ( 33.76223957822399768, 470.3517299622893120, 6.012945920426372659 ) ) ;
#2457 = ORIENTED_EDGE ( 'NONE', *, *, #57891, .T. ) ;
#2458 = MECHANICAL_DESIGN_GEOMETRIC_PRESENTATION_REPRESENTATION (  '', ( #35220 ), #33445 ) ;
#2459 = CARTESIAN_POINT ( 'NONE',  ( 4.296529052608091703, 53.80523624942429706, -8.056204503449647447 ) ) ;
#2460 = EDGE_CURVE ( 'NONE', #83253, #25084, #68584, .T. ) ;
#2461 = ORIENTED_EDGE ( 'NONE', *, *, #98829, .F. ) ;
#2462 =( NAMED_UNIT ( * ) PLANE_ANGLE_UNIT ( ) SI_UNIT ( $, .RADIAN. ) );
#2463 = DIRECTION ( 'NONE',  ( 1.000000000000000000, 0.000000000000000000, 0.000000000000000000 ) ) ;
#2464 = CARTESIAN_POINT ( 'NONE',  ( 6.192999873758675555, 41.95244004319645370, -69.88362896166722749 ) ) ;
#2465 = CARTESIAN_POINT ( 'NONE',  ( -43.69716417793774355, 49.99999999999999289, 48.48761666241306756 ) ) ;
#2466 = CARTESIAN_POINT ( 'NONE',  ( 5.963307081834043899, -13.30359940716316558, 13.46515011340868639 ) ) ;
#2467 = LINE ( 'NONE', #28391, #22008 ) ;
#2468 = EDGE_LOOP ( 'NONE', ( #92470, #16063, #88334, #3572, #27114 ) ) ;
#2469 = CARTESIAN_POINT ( 'NONE',  ( 92.47524522096102828, -60.00000000000000000, -0.8168806114483707637 ) ) ;
#2471 = CARTESIAN_POINT ( 'NONE',  ( 23.10491929295638869, -60.35294240224059337, 34.93602920169672643 ) ) ;
#2470 = CARTESIAN_POINT ( 'NONE',  ( -77.72307990868957006, -60.00000000000013500, 197.5629538559897469 ) ) ;
#2473 = CARTESIAN_POINT ( 'NONE',  ( -4.425930005958662145E-15, 43.22324503868515677, 36.14046114390016839 ) ) ;
#2472 = PRODUCT_DEFINITION_CONTEXT ( 'detailed design', #67293, 'design' ) ;
#2474 = CARTESIAN_POINT ( 'NONE',  ( -23.21751746555280249, -1.200000000000000030E-05, -30.70617127781034839 ) ) ;
#2475 = CARTESIAN_POINT ( 'NONE',  ( -42.51571275536706196, -22.24532317153370187, 36.74399635000383313 ) ) ;
#2476 = CARTESIAN_POINT ( 'NONE',  ( -20.60725157157436271, 18.64284798593326897, -32.43860525506139680 ) ) ;
#2477 = UNCERTAINTY_MEASURE_WITH_UNIT (LENGTH_MEASURE( 1.000000000000000082E-05 ), #87426, 'distance_accuracy_value', 'NONE');
#2478 = EDGE_LOOP ( 'NONE', ( #75258, #41029, #82508, #53204, #82867, #87980 ) ) ;
#2479 = PRESENTATION_STYLE_ASSIGNMENT (( #51025 ) ) ;
#2480 = CARTESIAN_POINT ( 'NONE',  ( 8.000000000000000000, 9.797174393178825657E-16, -9.274828571428571422 ) ) ;
#2481 = CARTESIAN_POINT ( 'NONE',  ( 6.999999999999998224, -12.54465221550629472, 8.223849511755000563 ) ) ;
#2482 = CARTESIAN_POINT ( 'NONE',  ( 7.151217271224854954, -63.21250599554285543, -3.587901469523285591 ) ) ;
#2483 = CARTESIAN_POINT ( 'NONE',  ( -30.00000000000000355, 489.8675765671131330, 6.488452894192523246 ) ) ;
#2484 = EDGE_LOOP ( 'NONE', ( #45656, #81810, #78497, #10601 ) ) ;
#2485 = FILL_AREA_STYLE_COLOUR ( '', #14951 ) ;
#2486 = ORIENTED_EDGE ( 'NONE', *, *, #94247, .T. ) ;
#2487 = CARTESIAN_POINT ( 'NONE',  ( 95.78288065149338593, -30.00000000000000711, 191.3120139408427463 ) ) ;
#2488 = CARTESIAN_POINT ( 'NONE',  ( 42.28239405630658609, 39.52470879392900116, -49.91881956612604654 ) ) ;
#2489 = MECHANICAL_DESIGN_GEOMETRIC_PRESENTATION_REPRESENTATION (  '', ( #672 ), #12794 ) ;
#2490 = CARTESIAN_POINT ( 'NONE',  ( -4.904566723942682671, -82.97757297529254572, 3.460360782932704549 ) ) ;
#2491 = CARTESIAN_POINT ( 'NONE',  ( 81.26282277270112786, -30.00000000000000000, 25.32439451913061390 ) ) ;
#2492 = AXIS2_PLACEMENT_3D ( 'NONE', #100963, #1171, #51344 ) ;
#2493 = CARTESIAN_POINT ( 'NONE',  ( -32.16538108541509189, 380.2607361627312343, 24.62015355867497490 ) ) ;
#2494 = VERTEX_POINT ( 'NONE', #52637 ) ;
#2495 = EDGE_CURVE ( 'NONE', #39308, #32062, #96125, .T. ) ;
#2496 = PRODUCT_DEFINITION_FORMATION_WITH_SPECIFIED_SOURCE ( 'ANY', '', #75968, .NOT_KNOWN. ) ;
#2497 = AXIS2_PLACEMENT_3D ( 'NONE', #44193, #77081, #43125 ) ;
#2498 = EDGE_LOOP ( 'NONE', ( #37662, #11773, #16239, #82159 ) ) ;
#2499 = ORIENTED_EDGE ( 'NONE', *, *, #52701, .F. ) ;
#2501 = ORIENTED_EDGE ( 'NONE', *, *, #66634, .F. ) ;
#2500 = CARTESIAN_POINT ( 'NONE',  ( -46.81211797174974265, 13.24924033427093129, -15.90734432316361158 ) ) ;
#2502 = FACE_BOUND ( 'NONE', #9476, .T. ) ;
#2503 = DIRECTION ( 'NONE',  ( 0.000000000000000000, 0.000000000000000000, -1.000000000000000000 ) ) ;
#2504 = CARTESIAN_POINT ( 'NONE',  ( 37.75272971733728866, 439.5327643512869145, 23.94694555366715605 ) ) ;
#2505 = CARTESIAN_POINT ( 'NONE',  ( -30.62731428441585280, 345.4184166943421133, 19.40310956832407996 ) ) ;
#2506 = EDGE_CURVE ( 'NONE', #79080, #28854, #19010, .T. ) ;
#2507 = ORIENTED_EDGE ( 'NONE', *, *, #54982, .T. ) ;
#2508 = CARTESIAN_POINT ( 'NONE',  ( -7.996668422912395435, 49.99999999999999289, -78.85453279917057046 ) ) ;
#2509 = ORIENTED_EDGE ( 'NONE', *, *, #101781, .F. ) ;
#2510 = CARTESIAN_POINT ( 'NONE',  ( -2.797224791467303184, 15.83450757143047305, -9.607634652978001455 ) ) ;
#2511 = CARTESIAN_POINT ( 'NONE',  ( 77.13440917754967074, -38.47324727432590663, 185.0008781656527788 ) ) ;
#2512 = DIRECTION ( 'NONE',  ( -0.7142857142857147457, -0.6998542122237648710, 0.000000000000000000 ) ) ;
#2513 = CARTESIAN_POINT ( 'NONE',  ( 33.88977485408606327, 303.0407094117610427, 11.82755560641012949 ) ) ;
#2514 = CARTESIAN_POINT ( 'NONE',  ( -4.905194654929163178, 247.9760560498015423, 3.459476078998869220 ) ) ;
#2515 = VERTEX_POINT ( 'NONE', #76379 ) ;
#2516 = CARTESIAN_POINT ( 'NONE',  ( 28.46830025707781076, 12.99948816575240151, -40.55052036360860512 ) ) ;
#2517 = DIRECTION ( 'NONE',  ( -1.000000000000000000, -1.224606353822377258E-16, -0.000000000000000000 ) ) ;
#2518 = CARTESIAN_POINT ( 'NONE',  ( 40.14457621257771081, 319.6395341497199070, 7.969219972960137177 ) ) ;
#2519 = AXIS2_PLACEMENT_3D ( 'NONE', #7380, #73712, #49436 ) ;
#2520 = CARTESIAN_POINT ( 'NONE',  ( 4.966176485634622217, 41.64999999999998437, -70.47555195150158625 ) ) ;
#2521 = EDGE_CURVE ( 'NONE', #59573, #6296, #77259, .T. ) ;
#2522 = ORIENTED_EDGE ( 'NONE', *, *, #82081, .F. ) ;
#2524 = CARTESIAN_POINT ( 'NONE',  ( 5.448357755207406505, 41.97585525106359228, -59.38396075874230462 ) ) ;
#2523 =( NAMED_UNIT ( * ) SI_UNIT ( $, .STERADIAN. ) SOLID_ANGLE_UNIT ( ) );
#2525 = CARTESIAN_POINT ( 'NONE',  ( -4.448407490268954767, -1.969035902430321006, 102.6871849564181076 ) ) ;
#2526 = CARTESIAN_POINT ( 'NONE',  ( -46.00000000000000000, 438.2046082539383178, 15.52554165154989718 ) ) ;
#2527 = CARTESIAN_POINT ( 'NONE',  ( 43.43869229197123616, 464.9661605157746180, 13.42065392471466900 ) ) ;
#2528 = CARTESIAN_POINT ( 'NONE',  ( 7.447654142610081962, 302.7211820200652141, 9.909313547127384325 ) ) ;
#2529 = EDGE_CURVE ( 'NONE', #74150, #74647, #53708, .T. ) ;
#2530 = SURFACE_SIDE_STYLE ('',( #77502 ) ) ;
#2531 = AXIS2_PLACEMENT_3D ( 'NONE', #10388, #3381, #10910 ) ;
#2532 = CIRCLE ( 'NONE', #28374, 4.000000000000000888 ) ;
#2533 = DIRECTION ( 'NONE',  ( 0.8191520442889881348, 0.000000000000000000, 0.5735764363510513775 ) ) ;
#2534 = MECHANICAL_DESIGN_GEOMETRIC_PRESENTATION_REPRESENTATION (  '', ( #43885 ), #61148 ) ;
#2535 =( REPRESENTATION_RELATIONSHIP ('NONE','NONE', #69581, #7490 ) REPRESENTATION_RELATIONSHIP_WITH_TRANSFORMATION ( #52424 )SHAPE_REPRESENTATION_RELATIONSHIP( ) );
#2536 = CARTESIAN_POINT ( 'NONE',  ( 86.21552468565893435, -35.53747912697327394, 186.1477005681167043 ) ) ;
#2537 = AXIS2_PLACEMENT_3D ( 'NONE', #38078, #60218, #68831 ) ;
#2538 = CARTESIAN_POINT ( 'NONE',  ( 0.000000000000000000, 48.50000000000000000, 0.000000000000000000 ) ) ;
#2539 = CARTESIAN_POINT ( 'NONE',  ( -3.242641670810647803, 35.58872425396818073, 5.000000000000000000 ) ) ;
#2540 = EDGE_LOOP ( 'NONE', ( #72395, #48934, #97791, #99475, #11796, #101917 ) ) ;
#2541 = MECHANICAL_DESIGN_GEOMETRIC_PRESENTATION_REPRESENTATION (  '', ( #4249 ), #73113 ) ;
#2542 = CARTESIAN_POINT ( 'NONE',  ( -6.837824896291514243, 3.947820044545419016, -6.564402953523714501 ) ) ;
#2543 = PRESENTATION_STYLE_ASSIGNMENT (( #45678 ) ) ;
#2544 = LINE ( 'NONE', #17682, #16266 ) ;
#2545 = CARTESIAN_POINT ( 'NONE',  ( 17.81438722625302518, 1.482358050883964840E-15, 0.000000000000000000 ) ) ;
#2546 = CIRCLE ( 'NONE', #57651, 5.000000000000002665 ) ;
#2547 = CARTESIAN_POINT ( 'NONE',  ( -90.19056545505544875, -30.00000000000000000, 89.60777242590961578 ) ) ;
#2548 = CARTESIAN_POINT ( 'NONE',  ( -9.090909090909093493, 16.00000000000000000, 4.165977904505304252 ) ) ;
#2549 = CARTESIAN_POINT ( 'NONE',  ( 36.89180422215369504, 490.9813389901171377, 12.46623009904601886 ) ) ;
#2550 = CARTESIAN_POINT ( 'NONE',  ( -2.499999999999963141, -18.83381654053417620, 27.02533567785737034 ) ) ;
#2551 = CARTESIAN_POINT ( 'NONE',  ( -19.20992587373993743, 50.00000000000000000, 60.30093796704041154 ) ) ;
#2552 = CARTESIAN_POINT ( 'NONE',  ( 6.618366600630484875, -4.380080200177189020, -16.79229307443605634 ) ) ;
#2553 = CARTESIAN_POINT ( 'NONE',  ( 41.45706716801920777, 469.3214718807730605, 0.9913651918923074291 ) ) ;
#2554 = CARTESIAN_POINT ( 'NONE',  ( 22.68445741908610458, -19.34685978730561828, -33.34832530438864495 ) ) ;
#2555 = CARTESIAN_POINT ( 'NONE',  ( -22.30031860479850891, -32.51783567543096609, 30.11000684557585316 ) ) ;
#2556 = ORIENTED_EDGE ( 'NONE', *, *, #29649, .T. ) ;
#2557 = CARTESIAN_POINT ( 'NONE',  ( 6.222742520105473574, -7.673830019007163550, 0.2914634815676374613 ) ) ;
#2558 = CARTESIAN_POINT ( 'NONE',  ( -9.221249107921748234, 106.0482137149848683, 3.869340886054259521 ) ) ;
#2559 = CARTESIAN_POINT ( 'NONE',  ( -21.50683366985505529, -46.43907677105036669, 32.33084832063442349 ) ) ;
#2560 = CARTESIAN_POINT ( 'NONE',  ( -47.12618484245456330, -26.81580167950459170, -28.69496456390906758 ) ) ;
#2561 = AXIS2_PLACEMENT_3D ( 'NONE', #34284, #18629, #100571 ) ;
#2563 = CARTESIAN_POINT ( 'NONE',  ( 41.31926252412274181, 484.8188849810109105, -3.609462884267104599 ) ) ;
#2562 = CARTESIAN_POINT ( 'NONE',  ( -37.56673239365863282, -1.200000000000000030E-05, -12.20617127781024713 ) ) ;
#2564 = EDGE_CURVE ( 'NONE', #4789, #50935, #13795, .T. ) ;
#106785 = CARTESIAN_POINT ( 'NONE',  ( 69.96852216794175661, -47.40896019409530027, -24.11339453208464434 ) ) ;
#2566 = VERTEX_POINT ( 'NONE', #68855 ) ;
#2567 = B_SPLINE_CURVE_WITH_KNOTS ( 'NONE', 3,
 ( #39205, #46226, #104989, #12775, #64534, #37642, #54824, #79114, #30061, #62943, #46747, #49921 ),
 .UNSPECIFIED., .F., .F.,
 ( 4, 2, 2, 2, 2, 4 ),
 ( 8.673617379884035472E-19, 0.001111604437821193773, 0.002223208875642386680, 0.003334813313463579586, 0.003890615532374176039, 0.004446417751284772492 ),
 .UNSPECIFIED. ) ;
#2568 = CARTESIAN_POINT ( 'NONE',  ( 5.817833032102704749, -1.364745674339625570, -6.499999999999999112 ) ) ;
#2569 = ORIENTED_EDGE ( 'NONE', *, *, #48926, .T. ) ;
#2570 = DIRECTION ( 'NONE',  ( 0.000000000000000000, 0.000000000000000000, -1.000000000000000000 ) ) ;
#2571 = EDGE_CURVE ( 'NONE', #42449, #41982, #85836, .T. ) ;
#2572 = EDGE_CURVE ( 'NONE', #17858, #44884, #47225, .T. ) ;
#2573 = DIRECTION ( 'NONE',  ( 0.000000000000000000, 0.000000000000000000, -1.000000000000000000 ) ) ;
#2574 = CARTESIAN_POINT ( 'NONE',  ( 23.73746414932995208, 6.123233995736772199E-16, -5.000000000000001776 ) ) ;
#2575 = VERTEX_POINT ( 'NONE', #46676 ) ;
#2576 = SURFACE_STYLE_USAGE ( .BOTH. , #10140 ) ;
#2577 = CARTESIAN_POINT ( 'NONE',  ( 98.60524411875431383, -37.77932106365781095, 192.1824683179078761 ) ) ;
#2578 = CARTESIAN_POINT ( 'NONE',  ( -6.928203230275510549, -9.731166754910027805, -4.000000000000000888 ) ) ;
#2579 = VERTEX_POINT ( 'NONE', #55799 ) ;
#2580 = EDGE_CURVE ( 'NONE', #66630, #106311, #5686, .T. ) ;
#2581 = EDGE_LOOP ( 'NONE', ( #64797, #86771, #46556, #67787 ) ) ;
#2582 = ORIENTED_EDGE ( 'NONE', *, *, #56675, .F. ) ;
#2583 = CARTESIAN_POINT ( 'NONE',  ( 24.78221252497267812, 307.0969609602097421, 9.444540541783652543 ) ) ;
#2584 = FACE_OUTER_BOUND ( 'NONE', #20421, .T. ) ;
#2585 = DIRECTION ( 'NONE',  ( 0.000000000000000000, 1.000000000000000000, 0.000000000000000000 ) ) ;
#2586 = EDGE_LOOP ( 'NONE', ( #29695, #56583, #5994, #83844, #105918, #100891 ) ) ;
#2587 = STYLED_ITEM ( 'NONE', ( #104117 ), #63298 ) ;
#2588 = DIRECTION ( 'NONE',  ( -1.000000000000000000, -1.224606353822377258E-16, -0.000000000000000000 ) ) ;
#2589 = SURFACE_STYLE_FILL_AREA ( #84593 ) ;
#2590 = LINE ( 'NONE', #35540, #78896 ) ;
#2591 = CARTESIAN_POINT ( 'NONE',  ( -61.39119026585446193, -59.99999999998052402, -37.72981658969594321 ) ) ;
#2592 = CARTESIAN_POINT ( 'NONE',  ( 23.58349330513380337, -3.851859888774471706E-31, 4.000000000000001776 ) ) ;
#2593 = LINE ( 'NONE', #58178, #99366 ) ;
#2594 = CARTESIAN_POINT ( 'NONE',  ( -6.839476510410545274, 41.56703046073248231, -58.82533836030189178 ) ) ;
#2595 = AXIS2_PLACEMENT_3D ( 'NONE', #8469, #23094, #55928 ) ;
#2596 = CARTESIAN_POINT ( 'NONE',  ( -89.66254536497091010, -30.00000000000007461, 1.293233577394788725 ) ) ;
#2597 = DIRECTION ( 'NONE',  ( 0.000000000000000000, 0.000000000000000000, 1.000000000000000000 ) ) ;
#2598 = CARTESIAN_POINT ( 'NONE',  ( -49.28595117375603962, -56.83155379549049968, 55.29437192555985803 ) ) ;
#2599 = EDGE_LOOP ( 'NONE', ( #13977, #27475, #62002, #75144, #46558, #25817 ) ) ;
#2600 = CARTESIAN_POINT ( 'NONE',  ( -2.100000000000004530, 1.040949779275250140E-15, -8.500000000000000000 ) ) ;
#2601 = STYLED_ITEM ( 'NONE', ( #56556 ), #88119 ) ;
#2602 = EDGE_LOOP ( 'NONE', ( #104914, #105323, #91552, #92595, #60643, #23938 ) ) ;
#2603 = DIRECTION ( 'NONE',  ( -1.000000000000000000, -0.000000000000000000, -0.000000000000000000 ) ) ;
#2604 =( GEOMETRIC_REPRESENTATION_CONTEXT ( 3 ) GLOBAL_UNCERTAINTY_ASSIGNED_CONTEXT ( ( #62341 ) ) GLOBAL_UNIT_ASSIGNED_CONTEXT ( ( #97403, #106027, #23565 ) ) REPRESENTATION_CONTEXT ( 'NONE', 'WORKASPACE' ) );
#2605 = CARTESIAN_POINT ( 'NONE',  ( -8.392508714418884352, 295.8888084830546745, -10.03187903922855462 ) ) ;
#2606 = CARTESIAN_POINT ( 'NONE',  ( 0.000000000000000000, -46.00000000000000000, 118.0000000000000000 ) ) ;
#2607 = ORIENTED_EDGE ( 'NONE', *, *, #58675, .F. ) ;
#2608 = CARTESIAN_POINT ( 'NONE',  ( 5.725989721596479676, 246.4232288874353287, 1.809923354557179564 ) ) ;
#2609 = MECHANICAL_DESIGN_GEOMETRIC_PRESENTATION_REPRESENTATION (  '', ( #33593 ), #16398 ) ;
#2610 = CARTESIAN_POINT ( 'NONE',  ( 109.6017100556251052, -29.99999999998994582, 173.2570657943911101 ) ) ;
#2611 = DIRECTION ( 'NONE',  ( -1.000000000000000000, 0.000000000000000000, 0.000000000000000000 ) ) ;
#2612 = CARTESIAN_POINT ( 'NONE',  ( 3.350247031700846367, -48.92879585575218471, 104.4269854689279242 ) ) ;
#2613 = CARTESIAN_POINT ( 'NONE',  ( 6.814345205900305125, 41.80574652968896032, -59.39410049655393919 ) ) ;
#2614 = COLOUR_RGB ( '', 0.31764706, 0.68627451, 0.89019608) ;
#2615 = CARTESIAN_POINT ( 'NONE',  ( 86.72120758077696223, -30.00000000000000355, 182.5673864577368306 ) ) ;
#2616 =( BOUNDED_CURVE ( )  B_SPLINE_CURVE ( 2, ( #37375, #70237, #94530 ),
 .UNSPECIFIED., .F., .F. ) 
 B_SPLINE_CURVE_WITH_KNOTS ( ( 3, 3 ),
 ( 0.000000000000000000, 1.000000000000000000 ),
 .UNSPECIFIED. ) 
 CURVE ( )  GEOMETRIC_REPRESENTATION_ITEM ( )  RATIONAL_B_SPLINE_CURVE ( ( 1.000000000000000000, 1.857142857142858317, 1.000000000000000000 ) ) 
 REPRESENTATION_ITEM ( '' )  );
#2617 = CARTESIAN_POINT ( 'NONE',  ( -10.90994580868044217, 43.80550646406358339, -13.06265761667911818 ) ) ;
#2618 = CARTESIAN_POINT ( 'NONE',  ( -32.91522635463739732, 465.6822307888476189, 10.74522530471147164 ) ) ;
#2619 = EDGE_CURVE ( 'NONE', #37787, #26114, #15366, .T. ) ;
#2620 = ORIENTED_EDGE ( 'NONE', *, *, #83208, .T. ) ;
#2621 = ORIENTED_EDGE ( 'NONE', *, *, #105168, .T. ) ;
#2622 = CARTESIAN_POINT ( 'NONE',  ( 51.04619832299282223, -29.11810138070153897, 48.95650004900380736 ) ) ;
#2623 = CARTESIAN_POINT ( 'NONE',  ( 6.426573913663801818, 41.32130124522555548, -58.37301945749069887 ) ) ;
#2624 = DIRECTION ( 'NONE',  ( 0.000000000000000000, -0.3420201433256727652, -0.9396926207859068736 ) ) ;
#2625 = EDGE_CURVE ( 'NONE', #4198, #6482, #47723, .T. ) ;
#2626 = EDGE_CURVE ( 'NONE', #36026, #35969, #34172, .T. ) ;
#2627 = VERTEX_POINT ( 'NONE', #22442 ) ;
#2628 = CARTESIAN_POINT ( 'NONE',  ( -85.44393953219409354, -38.35987823094075111, -22.43841095247546846 ) ) ;
#2629 = ORIENTED_EDGE ( 'NONE', *, *, #84130, .T. ) ;
#2630 = CARTESIAN_POINT ( 'NONE',  ( 14.29190075645217206, 6.456385560668103984, 7.561819230143444592 ) ) ;
#2631 = CARTESIAN_POINT ( 'NONE',  ( 106.4348537030854942, -38.37040168822593955, 195.7536246194525233 ) ) ;
#2632 = CARTESIAN_POINT ( 'NONE',  ( 10.65954291562494660, 18.20485743982220939, 9.432410022334257960 ) ) ;
#2633 = CARTESIAN_POINT ( 'NONE',  ( 86.97191705326012823, -60.14714815928688552, 29.24646490916457253 ) ) ;
#2634 = CARTESIAN_POINT ( 'NONE',  ( 33.97359119245064818, 434.1099241184709285, 11.80501937577160732 ) ) ;
#2635 = FACE_OUTER_BOUND ( 'NONE', #40239, .T. ) ;
#2636 = CARTESIAN_POINT ( 'NONE',  ( -24.29660821760276690, 25.57666289385988634, -31.30556287864644105 ) ) ;
#2637 = CONICAL_SURFACE ( 'NONE', #73229, 4.172000000000001485, 0.9599310885968750373 ) ;
#2638 = CARTESIAN_POINT ( 'NONE',  ( 31.46253585067004721, 4.999999999999994671, 6.123233995736758394E-16 ) ) ;
#2639 = CARTESIAN_POINT ( 'NONE',  ( 8.361479372587984571, 121.1764542251201249, 0.000000000000000000 ) ) ;
#2640 = VERTEX_POINT ( 'NONE', #7263 ) ;
#2641 = CARTESIAN_POINT ( 'NONE',  ( 0.08485693624074397423, 36.30024107553217050, 29.75000000000000000 ) ) ;
#2642 = EDGE_CURVE ( 'NONE', #54959, #35138, #62880, .T. ) ;
#2643 = CARTESIAN_POINT ( 'NONE',  ( -33.00000000000000000, 500.0000000000002274, 12.00000000000000711 ) ) ;
#2644 = DIRECTION ( 'NONE',  ( -1.000000000000000000, -1.224606353822377258E-16, -0.000000000000000000 ) ) ;
#2645 = ORIENTED_EDGE ( 'NONE', *, *, #53175, .T. ) ;
#2646 = CARTESIAN_POINT ( 'NONE',  ( -28.87041204057529953, 309.8980437891780753, -7.840642016239513623 ) ) ;
#2647 = CARTESIAN_POINT ( 'NONE',  ( -27.64572936686021620, 308.2012678581347700, 11.18963121372878078 ) ) ;
#2648 = DIRECTION ( 'NONE',  ( -1.000000000000000000, -1.224606353822377258E-16, -0.000000000000000000 ) ) ;
#2649 = DIRECTION ( 'NONE',  ( -1.000000000000000000, -0.000000000000000000, -0.000000000000000000 ) ) ;
#2650 = CARTESIAN_POINT ( 'NONE',  ( 8.000000000000000000, -18.49999999999999289, 0.000000000000000000 ) ) ;
#2651 =( NAMED_UNIT ( * ) SI_UNIT ( $, .STERADIAN. ) SOLID_ANGLE_UNIT ( ) );
#2652 = CARTESIAN_POINT ( 'NONE',  ( 9.797174393178825657E-16, 115.0000000000000000, 8.000000000000000000 ) ) ;
#2653 = ORIENTED_EDGE ( 'NONE', *, *, #45199, .F. ) ;
#2654 = CARTESIAN_POINT ( 'NONE',  ( 82.22664787600508873, -53.54757062451568572, 182.7241912098365333 ) ) ;
#2655 = EDGE_CURVE ( 'NONE', #74273, #71336, #85851, .T. ) ;
#2656 = DIRECTION ( 'NONE',  ( 1.000000000000000000, -0.000000000000000000, -0.000000000000000000 ) ) ;
#2657 = CIRCLE ( 'NONE', #87073, 4.000000000000000888 ) ;
#2658 = DIRECTION ( 'NONE',  ( -1.000000000000000000, -0.000000000000000000, -0.000000000000000000 ) ) ;
#2659 = ORIENTED_EDGE ( 'NONE', *, *, #20483, .T. ) ;
#2660 = CARTESIAN_POINT ( 'NONE',  ( -87.99615528876792325, -45.26544677176889309, 58.11335563032940144 ) ) ;
#2661 = CYLINDRICAL_SURFACE ( 'NONE', #12880, 4.000000000000000000 ) ;
#2662 = CARTESIAN_POINT ( 'NONE',  ( -11.46641754970852389, -3.000000000000002665, -75.26692388747358109 ) ) ;
#2663 = DIRECTION ( 'NONE',  ( -0.000000000000000000, -0.000000000000000000, -1.000000000000000000 ) ) ;
#2664 = CARTESIAN_POINT ( 'NONE',  ( -25.04254350662498396, -27.72387814640729786, -38.37349969813231354 ) ) ;
#2665 = CIRCLE ( 'NONE', #13045, 60.50000000000000000 ) ;
#2666 = CARTESIAN_POINT ( 'NONE',  ( 51.08421898080068502, -60.00000000000001421, 74.55324466403668282 ) ) ;
#2667 = CONICAL_SURFACE ( 'NONE', #66429, 4.000000000000007105, 0.9599310885968835860 ) ;
#2668 = CARTESIAN_POINT ( 'NONE',  ( 29.78312297350667492, -32.30613403230655933, 40.45056335855814211 ) ) ;
#2669 = CARTESIAN_POINT ( 'NONE',  ( 7.999885325681426629, 108.9997706512993858, 0.2682325777720065418 ) ) ;
#2670 = CARTESIAN_POINT ( 'NONE',  ( -4.871453668401689791E-08, -12.57758911513053413, 32.18678843846154081 ) ) ;
#2672 = CARTESIAN_POINT ( 'NONE',  ( -11.11678473387292598, 19.57455013713238046, 8.700105968029125947 ) ) ;
#2671 = CARTESIAN_POINT ( 'NONE',  ( -29.94728110026810342, -32.41561811289711414, 40.54398215057806709 ) ) ;
#2673 = CARTESIAN_POINT ( 'NONE',  ( 3.947200808969410168, 295.9771890841021786, -10.00641236124329225 ) ) ;
#2674 = CIRCLE ( 'NONE', #81884, 5.000000000000001776 ) ;
#2675 = CARTESIAN_POINT ( 'NONE',  ( 38.68218982724705057, 320.0845437455996603, 16.10279619727025135 ) ) ;
#2676 = DIRECTION ( 'NONE',  ( -1.000000000000000000, 0.000000000000000000, 0.000000000000000000 ) ) ;
#2677 = CONICAL_SURFACE ( 'NONE', #11288, 8.000000000000000000, 1.047197551196600296 ) ;
#2678 = VECTOR ( 'NONE', #97428, 1000.000000000000000 ) ;
#2679 = CARTESIAN_POINT ( 'NONE',  ( -18.00000000000000355, 12.99999999999999467, 7.500000000000000000 ) ) ;
#2680 = COLOUR_RGB ( '', 0.40784314, 0.44705882, 0.49803922) ;
#2681 = VERTEX_POINT ( 'NONE', #79573 ) ;
#2682 = CARTESIAN_POINT ( 'NONE',  ( -17.35892867067943257, 294.5707697310705839, -10.05973541782409164 ) ) ;
#2683 = AXIS2_PLACEMENT_3D ( 'NONE', #101203, #1953, #77463 ) ;
#2684 = PRESENTATION_STYLE_ASSIGNMENT (( #76042 ) ) ;
#2685 = ORIENTED_EDGE ( 'NONE', *, *, #14362, .T. ) ;
#2686 = DIRECTION ( 'NONE',  ( -1.000000000000000000, -1.224606353822377258E-16, -0.000000000000000000 ) ) ;
#2687 = CARTESIAN_POINT ( 'NONE',  ( 24.83349330513380693, 4.000000000000003553, 0.000000000000000000 ) ) ;
#2688 = CARTESIAN_POINT ( 'NONE',  ( 11.31153846153846132, -4.171999999999999709, 0.000000000000000000 ) ) ;
#2690 = CARTESIAN_POINT ( 'NONE',  ( 29.14228781303362936, -60.22829445328315501, -35.25039815003416521 ) ) ;
#2689 = CARTESIAN_POINT ( 'NONE',  ( 9.483056940782045530, 252.4438779010656617, -3.177305548492613596 ) ) ;
#2691 = EDGE_CURVE ( 'NONE', #21078, #3869, #37080, .T. ) ;
#2692 = EDGE_LOOP ( 'NONE', ( #80303, #952, #87603, #34761, #102068 ) ) ;
#2693 = CARTESIAN_POINT ( 'NONE',  ( 28.35797521712592939, 36.30483405049672285, 8.953371298144853441 ) ) ;
#2694 = CARTESIAN_POINT ( 'NONE',  ( 34.10284876471455817, 6.123233995736772199E-16, -5.000000000000001776 ) ) ;
#2695 = VERTEX_POINT ( 'NONE', #38098 ) ;
#2696 = EDGE_CURVE ( 'NONE', #94469, #35136, #82320, .T. ) ;
#2697 = PLANE ( 'NONE',  #4168 ) ;
#2698 = EDGE_CURVE ( 'NONE', #37342, #96258, #37652, .T. ) ;
#2699 = DIRECTION ( 'NONE',  ( -1.000000000000000000, -1.224606353822377258E-16, -0.000000000000000000 ) ) ;
#2700 = CARTESIAN_POINT ( 'NONE',  ( -93.93600680990350327, -59.99999999999999289, 40.82566283017103359 ) ) ;
#2701 =( NAMED_UNIT ( * ) PLANE_ANGLE_UNIT ( ) SI_UNIT ( $, .RADIAN. ) );
#2702 = CARTESIAN_POINT ( 'NONE',  ( -16.10302234481894601, 5.501632350617743583, 4.770674012961006127 ) ) ;
#2703 = CARTESIAN_POINT ( 'NONE',  ( 40.62630098558985026, 465.1700311123280471, 17.15319754903183380 ) ) ;
#2704 = CARTESIAN_POINT ( 'NONE',  ( 39.69476719265632170, 459.8381870091881183, 1.879428691192534639 ) ) ;
#2706 = DIRECTION ( 'NONE',  ( -1.000000000000000000, -1.224606353822377258E-16, -0.000000000000000000 ) ) ;
#2705 = CARTESIAN_POINT ( 'NONE',  ( -8.737863884121431113, -3.000000000000002665, -90.03618980231151170 ) ) ;
#2707 = CARTESIAN_POINT ( 'NONE',  ( -84.32039038253493857, -32.46127920068834527, 171.3701678123200907 ) ) ;
#2708 = VERTEX_POINT ( 'NONE', #105446 ) ;
#2709 = CARTESIAN_POINT ( 'NONE',  ( -43.62838954006690528, 434.9736691849527119, 14.34345830637882813 ) ) ;
#2710 = EDGE_CURVE ( 'NONE', #12734, #106589, #8348, .T. ) ;
#2711 = ORIENTED_EDGE ( 'NONE', *, *, #54811, .F. ) ;
#2712 = ADVANCED_FACE ( 'NONE', ( #59027 ), #23137, .T. ) ;
#2713 = AXIS2_PLACEMENT_3D ( 'NONE', #83592, #84676, #9166 ) ;
#2714 = ORIENTED_EDGE ( 'NONE', *, *, #61379, .T. ) ;
#2715 = CARTESIAN_POINT ( 'NONE',  ( -18.68300284223528607, 303.6622989438827744, -10.04032382280791325 ) ) ;
#2716 = CARTESIAN_POINT ( 'NONE',  ( 0.2578475836320712200, 6.890627091270371096, 1.065083781909173410 ) ) ;
#2717 = ORIENTED_EDGE ( 'NONE', *, *, #21402, .F. ) ;
#2718 = B_SPLINE_CURVE_WITH_KNOTS ( 'NONE', 3,
 ( #25347, #50116, #66844, #57135 ),
 .UNSPECIFIED., .F., .F.,
 ( 4, 4 ),
 ( 9.813077866773594792E-18, 0.002032023592285936864 ),
 .UNSPECIFIED. ) ;
#2719 = DIRECTION ( 'NONE',  ( 0.000000000000000000, 1.000000000000000000, 0.000000000000000000 ) ) ;
#2720 = CARTESIAN_POINT ( 'NONE',  ( -72.13200937809398283, -57.67118076099990986, -33.88443861317198724 ) ) ;
#2721 = CARTESIAN_POINT ( 'NONE',  ( 7.344361273354515163, -12.44560530588525538, -3.175733139645583236 ) ) ;
#2722 = CARTESIAN_POINT ( 'NONE',  ( 0.08224679563971407092, 7.710515798486365036, 2.644994884459111351 ) ) ;
#2723 = CARTESIAN_POINT ( 'NONE',  ( -9.699189539447123920, 101.8230777175328541, -2.444343703917210675 ) ) ;
#2724 = DIRECTION ( 'NONE',  ( 0.000000000000000000, 0.000000000000000000, 1.000000000000000000 ) ) ;
#2725 = CARTESIAN_POINT ( 'NONE',  ( 90.94603201905546541, -14.21045842199432663, 57.96280492189741551 ) ) ;
#2726 = CARTESIAN_POINT ( 'NONE',  ( -105.0772696006729632, -59.99999999999994316, 202.2127603465211223 ) ) ;
#2727 = CARTESIAN_POINT ( 'NONE',  ( -59.57600778041714307, -42.96618104056574339, 72.74187206144701179 ) ) ;
#2728 = ORIENTED_EDGE ( 'NONE', *, *, #33471, .T. ) ;
#2729 = CARTESIAN_POINT ( 'NONE',  ( 70.41111111111112564, 3.309500000000014541, 0.000000000000000000 ) ) ;
#2730 = EDGE_LOOP ( 'NONE', ( #37276, #78580, #11053 ) ) ;
#2731 = CARTESIAN_POINT ( 'NONE',  ( -102.8035547126978884, -37.82057828177080694, 172.5329001939995237 ) ) ;
#2732 = DIRECTION ( 'NONE',  ( 0.2237693372482006948, 0.01887181578571533666, 0.9744594082240938260 ) ) ;
#2733 = CARTESIAN_POINT ( 'NONE',  ( 15.92158449169821566, 43.99413677374014497, -88.61144016494736775 ) ) ;
#2734 = ORIENTED_EDGE ( 'NONE', *, *, #52484, .F. ) ;
#2735 = CARTESIAN_POINT ( 'NONE',  ( 7.141975279376893582, -5.000000000001887379, -70.98863559356587416 ) ) ;
#2736 = CARTESIAN_POINT ( 'NONE',  ( -42.86245485551749823, -60.00000000000001421, 56.60147671463673191 ) ) ;
#2737 = CARTESIAN_POINT ( 'NONE',  ( -3.349796915303539624, -1.132149698118623871, 104.5044954676219930 ) ) ;
#2738 = CARTESIAN_POINT ( 'NONE',  ( 5.082755093536324154, -12.21875000204838635, 5.082755093536326818 ) ) ;
#2739 = CARTESIAN_POINT ( 'NONE',  ( 0.000000000000000000, 0.000000000000000000, 0.000000000000000000 ) ) ;
#2740 = CARTESIAN_POINT ( 'NONE',  ( 16.64348903516496492, 43.47556584774762456, -6.657797401562562278 ) ) ;
#2741 = CARTESIAN_POINT ( 'NONE',  ( 10.38447319516995115, -0.000000000000000000, 13.52495681779773484 ) ) ;
#2742 = CARTESIAN_POINT ( 'NONE',  ( 8.099999999999999645, 0.000000000000000000, 8.400000000000000355 ) ) ;
#2743 = CARTESIAN_POINT ( 'NONE',  ( 26.54817876223620488, 310.6276912632132507, 11.31208242866018132 ) ) ;
#2744 = CARTESIAN_POINT ( 'NONE',  ( 11.63797817910942278, -10.74185076926238835, 10.47199366613784299 ) ) ;
#2745 = CARTESIAN_POINT ( 'NONE',  ( -3.313708498984765161, -14.65625000409677092, 7.999999999999998224 ) ) ;
#2746 = AXIS2_PLACEMENT_3D ( 'NONE', #28991, #37062, #54782 ) ;
#2747 = SURFACE_STYLE_FILL_AREA ( #52362 ) ;
#2748 = UNCERTAINTY_MEASURE_WITH_UNIT (LENGTH_MEASURE( 1.000000000000000082E-05 ), #97020, 'distance_accuracy_value', 'NONE');
#2749 = CARTESIAN_POINT ( 'NONE',  ( -30.13293448531765151, -22.12503195913166110, 30.04311387844209946 ) ) ;
#2750 = UNCERTAINTY_MEASURE_WITH_UNIT (LENGTH_MEASURE( 1.000000000000000082E-05 ), #102451, 'distance_accuracy_value', 'NONE');
#2751 = CARTESIAN_POINT ( 'NONE',  ( 43.22147467150615796, -46.43435577793969316, 43.42933933853470307 ) ) ;
#2752 = CARTESIAN_POINT ( 'NONE',  ( 12.33349330513380337, 1.593028355512270567E-15, 0.000000000000000000 ) ) ;
#2753 = DIRECTION ( 'NONE',  ( -1.000000000000000000, -0.000000000000000000, -0.000000000000000000 ) ) ;
#2754 = EDGE_CURVE ( 'NONE', #17070, #82494, #76840, .T. ) ;
#2755 = CARTESIAN_POINT ( 'NONE',  ( -97.76083068359459105, -38.48065516424733801, 201.0208589095672949 ) ) ;
#2756 = MECHANICAL_DESIGN_GEOMETRIC_PRESENTATION_REPRESENTATION (  '', ( #81967 ), #99133 ) ;
#2757 = ORIENTED_EDGE ( 'NONE', *, *, #22073, .F. ) ;
#2759 = CARTESIAN_POINT ( 'NONE',  ( -28.18165013807819363, 36.45077351536222920, 8.150803961754188975 ) ) ;
#2758 = CARTESIAN_POINT ( 'NONE',  ( -9.500000000000001776, -5.000000000000000000, -36.97043916959992771 ) ) ;
#2760 = CARTESIAN_POINT ( 'NONE',  ( 43.68778998544354408, -60.00000000000005684, 47.36496327955963181 ) ) ;
#2761 = CARTESIAN_POINT ( 'NONE',  ( -18.94687734119027311, 49.29083859698900483, 62.03598969463124035 ) ) ;
#2762 = CARTESIAN_POINT ( 'NONE',  ( -7.176875562314381618, 41.55694621307963388, -59.30926738746194360 ) ) ;
#2763 = AXIS2_PLACEMENT_3D ( 'NONE', #105700, #25226, #91008 ) ;
#2764 = MECHANICAL_DESIGN_GEOMETRIC_PRESENTATION_REPRESENTATION (  '', ( #69981 ), #28682 ) ;
#2765 = CARTESIAN_POINT ( 'NONE',  ( 6.561888995895321486, 40.92548677608137808, -71.07459853153341101 ) ) ;
#2766 = CARTESIAN_POINT ( 'NONE',  ( 91.95555555555554861, 1.023464760207051730E-14, 0.000000000000000000 ) ) ;
#2767 = AXIS2_PLACEMENT_3D ( 'NONE', #31671, #31150, #97421 ) ;
#2768 = DIRECTION ( 'NONE',  ( -1.000000000000000000, -1.224606353822377258E-16, -0.000000000000000000 ) ) ;
#2769 = DIRECTION ( 'NONE',  ( 0.000000000000000000, 0.000000000000000000, 1.000000000000000000 ) ) ;
#2770 = CARTESIAN_POINT ( 'NONE',  ( 112.0087755282777380, -60.00000000000000000, 164.6420903483667360 ) ) ;
#2771 = DIRECTION ( 'NONE',  ( 0.000000000000000000, -1.000000000000000000, 0.000000000000000000 ) ) ;
#2772 = ORIENTED_EDGE ( 'NONE', *, *, #33202, .T. ) ;
#2773 = FILL_AREA_STYLE ('',( #28163 ) ) ;
#2774 = DIRECTION ( 'NONE',  ( 0.000000000000000000, 0.000000000000000000, 1.000000000000000000 ) ) ;
#2775 = ORIENTED_EDGE ( 'NONE', *, *, #92848, .T. ) ;
#2777 = DIRECTION ( 'NONE',  ( 0.000000000000000000, 0.000000000000000000, -1.000000000000000000 ) ) ;
#2776 = CARTESIAN_POINT ( 'NONE',  ( -59.44538817165069844, -38.34335046808914882, 94.60634109114953105 ) ) ;
#2778 = CARTESIAN_POINT ( 'NONE',  ( 12.49694919028371842, -3.284571130112392545, -14.00564984344996411 ) ) ;
#2779 = CARTESIAN_POINT ( 'NONE',  ( 5.947762761376476526, -6.880090707843042885, 1.083333333333332593 ) ) ;
#2780 = AXIS2_PLACEMENT_3D ( 'NONE', #38368, #105202, #96587 ) ;
#2781 = CARTESIAN_POINT ( 'NONE',  ( 6.738100180926640093, 41.71798714554645215, -59.05424661244425266 ) ) ;
#2782 = CARTESIAN_POINT ( 'NONE',  ( 7.188101187499999156, -18.12500000204838457, 2.977408999572654924 ) ) ;
#2783 =( NAMED_UNIT ( * ) PLANE_ANGLE_UNIT ( ) SI_UNIT ( $, .RADIAN. ) );
#2784 = PRODUCT_DEFINITION_SHAPE ( 'NONE', 'NONE',  #50892 ) ;
#2785 = UNCERTAINTY_MEASURE_WITH_UNIT (LENGTH_MEASURE( 1.000000000000000082E-05 ), #98574, 'distance_accuracy_value', 'NONE');
#2786 = FACE_BOUND ( 'NONE', #70567, .T. ) ;
#2788 = ORIENTED_EDGE ( 'NONE', *, *, #20568, .F. ) ;
#2787 = CARTESIAN_POINT ( 'NONE',  ( -10.28624191511820207, -1.200000000000000030E-05, 14.15779740156163946 ) ) ;
#2789 = CARTESIAN_POINT ( 'NONE',  ( 81.31019069296409896, -49.92858064726677014, 170.6618749361798280 ) ) ;
#2790 = ADVANCED_FACE ( 'NONE', ( #40699 ), #35967, .T. ) ;
#2792 = AXIS2_PLACEMENT_3D ( 'NONE', #70403, #18686, #51544 ) ;
#2791 = DIRECTION ( 'NONE',  ( -1.000000000000000000, 0.000000000000000000, 0.000000000000000000 ) ) ;
#2793 = CARTESIAN_POINT ( 'NONE',  ( 9.843481099141458301, 88.59204556153383692, -1.779148000612192693 ) ) ;
#2794 = ORIENTED_EDGE ( 'NONE', *, *, #73377, .F. ) ;
#2795 = CARTESIAN_POINT ( 'NONE',  ( -6.125000000000002665, -15.62228920881133654, 14.41094225130411211 ) ) ;
#2796 = DIRECTION ( 'NONE',  ( -0.000000000000000000, 0.000000000000000000, -1.000000000000000000 ) ) ;
#2797 = CARTESIAN_POINT ( 'NONE',  ( 1.647285698089598460, -3.000000000000002665, -70.00000000000000000 ) ) ;
#2798 = LINE ( 'NONE', #17412, #267 ) ;
#2799 = AXIS2_PLACEMENT_3D ( 'NONE', #15203, #105805, #48091 ) ;
#2800 = CARTESIAN_POINT ( 'NONE',  ( -5.856955515201470064, 253.7828905888086410, 1.326217528971443294 ) ) ;
#2801 = CARTESIAN_POINT ( 'NONE',  ( -43.52075891743682234, 484.7805561108189636, 4.063293749114582631 ) ) ;
#2802 = CARTESIAN_POINT ( 'NONE',  ( 7.878970821878172437, 3.088077109979846302, 14.68021914166114783 ) ) ;
#2803 = ORIENTED_EDGE ( 'NONE', *, *, #49663, .F. ) ;
#2804 = DIRECTION ( 'NONE',  ( -2.289888280286174020E-15, 0.1409055682485933769, -0.9900230405584211635 ) ) ;
#2805 = CARTESIAN_POINT ( 'NONE',  ( 35.39685905336809668, 18.64284798592731462, 14.96610495030122934 ) ) ;
#2806 = CARTESIAN_POINT ( 'NONE',  ( 86.80848714680104194, -20.64835433331844783, 185.6727037537062586 ) ) ;
#2807 = CARTESIAN_POINT ( 'NONE',  ( 43.50377727019363761, 435.9167426301696082, 18.24083946424738301 ) ) ;
#2808 = CARTESIAN_POINT ( 'NONE',  ( -5.082755093536326818, -22.71875000204838457, 5.082755093536325042 ) ) ;
#2809 = CARTESIAN_POINT ( 'NONE',  ( -42.74810220189110765, 488.2594957234280173, 9.352615981973224635 ) ) ;
#2810 = CARTESIAN_POINT ( 'NONE',  ( 43.86650669486618881, 1.474610560812782335E-15, 0.000000000000000000 ) ) ;
#2811 = CARTESIAN_POINT ( 'NONE',  ( 41.09279801121592612, 437.4012895414161335, 21.36373234332642923 ) ) ;
#2812 = AXIS2_PLACEMENT_3D ( 'NONE', #43526, #85046, #52129 ) ;
#2813 = ITEM_DEFINED_TRANSFORMATION ( 'NONE', 'NONE', #62804,  #10728 ) ;
#2814 = VERTEX_POINT ( 'NONE', #48778 ) ;
#2815 = DIRECTION ( 'NONE',  ( -0.5735764363510497121, 0.8191520442889892450, 1.003171929053521665E-16 ) ) ;
#2816 = SURFACE_STYLE_FILL_AREA ( #76705 ) ;
#2817 =( NAMED_UNIT ( * ) PLANE_ANGLE_UNIT ( ) SI_UNIT ( $, .RADIAN. ) );
#2818 = CARTESIAN_POINT ( 'NONE',  ( 21.84999999999999787, 1.533819458162526451E-15, 0.000000000000000000 ) ) ;
#2819 = AXIS2_PLACEMENT_3D ( 'NONE', #103380, #93700, #52687 ) ;
#2820 = ORIENTED_EDGE ( 'NONE', *, *, #74300, .F. ) ;
#2821 = CARTESIAN_POINT ( 'NONE',  ( 8.000000000000000000, -16.90624999999999289, -3.313708498984761164 ) ) ;
#2822 = CARTESIAN_POINT ( 'NONE',  ( -10.51296777078104050, 50.00000000000000000, -92.64705882352942012 ) ) ;
#2823 = VECTOR ( 'NONE', #83219, 999.9999999999998863 ) ;
#2824 = CARTESIAN_POINT ( 'NONE',  ( 4.733165431326070832E-26, 13.70447791526910919, -49.25000000000000000 ) ) ;
#2825 = CARTESIAN_POINT ( 'NONE',  ( -34.88900972249400212, 464.6206820655984870, 18.69027339340994232 ) ) ;
#2826 = CARTESIAN_POINT ( 'NONE',  ( -17.16184658094835314, 36.31812281971417633, 24.24086490087779922 ) ) ;
#2827 = CARTESIAN_POINT ( 'NONE',  ( -93.50040392359746022, -60.00000000000000000, 202.5177011504292466 ) ) ;
#2828 = PRODUCT_DEFINITION_SHAPE ( 'NONE', 'NONE',  #106813 ) ;
#2829 = CONICAL_SURFACE ( 'NONE', #16622, 11.96035173608223090, 1.221730476396025722 ) ;
#2830 = CARTESIAN_POINT ( 'NONE',  ( 19.50000000000170175, 50.00000000000003553, 59.91915230424470451 ) ) ;
#2831 = AXIS2_PLACEMENT_3D ( 'NONE', #25998, #60988, #2181 ) ;
#2832 = CARTESIAN_POINT ( 'NONE',  ( 9.040080106534270854, 43.92515280565064018, -14.03042987452793788 ) ) ;
#2833 = CARTESIAN_POINT ( 'NONE',  ( -82.95741313463533118, -57.28139562845189658, 188.3880023493264275 ) ) ;
#2834 = CARTESIAN_POINT ( 'NONE',  ( -4.048979898151962686, 53.98330245238265945, -7.635038885512192230 ) ) ;
#2835 = VECTOR ( 'NONE', #86940, 1000.000000000000000 ) ;
#2836 = ADVANCED_FACE ( 'NONE', ( #67115 ), #3976, .F. ) ;
#2837 = ORIENTED_EDGE ( 'NONE', *, *, #93820, .T. ) ;
#2838 = CARTESIAN_POINT ( 'NONE',  ( 8.000000000000000000, -25.90624999999999645, -3.313708498984761164 ) ) ;
#2839 = ADVANCED_FACE ( 'NONE', ( #94600 ), #53586, .F. ) ;
#2840 = CARTESIAN_POINT ( 'NONE',  ( 3.459690225508319283, -1.108983740916838379, 104.5059395991341660 ) ) ;
#2841 = CARTESIAN_POINT ( 'NONE',  ( -85.42014498610673456, -52.71254651111112111, 0.1204113182908394392 ) ) ;
#2842 = CARTESIAN_POINT ( 'NONE',  ( -6.163128221576519294, -12.12876728480168254, -8.844179776184848407 ) ) ;
#2843 = CARTESIAN_POINT ( 'NONE',  ( -4.921285567847696107, 6.866253350555239443, -5.000000000000000000 ) ) ;
#2844 = CARTESIAN_POINT ( 'NONE',  ( 18.58349330513380693, 1.593028355512270962E-15, 0.000000000000000000 ) ) ;
#2845 = CARTESIAN_POINT ( 'NONE',  ( -6.163737169368993740, -12.13805321688065320, 11.84025182891627992 ) ) ;
#2846 = CARTESIAN_POINT ( 'NONE',  ( 23.70422451878993186, 42.00000000000000000, 88.20421627933662023 ) ) ;
#2847 = CARTESIAN_POINT ( 'NONE',  ( 72.11378188144121282, -59.99999999999999289, 177.1381934468311670 ) ) ;
#2848 = CARTESIAN_POINT ( 'NONE',  ( -87.24749885984873288, -14.21045842199425024, -0.3946065656837255964 ) ) ;
#2849 = CARTESIAN_POINT ( 'NONE',  ( -72.91763775797275571, -42.96435045428120958, 114.3462633838142892 ) ) ;
#2850 = ORIENTED_EDGE ( 'NONE', *, *, #40644, .F. ) ;
#2851 = CARTESIAN_POINT ( 'NONE',  ( 109.5593579388806091, -60.00000000000008527, 197.6560947019162597 ) ) ;
#2852 = CARTESIAN_POINT ( 'NONE',  ( 63.17895952939625914, 40.83918185556188263, 15.56336160550995906 ) ) ;
#2853 = CARTESIAN_POINT ( 'NONE',  ( 51.50543603504199552, -57.67116266638129218, -39.62106952943562277 ) ) ;
#2854 = ORIENTED_EDGE ( 'NONE', *, *, #51839, .T. ) ;
#2855 = DIRECTION ( 'NONE',  ( 0.5735764363510490460, 0.8191520442889896891, 0.000000000000000000 ) ) ;
#2856 = CARTESIAN_POINT ( 'NONE',  ( -7.188101187500000044, -24.78125000204838813, -8.802885111219163269E-16 ) ) ;
#2857 = CARTESIAN_POINT ( 'NONE',  ( -1.249627314476824180, 27.80309404206683155, -39.33848994184150172 ) ) ;
#2858 = ORIENTED_EDGE ( 'NONE', *, *, #105350, .T. ) ;
#2859 = AXIS2_PLACEMENT_3D ( 'NONE', #60601, #11472, #28790 ) ;
#2860 = DIRECTION ( 'NONE',  ( -0.000000000000000000, -0.000000000000000000, -1.000000000000000000 ) ) ;
#2861 = ORIENTED_EDGE ( 'NONE', *, *, #59032, .T. ) ;
#2862 = DIRECTION ( 'NONE',  ( 0.000000000000000000, 1.000000000000000000, 0.000000000000000000 ) ) ;
#2863 = CARTESIAN_POINT ( 'NONE',  ( 47.55680477683365126, 16.06931990738367233, -16.76905664007707841 ) ) ;
#2864 = CARTESIAN_POINT ( 'NONE',  ( -35.02057590403620679, -60.00000000000246558, 49.66482031158606958 ) ) ;
#2865 = CARTESIAN_POINT ( 'NONE',  ( 21.11457545795382984, 303.9328293617413692, -9.982777457638777108 ) ) ;
#2866 = CARTESIAN_POINT ( 'NONE',  ( 4.401442555609581635E-16, -12.78125000204838280, -7.188101187500000044 ) ) ;
#2867 = CARTESIAN_POINT ( 'NONE',  ( -10.00000000000000178, -15.00000000000000000, -9.999999999999998224 ) ) ;
#2868 =( GEOMETRIC_REPRESENTATION_CONTEXT ( 3 ) GLOBAL_UNCERTAINTY_ASSIGNED_CONTEXT ( ( #35159 ) ) GLOBAL_UNIT_ASSIGNED_CONTEXT ( ( #1533, #18847, #75975 ) ) REPRESENTATION_CONTEXT ( 'NONE', 'WORKASPACE' ) );
#2869 = CARTESIAN_POINT ( 'NONE',  ( 11.89131030317610183, 1.482358050883964840E-15, 0.000000000000000000 ) ) ;
#2870 = DIRECTION ( 'NONE',  ( 0.000000000000000000, -1.000000000000000000, 0.000000000000000000 ) ) ;
#2871 = DIRECTION ( 'NONE',  ( 1.224646799147353700E-16, 0.000000000000000000, -1.000000000000000000 ) ) ;
#2872 = ORIENTED_EDGE ( 'NONE', *, *, #35904, .F. ) ;
#2874 = CARTESIAN_POINT ( 'NONE',  ( 33.01644511546025740, -60.30961634571765018, 38.16996237056868324 ) ) ;
#2873 = CARTESIAN_POINT ( 'NONE',  ( 20.59999999999999787, 3.309500000000003439, 0.000000000000000000 ) ) ;
#2875 = CARTESIAN_POINT ( 'NONE',  ( 41.50669491856072568, 5.000000000000002665, 0.000000000000000000 ) ) ;
#2876 = EDGE_LOOP ( 'NONE', ( #92110, #45201, #50312, #39231 ) ) ;
#2877 = CARTESIAN_POINT ( 'NONE',  ( -1.308996938995748316, 48.00000000000000711, -75.00000000000001421 ) ) ;
#2878 = ADVANCED_FACE ( 'NONE', ( #68727 ), #101549, .F. ) ;
#2880 = CARTESIAN_POINT ( 'NONE',  ( 7.922281120364393914, 4.573931137438267847, -8.047472243342932430 ) ) ;
#2879 = CARTESIAN_POINT ( 'NONE',  ( 6.701893401236465486, 41.44328394225253476, -70.59544911815949320 ) ) ;
#2881 = CYLINDRICAL_SURFACE ( 'NONE', #76744, 8.000000000000000000 ) ;
#2882 = CARTESIAN_POINT ( 'NONE',  ( -20.19958611121843362, 294.7560298975799924, -2.020357152961808289 ) ) ;
#2884 = CONICAL_SURFACE ( 'NONE', #63193, 3.309500000000007880, 0.9599310885968770357 ) ;
#2883 = DIRECTION ( 'NONE',  ( 0.000000000000000000, -1.000000000000000000, 0.000000000000000000 ) ) ;
#2885 = CARTESIAN_POINT ( 'NONE',  ( -34.16642289233707430, 463.8422268500496557, 18.98106911353877280 ) ) ;
#2886 = VERTEX_POINT ( 'NONE', #36906 ) ;
#2887 = CARTESIAN_POINT ( 'NONE',  ( 92.56471944205797797, -60.00000000000000711, -2.224637919256570395 ) ) ;
#2888 = CIRCLE ( 'NONE', #37354, 4.000000000000001776 ) ;
#2889 = DIRECTION ( 'NONE',  ( 0.000000000000000000, 0.000000000000000000, 1.000000000000000000 ) ) ;
#2890 = CARTESIAN_POINT ( 'NONE',  ( -35.76606322701502449, 391.3003520932923038, 5.706814156549728345 ) ) ;
#2891 = CARTESIAN_POINT ( 'NONE',  ( -6.280859837934959167, 40.29318109963620032, -71.19386791582113005 ) ) ;
#2892 = DIRECTION ( 'NONE',  ( -1.000000000000000000, 0.000000000000000000, 0.000000000000000000 ) ) ;
#2893 = EDGE_CURVE ( 'NONE', #59552, #21594, #61508, .T. ) ;
#2894 = ORIENTED_EDGE ( 'NONE', *, *, #51724, .F. ) ;
#2895 = CARTESIAN_POINT ( 'NONE',  ( -93.89469422640124208, -30.00000000003503686, 199.9082004840001332 ) ) ;
#2896 = EDGE_LOOP ( 'NONE', ( #24599, #12781 ) ) ;
#2897 = CARTESIAN_POINT ( 'NONE',  ( 7.999999999999998224, -11.09374999999999289, 3.313708498984766049 ) ) ;
#2898 = CARTESIAN_POINT ( 'NONE',  ( 0.000000000000000000, 0.000000000000000000, 0.000000000000000000 ) ) ;
#2899 = CARTESIAN_POINT ( 'NONE',  ( 4.999999999999993783, -46.00000000000000000, 102.2532056551910387 ) ) ;
#2900 = DIRECTION ( 'NONE',  ( 0.000000000000000000, -1.000000000000000000, 0.000000000000000000 ) ) ;
#2901 = CARTESIAN_POINT ( 'NONE',  ( 83.19333843231504488, -37.80199420799200993, -9.185050932785989275 ) ) ;
#2902 = CIRCLE ( 'NONE', #87312, 4.000000000000000888 ) ;
#2903 = CARTESIAN_POINT ( 'NONE',  ( -41.62319636543390544, 315.3244859196361745, -5.086071370403092651 ) ) ;
#2904 = LINE ( 'NONE', #100543, #59383 ) ;
#2905 = CARTESIAN_POINT ( 'NONE',  ( -10.28624191512074226, 46.12099395432516502, 12.90779740155501187 ) ) ;
#2906 = CARTESIAN_POINT ( 'NONE',  ( -15.63133122982432788, 304.5550785334672241, 8.873930169606314422 ) ) ;
#2907 = ORIENTED_EDGE ( 'NONE', *, *, #36895, .T. ) ;
#2908 = FACE_OUTER_BOUND ( 'NONE', #69505, .T. ) ;
#2909 = ORIENTED_EDGE ( 'NONE', *, *, #91249, .F. ) ;
#2910 = CARTESIAN_POINT ( 'NONE',  ( 33.00000000000000000, 490.5636507777048791, 7.413185101890169548 ) ) ;
#2911 = FACE_OUTER_BOUND ( 'NONE', #70556, .T. ) ;
#2912 = STYLED_ITEM ( 'NONE', ( #8871 ), #23880 ) ;
#2913 = CIRCLE ( 'NONE', #99363, 12.00000000000003908 ) ;
#2914 = VECTOR ( 'NONE', #29107, 1000.000000000000000 ) ;
#2915 = CONICAL_SURFACE ( 'NONE', #63217, 4.000000000000001776, 0.9599310885968774798 ) ;
#2917 = VERTEX_POINT ( 'NONE', #55155 ) ;
#2916 = CARTESIAN_POINT ( 'NONE',  ( 5.290067270632455632, 51.34639538792298197, 8.531152949374481764 ) ) ;
#2918 = CARTESIAN_POINT ( 'NONE',  ( 76.37327748893468993, -36.02034588710548491, 123.8589219231648855 ) ) ;
#2919 = ADVANCED_FACE ( 'NONE', ( #71882 ), #87035, .T. ) ;
#2920 = AXIS2_PLACEMENT_3D ( 'NONE', #53793, #102886, #79128 ) ;
#2921 = ORIENTED_EDGE ( 'NONE', *, *, #80243, .F. ) ;
#2922 = CARTESIAN_POINT ( 'NONE',  ( 1.078711167028171491, -50.02722306961814525, 40.96723994058017126 ) ) ;
#2924 = CARTESIAN_POINT ( 'NONE',  ( 88.20199406385988539, -2.002967142162725287E-29, 5.000000000000011546 ) ) ;
#2923 = PRESENTATION_LAYER_ASSIGNMENT (  '', '', ( #30525 ) ) ;
#2925 = CARTESIAN_POINT ( 'NONE',  ( -1.320432766682874540E-15, -24.03125000204838457, 7.188101187500000044 ) ) ;
#2926 = CARTESIAN_POINT ( 'NONE',  ( -104.5387911149144600, -57.64184148030879840, 201.9936694370400971 ) ) ;
#2927 = ADVANCED_FACE ( 'NONE', ( #13638 ), #105319, .F. ) ;
#2928 = ORIENTED_EDGE ( 'NONE', *, *, #73513, .F. ) ;
#2929 = FACE_OUTER_BOUND ( 'NONE', #102349, .T. ) ;
#2930 = CARTESIAN_POINT ( 'NONE',  ( 104.0473560679520801, -45.28269839500234895, 172.6637801801720684 ) ) ;
#2931 = EDGE_CURVE ( 'NONE', #52425, #96464, #4502, .T. ) ;
#2932 = DIRECTION ( 'NONE',  ( -0.9081249930085217859, -0.3474488548199749505, -0.2336413712456777148 ) ) ;
#2933 = CARTESIAN_POINT ( 'NONE',  ( 57.45015997180046696, 6.975173280561618775E-15, 0.000000000000000000 ) ) ;
#2934 = CARTESIAN_POINT ( 'NONE',  ( -8.000000000000000000, -18.03125000409677625, -3.313708498984762496 ) ) ;
#2935 = CARTESIAN_POINT ( 'NONE',  ( 29.08076923076923137, 1.411358822780289120E-15, 0.000000000000000000 ) ) ;
#2936 = CARTESIAN_POINT ( 'NONE',  ( 9.253800200985700997, 248.6998966891182192, -3.791983798715486742 ) ) ;
#2937 = CARTESIAN_POINT ( 'NONE',  ( -46.00000000000000000, 500.0000000000002274, -12.00000000000000711 ) ) ;
#2938 = AXIS2_PLACEMENT_3D ( 'NONE', #34087, #17353, #89632 ) ;
#2939 =( LENGTH_UNIT ( ) NAMED_UNIT ( * ) SI_UNIT ( .MILLI., .METRE. ) );
#2940 = DIRECTION ( 'NONE',  ( 0.000000000000000000, -1.000000000000000000, 0.000000000000000000 ) ) ;
#2942 = EDGE_CURVE ( 'NONE', #74862, #76857, #36953, .T. ) ;
#2941 = CARTESIAN_POINT ( 'NONE',  ( 89.88291765283142354, 410.1183258646379386, 267.1969486012845891 ) ) ;
#2943 = CARTESIAN_POINT ( 'NONE',  ( 33.82585650164579505, 464.6969192971359917, 6.993179704490867010 ) ) ;
#2944 = VERTEX_POINT ( 'NONE', #54614 ) ;
#2945 = CARTESIAN_POINT ( 'NONE',  ( -2.634824035318301672, -49.75410657075519083, 40.87749690338997510 ) ) ;
#2946 = CARTESIAN_POINT ( 'NONE',  ( 10.50000000000000178, -5.000000000000000000, -12.52300748975612166 ) ) ;
#2947 = FACE_OUTER_BOUND ( 'NONE', #77757, .T. ) ;
#2948 = CARTESIAN_POINT ( 'NONE',  ( -88.78165138298567172, -30.00000000000001066, 188.3707320087108030 ) ) ;
#2949 = EDGE_LOOP ( 'NONE', ( #54230, #90431, #43201, #105627 ) ) ;
#2950 = CARTESIAN_POINT ( 'NONE',  ( -1.757245493087633337, -4.333298119783843383, 17.83319508841453427 ) ) ;
#2951 = CARTESIAN_POINT ( 'NONE',  ( 81.60669281017756305, -57.51821468741594856, 200.2139519186157770 ) ) ;
#2953 = CARTESIAN_POINT ( 'NONE',  ( 1.308996938995746984, 47.99999999999999289, -75.00000000000000000 ) ) ;
#2952 = CARTESIAN_POINT ( 'NONE',  ( -14.97625732068919469, 1.268789641109800748, -0.8714310519133426913 ) ) ;
#2954 = AXIS2_PLACEMENT_3D ( 'NONE', #68956, #94281, #4204 ) ;
#2955 = CARTESIAN_POINT ( 'NONE',  ( 66.88170049462542011, -38.03301857054354684, -32.23619581494182995 ) ) ;
#2956 =( NAMED_UNIT ( * ) SI_UNIT ( $, .STERADIAN. ) SOLID_ANGLE_UNIT ( ) );
#2957 = CARTESIAN_POINT ( 'NONE',  ( 5.036189803708992940, -3.000000000000003109, -76.26213611645744095 ) ) ;
#2958 = CARTESIAN_POINT ( 'NONE',  ( -51.02129726669660670, -60.00000000000000000, 74.38172674847689336 ) ) ;
#2959 =( GEOMETRIC_REPRESENTATION_CONTEXT ( 3 ) GLOBAL_UNCERTAINTY_ASSIGNED_CONTEXT ( ( #93375 ) ) GLOBAL_UNIT_ASSIGNED_CONTEXT ( ( #93969, #105623, #78297 ) ) REPRESENTATION_CONTEXT ( 'NONE', 'WORKASPACE' ) );
#2960 = CARTESIAN_POINT ( 'NONE',  ( -10.51296777078104050, 50.00000000000000000, -92.64705882352942012 ) ) ;
#2961 = CARTESIAN_POINT ( 'NONE',  ( 52.56483885390522204, 48.00000000000000000, -38.23529411764705799 ) ) ;
#2962 = VECTOR ( 'NONE', #33069, 1000.000000000000000 ) ;
#2963 = CARTESIAN_POINT ( 'NONE',  ( -85.92024107957429635, -53.82049793324690512, 191.8561986361768277 ) ) ;
#2964 = ORIENTED_EDGE ( 'NONE', *, *, #6813, .T. ) ;
#2965 = CARTESIAN_POINT ( 'NONE',  ( -41.98130293123099932, 462.0609698853085661, 3.143960326148259377 ) ) ;
#2966 = CARTESIAN_POINT ( 'NONE',  ( -4.115265312743041193, -56.88410095382541698, 33.36240466207844690 ) ) ;
#2967 = CARTESIAN_POINT ( 'NONE',  ( -46.00000000000000000, 450.0000000000002274, 18.20242257375371153 ) ) ;
#2968 = CARTESIAN_POINT ( 'NONE',  ( -37.45552949318529556, 490.9506234891537702, 12.34579642396192156 ) ) ;
#2970 = DIRECTION ( 'NONE',  ( -0.000000000000000000, -1.000000000000000000, -0.000000000000000000 ) ) ;
#2969 = CARTESIAN_POINT ( 'NONE',  ( -39.34066475191858103, 315.0823817570354208, 6.824423801037188930 ) ) ;
#2971 = ADVANCED_FACE ( 'NONE', ( #96701 ), #25647, .T. ) ;
#2972 = ORIENTED_EDGE ( 'NONE', *, *, #70560, .F. ) ;
#2973 = CARTESIAN_POINT ( 'NONE',  ( -35.71679196358923747, 338.0497572594834992, -1.698451522311290374 ) ) ;
#2974 = DIRECTION ( 'NONE',  ( 1.000000000000000000, 1.224606353822377258E-16, 0.000000000000000000 ) ) ;
#2975 = CARTESIAN_POINT ( 'NONE',  ( 11.36650669486618881, 1.474610560812782335E-15, 0.000000000000000000 ) ) ;
#2976 = CARTESIAN_POINT ( 'NONE',  ( -30.00000000000000000, 0.000000000000000000, 5.999999999999998224 ) ) ;
#2977 = PRESENTATION_LAYER_ASSIGNMENT (  '', '', ( #49484 ) ) ;
#2978 = AXIS2_PLACEMENT_3D ( 'NONE', #34068, #74474, #74998 ) ;
#2979 = CARTESIAN_POINT ( 'NONE',  ( 27.31492851351466200, 296.3978788581767390, -1.665144278812466183 ) ) ;
#2980 = EDGE_CURVE ( 'NONE', #76213, #10553, #71785, .T. ) ;
#2981 = CARTESIAN_POINT ( 'NONE',  ( 35.76320840016588676, 388.4727839510825333, 5.610592865731860002 ) ) ;
#2982 = DIRECTION ( 'NONE',  ( 0.000000000000000000, 0.000000000000000000, -1.000000000000000000 ) ) ;
#2983 = CARTESIAN_POINT ( 'NONE',  ( 9.183451665179635626, 53.50050700487116728, -3.876548107677253441 ) ) ;
#2984 = CARTESIAN_POINT ( 'NONE',  ( 95.66379843407523254, -59.99999999999997158, 35.18487050012404893 ) ) ;
#2985 = CARTESIAN_POINT ( 'NONE',  ( -82.92168442201257506, -18.68762057716829617, 141.1249244015832005 ) ) ;
#2986 = ORIENTED_EDGE ( 'NONE', *, *, #75474, .F. ) ;
#2987 = DIRECTION ( 'NONE',  ( -0.5735764363510510444, -0.8191520442889883569, 0.000000000000000000 ) ) ;
#2988 = DIRECTION ( 'NONE',  ( -1.000000000000000000, -1.224606353822377258E-16, -0.000000000000000000 ) ) ;
#2989 = VECTOR ( 'NONE', #10092, 1000.000000000000000 ) ;
#2990 = CARTESIAN_POINT ( 'NONE',  ( 38.37663786125177978, -57.69558054003382352, 53.18690643716654876 ) ) ;
#2991 = CIRCLE ( 'NONE', #59839, 4.999999999999993783 ) ;
#2992 = AXIS2_PLACEMENT_3D ( 'NONE', #9193, #58842, #1081 ) ;
#2993 = AXIS2_PLACEMENT_3D ( 'NONE', #33026, #81514, #9236 ) ;
#2994 = CYLINDRICAL_SURFACE ( 'NONE', #45972, 5.000000000000002665 ) ;
#2995 = ADVANCED_FACE ( 'NONE', ( #22840 ), #30703, .F. ) ;
#2996 = CARTESIAN_POINT ( 'NONE',  ( 36.70943602865214928, 339.3630517424467712, -1.204202434040655856 ) ) ;
#2997 = DIRECTION ( 'NONE',  ( -1.000000000000000000, -1.224606353822377258E-16, -0.000000000000000000 ) ) ;
#2998 = VERTEX_POINT ( 'NONE', #46553 ) ;
#2999 = DIRECTION ( 'NONE',  ( -0.5735764363510512664, 0.8191520442889881348, 1.003171929053520309E-16 ) ) ;
#3000 = CARTESIAN_POINT ( 'NONE',  ( 31.96364149859393677, 438.9703530481821758, 23.62892465267417208 ) ) ;
#3001 = CARTESIAN_POINT ( 'NONE',  ( 4.401442555609581635E-16, -30.78125000204838813, -7.188101187500000044 ) ) ;
#3002 = EDGE_LOOP ( 'NONE', ( #92647, #32866, #64656, #29676 ) ) ;
#3003 =( LENGTH_UNIT ( ) NAMED_UNIT ( * ) SI_UNIT ( .MILLI., .METRE. ) );
#3004 = AXIS2_PLACEMENT_3D ( 'NONE', #74335, #98083, #408 ) ;
#3005 = CARTESIAN_POINT ( 'NONE',  ( -7.899999792244740249, 11.02739026146940660, -13.00000000000001066 ) ) ;
#3006 = CARTESIAN_POINT ( 'NONE',  ( 6.701893401236465486, 41.44328394225253476, -70.59544911815949320 ) ) ;
#3007 = CARTESIAN_POINT ( 'NONE',  ( 5.957442974701733007, 49.99999999999999289, 65.00000000000000000 ) ) ;
#3008 = CARTESIAN_POINT ( 'NONE',  ( 0.000000000000000000, 0.000000000000000000, 0.000000000000000000 ) ) ;
#3009 = CARTESIAN_POINT ( 'NONE',  ( -23.38216085046615689, 27.34669553923654561, -33.20617127781036260 ) ) ;
#3010 = EDGE_LOOP ( 'NONE', ( #61446, #47558, #91406, #85811, #6860 ) ) ;
#3011 = CARTESIAN_POINT ( 'NONE',  ( 47.02104799127375401, -59.99999999999997868, -38.48628389369286396 ) ) ;
#3013 = CARTESIAN_POINT ( 'NONE',  ( 22.29962909612223498, -32.51552189962478678, 30.10951381722811249 ) ) ;
#3012 = CARTESIAN_POINT ( 'NONE',  ( -76.70274796309844589, -29.99999999999996447, 172.7051753936532066 ) ) ;
#3014 = CARTESIAN_POINT ( 'NONE',  ( -3.409519076813957649E-15, 51.11204936430951307, 27.84083606136722366 ) ) ;
#3015 = CARTESIAN_POINT ( 'NONE',  ( -33.84603987176726747, -46.43407376650471718, 36.05494947502590009 ) ) ;
#3016 = ADVANCED_FACE ( 'NONE', ( #87556 ), #6612, .T. ) ;
#3017 = AXIS2_PLACEMENT_3D ( 'NONE', #2097, #52252, #60381 ) ;
#3018 = UNCERTAINTY_MEASURE_WITH_UNIT (LENGTH_MEASURE( 1.000000000000000082E-05 ), #42303, 'distance_accuracy_value', 'NONE');
#3019 = ORIENTED_EDGE ( 'NONE', *, *, #75288, .F. ) ;
#3020 = DIRECTION ( 'NONE',  ( 0.000000000000000000, 0.000000000000000000, 1.000000000000000000 ) ) ;
#3021 = CARTESIAN_POINT ( 'NONE',  ( -4.472135954999578722, 249.9999999999999432, 4.000000000000002665 ) ) ;
#3022 = CARTESIAN_POINT ( 'NONE',  ( -13.45844672282477816, -54.52686498230426793, 23.14344092887451154 ) ) ;
#3023 = DIRECTION ( 'NONE',  ( -1.000000000000000000, 0.000000000000000000, 0.000000000000000000 ) ) ;
#3024 = CARTESIAN_POINT ( 'NONE',  ( 7.211357414135266986, -62.98853460065557641, 3.467230644691331687 ) ) ;
#3025 = CARTESIAN_POINT ( 'NONE',  ( -14.44581512912408705, 5.963299184987270074, 7.135127315202455911 ) ) ;
#3027 = VERTEX_POINT ( 'NONE', #5040 ) ;
#3026 = CIRCLE ( 'NONE', #46156, 5.000000000000002665 ) ;
#3028 = DIRECTION ( 'NONE',  ( 0.000000000000000000, 0.000000000000000000, -1.000000000000000000 ) ) ;
#3029 = ORIENTED_EDGE ( 'NONE', *, *, #79397, .F. ) ;
#3030 = CARTESIAN_POINT ( 'NONE',  ( 98.32497725137756106, -30.00000000000000711, 190.1228518036747630 ) ) ;
#3031 = CARTESIAN_POINT ( 'NONE',  ( 33.09766195399677713, 40.69685746902134582, -62.13808003497683075 ) ) ;
#3032 = UNCERTAINTY_MEASURE_WITH_UNIT (LENGTH_MEASURE( 1.000000000000000082E-05 ), #5940, 'distance_accuracy_value', 'NONE');
#3033 = CARTESIAN_POINT ( 'NONE',  ( -5.856955515201466511, -81.21710941119138738, 1.326217528971465942 ) ) ;
#3034 = TOROIDAL_SURFACE ( 'NONE', #73617, 9.500000000000000000, 2.000000000000000000 ) ;
#3035 = CARTESIAN_POINT ( 'NONE',  ( 82.00736216671209888, -29.99999999999999645, 34.01753071249959959 ) ) ;
#3036 = CARTESIAN_POINT ( 'NONE',  ( -25.35453098390112103, 306.3427856472554254, 10.49981900249395750 ) ) ;
#3037 = EDGE_CURVE ( 'NONE', #74863, #65506, #37973, .T. ) ;
#3038 = ORIENTED_EDGE ( 'NONE', *, *, #37140, .T. ) ;
#3039 = VERTEX_POINT ( 'NONE', #78385 ) ;
#3040 = ORIENTED_EDGE ( 'NONE', *, *, #91556, .T. ) ;
#3041 = CARTESIAN_POINT ( 'NONE',  ( -47.57454933833918176, 12.59078750739570829, -14.43852527042941070 ) ) ;
#3042 = FILL_AREA_STYLE_COLOUR ( '', #61310 ) ;
#3043 = CARTESIAN_POINT ( 'NONE',  ( 3.313708498984722972, -15.21874999999999112, -8.000000000000040856 ) ) ;
#3044 = CARTESIAN_POINT ( 'NONE',  ( 43.00000000000000000, 436.5989882784185738, 19.94133085611158407 ) ) ;
#3045 = CARTESIAN_POINT ( 'NONE',  ( -31.35172730056181578, 439.1959017414955042, 22.91783259691881014 ) ) ;
#3046 = CARTESIAN_POINT ( 'NONE',  ( 0.000000000000000000, 4.898587196589412829E-16, -4.000000000000000000 ) ) ;
#3047 =( NAMED_UNIT ( * ) PLANE_ANGLE_UNIT ( ) SI_UNIT ( $, .RADIAN. ) );
#3048 = TOROIDAL_SURFACE ( 'NONE', #58084, 12.00000000000000000, 2.000000000000000000 ) ;
#3049 = ORIENTED_EDGE ( 'NONE', *, *, #70416, .F. ) ;
#3050 = CARTESIAN_POINT ( 'NONE',  ( 2.617478844991759868, 50.00000000000001421, -94.73972676610910071 ) ) ;
#3051 = VERTEX_POINT ( 'NONE', #79967 ) ;
#3052 = DIRECTION ( 'NONE',  ( 1.000000000000000000, 0.000000000000000000, 0.000000000000000000 ) ) ;
#3053 = CARTESIAN_POINT ( 'NONE',  ( 72.53904111559185708, -38.32615141910980583, 149.3261510640276697 ) ) ;
#3054 = CARTESIAN_POINT ( 'NONE',  ( 8.000000000000000000, -11.09375000409677092, -3.313708498984761164 ) ) ;
#3055 = CARTESIAN_POINT ( 'NONE',  ( 24.17704328875259634, 304.0406177940266730, 10.19684960573361465 ) ) ;
#3056 = CIRCLE ( 'NONE', #63352, 4.000000000000001776 ) ;
#3057 = DIRECTION ( 'NONE',  ( -1.000000000000000000, -1.224606353822377258E-16, -0.000000000000000000 ) ) ;
#3058 = CONICAL_SURFACE ( 'NONE', #106358, 3.309500000000001663, 0.9599310885968770357 ) ;
#3059 = ORIENTED_EDGE ( 'NONE', *, *, #40415, .T. ) ;
#3060 = DIRECTION ( 'NONE',  ( -0.000000000000000000, 1.000000000000000000, -0.000000000000000000 ) ) ;
#3061 = CARTESIAN_POINT ( 'NONE',  ( 16.96324018633373143, 45.77154698568147495, -4.157797401561765582 ) ) ;
#3062 = CARTESIAN_POINT ( 'NONE',  ( 38.00810289691445831, 309.9188390917963716, 5.520346969804636572 ) ) ;
#3063 = DIRECTION ( 'NONE',  ( 0.000000000000000000, -1.000000000000000000, 0.000000000000000000 ) ) ;
#3064 = EDGE_CURVE ( 'NONE', #75855, #27394, #51372, .T. ) ;
#3065 = VERTEX_POINT ( 'NONE', #63280 ) ;
#3067 =( LENGTH_UNIT ( ) NAMED_UNIT ( * ) SI_UNIT ( .MILLI., .METRE. ) );
#3066 =( LENGTH_UNIT ( ) NAMED_UNIT ( * ) SI_UNIT ( .MILLI., .METRE. ) );
#3068 = SURFACE_STYLE_USAGE ( .BOTH. , #76954 ) ;
#3069 = FACE_OUTER_BOUND ( 'NONE', #14383, .T. ) ;
#3070 = CONICAL_SURFACE ( 'NONE', #51231, 4.000000000000007105, 0.9599310885968835860 ) ;
#3072 = DIRECTION ( 'NONE',  ( 0.000000000000000000, 1.000000000000000000, 0.000000000000000000 ) ) ;
#3071 = CIRCLE ( 'NONE', #8219, 4.000000000000007105 ) ;
#3073 = EDGE_CURVE ( 'NONE', #12309, #49969, #66876, .T. ) ;
#3074 = CARTESIAN_POINT ( 'NONE',  ( 1.224646799147353454E-15, -78.00000000000000000, 17.00000000000000000 ) ) ;
#3075 = AXIS2_PLACEMENT_3D ( 'NONE', #29172, #80838, #63083 ) ;
#3076 = CARTESIAN_POINT ( 'NONE',  ( 5.619193549420741007, 4.261310591078456333, -5.875704392893664085 ) ) ;
#3077 = CARTESIAN_POINT ( 'NONE',  ( 86.23413113060379942, -28.25917168182434125, 183.4403566737863969 ) ) ;
#3078 =( LENGTH_UNIT ( ) NAMED_UNIT ( * ) SI_UNIT ( .MILLI., .METRE. ) );
#3079 = CARTESIAN_POINT ( 'NONE',  ( -8.813577900734397730, 133.4610148809356929, 4.999999999999998224 ) ) ;
#3080 = ORIENTED_EDGE ( 'NONE', *, *, #71874, .T. ) ;
#3081 = FACE_OUTER_BOUND ( 'NONE', #80474, .T. ) ;
#3082 = ADVANCED_FACE ( 'NONE', ( #47597 ), #47902, .T. ) ;
#3083 = CARTESIAN_POINT ( 'NONE',  ( 9.953686224012043837, -16.20368524395693655, -34.82632026490023236 ) ) ;
#3084 = CARTESIAN_POINT ( 'NONE',  ( 22.33349330513380337, 4.000000000000003553, 0.000000000000000000 ) ) ;
#3085 = CARTESIAN_POINT ( 'NONE',  ( 5.000000000000000888, -14.03284112334355704, 9.638321537241061776 ) ) ;
#3086 = AXIS2_PLACEMENT_3D ( 'NONE', #26285, #59146, #92560 ) ;
#3087 = CARTESIAN_POINT ( 'NONE',  ( -87.74588082317708881, -29.99999999999998934, 75.10738559680038406 ) ) ;
#3088 = CIRCLE ( 'NONE', #102955, 7.000000000000000000 ) ;
#3089 = FILL_AREA_STYLE_COLOUR ( '', #103653 ) ;
#3090 = CARTESIAN_POINT ( 'NONE',  ( 0.009260245579808886948, -57.67120202535643614, 41.61186695095138788 ) ) ;
#3092 = CARTESIAN_POINT ( 'NONE',  ( 0.000000000000000000, 0.000000000000000000, 0.000000000000000000 ) ) ;
#3091 = CARTESIAN_POINT ( 'NONE',  ( -9.797537890442951536, 246.5344220233380099, 2.014215961808872635 ) ) ;
#3093 = B_SPLINE_CURVE_WITH_KNOTS ( 'NONE', 3,
 ( #66354, #9700, #41552, #50678 ),
 .UNSPECIFIED., .F., .F.,
 ( 4, 4 ),
 ( 2.168404344971008868E-19, 0.002009015923125643047 ),
 .UNSPECIFIED. ) ;
#3094 = AXIS2_PLACEMENT_3D ( 'NONE', #80471, #7116, #97192 ) ;
#3095 = CARTESIAN_POINT ( 'NONE',  ( 4.371444047847319325, -52.53631654761795033, 40.30117609609928309 ) ) ;
#3096 = DIRECTION ( 'NONE',  ( -1.000000000000000000, -0.000000000000000000, -0.000000000000000000 ) ) ;
#3097 = CARTESIAN_POINT ( 'NONE',  ( -46.00000000000000000, 450.0000000000002274, 13.20242257375370976 ) ) ;
#3098 = CARTESIAN_POINT ( 'NONE',  ( -9.151133496029540737, 15.07443463110275417, 4.034557488804506598 ) ) ;
#3099 = CARTESIAN_POINT ( 'NONE',  ( 5.000000000000000000, 6.123233995736766282E-16, -2.868028571428571372 ) ) ;
#3101 = EDGE_CURVE ( 'NONE', #43916, #92807, #26758, .T. ) ;
#3100 = CARTESIAN_POINT ( 'NONE',  ( 56.00069051983414425, -28.66156656293939875, -26.27684122581554860 ) ) ;
#3102 = CIRCLE ( 'NONE', #63417, 4.000000000000001776 ) ;
#3103 = CARTESIAN_POINT ( 'NONE',  ( -25.83922611890834986, -32.52481888390300924, 30.74902383434352515 ) ) ;
#3104 = VERTEX_POINT ( 'NONE', #48653 ) ;
#3105 = FACE_OUTER_BOUND ( 'NONE', #16111, .T. ) ;
#3106 = CARTESIAN_POINT ( 'NONE',  ( -16.37657220773485989, -18.58804370566180353, 27.19384971940823448 ) ) ;
#3108 = CARTESIAN_POINT ( 'NONE',  ( -17.49999999999997513, 45.00000000000000711, -500000.0000000000582 ) ) ;
#3107 = CARTESIAN_POINT ( 'NONE',  ( 43.41290683822506935, 487.0833545439620593, 7.569976829064905210 ) ) ;
#3109 = EDGE_CURVE ( 'NONE', #6957, #89827, #80638, .T. ) ;
#3110 = EDGE_LOOP ( 'NONE', ( #13685, #43062, #36659, #66962 ) ) ;
#3111 = AXIS2_PLACEMENT_3D ( 'NONE', #63741, #63204, #39464 ) ;
#3112 = CARTESIAN_POINT ( 'NONE',  ( 6.172076129340175576, 1.395179846525673950, -6.500000000000603073 ) ) ;
#3113 = EDGE_LOOP ( 'NONE', ( #74997, #77625, #9958, #10789, #7746 ) ) ;
#3114 = CARTESIAN_POINT ( 'NONE',  ( 9.289992159469221633, 50.00000000000000711, -94.32837231712201742 ) ) ;
#3115 = EDGE_CURVE ( 'NONE', #80889, #83253, #65394, .T. ) ;
#3116 = VECTOR ( 'NONE', #106742, 1000.000000000000000 ) ;
#3117 = CARTESIAN_POINT ( 'NONE',  ( 0.000000000000000000, 0.000000000000000000, 4.000000000000000000 ) ) ;
#3118 = LINE ( 'NONE', #61370, #54375 ) ;
#3119 = VERTEX_POINT ( 'NONE', #49729 ) ;
#3120 =( NAMED_UNIT ( * ) PLANE_ANGLE_UNIT ( ) SI_UNIT ( $, .RADIAN. ) );
#3121 = CARTESIAN_POINT ( 'NONE',  ( 11.84999999999999787, 3.309500000000003439, 4.052968581778167743E-16 ) ) ;
#3122 = CARTESIAN_POINT ( 'NONE',  ( 100.8769579830505592, -45.28053191621518891, 191.5263513813913789 ) ) ;
#3123 = AXIS2_PLACEMENT_3D ( 'NONE', #15592, #80854, #23720 ) ;
#3125 = CARTESIAN_POINT ( 'NONE',  ( 35.11650669486618170, -3.999999999999998224, 0.000000000000000000 ) ) ;
#3124 = SURFACE_SIDE_STYLE ('',( #77006 ) ) ;
#3126 = MECHANICAL_DESIGN_GEOMETRIC_PRESENTATION_REPRESENTATION (  '', ( #99502 ), #8270 ) ;
#3127 = EDGE_LOOP ( 'NONE', ( #69501, #44962, #48378, #27285 ) ) ;
#3128 = VERTEX_POINT ( 'NONE', #34124 ) ;
#3129 = EDGE_LOOP ( 'NONE', ( #93239, #96111, #27042, #10278 ) ) ;
#3130 = CARTESIAN_POINT ( 'NONE',  ( 27.76828805976974834, 314.2092757663235147, 11.21267187466577298 ) ) ;
#3131 = DIRECTION ( 'NONE',  ( -1.000000000000000000, -1.224606353822377258E-16, -0.000000000000000000 ) ) ;
#3132 = DIRECTION ( 'NONE',  ( 1.000000000000000000, 1.224606353822377258E-16, 0.000000000000000000 ) ) ;
#3133 = EDGE_LOOP ( 'NONE', ( #99013, #9219, #4853, #12269 ) ) ;
#3134 = EDGE_CURVE ( 'NONE', #60462, #54541, #14912, .T. ) ;
#3135 = DIRECTION ( 'NONE',  ( -1.000000000000000000, -1.224606353822377258E-16, -0.000000000000000000 ) ) ;
#3136 = CARTESIAN_POINT ( 'NONE',  ( -6.528714966258958974, 41.70354536991147398, -70.35321464783143597 ) ) ;
#3137 = B_SPLINE_CURVE_WITH_KNOTS ( 'NONE', 3,
 ( #4700, #21434, #87746, #103389 ),
 .UNSPECIFIED., .F., .F.,
 ( 4, 4 ),
 ( 0.000000000000000000, 0.001872901900679948758 ),
 .UNSPECIFIED. ) ;
#3138 = CARTESIAN_POINT ( 'NONE',  ( -47.54236909243191889, -59.99999999996124700, -40.79170333304822549 ) ) ;
#3139 = CARTESIAN_POINT ( 'NONE',  ( 0.000000000000000000, 0.000000000000000000, 4.000000000000000000 ) ) ;
#3140 = AXIS2_PLACEMENT_3D ( 'NONE', #79796, #80849, #64683 ) ;
#3141 = CARTESIAN_POINT ( 'NONE',  ( -31.21933008645656926, 405.2090764464551853, 25.56980379099173817 ) ) ;
#3142 = CIRCLE ( 'NONE', #22098, 6.500000000000000000 ) ;
#3143 = DIRECTION ( 'NONE',  ( 0.000000000000000000, -1.000000000000000000, 0.000000000000000000 ) ) ;
#3144 = PRESENTATION_LAYER_ASSIGNMENT (  '', '', ( #18647 ) ) ;
#3145 = CARTESIAN_POINT ( 'NONE',  ( -95.02173393737120932, -60.00000000000007105, -3.234914688897275070 ) ) ;
#3146 = CARTESIAN_POINT ( 'NONE',  ( 36.08349330513379982, 4.000000000000003553, 0.000000000000000000 ) ) ;
#3147 = CARTESIAN_POINT ( 'NONE',  ( -47.88475624650544660, -56.82326849868364604, 52.80298889764087278 ) ) ;
#3148 = ORIENTED_EDGE ( 'NONE', *, *, #34199, .F. ) ;
#3149 = FACE_OUTER_BOUND ( 'NONE', #71581, .T. ) ;
#3150 = ORIENTED_EDGE ( 'NONE', *, *, #81419, .T. ) ;
#3151 = CARTESIAN_POINT ( 'NONE',  ( 0.000000000000000000, 6.123233995736770227E-16, -5.000000000000002665 ) ) ;
#3152 = VECTOR ( 'NONE', #87057, 1000.000000000000000 ) ;
#3153 = CARTESIAN_POINT ( 'NONE',  ( -9.720388148956621066, 294.7585724938156773, -10.04291177946082314 ) ) ;
#3154 = CARTESIAN_POINT ( 'NONE',  ( 8.929771841637641927, 5.000000000000003553, 0.000000000000000000 ) ) ;
#3155 = ORIENTED_EDGE ( 'NONE', *, *, #80792, .F. ) ;
#3156 = FILL_AREA_STYLE ('',( #42538 ) ) ;
#3157 = ORIENTED_EDGE ( 'NONE', *, *, #98683, .F. ) ;
#3158 = CARTESIAN_POINT ( 'NONE',  ( 90.08055447028598905, -30.00000000002782841, -8.126024404956387670 ) ) ;
#3159 = CARTESIAN_POINT ( 'NONE',  ( 3.352941176470587870, -48.79941684889504927, 104.5794940929807524 ) ) ;
#3160 = CARTESIAN_POINT ( 'NONE',  ( -5.000000000000000000, -15.93202192939577344, -5.930487099830192399 ) ) ;
#3161 = CARTESIAN_POINT ( 'NONE',  ( 7.754160006507071046, 42.00000000000000711, -59.23741894013591036 ) ) ;
#3162 = CARTESIAN_POINT ( 'NONE',  ( 89.34851512668548423, -30.00000000000000355, 189.1863861107025286 ) ) ;
#3163 = CARTESIAN_POINT ( 'NONE',  ( -11.53040807487433739, 43.41108915750923813, -13.95613592774078882 ) ) ;
#3164 = CARTESIAN_POINT ( 'NONE',  ( -1.219175067079236729, 36.86153658035306080, 28.18154403026957766 ) ) ;
#3165 = STYLED_ITEM ( 'NONE', ( #87753 ), #44467 ) ;
#3166 = ORIENTED_EDGE ( 'NONE', *, *, #43628, .F. ) ;
#3167 = VERTEX_POINT ( 'NONE', #83167 ) ;
#3168 = CARTESIAN_POINT ( 'NONE',  ( 54.15937250249886148, -32.56281511288196384, 55.81529859889931089 ) ) ;
#3169 = CARTESIAN_POINT ( 'NONE',  ( 0.000000000000000000, 0.000000000000000000, -7.424942857142857733 ) ) ;
#3170 = CARTESIAN_POINT ( 'NONE',  ( -43.51882896341776075, 485.1238987962696001, -1.698943142573396292 ) ) ;
#3171 = EDGE_LOOP ( 'NONE', ( #74284, #98708, #71481, #35631, #68430 ) ) ;
#3172 = CARTESIAN_POINT ( 'NONE',  ( -91.47181070595220831, -38.38037305410311717, -6.014377416796397924 ) ) ;
#3173 = CIRCLE ( 'NONE', #29101, 10.02537308446410869 ) ;
#3174 = ORIENTED_EDGE ( 'NONE', *, *, #9014, .F. ) ;
#3175 = DIRECTION ( 'NONE',  ( 0.000000000000000000, 0.8047643452607258219, -0.5935944310697964799 ) ) ;
#3176 = CARTESIAN_POINT ( 'NONE',  ( 108.3599484846729695, -38.35745757732994576, 191.9951766408777019 ) ) ;
#3177 = CARTESIAN_POINT ( 'NONE',  ( 12.35931481849550195, 17.95192587946648288, 8.704851652794047823 ) ) ;
#3178 = CARTESIAN_POINT ( 'NONE',  ( 85.12609559102118340, -52.70885996367997706, 4.505813679903315716 ) ) ;
#3179 = CARTESIAN_POINT ( 'NONE',  ( 32.57720510843783757, 345.4073167506460891, 19.87011376397160944 ) ) ;
#3180 = DIRECTION ( 'NONE',  ( -1.000000000000000000, -1.224606353822377258E-16, -0.000000000000000000 ) ) ;
#3181 = CARTESIAN_POINT ( 'NONE',  ( 26.36650669486618881, 1.474610560812782335E-15, 0.000000000000000000 ) ) ;
#3182 =( REPRESENTATION_RELATIONSHIP ('NONE','NONE', #69581, #19231 ) REPRESENTATION_RELATIONSHIP_WITH_TRANSFORMATION ( #83204 )SHAPE_REPRESENTATION_RELATIONSHIP( ) );
#3183 = AXIS2_PLACEMENT_3D ( 'NONE', #25997, #76609, #17337 ) ;
#3184 = CARTESIAN_POINT ( 'NONE',  ( -23.54609178594817820, 25.19604284925236470, -33.16510347394218172 ) ) ;
#3185 = CARTESIAN_POINT ( 'NONE',  ( 0.000000000000000000, 0.000000000000000000, 0.000000000000000000 ) ) ;
#3186 = CARTESIAN_POINT ( 'NONE',  ( 7.869427812662803667, 64.69537499113458523, -2.456618345357718155E-12 ) ) ;
#3187 = VERTEX_POINT ( 'NONE', #56745 ) ;
#3188 = DIRECTION ( 'NONE',  ( -0.000000000000000000, -0.000000000000000000, -1.000000000000000000 ) ) ;
#3189 = ADVANCED_FACE ( 'NONE', ( #83 ), #68378, .T. ) ;
#3190 = CARTESIAN_POINT ( 'NONE',  ( 7.121430446328069763, 40.29466766088835072, -71.00332351279642751 ) ) ;
#3191 = DIRECTION ( 'NONE',  ( -1.000000000000000000, -0.000000000000000000, -0.000000000000000000 ) ) ;
#3192 = VERTEX_POINT ( 'NONE', #64856 ) ;
#3193 = EDGE_CURVE ( 'NONE', #22140, #5765, #43423, .T. ) ;
#3194 = CARTESIAN_POINT ( 'NONE',  ( -24.89134784884370433, 306.1294686800183058, -8.721742491190038749 ) ) ;
#3195 = CIRCLE ( 'NONE', #103061, 2.000000000000000444 ) ;
#3196 = CARTESIAN_POINT ( 'NONE',  ( -34.06266673247649379, 303.3474602219233702, 11.90248453523486560 ) ) ;
#3197 = DIRECTION ( 'NONE',  ( 1.000000000000000000, 0.000000000000000000, 0.000000000000000000 ) ) ;
#3198 = DIRECTION ( 'NONE',  ( -1.000000000000000000, -0.000000000000000000, -0.000000000000000000 ) ) ;
#3199 = CARTESIAN_POINT ( 'NONE',  ( -8.000000000000000000, -22.34374999999999289, -3.313708498984762496 ) ) ;
#3200 = CARTESIAN_POINT ( 'NONE',  ( 16.05552553557446060, -15.52039114152552735, 31.56705366141566316 ) ) ;
#3201 = MECHANICAL_DESIGN_GEOMETRIC_PRESENTATION_REPRESENTATION (  '', ( #101367 ), #18705 ) ;
#3202 = EDGE_CURVE ( 'NONE', #48016, #62320, #98709, .T. ) ;
#3203 = DIRECTION ( 'NONE',  ( -1.000000000000000000, -0.000000000000000000, -0.000000000000000000 ) ) ;
#3204 = AXIS2_PLACEMENT_3D ( 'NONE', #26924, #3679, #77022 ) ;
#3205 = ORIENTED_EDGE ( 'NONE', *, *, #2312, .T. ) ;
#3206 = CARTESIAN_POINT ( 'NONE',  ( 83.88774053950423593, -50.14893828415973331, 186.5792076936381534 ) ) ;
#3207 = CARTESIAN_POINT ( 'NONE',  ( -37.56673239365849781, 27.88554838446201600, 10.95617127781066102 ) ) ;
#3208 = VECTOR ( 'NONE', #49503, 1000.000000000000000 ) ;
#3209 = CARTESIAN_POINT ( 'NONE',  ( -15.88102029263269444, 46.13028405480689997, 4.403441971141869971 ) ) ;
#3210 = EDGE_LOOP ( 'NONE', ( #10478, #57298, #37512, #1546 ) ) ;
#3211 = CARTESIAN_POINT ( 'NONE',  ( -88.45092629199805856, -52.70969016536442098, 52.48989280492887843 ) ) ;
#3212 = EDGE_CURVE ( 'NONE', #90932, #42388, #39046, .T. ) ;
#3213 = DIRECTION ( 'NONE',  ( -0.000000000000000000, -1.000000000000000000, -0.000000000000000000 ) ) ;
#3214 = DIRECTION ( 'NONE',  ( 0.000000000000000000, 0.000000000000000000, 1.000000000000000000 ) ) ;
#3215 = CARTESIAN_POINT ( 'NONE',  ( 15.04647843581836497, -3.000000000000002665, -85.64811627162752927 ) ) ;
#3216 = CARTESIAN_POINT ( 'NONE',  ( -23.57853350939547354, -27.17268373882357224, -38.41116532901637726 ) ) ;
#3217 = CARTESIAN_POINT ( 'NONE',  ( 23.81365055911821216, -60.00000000000000000, 40.86761593640069634 ) ) ;
#3218 = CARTESIAN_POINT ( 'NONE',  ( 35.44951030812982395, -35.74875123850512892, 44.64175081870536133 ) ) ;
#3219 =( GEOMETRIC_REPRESENTATION_CONTEXT ( 3 ) GLOBAL_UNCERTAINTY_ASSIGNED_CONTEXT ( ( #23648 ) ) GLOBAL_UNIT_ASSIGNED_CONTEXT ( ( #10926, #85379, #51401 ) ) REPRESENTATION_CONTEXT ( 'NONE', 'WORKASPACE' ) );
#3220 = CARTESIAN_POINT ( 'NONE',  ( 1.276500347575403982, -1.740950606958863416E-15, 101.3106844269255760 ) ) ;
#3221 = CARTESIAN_POINT ( 'NONE',  ( 45.12508949386340618, -28.33865188907569532, 40.20852945013428581 ) ) ;
#3222 = CONICAL_SURFACE ( 'NONE', #92754, 5.000000000000000000, 0.9599310885968913576 ) ;
#3224 = CARTESIAN_POINT ( 'NONE',  ( -11.22818708771012375, 17.69611070818088905, 8.853064228155091087 ) ) ;
#3223 = CARTESIAN_POINT ( 'NONE',  ( 33.89780391220055833, 435.9360085663053042, 7.958081226251983331 ) ) ;
#3225 = CARTESIAN_POINT ( 'NONE',  ( 5.800920608168121717, 296.2164713808183478, -10.01425861749307700 ) ) ;
#3226 = CARTESIAN_POINT ( 'NONE',  ( 33.56345473223404241, 299.9083031499212666, -8.874823776838020706 ) ) ;
#3227 = CARTESIAN_POINT ( 'NONE',  ( 43.28639662975297853, 353.0009670098160086, 11.32799993555481954 ) ) ;
#3228 = LINE ( 'NONE', #85759, #94927 ) ;
#3229 = ORIENTED_EDGE ( 'NONE', *, *, #89579, .T. ) ;
#3230 = CARTESIAN_POINT ( 'NONE',  ( 4.366061277241470862, -4.984806845751398541, -0.09463688534108255501 ) ) ;
#3231 = CARTESIAN_POINT ( 'NONE',  ( 8.099999999999999645, 3.752776749732561257, -6.499999999999999112 ) ) ;
#3232 = ORIENTED_EDGE ( 'NONE', *, *, #82323, .F. ) ;
#3233 = LINE ( 'NONE', #37226, #100467 ) ;
#3235 = CARTESIAN_POINT ( 'NONE',  ( -18.94239008060200291, -34.58964377142442004, -31.89223463875953613 ) ) ;
#3234 = CARTESIAN_POINT ( 'NONE',  ( 9.380871178326138704, 252.0111637979832153, 3.467392232194206780 ) ) ;
#3236 = EDGE_CURVE ( 'NONE', #2115, #35969, #58908, .T. ) ;
#3237 = ORIENTED_EDGE ( 'NONE', *, *, #21665, .T. ) ;
#3238 = AXIS2_PLACEMENT_3D ( 'NONE', #63747, #45439, #88543 ) ;
#3239 = DIRECTION ( 'NONE',  ( 0.000000000000000000, 0.000000000000000000, 1.000000000000000000 ) ) ;
#3240 = CARTESIAN_POINT ( 'NONE',  ( 5.007715329123895321E-16, -7.505553499465175804, -6.064240316920414209 ) ) ;
#3241 = AXIS2_PLACEMENT_3D ( 'NONE', #100713, #26877, #100187 ) ;
#3242 = ORIENTED_EDGE ( 'NONE', *, *, #38802, .T. ) ;
#3243 = ADVANCED_FACE ( 'NONE', ( #51852 ), #97601, .T. ) ;
#3244 = CARTESIAN_POINT ( 'NONE',  ( 101.2019940638598854, -5.000000000000000888, 6.123233995736779101E-16 ) ) ;
#3245 = VECTOR ( 'NONE', #95115, 1000.000000000000000 ) ;
#3246 = CARTESIAN_POINT ( 'NONE',  ( 29.68315524076959377, 13.12249633091058243, -39.60535821593525441 ) ) ;
#3247 = VECTOR ( 'NONE', #91322, 1000.000000000000000 ) ;
#3248 = CARTESIAN_POINT ( 'NONE',  ( 65.03872891708842019, 6.856755485862130937E-15, 0.000000000000000000 ) ) ;
#3249 = CARTESIAN_POINT ( 'NONE',  ( -93.42203525153540511, -59.99999999999998579, 36.32810924189196555 ) ) ;
#3250 = CARTESIAN_POINT ( 'NONE',  ( 37.38561277374697056, 6.123233995736770227E-16, -5.000000000000002665 ) ) ;
#3251 = CARTESIAN_POINT ( 'NONE',  ( 4.898587196589412829E-16, -12.12499999999999289, -8.000000000000000000 ) ) ;
#3252 = DIRECTION ( 'NONE',  ( 0.000000000000000000, 1.000000000000000000, 0.000000000000000000 ) ) ;
#3254 = CYLINDRICAL_SURFACE ( 'NONE', #78822, 1.250000000000001110 ) ;
#3253 = CARTESIAN_POINT ( 'NONE',  ( -34.89791961505246576, 436.0442787761182899, 7.592671863475971783 ) ) ;
#3255 = AXIS2_PLACEMENT_3D ( 'NONE', #62065, #21089, #28642 ) ;
#3256 = CARTESIAN_POINT ( 'NONE',  ( -83.91177200283225091, -32.50788753430207834, 167.3447669332486214 ) ) ;
#3257 = VERTEX_POINT ( 'NONE', #76129 ) ;
#3258 = CARTESIAN_POINT ( 'NONE',  ( 6.642722263319527087, 41.46658730130243953, -70.60825968728163105 ) ) ;
#3259 = EDGE_LOOP ( 'NONE', ( #50709, #49256, #100260, #36531, #1388, #54276 ) ) ;
#3260 = VERTEX_POINT ( 'NONE', #46300 ) ;
#3261 = CARTESIAN_POINT ( 'NONE',  ( -4.324717655747483569, -1.111686313677800131, 104.4045892612656417 ) ) ;
#3263 =( BOUNDED_SURFACE ( )  B_SPLINE_SURFACE ( 3, 2, ( 
 ( #42064, #66341, #8634 ),
 ( #33468, #2120, #92200 ),
 ( #74950, #34014, #25941 ),
 ( #1588, #25391, #42594 ) ),
 .UNSPECIFIED., .F., .F., .T. ) 
 B_SPLINE_SURFACE_WITH_KNOTS ( ( 4, 4 ),
 ( 3, 3 ),
 ( 0.000000000000000000, 0.001940382064934518527 ),
 ( 0.000000000000000000, 1.000000000000000000 ),
 .UNSPECIFIED. ) 
 GEOMETRIC_REPRESENTATION_ITEM ( )  RATIONAL_B_SPLINE_SURFACE ( (
 ( 1.000000000000000000, 0.8014084173415135792, 1.000000000000000000),
 ( 1.000000000000000000, 0.8101072955757671057, 1.000000000000000000),
 ( 1.000000000000000000, 0.8191355677487397458, 1.000000000000000000),
 ( 1.000000000000000000, 0.8274249441182489617, 1.000000000000000000) ) ) 
 REPRESENTATION_ITEM ( '' )  SURFACE ( )  );
#3262 = CARTESIAN_POINT ( 'NONE',  ( 17.55833715088428093, -4.999999999999999112, -1.075502477178110317 ) ) ;
#3264 = DIRECTION ( 'NONE',  ( -1.000000000000000000, -1.224606353822377258E-16, -0.000000000000000000 ) ) ;
#3265 = EDGE_LOOP ( 'NONE', ( #22993, #29012, #78146, #84988 ) ) ;
#3266 = EDGE_CURVE ( 'NONE', #82529, #31918, #34401, .T. ) ;
#3267 = CARTESIAN_POINT ( 'NONE',  ( -80.00483118099813851, -57.67118036264142944, -30.22182926596574148 ) ) ;
#3268 = CARTESIAN_POINT ( 'NONE',  ( -5.647817967127097383, -68.45126406528792984, -2.038183545141174058 ) ) ;
#3269 = VECTOR ( 'NONE', #29765, 1000.000000000000000 ) ;
#3270 = DIRECTION ( 'NONE',  ( 0.000000000000000000, 0.000000000000000000, 1.000000000000000000 ) ) ;
#3271 = CARTESIAN_POINT ( 'NONE',  ( 23.38216085046638781, 27.34669553923654561, 33.20617127781017786 ) ) ;
#3272 = CARTESIAN_POINT ( 'NONE',  ( 36.08349330513379982, 1.593028355512270962E-15, 0.000000000000000000 ) ) ;
#3273 = CARTESIAN_POINT ( 'NONE',  ( -17.83066785977178625, 36.70615155823221443, -22.40577935710505386 ) ) ;
#3274 = CARTESIAN_POINT ( 'NONE',  ( 94.62301060094824834, -14.21045842199438525, 80.84833697736402769 ) ) ;
#3275 = EDGE_CURVE ( 'NONE', #84222, #25443, #53646, .T. ) ;
#3276 = CARTESIAN_POINT ( 'NONE',  ( -77.72307990868957006, -60.00000000000013500, 197.5629538559897469 ) ) ;
#3277 = CARTESIAN_POINT ( 'NONE',  ( -54.36348728659673668, -49.91102849765379545, 63.10952282595231821 ) ) ;
#3278 = ORIENTED_EDGE ( 'NONE', *, *, #32936, .F. ) ;
#3279 = CARTESIAN_POINT ( 'NONE',  ( 6.984140731825568160, 16.97242079111239832, 0.5385323539060852260 ) ) ;
#3280 = ORIENTED_EDGE ( 'NONE', *, *, #13425, .F. ) ;
#3281 = CARTESIAN_POINT ( 'NONE',  ( -102.8828697075181680, -52.71162264969420619, 190.2909648261160953 ) ) ;
#3282 = ADVANCED_FACE ( 'NONE', ( #9791 ), #49405, .T. ) ;
#3283 = CARTESIAN_POINT ( 'NONE',  ( 31.84999999999999787, 3.309500000000003439, 4.052968581778167743E-16 ) ) ;
#3284 = ORIENTED_EDGE ( 'NONE', *, *, #105138, .F. ) ;
#3285 = CARTESIAN_POINT ( 'NONE',  ( -22.53767922124185574, -59.99999999999998579, 40.61082087230103355 ) ) ;
#3286 = CARTESIAN_POINT ( 'NONE',  ( -1.226488475359366337, -0.004841394705047758623, 101.2642676850169892 ) ) ;
#3287 = CARTESIAN_POINT ( 'NONE',  ( -5.082755093536326818, -15.59375000204838635, 5.082755093536325042 ) ) ;
#3288 = CARTESIAN_POINT ( 'NONE',  ( -1.099010308150110360, 36.97177997581172804, -27.88336368392158349 ) ) ;
#3289 = CARTESIAN_POINT ( 'NONE',  ( 7.002641335706725201, -83.94912737319167206, 3.868676264653294172 ) ) ;
#3290 = CARTESIAN_POINT ( 'NONE',  ( -31.21933008645656926, 405.2090764464551853, 25.56980379099173817 ) ) ;
#3291 = SURFACE_STYLE_USAGE ( .BOTH. , #28664 ) ;
#3292 = CARTESIAN_POINT ( 'NONE',  ( -8.182558299557642911, 38.50572386936678271, -0.000000000000000000 ) ) ;
#3293 = CARTESIAN_POINT ( 'NONE',  ( -5.656854249492381470, -14.75000000409677092, 5.656854249492379694 ) ) ;
#3294 = CARTESIAN_POINT ( 'NONE',  ( -5.365535441410388628, 42.28877518162276061, -59.25308630239388208 ) ) ;
#3295 = CARTESIAN_POINT ( 'NONE',  ( -30.66975189450997163, -32.54514858898122043, 32.11485851461230112 ) ) ;
#3296 = DIRECTION ( 'NONE',  ( -1.000000000000000000, -0.000000000000000000, 0.000000000000000000 ) ) ;
#3297 = CARTESIAN_POINT ( 'NONE',  ( 47.71926515674179115, -36.06417799759196186, 46.18337568543712734 ) ) ;
#3298 = CARTESIAN_POINT ( 'NONE',  ( -32.94539137533585205, 488.0149952105291504, 9.145905951731968742 ) ) ;
#3299 = CARTESIAN_POINT ( 'NONE',  ( 7.322849800245818663, 11.36060796471277889, 7.896605822936082213E-15 ) ) ;
#3300 = B_SPLINE_CURVE_WITH_KNOTS ( 'NONE', 3,
 ( #3988, #13649, #4510, #36400, #86524, #69266 ),
 .UNSPECIFIED., .F., .F.,
 ( 4, 2, 4 ),
 ( 0.000000000000000000, 0.0003491763592121695367, 0.0006983527184243390733 ),
 .UNSPECIFIED. ) ;
#3301 = CARTESIAN_POINT ( 'NONE',  ( -85.95206158600240087, -38.64469160019880434, 199.0332504256811603 ) ) ;
#3302 = ORIENTED_EDGE ( 'NONE', *, *, #4195, .T. ) ;
#3304 = CARTESIAN_POINT ( 'NONE',  ( -42.37751841893185656, 435.9440627571721620, 7.948837343527475063 ) ) ;
#3303 = CARTESIAN_POINT ( 'NONE',  ( 84.58395683528345899, -38.35848370293111032, -23.21156260195221677 ) ) ;
#3305 = CARTESIAN_POINT ( 'NONE',  ( -18.97587827957842066, 49.43159474368409434, 61.96476824398673955 ) ) ;
#3306 = CARTESIAN_POINT ( 'NONE',  ( 41.70256300459684695, 461.0340457114389778, 3.032228049028138361 ) ) ;
#3307 = VECTOR ( 'NONE', #30858, 1000.000000000000227 ) ;
#3308 = CARTESIAN_POINT ( 'NONE',  ( 6.870942159525867510, 40.00000000392758182, -71.15487301629636363 ) ) ;
#3309 = CARTESIAN_POINT ( 'NONE',  ( 0.000000000000000000, 50.50000000000000000, 0.000000000000000000 ) ) ;
#3310 = CARTESIAN_POINT ( 'NONE',  ( 5.000000000000000888, -57.08339339093014786, 10.85455184355725144 ) ) ;
#3311 = CARTESIAN_POINT ( 'NONE',  ( 27.61650669486618881, 4.000000000000003553, 4.898587196589414801E-16 ) ) ;
#3312 = CARTESIAN_POINT ( 'NONE',  ( 106.5873745654861580, -59.99999999999999289, 197.6168797630004406 ) ) ;
#3313 = CARTESIAN_POINT ( 'NONE',  ( -7.212408192734265810, -67.01517089320368825, -3.465038817813883121 ) ) ;
#3314 = ORIENTED_EDGE ( 'NONE', *, *, #41239, .T. ) ;
#3315 = CARTESIAN_POINT ( 'NONE',  ( 36.59842210978576560, 438.2481675559515111, 3.880703544898916224 ) ) ;
#3316 = ADVANCED_FACE ( 'NONE', ( #59984 ), #71296, .F. ) ;
#3317 = AXIS2_PLACEMENT_3D ( 'NONE', #18814, #17717, #2041 ) ;
#3318 = CARTESIAN_POINT ( 'NONE',  ( -80.60042778259895613, -30.00000000000000711, -12.84585300385902684 ) ) ;
#3319 = ORIENTED_EDGE ( 'NONE', *, *, #17107, .T. ) ;
#3321 = CARTESIAN_POINT ( 'NONE',  ( 5.293250127137346439, 18.43355203274099807, -37.80931412032270345 ) ) ;
#3320 = CARTESIAN_POINT ( 'NONE',  ( -85.21905093902094563, -38.68651908961214758, 198.6209921461202725 ) ) ;
#3322 = CARTESIAN_POINT ( 'NONE',  ( 46.00000000000000711, 438.0945115977546038, 11.27406305469638070 ) ) ;
#3323 = CARTESIAN_POINT ( 'NONE',  ( 6.162888688655344893, -3.752776749732565253, 6.499999999999999112 ) ) ;
#3324 = CARTESIAN_POINT ( 'NONE',  ( -33.00000000000000000, 489.5971041675261404, 10.80646835458718868 ) ) ;
#3325 = CARTESIAN_POINT ( 'NONE',  ( -1.320432766682874540E-15, -10.90625000204838457, 7.188101187500000044 ) ) ;
#3326 = CARTESIAN_POINT ( 'NONE',  ( 0.000000000000000000, -5.000000000000002665, -73.00000000000001421 ) ) ;
#3327 = EDGE_CURVE ( 'NONE', #81483, #89014, #70580, .T. ) ;
#3328 = AXIS2_PLACEMENT_3D ( 'NONE', #35715, #50768, #83679 ) ;
#3329 = EDGE_CURVE ( 'NONE', #8093, #72947, #61975, .T. ) ;
#3330 = ADVANCED_FACE ( 'NONE', ( #103467 ), #29616, .T. ) ;
#3331 = CARTESIAN_POINT ( 'NONE',  ( 29.99961410214308799, 17.76511157208309655, -39.64372791628649395 ) ) ;
#3333 = VERTEX_POINT ( 'NONE', #103987 ) ;
#3332 = DIRECTION ( 'NONE',  ( -1.000000000000000000, -1.224606353822377258E-16, -0.000000000000000000 ) ) ;
#3334 = CARTESIAN_POINT ( 'NONE',  ( 85.11568698743305106, -25.45901852875848093, 167.9889055482516369 ) ) ;
#3335 = EDGE_CURVE ( 'NONE', #21469, #9002, #30130, .T. ) ;
#3336 = CARTESIAN_POINT ( 'NONE',  ( -43.65587342670181670, 462.3497007921330351, 4.817139433394860504 ) ) ;
#3338 = EDGE_CURVE ( 'NONE', #14833, #87241, #63216, .T. ) ;
#3337 = CARTESIAN_POINT ( 'NONE',  ( 2.837346585668846011, -6.232092946297409952, -6.171287963165208446 ) ) ;
#3339 = ORIENTED_EDGE ( 'NONE', *, *, #64113, .T. ) ;
#3340 = FACE_OUTER_BOUND ( 'NONE', #26445, .T. ) ;
#3341 = EDGE_CURVE ( 'NONE', #52131, #63286, #42708, .T. ) ;
#3342 = CARTESIAN_POINT ( 'NONE',  ( 16.75187969033571989, 34.99134772383131065, 21.80698433968582961 ) ) ;
#3343 = CARTESIAN_POINT ( 'NONE',  ( 0.000000000000000000, 0.000000000000000000, 4.000000000000000000 ) ) ;
#3344 = DIRECTION ( 'NONE',  ( 1.000000000000000000, 0.000000000000000000, 0.000000000000000000 ) ) ;
#3345 = CARTESIAN_POINT ( 'NONE',  ( -4.496882872040836254, 250.5378866548961696, 3.972797206970395845 ) ) ;
#3346 = CARTESIAN_POINT ( 'NONE',  ( 0.1553986885509386628, 12.93312546826206777, 51.74235877965696062 ) ) ;
#3347 = B_SPLINE_SURFACE_WITH_KNOTS ( 'NONE', 3, 1, ( 
 ( #38181, #80180, #58983 ),
 ( #42245, #91871, #105006 ),
 ( #31148, #55369, #14374 ),
 ( #72626, #88817, #15990 ),
 ( #88299, #32191, #65070 ),
 ( #97419, #6287, #56426 ),
 ( #31668, #30609, #40262 ),
 ( #75135, #23046, #23580 ),
 ( #22526, #48868, #55882 ),
 ( #39224, #1231, #48340 ),
 ( #38690, #72099, #81760 ),
 ( #106040, #47805, #34201 ),
 ( #80708, #89359, #9335 ),
 ( #79659, #71556, #6826 ),
 ( #73136, #39745, #46763 ),
 ( #81235, #97968, #67073 ),
 ( #63498, #24118, #96396 ),
 ( #26129, #18536, #100485 ),
 ( #44934, #44389, #69208 ),
 ( #68678, #19089, #67606 ),
 ( #75678, #26643, #52460 ),
 ( #85931, #28778, #12001 ),
 ( #93478, #28238, #60589 ),
 ( #101019, #102076, #84842 ),
 ( #59516, #1777, #11462 ),
 ( #92925, #36338, #84312 ),
 ( #77818, #51400, #92389 ),
 ( #10409, #61659, #34735 ),
 ( #17997, #76205, #43323 ),
 ( #2309, #35256, #101558 ),
 ( #60065, #61109, #19627 ),
 ( #9874, #53008, #3928 ),
 ( #68123, #20158, #27175 ),
 ( #93996, #43846, #51929 ),
 ( #10925, #76736, #36860 ),
 ( #2847, #69729, #35800 ),
 ( #102619, #27715, #85378 ),
 ( #77285, #50858, #3395 ),
 ( #83764, #42786, #87509 ),
 ( #46503, #22788, #104196 ),
 ( #6029, #79398, #103156 ),
 ( #39490, #96126, #37393 ),
 ( #95593, #4991, #94548 ),
 ( #38952, #71829, #86467 ),
 ( #37921, #20699, #30885 ),
 ( #72365, #105271, #5514 ),
 ( #53538, #12525, #70783 ),
 ( #14117, #78863, #31416 ),
 ( #38438, #95075, #96652 ),
 ( #45459, #103678, #78333 ),
 ( #62701, #21208, #70255 ),
 ( #14642, #47019, #104734 ),
 ( #71303, #21729, #29301 ),
 ( #4450, #62190, #22259 ),
 ( #13588, #54038, #86983 ),
 ( #13052, #63764, #29823 ),
 ( #55624, #30340, #54570 ),
 ( #55106, #88561, #45984 ),
 ( #63233, #47550, #88037 ),
 ( #80447, #79921, #6557 ),
 ( #97691, #75006, #48076 ),
 ( #64809, #42120, #90684 ),
 ( #23855, #97165, #25456 ),
 ( #80976, #1102, #557 ),
 ( #49680, #82587, #7093 ),
 ( #56700, #73952, #83116 ),
 ( #15187, #24905, #64293 ),
 ( #7612, #16252, #41068 ),
 ( #74482, #81493, #58310 ),
 ( #91235, #33004, #32 ),
 ( #89623, #33525, #65871 ),
 ( #73410, #17341, #57228 ),
 ( #40009, #16794, #66398 ),
 ( #105792, #41598, #40531 ),
 ( #9212, #98750, #72880 ),
 ( #65342, #57759, #15722 ),
 ( #31931, #50216, #23312 ),
 ( #48607, #106307, #32472 ),
 ( #8161, #90147, #98232 ),
 ( #8692, #99279, #24388 ),
 ( #56148, #89091, #49136 ),
 ( #82037, #92803, #91753 ),
 ( #44809, #28116, #84190 ),
 ( #10805, #9740, #44267 ),
 ( #60990, #100359, #93877 ),
 ( #76612, #99828, #34610 ),
 ( #51267, #93352, #43197 ),
 ( #27053, #18411, #18963 ),
 ( #43722, #17872, #52338 ),
 ( #42657, #35675, #3274 ),
 ( #36215, #11881, #52880 ),
 ( #34076, #77158, #85251 ),
 ( #26000, #10286, #2725 ),
 ( #35132, #11334, #76082 ),
 ( #2183, #75556, #19503 ),
 ( #100887, #68551, #69082 ),
 ( #101438, #27590, #50725 ),
 ( #1651, #101955, #68002 ),
 ( #20036, #60472, #85807 ),
 ( #84718, #59937, #83636 ),
 ( #77697, #66948, #51807 ),
 ( #58861, #67481, #26523 ),
 ( #59395, #92256, #54440 ),
 ( #103556, #4866, #14516 ),
 ( #22128, #53422, #104074 ),
 ( #13993, #70663, #46386 ),
 ( #88443, #63646, #104608 ),
 ( #46900, #21093, #30760 ),
 ( #96535, #79276, #5397 ),
 ( #4332, #79805, #38319 ),
 ( #3807, #38833, #71180 ),
 ( #62579, #71697, #13464 ),
 ( #54980, #95463, #12406 ),
 ( #55504, #30217, #86340 ),
 ( #37802, #53929, #36746 ),
 ( #87911, #5902, #102501 ),
 ( #63102, #22666, #29705 ),
 ( #86860, #45337, #78730 ),
 ( #96004, #21609, #87390 ),
 ( #47427, #69608, #28644 ),
 ( #94421, #61529, #78216 ),
 ( #20584, #37265, #70130 ),
 ( #103036, #29193, #62069 ),
 ( #94956, #12936, #45857 ),
 ( #40405, #7489, #41467 ),
 ( #74357, #39368, #49011 ),
 ( #16128, #49556, #56577 ),
 ( #91107, #81912, #98632 ),
 ( #73832, #72246, #90556 ),
 ( #8028, #24783, #58181 ),
 ( #435, #106182, #106726 ),
 ( #33405, #17215, #31803 ),
 ( #64691, #88965, #47950 ),
 ( #32346, #15595, #16665 ),
 ( #24260, #48486, #105148 ),
 ( #66275, #40939, #97563 ),
 ( #89501, #15063, #82463 ),
 ( #23187, #6970, #23725 ),
 ( #32876, #99163, #80857 ),
 ( #39888, #80318, #65752 ),
 ( #72761, #6431, #25320 ),
 ( #31290, #8566, #105668 ),
 ( #57632, #56034, #98110 ),
 ( #90022, #64177, #65216 ),
 ( #97047, #81381, #73287 ),
 ( #57108, #26928, #25877 ),
 ( #67356, #44141, #9618 ),
 ( #18835, #92679, #9091 ),
 ( #93218, #51680, #27996 ),
 ( #85124, #84600, #27463 ),
 ( #66817, #76487, #60342 ),
 ( #2061, #58734, #10682 ),
 ( #59801, #52212, #60863 ),
 ( #101831, #59266, #1522 ),
 ( #19380, #42000, #100234 ),
 ( #77025, #51142, #101315 ),
 ( #91632, #18288, #17743 ),
 ( #35010, #10162, #43598 ),
 ( #3145, #2596, #35545 ),
 ( #11208, #50602, #68420 ),
 ( #84061, #36088, #68959 ),
 ( #43075, #93752, #99706 ),
 ( #50090, #82995, #74879 ),
 ( #75963, #967, #33948 ),
 ( #83517, #42528, #75430 ),
 ( #34489, #26402, #92140 ),
 ( #67876, #100760, #77568 ),
 ( #87261, #94828, #38200 ),
 ( #71059, #104482, #79679 ),
 ( #45727, #61396, #45215 ),
 ( #30629, #46263, #21479 ),
 ( #70540, #78608, #61938 ),
 ( #62452, #103431, #20975 ),
 ( #54859, #46786, #95344 ),
 ( #22005, #29069, #94285 ),
 ( #4739, #69480, #53292 ),
 ( #53808, #103951, #71576 ),
 ( #5789, #37679, #86738 ),
 ( #12812, #20452, #70004 ),
 ( #30096, #37138, #79148 ),
 ( #13871, #29581, #4208 ),
 ( #54315, #3684, #62980 ),
 ( #28513, #13336, #95881 ),
 ( #87788, #63518, #38711 ),
 ( #5274, #78090, #19905 ),
 ( #52747, #85670, #11745 ),
 ( #44681, #36615, #102904 ),
 ( #102365, #86213, #12285 ),
 ( #81256, #96928, #98509 ),
 ( #22547, #72645, #14392 ),
 ( #64571, #23063, #72119 ),
 ( #16537, #16008, #40807 ),
 ( #40281, #97438, #39244 ),
 ( #47304, #105028, #24139 ),
 ( #15470, #74235, #33278 ),
 ( #65088, #106603, #32210 ),
 ( #105547, #73701, #56447 ),
 ( #31169, #80200, #89897 ),
 ( #23599, #7901, #55902 ),
 ( #49427, #88838, #64053 ),
 ( #14932, #312, #6304 ),
 ( #56982, #96416, #90433 ),
 ( #48364, #73158, #47824 ),
 ( #6846, #82331, #80728 ),
 ( #97985, #48884, #55389 ),
 ( #32753, #81778, #88318 ),
 ( #24658, #65627, #57510 ),
 ( #39771, #8441, #41342 ),
 ( #31685, #89380, #7370 ),
 ( #106059, #68289, #44011 ),
 ( #11085, #75297, #17620 ),
 ( #43481, #58051, #9490 ),
 ( #60222, #67232, #10565 ),
 ( #74759, #34357, #839 ),
 ( #51012, #26275, #100640 ),
 ( #93090, #34886, #26800 ),
 ( #101184, #33812, #51556 ),
 ( #100110, #19262, #92552 ),
 ( #67753, #10039, #59137 ),
 ( #18700, #17084, #8966 ),
 ( #41871, #92019, #76899 ),
 ( #25194, #59671, #76357 ),
 ( #2470, #18155, #83928 ),
 ( #84470, #35418, #66688 ),
 ( #90973, #27345, #42946 ),
 ( #52090, #3012, #85001 ),
 ( #75837, #66148, #99030 ),
 ( #91506, #99569, #49961 ),
 ( #82869, #25748, #58603 ),
 ( #50481, #83393, #42402 ),
 ( #1390, #1935, #54201 ),
 ( #78491, #20327, #38083 ),
 ( #87140, #13217, #27880 ),
 ( #45619, #29977, #37016 ),
 ( #86089, #44555, #4088 ),
 ( #95230, #20858, #102780 ),
 ( #21361, #68834, #12161 ),
 ( #79031, #69884, #36495 ),
 ( #53691, #46145, #94709 ),
 ( #70940, #28942, #103832 ),
 ( #52617, #35964, #95750 ),
 ( #11625, #61816, #13748 ),
 ( #46659, #102242, #5150 ),
 ( #86624, #62865, #12687 ),
 ( #79557, #37552, #21892 ),
 ( #29464, #101713, #54733 ),
 ( #4622, #87669, #60745 ),
 ( #93633, #70420, #62335 ),
 ( #77442, #61267, #69363 ),
 ( #19784, #103316, #28394 ),
 ( #85545, #77971, #3557 ),
 ( #94157, #53172, #45092 ),
 ( #23477, #71998, #15349 ),
 ( #64451, #63404, #73033 ),
 ( #106471, #55782, #97324 ),
 ( #88193, #15883, #22947 ),
 ( #104910, #32629, #81138 ),
 ( #71457, #6186, #48759 ),
 ( #90302, #5671, #40682 ),
 ( #89779, #56858, #22422 ),
 ( #81652, #39652, #47177 ),
 ( #7247, #7777, #89251 ),
 ( #16411, #24540, #57390 ) ),
 .UNSPECIFIED., .T., .F., .F.,
 ( 4, 1, 1, 1, 1, 1, 1, 1, 1, 1, 1, 1, 1, 1, 1, 1, 1, 1, 1, 1, 1, 1, 1, 1, 1, 1, 1, 1, 1, 1, 1, 1, 1, 1, 1, 1, 1, 1, 1, 1, 1, 1, 1, 1, 1, 1, 1, 1, 1, 1, 1, 1, 1, 1, 1, 1, 1, 1, 1, 1, 1, 1, 1, 1, 1, 1, 1, 1, 1, 1, 1, 1, 1, 1, 1, 1, 1, 1, 1, 1, 1, 1, 1, 1, 1, 1, 1, 1, 1, 1, 1, 1, 1, 1, 1, 1, 1, 1, 1, 1, 1, 1, 1, 1, 1, 1, 1, 1, 1, 1, 1, 1, 1, 1, 1, 1, 1, 1, 1, 1, 1, 1, 1, 1, 1, 1, 1, 1, 1, 1, 2, 1, 1, 1, 1, 1, 1, 1, 1, 1, 1, 1, 1, 1, 1, 1, 1, 1, 1, 1, 1, 1, 1, 1, 1, 1, 1, 1, 1, 1, 1, 1, 1, 1, 1, 1, 1, 1, 1, 1, 1, 1, 1, 1, 1, 1, 1, 1, 1, 1, 1, 1, 1, 1, 1, 1, 1, 1, 1, 1, 1, 1, 1, 1, 1, 1, 1, 1, 1, 1, 1, 1, 1, 1, 1, 1, 1, 1, 1, 1, 1, 1, 1, 1, 1, 1, 1, 1, 1, 1, 1, 1, 1, 1, 1, 1, 1, 1, 1, 1, 1, 1, 1, 1, 1, 1, 1, 1, 1, 1, 1, 1, 1, 1, 1, 1, 1, 1, 1, 1, 1, 1, 1, 1, 1, 1, 1, 1, 1, 4 ),
 ( 2, 1, 2 ),
 ( 0.000000000000000000, 0.003906146814772826562, 0.007812293629545653123, 0.01171844044431847968, 0.01562458725909130625, 0.01953073407386413107, 0.02343688088863695937, 0.02734302770340978420, 0.03124917451818261249, 0.03320224792556902144, 0.03515532133295543732, 0.03710839474034185320, 0.03906146814772826215, 0.04296761496250108697, 0.04687376177727391874, 0.05468605540681956839, 0.06249834903636522498, 0.07031064266591087464, 0.07812293629545652429, 0.08593522992500217395, 0.09374752355454783748, 0.1015598171840934594, 0.1093721108136391368, 0.1132782576284119685, 0.1171844044431848003, 0.1210905512579576043, 0.1249966980727304500, 0.1289028448875032540, 0.1328089917022760857, 0.1367151385170488620, 0.1406212853318217493, 0.1445274321465945810, 0.1484335789613673851, 0.1523397257761402168, 0.1562458725909130486, 0.1601520194056858248, 0.1640581662204587121, 0.1679643130352315439, 0.1718704598500043479, 0.1757766066647771797, 0.1796827534795499559, 0.1816358268869364412, 0.1835889002943228432, 0.1855419737017092452, 0.1874950471090956750, 0.1914011939238684790, 0.1933542673312549365, 0.1953073407386413107, 0.1992134875534140870, 0.2011665609608005445, 0.2031196343681869187, 0.2050727077755734040, 0.2060492444792665356, 0.2070257811829598060, 0.2089788545903461525, 0.2109319279977326378, 0.2128850014051190120, 0.2148380748125054418, 0.2167911482198918716, 0.2187442216272782736, 0.2206972950346647311, 0.2226503684420510498, 0.2246034418494375351, 0.2265565152568239371, 0.2285095886642103391, 0.2304626620715967689, 0.2324157354789831431, 0.2343688088863696006, 0.2363218822937560304, 0.2382749557011424046, 0.2402280291085288344, 0.2421811025159151809, 0.2441341759233016939, 0.2460872493306880127, 0.2499933961454608999, 0.2538995429602335929, 0.2578056897750065080, 0.2617118365897793675, 0.2656179834045521715, 0.2695241302193249755, 0.2734302770340977240, 0.2773364238488707501, 0.2812425706636434986, 0.2851487174784163581, 0.2890548642931891621, 0.2968671579227347701, 0.3046794515522804336, 0.3124917451818260972, 0.3203040388113716497, 0.3281163324409174242, 0.3359286260704630878, 0.3437409197000086958, 0.3476470665147816108, 0.3515532133295543593, 0.3554593601443271633, 0.3593655069590999118, 0.3632716537738728824, 0.3671778005886456864, 0.3710839474034184904, 0.3749900942181913499, 0.3788962410329640984, 0.3828023878477369579, 0.3867085346625097619, 0.3906146814772826215, 0.3945208282920554810, 0.3984269751068281740, 0.4023331219216010890, 0.4042861953289875743, 0.4062392687363738375, 0.4081923421437603228, 0.4101454155511468080, 0.4120984889585330713, 0.4140515623659196121, 0.4160046357733060973, 0.4179577091806923050, 0.4199107825880789013, 0.4218638559954652756, 0.4257700028102379686, 0.4296761496250108836, 0.4335822964397836876, 0.4374884432545565471, 0.4413945900693294067, 0.4453007368841020996, 0.4492068836988750702, 0.4531130305136478742, 0.4609253241431935377, 0.4687376177727392013, 0.4765499114022848093, 0.4843622050318303618, 0.4921744986613760253, 0.4999867922909217999, 0.5077994986613761919, 0.5156122050318305838, 0.5234249114022848648, 0.5312376177727392568, 0.5390503241431936488, 0.5468630305136479297, 0.5507693836988751812, 0.5546757368841022107, 0.5585820900693294622, 0.5624884432545566026, 0.5663947964397838541, 0.5703011496250109946, 0.5742075028102381351, 0.5781138559954652756, 0.5800670325880789013, 0.5820202091806925271, 0.5839733857733060418, 0.5859265623659195565, 0.5878797389585332933, 0.5898329155511468080, 0.5917860921437604338, 0.5937392687363740595, 0.5956924453289873522, 0.5976456219216012000, 0.6015519751068284515, 0.6054583282920554810, 0.6093646814772826215, 0.6132710346625098730, 0.6171773878477370134, 0.6210837410329641539, 0.6249900942181914054, 0.6288964474034186569, 0.6328028005886456864, 0.6367091537738729379, 0.6406155069591000784, 0.6445218601443273299, 0.6484282133295544703, 0.6523345665147814998, 0.6562409197000087513, 0.6640536260704632543, 0.6718663324409175353, 0.6796790388113718162, 0.6874917451818260972, 0.6953044515522806002, 0.7031171579227348811, 0.7109298642931891621, 0.7148362174784161915, 0.7187425706636435541, 0.7226489238488706945, 0.7265552770340979460, 0.7304616302193250865, 0.7343679834045522270, 0.7382743365897792565, 0.7421806897750065080, 0.7460870429602337595, 0.7499933961454610110, 0.7538997493306882625, 0.7558529259233015551, 0.7578061025159152919, 0.7597592791085288066, 0.7617124557011423214, 0.7636656322937560581, 0.7656188088863695729, 0.7675719854789833096, 0.7695251620715968244, 0.7714783386642103391, 0.7734315152568238538, 0.7753846918494375906, 0.7773378684420511053, 0.7792910450346646201, 0.7812442216272783568, 0.7831973982198916495, 0.7851505748125056083, 0.7871037514051189010, 0.7890569279977326378, 0.7910101045903461525, 0.7929632811829598893, 0.7949164577755734040, 0.7968696343681870298, 0.7988228109608006555, 0.8007759875534141703, 0.8046823407386413107, 0.8066355173312547144, 0.8085886939238684512, 0.8124950471090957027, 0.8144482237017094395, 0.8164014002943229542, 0.8183545768869363579, 0.8203077534795502057, 0.8242141066647772352, 0.8281204598500044867, 0.8320268130352314051, 0.8359331662204587676, 0.8398395194056857971, 0.8437458725909130486, 0.8476522257761403001, 0.8515585789613675516, 0.8554649321465945810, 0.8593712853318218325, 0.8632776385170490840, 0.8671839917022761135, 0.8710903448875033650, 0.8749966980727305055, 0.8789030512579574239, 0.8828094044431848975, 0.8867157576284119269, 0.8906221108136391784, 0.8984348171840934594, 0.9062475235545479624, 0.9140602299250022433, 0.9218729362954565243, 0.9296856426659108052, 0.9374983490363653083, 0.9453110554068195892, 0.9531237617772740922, 0.9570301149625010106, 0.9609364681477282621, 0.9628896447403418879, 0.9648428213329554026, 0.9667959979255691394, 0.9687491745181826541, 0.9726555277034099056, 0.9765618808886369351, 0.9804682340738641866, 0.9843745872590914381, 0.9882809404443185786, 0.9921872936295457190, 0.9960936468147727485, 1.000000000000000000 ),
 ( 0.000000000000000000, 1.000000000000000000, 1.526318052600188269 ),
 .UNSPECIFIED. ) ;
#3348 = CARTESIAN_POINT ( 'NONE',  ( 6.638999116915723420, 3.157894740940597522, 14.66382285780688655 ) ) ;
#3349 = EDGE_LOOP ( 'NONE', ( #102749, #95468, #60400, #41036 ) ) ;
#3350 = SHAPE_REPRESENTATION_RELATIONSHIP ( 'NONE' , 'NONE' ,  #88164, #88554 ) ;
#3351 = VECTOR ( 'NONE', #73625, 1000.000000000000000 ) ;
#3352 = CARTESIAN_POINT ( 'NONE',  ( -81.05938286033433826, -29.99999999999999645, -11.75216569974085523 ) ) ;
#3353 = DIRECTION ( 'NONE',  ( -1.000000000000000000, -0.000000000000000000, -0.000000000000000000 ) ) ;
#3354 = CARTESIAN_POINT ( 'NONE',  ( 86.68749933009506492, -17.00766437030456402, 185.5393203993762370 ) ) ;
#3356 = CARTESIAN_POINT ( 'NONE',  ( -14.11595029532502465, 2.410436752314748521, -5.024000119269296682 ) ) ;
#3355 = CARTESIAN_POINT ( 'NONE',  ( 42.80674476973947407, 434.8200572688797934, 17.89667068458266641 ) ) ;
#3357 = VECTOR ( 'NONE', #38581, 1000.000000000000000 ) ;
#3358 = CARTESIAN_POINT ( 'NONE',  ( 2.977408999572651815, -23.93750000204838457, 7.188101187500000933 ) ) ;
#3359 = CARTESIAN_POINT ( 'NONE',  ( 17.09834626446250638, 294.5833046993913626, -2.056795529506987297 ) ) ;
#3360 = CARTESIAN_POINT ( 'NONE',  ( 9.999872502480483760, -5.000000000000000000, 1.308371270547806331 ) ) ;
#3361 = AXIS2_PLACEMENT_3D ( 'NONE', #80700, #102877, #4713 ) ;
#3362 = CARTESIAN_POINT ( 'NONE',  ( 42.10086803841214476, 435.6552064019005002, 19.95582312411065828 ) ) ;
#3363 = CONTEXT_DEPENDENT_SHAPE_REPRESENTATION ( #2535, #2828 ) ;
#3364 = EDGE_LOOP ( 'NONE', ( #96309, #65907 ) ) ;
#3365 = CARTESIAN_POINT ( 'NONE',  ( 39.81879459130803411, 485.8579414158143095, -5.000253522669845019 ) ) ;
#3366 = CARTESIAN_POINT ( 'NONE',  ( -8.473474469297077150, 27.00279687855394428, 0.000000000000000000 ) ) ;
#3367 = SURFACE_STYLE_USAGE ( .BOTH. , #69178 ) ;
#3368 = ORIENTED_EDGE ( 'NONE', *, *, #4688, .F. ) ;
#3369 = CARTESIAN_POINT ( 'NONE',  ( -8.240492251933538626, 51.94749170291629525, -1.561714456288526787 ) ) ;
#3370 = ORIENTED_EDGE ( 'NONE', *, *, #60706, .F. ) ;
#3371 = CONICAL_SURFACE ( 'NONE', #68836, 4.172000000000001485, 0.9599310885968750373 ) ;
#3372 = EDGE_CURVE ( 'NONE', #58364, #25443, #76911, .T. ) ;
#3373 = CARTESIAN_POINT ( 'NONE',  ( 32.30809144287577794, 435.2315602164904362, 15.37655368195066963 ) ) ;
#3374 = CARTESIAN_POINT ( 'NONE',  ( -1.411247199636991373E-12, 7.746009256445978153, -51.75000000000450484 ) ) ;
#3375 = CARTESIAN_POINT ( 'NONE',  ( 8.099999999999999645, 0.000000000000000000, 4.000000000000000000 ) ) ;
#3376 = CARTESIAN_POINT ( 'NONE',  ( -17.96008057617824605, 36.59330496951920253, 22.69888471349226577 ) ) ;
#3377 = CARTESIAN_POINT ( 'NONE',  ( -111.1352917996996013, -60.00000000000000000, 186.5960929966779815 ) ) ;
#3378 = CARTESIAN_POINT ( 'NONE',  ( 19.50000000000146017, 49.99999999999911893, 59.56761335716116434 ) ) ;
#3379 = CARTESIAN_POINT ( 'NONE',  ( 5.441945782601297132, 4.363644636964920664, -0.3576316571898332519 ) ) ;
#3380 = CARTESIAN_POINT ( 'NONE',  ( -43.00000000000000000, 461.9428920847514632, 12.03309428281654725 ) ) ;
#3381 = DIRECTION ( 'NONE',  ( -1.000000000000000000, -1.224606353822377258E-16, -0.000000000000000000 ) ) ;
#3382 = CARTESIAN_POINT ( 'NONE',  ( -85.94455300974112788, -21.71266392783007504, 172.2523347831352964 ) ) ;
#3383 = CARTESIAN_POINT ( 'NONE',  ( -4.063221008705400372, 54.18599283795405341, -6.989960337625931608 ) ) ;
#3384 = EDGE_LOOP ( 'NONE', ( #61050, #90181, #23921, #56561 ) ) ;
#3385 = CARTESIAN_POINT ( 'NONE',  ( -9.268669127170596767, 46.19464124546546913, -13.41262564492496345 ) ) ;
#3386 = DIRECTION ( 'NONE',  ( 0.000000000000000000, 0.000000000000000000, 1.000000000000000000 ) ) ;
#3387 = CARTESIAN_POINT ( 'NONE',  ( -86.46969771635572499, -60.13837812595784982, 2.720957838497157333 ) ) ;
#3388 = AXIS2_PLACEMENT_3D ( 'NONE', #84982, #84452, #58027 ) ;
#3389 = CARTESIAN_POINT ( 'NONE',  ( -1.000000000000000000, -5.000000000000018652, -14.14213562373094568 ) ) ;
#3390 = MECHANICAL_DESIGN_GEOMETRIC_PRESENTATION_REPRESENTATION (  '', ( #98015 ), #65374 ) ;
#3391 = CARTESIAN_POINT ( 'NONE',  ( -3.727646769453142106, 20.26854631371922366, -5.000000000000000000 ) ) ;
#3392 = CARTESIAN_POINT ( 'NONE',  ( 7.849086896546205061, 81.65194826718307297, -4.999999999990173194 ) ) ;
#3393 = CARTESIAN_POINT ( 'NONE',  ( 27.10511071441176867, 36.60571256639526894, -10.05698433968634653 ) ) ;
#3394 = CARTESIAN_POINT ( 'NONE',  ( -79.13121736037263076, 42.00000000000000000, -45.60838156032659185 ) ) ;
#3395 = CARTESIAN_POINT ( 'NONE',  ( 78.54417320222145804, -14.21045842199432307, 165.9036888455924270 ) ) ;
#3396 =( GEOMETRIC_REPRESENTATION_CONTEXT ( 3 ) GLOBAL_UNCERTAINTY_ASSIGNED_CONTEXT ( ( #26806 ) ) GLOBAL_UNIT_ASSIGNED_CONTEXT ( ( #28727, #13547, #60546 ) ) REPRESENTATION_CONTEXT ( 'NONE', 'WORKASPACE' ) );
#3397 = PRESENTATION_STYLE_ASSIGNMENT (( #8289 ) ) ;
#3398 = EDGE_CURVE ( 'NONE', #101318, #85895, #51098, .T. ) ;
#3399 = CARTESIAN_POINT ( 'NONE',  ( -94.69971540129887444, -59.99999999999987921, 1.030331952319396782 ) ) ;
#3400 = CARTESIAN_POINT ( 'NONE',  ( -69.47556247483554159, -25.58659212672100125, 92.27640143973368936 ) ) ;
#3401 = VERTEX_POINT ( 'NONE', #31723 ) ;
#3402 = CARTESIAN_POINT ( 'NONE',  ( 86.51021125171571668, -60.00000000000013500, 203.5141634203183685 ) ) ;
#3403 = CARTESIAN_POINT ( 'NONE',  ( -39.07690614691289710, 40.83957160057924796, 52.28546855715760699 ) ) ;
#3404 = CARTESIAN_POINT ( 'NONE',  ( 22.37633122833116417, -57.67115084601979191, -43.62954971562658812 ) ) ;
#3405 = ORIENTED_EDGE ( 'NONE', *, *, #89956, .T. ) ;
#3406 = CARTESIAN_POINT ( 'NONE',  ( 13.97222917066916992, -57.87254792530227121, 26.08167946173673002 ) ) ;
#3407 = CARTESIAN_POINT ( 'NONE',  ( 5.082755093536325930, -23.84375000204838457, -5.082755093536325042 ) ) ;
#3408 = AXIS2_PLACEMENT_3D ( 'NONE', #36883, #4477, #70279 ) ;
#3409 = EDGE_CURVE ( 'NONE', #53391, #17004, #65304, .T. ) ;
#3410 = CARTESIAN_POINT ( 'NONE',  ( -0.7863538930209251765, 27.39022669171391300, -40.48520517837179256 ) ) ;
#3411 = ORIENTED_EDGE ( 'NONE', *, *, #32747, .F. ) ;
#3412 = CARTESIAN_POINT ( 'NONE',  ( -16.10302234481879680, 5.501632350609884980, -4.770674012950244069 ) ) ;
#3413 = ORIENTED_EDGE ( 'NONE', *, *, #53423, .F. ) ;
#3414 = CARTESIAN_POINT ( 'NONE',  ( -30.00000000000000000, 488.8442721620238558, 4.433647275927475206 ) ) ;
#3415 = CARTESIAN_POINT ( 'NONE',  ( 46.79638705082384575, 18.85256363620282016, -15.38003188690575662 ) ) ;
#3416 = CARTESIAN_POINT ( 'NONE',  ( 2.936182742933428427E-09, -59.99999999999998579, 41.99999999999666755 ) ) ;
#3417 = CARTESIAN_POINT ( 'NONE',  ( -10.28624191511820207, 43.99263840937192782, 12.90779740156163768 ) ) ;
#3418 = CARTESIAN_POINT ( 'NONE',  ( -7.188101187500000044, -9.406250002048384573, -8.802885111219163269E-16 ) ) ;
#3419 = CARTESIAN_POINT ( 'NONE',  ( -48.26904874857379468, 16.21976735686916271, 14.37315625587772949 ) ) ;
#3420 = CARTESIAN_POINT ( 'NONE',  ( 23.93420880016848074, -4.285714285714296246, -8.127057321558242009 ) ) ;
#3421 = FACE_OUTER_BOUND ( 'NONE', #40838, .T. ) ;
#3422 = AXIS2_PLACEMENT_3D ( 'NONE', #41883, #10053, #57522 ) ;
#3423 = CARTESIAN_POINT ( 'NONE',  ( -7.374560640982810611, 50.00000000000000000, -75.40399789251387119 ) ) ;
#3424 = CARTESIAN_POINT ( 'NONE',  ( 3.750000000000004885, -6.495190528383287365, 1.734723475976807094E-15 ) ) ;
#3425 = CARTESIAN_POINT ( 'NONE',  ( 42.34430797737972796, 436.4403912042729985, 6.776599765011303234 ) ) ;
#3426 = ORIENTED_EDGE ( 'NONE', *, *, #105196, .T. ) ;
#3428 = CARTESIAN_POINT ( 'NONE',  ( 32.92851612125411975, -46.42981575483278078, 35.59486626606223325 ) ) ;
#3427 = CARTESIAN_POINT ( 'NONE',  ( -6.928203230275507885, 105.0000000000000000, -4.000000000000001776 ) ) ;
#3429 = FILL_AREA_STYLE ('',( #28812 ) ) ;
#3430 = VERTEX_POINT ( 'NONE', #72682 ) ;
#3431 = CARTESIAN_POINT ( 'NONE',  ( 0.000000000000000000, 79.50000000000000000, 0.000000000000000000 ) ) ;
#3432 = AXIS2_PLACEMENT_3D ( 'NONE', #101971, #83136, #84736 ) ;
#3433 = PRODUCT_RELATED_PRODUCT_CATEGORY ( 'part', '', ( #101837 ) ) ;
#3435 = CARTESIAN_POINT ( 'NONE',  ( -35.56416567029047116, 496.2909070316903239, -10.19064917708978335 ) ) ;
#3434 = CARTESIAN_POINT ( 'NONE',  ( 30.56153846153846132, -4.171999999999999709, 5.616230220889763424E-16 ) ) ;
#3436 = DIRECTION ( 'NONE',  ( 0.000000000000000000, -1.000000000000000000, 0.000000000000000000 ) ) ;
#3437 = FACE_OUTER_BOUND ( 'NONE', #74348, .T. ) ;
#3438 = CARTESIAN_POINT ( 'NONE',  ( -7.500000000000007105, -4.999999999999999112, -68.91429205785460965 ) ) ;
#3439 = FACE_OUTER_BOUND ( 'NONE', #106693, .T. ) ;
#3440 = DIRECTION ( 'NONE',  ( 0.000000000000000000, 1.000000000000000000, 0.000000000000000000 ) ) ;
#3441 = ORIENTED_EDGE ( 'NONE', *, *, #47097, .F. ) ;
#3442 = CIRCLE ( 'NONE', #86152, 4.000000000000000000 ) ;
#3443 = CARTESIAN_POINT ( 'NONE',  ( 92.27650878891940067, -59.99999999999999289, 1.835041955732973351 ) ) ;
#3444 = CARTESIAN_POINT ( 'NONE',  ( 33.13158811909483603, 464.8683774687789310, 15.82274808412723743 ) ) ;
#3445 = CARTESIAN_POINT ( 'NONE',  ( -36.71129544689416946, 382.4568683582283484, 5.283419339595673669 ) ) ;
#3446 = CARTESIAN_POINT ( 'NONE',  ( -6.541889698517638685, 41.04792438554813572, -71.02384096075095954 ) ) ;
#3447 = CARTESIAN_POINT ( 'NONE',  ( -12.39315421835605768, 18.01515667718084757, -8.658431383304368012 ) ) ;
#3448 = ORIENTED_EDGE ( 'NONE', *, *, #3473, .T. ) ;
#3449 = CARTESIAN_POINT ( 'NONE',  ( -109.5905853243550467, -30.00000000000664357, 171.0618735817303104 ) ) ;
#3450 = VERTEX_POINT ( 'NONE', #6887 ) ;
#3451 = EDGE_CURVE ( 'NONE', #51169, #24752, #92456, .T. ) ;
#3452 = CARTESIAN_POINT ( 'NONE',  ( -9.301012663197237629, -55.30021075719776036, 23.32537848786287782 ) ) ;
#3453 = SURFACE_STYLE_FILL_AREA ( #77875 ) ;
#3454 = DIRECTION ( 'NONE',  ( 1.000000000000000000, 0.000000000000000000, 0.000000000000000000 ) ) ;
#3455 = CARTESIAN_POINT ( 'NONE',  ( 14.87468076903141245, 23.07153947554854767, -1.073492826214703433 ) ) ;
#3456 = CARTESIAN_POINT ( 'NONE',  ( 84.22572678630466214, -52.73862619169806720, -14.84760467275862972 ) ) ;
#3457 = CARTESIAN_POINT ( 'NONE',  ( -5.082755093536326818, -29.09375000204838813, 5.082755093536325042 ) ) ;
#3458 = VECTOR ( 'NONE', #102172, 1000.000000000000227 ) ;
#3459 = CARTESIAN_POINT ( 'NONE',  ( -17.86128288688793120, 34.21128401912330474, 23.65645931953497438 ) ) ;
#3460 = CARTESIAN_POINT ( 'NONE',  ( 9.204171687489081322, 45.78377104600746605, -14.80353108812691687 ) ) ;
#3461 = ORIENTED_EDGE ( 'NONE', *, *, #33936, .F. ) ;
#3462 = CARTESIAN_POINT ( 'NONE',  ( 98.31310517497099966, 1.030564683017419500E-14, 0.000000000000000000 ) ) ;
#3463 = ADVANCED_FACE ( 'NONE', ( #73197 ), #11445, .F. ) ;
#3464 = ORIENTED_EDGE ( 'NONE', *, *, #88915, .F. ) ;
#3465 = CARTESIAN_POINT ( 'NONE',  ( 49.19520577559729446, 7.745679164654342586, -16.05969994618069308 ) ) ;
#3467 = ORIENTED_EDGE ( 'NONE', *, *, #95223, .F. ) ;
#3466 = SURFACE_SIDE_STYLE ('',( #4518 ) ) ;
#3468 = CARTESIAN_POINT ( 'NONE',  ( 72.11924800345758513, -53.37899342557430060, 118.2001781568277750 ) ) ;
#3469 = ORIENTED_EDGE ( 'NONE', *, *, #85599, .F. ) ;
#3470 = CARTESIAN_POINT ( 'NONE',  ( 1.431705818242835271, -50.02825494199252887, 40.96159436747194604 ) ) ;
#3471 = EDGE_CURVE ( 'NONE', #96331, #81100, #62643, .T. ) ;
#3472 = CARTESIAN_POINT ( 'NONE',  ( -2.977408999572654480, -18.12500000204838457, 7.188101187499999156 ) ) ;
#3473 = EDGE_CURVE ( 'NONE', #4931, #60457, #56245, .T. ) ;
#3474 = CARTESIAN_POINT ( 'NONE',  ( -93.91996415714238822, -57.61928231945634593, 204.5092364001214946 ) ) ;
#3475 = VERTEX_POINT ( 'NONE', #75801 ) ;
#3476 = B_SPLINE_CURVE_WITH_KNOTS ( 'NONE', 3,
 ( #66202, #91037, #2526, #895 ),
 .UNSPECIFIED., .F., .F.,
 ( 4, 4 ),
 ( 0.000000000000000000, 0.002179111408645760528 ),
 .UNSPECIFIED. ) ;
#3477 = AXIS2_PLACEMENT_3D ( 'NONE', #71061, #87790, #24661 ) ;
#3478 =( NAMED_UNIT ( * ) SI_UNIT ( $, .STERADIAN. ) SOLID_ANGLE_UNIT ( ) );
#3479 = CARTESIAN_POINT ( 'NONE',  ( -33.14701693048364461, 42.84762493505142089, -64.93038575622274777 ) ) ;
#3480 = ADVANCED_FACE ( 'NONE', ( #35384 ), #66597, .T. ) ;
#3481 = CARTESIAN_POINT ( 'NONE',  ( -5.855777637195783925, -13.78106496758447719, -1.331220292256675597 ) ) ;
#3482 = CIRCLE ( 'NONE', #48267, 5.000000000000002665 ) ;
#3483 = DIRECTION ( 'NONE',  ( 0.3573389821851922776, -0.9339747597290041226, 0.000000000000000000 ) ) ;
#3484 = CARTESIAN_POINT ( 'NONE',  ( 49.24354615586579342, 13.35554545791556968, -15.29900703100353176 ) ) ;
#3485 = CARTESIAN_POINT ( 'NONE',  ( -1.469576158976823947E-15, -19.06250000409677270, 8.000000000000000000 ) ) ;
#3486 = CARTESIAN_POINT ( 'NONE',  ( -51.48836687262417655, -29.91056394135168262, 49.15659163052040270 ) ) ;
#3487 = CARTESIAN_POINT ( 'NONE',  ( -10.28624191511820207, -1.200000000000000030E-05, 12.90779740156163768 ) ) ;
#3488 = CARTESIAN_POINT ( 'NONE',  ( 29.66054107240687543, 5.000000000000002665, 0.000000000000000000 ) ) ;
#3489 = CARTESIAN_POINT ( 'NONE',  ( -37.06599482041617932, 437.8929527014068412, 4.336831230530949099 ) ) ;
#3490 = CARTESIAN_POINT ( 'NONE',  ( 0.000000000000000000, 27.68727484027578356, 0.000000000000000000 ) ) ;
#3491 = APPLICATION_PROTOCOL_DEFINITION ( 'draft international standard', 'automotive_design', 1998, #63831 ) ;
#3492 = CARTESIAN_POINT ( 'NONE',  ( 1.754457302166835930, -30.00000000000002132, -7.493468971370472076 ) ) ;
#3493 = ORIENTED_EDGE ( 'NONE', *, *, #101233, .T. ) ;
#3494 = AXIS2_PLACEMENT_3D ( 'NONE', #30252, #64725, #46423 ) ;
#3495 = FILL_AREA_STYLE_COLOUR ( '', #45710 ) ;
#3496 = CARTESIAN_POINT ( 'NONE',  ( 6.849999999999999645, 6.123233995736770227E-16, -5.000000000000002665 ) ) ;
#3497 = CIRCLE ( 'NONE', #74066, 4.000000000000001776 ) ;
#3498 = CARTESIAN_POINT ( 'NONE',  ( -57.05541872896377242, -28.84113649674122115, -25.95661199123281548 ) ) ;
#3499 = CARTESIAN_POINT ( 'NONE',  ( -87.75496598979771079, -29.99999999999999289, 186.1453428037212632 ) ) ;
#3500 = EDGE_LOOP ( 'NONE', ( #100297, #70026, #20225, #20569 ) ) ;
#3501 = CARTESIAN_POINT ( 'NONE',  ( -17.91929324317234418, -4.333298119783932201, -0.09842992240431641671 ) ) ;
#3502 = CARTESIAN_POINT ( 'NONE',  ( 83.57756196019212780, -57.54177920181132322, 201.5121743845033393 ) ) ;
#3503 = DIRECTION ( 'NONE',  ( 0.000000000000000000, 0.000000000000000000, 1.000000000000000000 ) ) ;
#3504 = EDGE_CURVE ( 'NONE', #65472, #72783, #16395, .T. ) ;
#3506 = CARTESIAN_POINT ( 'NONE',  ( 24.04396523262633067, -27.34829711589978984, -38.39905134658587826 ) ) ;
#3505 = CIRCLE ( 'NONE', #68963, 4.172000000000001485 ) ;
#3507 = FILL_AREA_STYLE ('',( #53121 ) ) ;
#3508 = CARTESIAN_POINT ( 'NONE',  ( 2.617478843592802029, -3.000000000000003109, -94.73972676668317661 ) ) ;
#3509 = CARTESIAN_POINT ( 'NONE',  ( -56.06363120456222049, -60.00000000000000711, 88.36825490483376200 ) ) ;
#3510 = CARTESIAN_POINT ( 'NONE',  ( -31.44385389780523354, 439.7015230996784680, 23.50466788255525330 ) ) ;
#3511 = AXIS2_PLACEMENT_3D ( 'NONE', #6834, #39754, #56434 ) ;
#3512 = FILL_AREA_STYLE ('',( #61224 ) ) ;
#3513 = CARTESIAN_POINT ( 'NONE',  ( -85.68179626072733868, -57.45883239149054589, 192.8351143831483512 ) ) ;
#3514 = ORIENTED_EDGE ( 'NONE', *, *, #45773, .T. ) ;
#3515 = CARTESIAN_POINT ( 'NONE',  ( 30.36582766586239046, 16.93822630193517398, 39.80117229897599174 ) ) ;
#3516 = CARTESIAN_POINT ( 'NONE',  ( -2.999853627381086518, -29.03101188044279368, 28.72356160493805532 ) ) ;
#3517 = CARTESIAN_POINT ( 'NONE',  ( -7.040972322291190189, 41.74416393942964731, -59.82830748482982841 ) ) ;
#3518 = DIRECTION ( 'NONE',  ( -0.000000000000000000, -0.000000000000000000, 1.000000000000000000 ) ) ;
#3520 = ADVANCED_FACE ( 'NONE', ( #59637 ), #45797, .T. ) ;
#3519 = DIRECTION ( 'NONE',  ( 1.000000000000000000, 0.000000000000000000, 0.000000000000000000 ) ) ;
#3521 = ORIENTED_EDGE ( 'NONE', *, *, #96460, .T. ) ;
#3522 = DIRECTION ( 'NONE',  ( 0.000000000000000000, -1.000000000000000000, 0.000000000000000000 ) ) ;
#3523 = FACE_OUTER_BOUND ( 'NONE', #13578, .T. ) ;
#3524 = DIRECTION ( 'NONE',  ( -1.000000000000000000, -0.000000000000000000, -0.000000000000000000 ) ) ;
#3525 = LINE ( 'NONE', #76867, #72255 ) ;
#3526 = EDGE_LOOP ( 'NONE', ( #73658, #49880, #3793, #83430, #80989 ) ) ;
#3527 = VECTOR ( 'NONE', #7053, 1000.000000000000000 ) ;
#3528 = CARTESIAN_POINT ( 'NONE',  ( 17.51640565573907438, 49.99999999999999289, 63.26730910660373297 ) ) ;
#3529 = CARTESIAN_POINT ( 'NONE',  ( 45.48003679188781234, 379.8448106960472614, 7.220331889307936457 ) ) ;
#3530 = CARTESIAN_POINT ( 'NONE',  ( -3.301606509414613644, -4.285714285714286476, 25.22241582816893413 ) ) ;
#3531 = CARTESIAN_POINT ( 'NONE',  ( 9.323684072238750176, 53.46633439451886005, -3.784536294736342565 ) ) ;
#3532 = CARTESIAN_POINT ( 'NONE',  ( 104.6755681235317326, -59.99999999999997158, 94.38101796850538960 ) ) ;
#3533 = AXIS2_PLACEMENT_3D ( 'NONE', #82497, #91140, #8598 ) ;
#3534 = CARTESIAN_POINT ( 'NONE',  ( -83.18631812101111223, -22.15354509450119025, 146.6237897504154546 ) ) ;
#3535 = ORIENTED_EDGE ( 'NONE', *, *, #3927, .F. ) ;
#3536 = CARTESIAN_POINT ( 'NONE',  ( 9.797174393178825657E-16, -30.00000000000000000, -8.000000000000000000 ) ) ;
#3537 = CARTESIAN_POINT ( 'NONE',  ( 8.572527594031464315E-16, 60.00000000000000000, -6.999999999999992895 ) ) ;
#3538 = CARTESIAN_POINT ( 'NONE',  ( 46.71400118704798388, -57.68116600608826161, 69.02050771961488351 ) ) ;
#3539 = CARTESIAN_POINT ( 'NONE',  ( -7.347171990171222689, -3.439186728100687596, -18.43985286355804831 ) ) ;
#3540 = CARTESIAN_POINT ( 'NONE',  ( 39.24201634569103447, 311.8066870805746476, 2.048417762942908560 ) ) ;
#3541 = EDGE_CURVE ( 'NONE', #14549, #76235, #44691, .T. ) ;
#3542 = CARTESIAN_POINT ( 'NONE',  ( 43.72580207737490809, 464.6834397206198446, 7.653156261474082456 ) ) ;
#3543 = VERTEX_POINT ( 'NONE', #59101 ) ;
#3544 = CARTESIAN_POINT ( 'NONE',  ( 0.000000000000000000, 0.000000000000000000, 0.000000000000000000 ) ) ;
#3545 = CARTESIAN_POINT ( 'NONE',  ( 32.15310320217080431, 439.7024266304582625, 23.94087012106557566 ) ) ;
#3546 = CARTESIAN_POINT ( 'NONE',  ( -5.082755093536326818, -24.21875000204838813, 5.082755093536325042 ) ) ;
#3547 = ORIENTED_EDGE ( 'NONE', *, *, #45819, .T. ) ;
#3549 = EDGE_CURVE ( 'NONE', #71545, #17004, #72925, .T. ) ;
#3548 = CARTESIAN_POINT ( 'NONE',  ( 20.77592568779148863, 1.482358050883964840E-15, 0.000000000000000000 ) ) ;
#3550 = CARTESIAN_POINT ( 'NONE',  ( 6.583551125402590465, 41.48989066035234430, -70.62107025640376889 ) ) ;
#3551 = CARTESIAN_POINT ( 'NONE',  ( 28.00203968317441294, 50.00000000000000000, 56.72941417029700517 ) ) ;
#3552 = DIRECTION ( 'NONE',  ( 0.5735764363510491570, -0.8191520442889895781, 1.003171929053522035E-16 ) ) ;
#3553 = AXIS2_PLACEMENT_3D ( 'NONE', #18158, #51017, #10043 ) ;
#3554 = CARTESIAN_POINT ( 'NONE',  ( 12.33349330513380693, 4.000000000000002665, 0.000000000000000000 ) ) ;
#3555 = VERTEX_POINT ( 'NONE', #84964 ) ;
#3556 = CARTESIAN_POINT ( 'NONE',  ( 51.11362513016616305, -59.99999999999997868, -37.68753618808192840 ) ) ;
#3558 = CARTESIAN_POINT ( 'NONE',  ( 23.12828282194952578, -22.07908306402419996, 28.45182989271827978 ) ) ;
#3557 = CARTESIAN_POINT ( 'NONE',  ( -37.63111671575072137, -14.21045842199439235, 41.24562198507008759 ) ) ;
#3559 = CARTESIAN_POINT ( 'NONE',  ( 72.28092228780033679, 43.22324503868516388, -36.14046114390014708 ) ) ;
#3560 = CARTESIAN_POINT ( 'NONE',  ( -36.41141080624493753, -49.89788766448109669, 38.20003062495130308 ) ) ;
#3561 = EDGE_LOOP ( 'NONE', ( #67221, #106661, #62567, #61835 ) ) ;
#3562 = AXIS2_PLACEMENT_3D ( 'NONE', #68522, #52850, #51778 ) ;
#3563 = FACE_OUTER_BOUND ( 'NONE', #45116, .T. ) ;
#3564 = B_SPLINE_CURVE_WITH_KNOTS ( 'NONE', 3,
 ( #82944, #48960, #9042, #43025, #915, #34962 ),
 .UNSPECIFIED., .F., .F.,
 ( 4, 2, 4 ),
 ( 0.02753256083616404531, 0.02987018135583072859, 0.03220780187549741186 ),
 .UNSPECIFIED. ) ;
#3565 = FACE_OUTER_BOUND ( 'NONE', #41606, .T. ) ;
#3566 = CARTESIAN_POINT ( 'NONE',  ( -13.50905259634051170, -55.29488368535347576, 23.32354201833150853 ) ) ;
#3567 = CARTESIAN_POINT ( 'NONE',  ( -1.248789410298115632, 51.75335132569763630, -8.832271914632384480 ) ) ;
#3568 = CARTESIAN_POINT ( 'NONE',  ( 0.7521598644401954470, 299.9999999999999432, 9.936704142781159987 ) ) ;
#3569 = CARTESIAN_POINT ( 'NONE',  ( 0.000000000000000000, -5.629165124598850767, -3.249999999999999556 ) ) ;
#3570 = ORIENTED_EDGE ( 'NONE', *, *, #49537, .T. ) ;
#3571 = DIRECTION ( 'NONE',  ( 0.000000000000000000, 1.000000000000000000, 0.000000000000000000 ) ) ;
#3572 = ORIENTED_EDGE ( 'NONE', *, *, #16347, .F. ) ;
#3573 = CARTESIAN_POINT ( 'NONE',  ( 90.37091339520917188, -30.00000000000016698, 190.1441424001023393 ) ) ;
#3574 = CARTESIAN_POINT ( 'NONE',  ( 39.47751996913581252, 39.86337285071881809, -53.66483119571051930 ) ) ;
#3575 = ADVANCED_FACE ( 'NONE', ( #74722 ), #45966, .T. ) ;
#3577 = CARTESIAN_POINT ( 'NONE',  ( -5.981691436642414317, -81.02730900805887870, -0.5384679144502629855 ) ) ;
#3576 = AXIS2_PLACEMENT_3D ( 'NONE', #35319, #1834, #26180 ) ;
#3578 = CARTESIAN_POINT ( 'NONE',  ( 76.79371475606434672, -30.00000000000000711, -16.79878599767251046 ) ) ;
#3579 =( BOUNDED_SURFACE ( )  B_SPLINE_SURFACE ( 3, 2, ( 
 ( #34118, #98278, #9254 ),
 ( #41640, #42164, #73454 ),
 ( #57802, #8732, #75045 ),
 ( #90726, #23897, #106352 ),
 ( #99321, #7655, #31972 ),
 ( #97207, #74523, #90190 ),
 ( #32514, #15232, #25495 ),
 ( #82082, #81530, #72920 ) ),
 .UNSPECIFIED., .F., .F., .F. ) 
 B_SPLINE_SURFACE_WITH_KNOTS ( ( 4, 2, 2, 4 ),
 ( 3, 3 ),
 ( 0.03205733154476830132, 0.03606343422293256662, 0.03806648556201470274, 0.04006953690109683885 ),
 ( 0.000000000000000000, 1.000000000000000000 ),
 .UNSPECIFIED. ) 
 GEOMETRIC_REPRESENTATION_ITEM ( )  RATIONAL_B_SPLINE_SURFACE ( (
 ( 1.000000000000000000, 0.8047781205924506853, 1.000000000000000000),
 ( 1.000000000000000000, 0.8123783054473237009, 1.000000000000000000),
 ( 1.000000000000000000, 0.8190665327891030190, 1.000000000000000000),
 ( 1.000000000000000000, 0.8191934993920665375, 1.000000000000000000),
 ( 1.000000000000000000, 0.8176088856299312813, 1.000000000000000000),
 ( 1.000000000000000000, 0.8122958243108089338, 1.000000000000000000),
 ( 1.000000000000000000, 0.8086309198479199045, 1.000000000000000000),
 ( 1.000000000000000000, 0.8047712443299024354, 1.000000000000000000) ) ) 
 REPRESENTATION_ITEM ( '' )  SURFACE ( )  );
#3580 = CARTESIAN_POINT ( 'NONE',  ( -30.83453506004888212, 330.9311655802554242, 16.54362330515257540 ) ) ;
#3581 = VERTEX_POINT ( 'NONE', #806 ) ;
#3582 = VECTOR ( 'NONE', #88790, 1000.000000000000000 ) ;
#3583 = ORIENTED_EDGE ( 'NONE', *, *, #83118, .T. ) ;
#3584 = ORIENTED_EDGE ( 'NONE', *, *, #57707, .F. ) ;
#3585 = LINE ( 'NONE', #30533, #92139 ) ;
#3586 = LINE ( 'NONE', #28420, #62108 ) ;
#3587 = CARTESIAN_POINT ( 'NONE',  ( 35.01485412685309484, 439.9564946629565725, 24.34373102818600998 ) ) ;
#3588 = CARTESIAN_POINT ( 'NONE',  ( -17.86524139598605743, 43.17258651664646152, -5.721017747561236710 ) ) ;
#3589 = CARTESIAN_POINT ( 'NONE',  ( -7.046289519167717508, -86.30591819944376653, -3.789821819998814512 ) ) ;
#3590 = FACE_OUTER_BOUND ( 'NONE', #50591, .T. ) ;
#3591 = EDGE_LOOP ( 'NONE', ( #104513, #19307, #67025, #28616, #102805, #31099 ) ) ;
#3592 = CARTESIAN_POINT ( 'NONE',  ( 10.48543666094731996, 50.00000000000000000, -91.04342776276723725 ) ) ;
#3593 = VECTOR ( 'NONE', #85180, 1000.000000000000000 ) ;
#3594 = ORIENTED_EDGE ( 'NONE', *, *, #68800, .F. ) ;
#3595 = CARTESIAN_POINT ( 'NONE',  ( -5.999787407977320797, -61.00031888815551895, 0.2740427891042978015 ) ) ;
#3596 = CARTESIAN_POINT ( 'NONE',  ( 60.37599435018250915, -38.34251099049790668, 97.59093692943510234 ) ) ;
#3597 = CARTESIAN_POINT ( 'NONE',  ( 31.31887015984906952, 437.4276192545529511, 20.46811517093788524 ) ) ;
#3598 = CARTESIAN_POINT ( 'NONE',  ( 27.29305843655094321, 296.4586347574746696, 2.285620244940167023 ) ) ;
#3599 = AXIS2_PLACEMENT_3D ( 'NONE', #64956, #65494, #98381 ) ;
#3600 = FACE_OUTER_BOUND ( 'NONE', #74002, .T. ) ;
#3602 = CARTESIAN_POINT ( 'NONE',  ( 59.77473313328942339, -39.48835101806282921, 71.62691032963155635 ) ) ;
#3601 = PRODUCT ( '3. Bracket', '3. Bracket', '', ( #6660 ) ) ;
#3603 = VERTEX_POINT ( 'NONE', #38043 ) ;
#3604 = CARTESIAN_POINT ( 'NONE',  ( -9.739726766683149961, -3.000000000000003109, -87.61747884359282068 ) ) ;
#3605 = ADVANCED_FACE ( 'NONE', ( #45053 ), #52581, .T. ) ;
#3606 = CARTESIAN_POINT ( 'NONE',  ( 55.74444444444444713, 6.915964383211875250E-15, 0.000000000000000000 ) ) ;
#3607 = DIRECTION ( 'NONE',  ( 0.000000000000000000, -1.000000000000000000, 0.000000000000000000 ) ) ;
#3608 = EDGE_CURVE ( 'NONE', #10075, #96318, #85505, .T. ) ;
#3609 = CARTESIAN_POINT ( 'NONE',  ( -9.810837553057309535, 51.28247512958390075, 2.841815975853968723 ) ) ;
#3610 = ORIENTED_EDGE ( 'NONE', *, *, #77241, .F. ) ;
#3612 = CYLINDRICAL_SURFACE ( 'NONE', #80511, 9.000000000000000000 ) ;
#3611 =( NAMED_UNIT ( * ) SI_UNIT ( $, .STERADIAN. ) SOLID_ANGLE_UNIT ( ) );
#3613 = SURFACE_STYLE_USAGE ( .BOTH. , #20380 ) ;
#3614 = CARTESIAN_POINT ( 'NONE',  ( 17.64519143783728694, 294.6036040355394903, 9.884243018850950691 ) ) ;
#3615 = CIRCLE ( 'NONE', #69053, 4.000000000000007105 ) ;
#3616 = EDGE_CURVE ( 'NONE', #63378, #63934, #71810, .T. ) ;
#3617 = CARTESIAN_POINT ( 'NONE',  ( 0.000000000000000000, 80.00000000000000000, 0.000000000000000000 ) ) ;
#3618 = AXIS2_PLACEMENT_3D ( 'NONE', #103862, #46696, #81174 ) ;
#3619 = CARTESIAN_POINT ( 'NONE',  ( 0.8808064505792866372, 6.997019658119234542, -5.875704392893885242 ) ) ;
#3620 = CARTESIAN_POINT ( 'NONE',  ( 86.45121968906420307, -35.49061221823143342, 186.8395049817269467 ) ) ;
#3621 = DIRECTION ( 'NONE',  ( 0.000000000000000000, 0.000000000000000000, -1.000000000000000000 ) ) ;
#3622 = CARTESIAN_POINT ( 'NONE',  ( -2.856172004554211608, 67.80853407705139091, 5.000000000000000000 ) ) ;
#3623 = ORIENTED_EDGE ( 'NONE', *, *, #51361, .T. ) ;
#3624 = FILL_AREA_STYLE_COLOUR ( '', #42979 ) ;
#3625 = CARTESIAN_POINT ( 'NONE',  ( -43.09948196127322007, 484.9577458347781658, -0.8563396247088991275 ) ) ;
#3626 = CARTESIAN_POINT ( 'NONE',  ( -7.004291982367331748, 40.56179000230169862, -71.01843131766943884 ) ) ;
#3627 = CARTESIAN_POINT ( 'NONE',  ( 35.45036406932405981, 436.3203772529684557, 5.179456583039796946 ) ) ;
#3628 = CARTESIAN_POINT ( 'NONE',  ( -96.78478928627799860, -29.99999999999999645, 129.2502935530884258 ) ) ;
#3629 = CIRCLE ( 'NONE', #75909, 4.172000000000001485 ) ;
#3630 = CARTESIAN_POINT ( 'NONE',  ( 0.000000000000000000, 0.000000000000000000, 0.000000000000000000 ) ) ;
#3631 = CARTESIAN_POINT ( 'NONE',  ( 2.316771770790045260, -57.67120512461058013, 41.60859164704628199 ) ) ;
#3633 = FILL_AREA_STYLE ('',( #20401 ) ) ;
#3632 = CARTESIAN_POINT ( 'NONE',  ( 36.25009977769053648, 490.9522084974081508, 12.45337240579055482 ) ) ;
#3634 = EDGE_CURVE ( 'NONE', #58039, #38733, #99365, .T. ) ;
#3635 = DIRECTION ( 'NONE',  ( 0.5735764363510557073, -0.8191520442889850262, 1.003171929053516612E-16 ) ) ;
#3636 = CARTESIAN_POINT ( 'NONE',  ( -5.141721953570575820, -19.24029832776622939, 27.08744995826211976 ) ) ;
#3637 = CARTESIAN_POINT ( 'NONE',  ( -19.18847942102290105, 50.00000000000000711, 60.33013323338799694 ) ) ;
#3638 = CARTESIAN_POINT ( 'NONE',  ( -42.57704743493911081, 486.1612337113409126, 7.852296464539661791 ) ) ;
#3639 =( LENGTH_UNIT ( ) NAMED_UNIT ( * ) SI_UNIT ( .MILLI., .METRE. ) );
#3640 = CARTESIAN_POINT ( 'NONE',  ( 28.44949503909961663, -21.18434267548764893, -32.45319859116707306 ) ) ;
#3641 = EDGE_CURVE ( 'NONE', #2998, #88621, #90904, .T. ) ;
#3642 =( LENGTH_UNIT ( ) NAMED_UNIT ( * ) SI_UNIT ( .MILLI., .METRE. ) );
#3643 = CARTESIAN_POINT ( 'NONE',  ( -26.49644935441500238, -49.91621229936360749, 33.89336801046082570 ) ) ;
#3644 = CIRCLE ( 'NONE', #32915, 4.000000000000007105 ) ;
#3645 = ORIENTED_EDGE ( 'NONE', *, *, #44250, .F. ) ;
#3646 = CARTESIAN_POINT ( 'NONE',  ( 41.72175139494278540, 485.6241823541927261, -4.286260377903978736 ) ) ;
#3647 = CARTESIAN_POINT ( 'NONE',  ( -9.842473135306409660, 108.5893181711358721, 1.785129593756277222 ) ) ;
#3648 = CARTESIAN_POINT ( 'NONE',  ( -19.02339800640524814, -39.47694344028838032, 30.89218607398163741 ) ) ;
#3649 = CIRCLE ( 'NONE', #84638, 5.000000000000001776 ) ;
#3652 = EDGE_CURVE ( 'NONE', #30663, #11120, #78738, .T. ) ;
#3651 = CARTESIAN_POINT ( 'NONE',  ( 0.3379341052171724313, 36.31244600152816560, -29.71494666831264198 ) ) ;
#3650 = SURFACE_STYLE_USAGE ( .BOTH. , #52178 ) ;
#3653 = EDGE_LOOP ( 'NONE', ( #14102, #42548, #16534, #14308, #83937 ) ) ;
#3654 = CIRCLE ( 'NONE', #29552, 4.000000000000000888 ) ;
#3655 = CARTESIAN_POINT ( 'NONE',  ( 6.332254158185223858, -2.698766916914401737, -6.499999999999998224 ) ) ;
#3656 = VERTEX_POINT ( 'NONE', #69847 ) ;
#3657 = SURFACE_STYLE_USAGE ( .BOTH. , #53265 ) ;
#3658 = CONICAL_SURFACE ( 'NONE', #53537, 4.172000000000001485, 0.9599310885968750373 ) ;
#3659 = DIRECTION ( 'NONE',  ( -1.000000000000000000, 0.000000000000000000, 0.000000000000000000 ) ) ;
#3660 = DIRECTION ( 'NONE',  ( 0.000000000000000000, -1.000000000000000000, 0.000000000000000000 ) ) ;
#3661 = EDGE_LOOP ( 'NONE', ( #78997, #21671, #2858, #102892 ) ) ;
#3662 = CARTESIAN_POINT ( 'NONE',  ( 0.000000000000000000, 0.000000000000000000, 0.000000000000000000 ) ) ;
#3663 = CARTESIAN_POINT ( 'NONE',  ( 11.69514296591890634, 50.00000000000000000, -81.87740575805389653 ) ) ;
#3664 = CARTESIAN_POINT ( 'NONE',  ( 101.3732779641561734, -45.28196344093066728, 190.6380055777363509 ) ) ;
#3665 = CARTESIAN_POINT ( 'NONE',  ( -7.934996450857311423, -6.131375435274703634, -1.050865690281775899 ) ) ;
#3666 = EDGE_CURVE ( 'NONE', #98535, #91921, #35738, .T. ) ;
#3667 = ORIENTED_EDGE ( 'NONE', *, *, #92544, .T. ) ;
#3668 = ORIENTED_EDGE ( 'NONE', *, *, #81648, .T. ) ;
#3669 = ORIENTED_EDGE ( 'NONE', *, *, #72906, .T. ) ;
#3670 = CARTESIAN_POINT ( 'NONE',  ( 23.87963945136024080, 306.2497715304713211, 10.24640825507572117 ) ) ;
#3671 = EDGE_CURVE ( 'NONE', #27490, #60305, #35765, .T. ) ;
#3672 = CARTESIAN_POINT ( 'NONE',  ( -39.83997765698394034, 460.7086825730506234, 2.106271324414739077 ) ) ;
#3673 = FILL_AREA_STYLE_COLOUR ( '', #64028 ) ;
#3674 = ORIENTED_EDGE ( 'NONE', *, *, #75635, .F. ) ;
#3675 = DIRECTION ( 'NONE',  ( -1.000000000000000000, 0.000000000000000000, 0.000000000000000000 ) ) ;
#3676 = CARTESIAN_POINT ( 'NONE',  ( -6.491942716630055621, 41.63185015298623171, -70.49544021750806166 ) ) ;
#3678 = CARTESIAN_POINT ( 'NONE',  ( -94.68899862568390802, -60.00000000000000000, 1.161127854999643105 ) ) ;
#3677 = TOROIDAL_SURFACE ( 'NONE', #57078, 12.00000000000000711, 3.000000000000000000 ) ;
#3679 = DIRECTION ( 'NONE',  ( -1.000000000000000000, 0.000000000000000000, 0.000000000000000000 ) ) ;
#3680 = CARTESIAN_POINT ( 'NONE',  ( 29.75767506032096676, -59.99999999999997868, 42.91511451735463112 ) ) ;
#3681 = CARTESIAN_POINT ( 'NONE',  ( 16.39435414257611257, -5.000000000000000000, -0.9786479702816777149 ) ) ;
#3682 = CARTESIAN_POINT ( 'NONE',  ( -5.945588682461652397, 41.44588094979337001, -58.45240144925728032 ) ) ;
#3683 = CIRCLE ( 'NONE', #82901, 4.000000000000001776 ) ;
#3685 = CARTESIAN_POINT ( 'NONE',  ( 7.130718316848325244, -39.47255126203687325, 30.45876176605233709 ) ) ;
#3684 = CARTESIAN_POINT ( 'NONE',  ( -104.6655502547336738, -29.99999999999993250, 124.7729330896767408 ) ) ;
#3686 = EDGE_CURVE ( 'NONE', #36949, #61957, #53132, .T. ) ;
#3687 = FACE_OUTER_BOUND ( 'NONE', #57216, .T. ) ;
#3688 = CARTESIAN_POINT ( 'NONE',  ( -48.04142550409461165, -39.52501460404417344, 47.69088070168321281 ) ) ;
#3689 = AXIS2_PLACEMENT_3D ( 'NONE', #66062, #24577, #228 ) ;
#3690 = ORIENTED_EDGE ( 'NONE', *, *, #21568, .T. ) ;
#3691 = CARTESIAN_POINT ( 'NONE',  ( -3.860250758805052307, 18.90906293816489026, 5.839574874194349619 ) ) ;
#3692 = B_SPLINE_CURVE_WITH_KNOTS ( 'NONE', 3,
 ( #2415, #84942, #11562, #1874 ),
 .UNSPECIFIED., .F., .F.,
 ( 4, 4 ),
 ( 0.000000000000000000, 1.000000000000000000 ),
 .UNSPECIFIED. ) ;
#3693 = PRODUCT_DEFINITION_SHAPE ( 'NONE', 'NONE',  #43009 ) ;
#3694 = VERTEX_POINT ( 'NONE', #74988 ) ;
#3695 = CARTESIAN_POINT ( 'NONE',  ( 0.2950248152710058802, 7.823291154770383393, -51.71678101502384806 ) ) ;
#3696 = CARTESIAN_POINT ( 'NONE',  ( 37.96538461538461462, 4.172000000000003261, 5.109226446042759579E-16 ) ) ;
#3697 = CARTESIAN_POINT ( 'NONE',  ( 4.497431761510337189, -9.459018757489689122, -3.972160586670082871 ) ) ;
#3698 = ORIENTED_EDGE ( 'NONE', *, *, #4582, .F. ) ;
#3699 = DIRECTION ( 'NONE',  ( -0.000000000000000000, -1.000000000000000000, -0.000000000000000000 ) ) ;
#3700 = ORIENTED_EDGE ( 'NONE', *, *, #81380, .T. ) ;
#3701 = CARTESIAN_POINT ( 'NONE',  ( 108.2638972020982067, -29.99999999998661693, 151.1580933454320927 ) ) ;
#3702 = CYLINDRICAL_SURFACE ( 'NONE', #50246, 65.00000000000000000 ) ;
#3703 = CARTESIAN_POINT ( 'NONE',  ( 3.753470829068648484, -48.91069040221620412, 104.5911851069064085 ) ) ;
#3704 = EDGE_CURVE ( 'NONE', #75804, #82092, #99810, .T. ) ;
#3705 = CARTESIAN_POINT ( 'NONE',  ( -4.948897516043240685, -15.25620596204638701, -6.941429743102868422 ) ) ;
#3706 = CARTESIAN_POINT ( 'NONE',  ( -30.67950393662606956, 18.64316884711714906, 23.57730434126661834 ) ) ;
#3707 = CARTESIAN_POINT ( 'NONE',  ( 95.82107296712156597, -30.00000000000000355, 191.3050472533331572 ) ) ;
#3708 = DIRECTION ( 'NONE',  ( -1.000000000000000000, -1.224606353822377258E-16, -0.000000000000000000 ) ) ;
#3709 = EDGE_LOOP ( 'NONE', ( #17749, #71832, #29570, #5003 ) ) ;
#3710 = CIRCLE ( 'NONE', #101855, 4.000000000000000888 ) ;
#3711 = VERTEX_POINT ( 'NONE', #24368 ) ;
#3712 = ORIENTED_EDGE ( 'NONE', *, *, #88764, .F. ) ;
#3713 = CARTESIAN_POINT ( 'NONE',  ( 54.43224963993771581, -25.62617297809076078, 53.68705043744507321 ) ) ;
#3714 = CARTESIAN_POINT ( 'NONE',  ( 6.315605428199792648, 41.49696752016053836, -58.51869397248536586 ) ) ;
#3715 = CARTESIAN_POINT ( 'NONE',  ( -5.500000000000007994, 42.00000000000000000, -65.90297133633691828 ) ) ;
#3716 = VERTEX_POINT ( 'NONE', #65854 ) ;
#3717 = CARTESIAN_POINT ( 'NONE',  ( -91.11385766084679005, -38.35479298179576801, 0.5733152911744004987 ) ) ;
#3718 = ORIENTED_EDGE ( 'NONE', *, *, #26732, .F. ) ;
#3719 = CARTESIAN_POINT ( 'NONE',  ( 60.63333333333333286, 6.915964383211875250E-15, 0.000000000000000000 ) ) ;
#3720 = CARTESIAN_POINT ( 'NONE',  ( 108.2770287625986754, -38.35766625322560941, 192.2059017873136497 ) ) ;
#3721 = CARTESIAN_POINT ( 'NONE',  ( 10.63959103012515506, 13.00689338755777591, 10.01966540347888390 ) ) ;
#3722 = CARTESIAN_POINT ( 'NONE',  ( 82.44406999259793167, -37.85557453133404948, 14.49103131622133311 ) ) ;
#3723 = CARTESIAN_POINT ( 'NONE',  ( 40.84956872111840909, 369.3158774004744487, 25.50800020339859131 ) ) ;
#3724 = CARTESIAN_POINT ( 'NONE',  ( 4.956067050182457301, -15.30475822382861928, -6.874165724332473637 ) ) ;
#3725 = CARTESIAN_POINT ( 'NONE',  ( -23.21751746555280249, 25.98869614573808207, -30.70617127781034839 ) ) ;
#3726 = VECTOR ( 'NONE', #13923, 1000.000000000000000 ) ;
#3727 = DIRECTION ( 'NONE',  ( -0.5166563581655519988, 0.4014477553984793223, 0.7562446080816918048 ) ) ;
#3728 = CARTESIAN_POINT ( 'NONE',  ( 9.240146679350036862, 139.9709698506905795, 5.000000000000307310 ) ) ;
#3729 = ORIENTED_EDGE ( 'NONE', *, *, #63845, .F. ) ;
#3730 = EDGE_CURVE ( 'NONE', #2343, #72931, #89073, .T. ) ;
#3731 = CARTESIAN_POINT ( 'NONE',  ( -9.852211596319794040, 15.56091200510340755, -1.749942564367551912 ) ) ;
#3732 = CARTESIAN_POINT ( 'NONE',  ( 15.50702112914487785, 36.95515616017750204, -23.25462944313571967 ) ) ;
#3733 = CARTESIAN_POINT ( 'NONE',  ( 0.000000000000000000, 0.000000000000000000, -8.553285714285713937 ) ) ;
#3734 = ORIENTED_EDGE ( 'NONE', *, *, #83507, .F. ) ;
#3735 = CARTESIAN_POINT ( 'NONE',  ( -27.78400705216732902, 308.4281219000443457, -8.192438691479090096 ) ) ;
#3736 = CARTESIAN_POINT ( 'NONE',  ( -39.47463750696404361, 315.8169378728001675, 7.009586823238445952 ) ) ;
#3737 = DIRECTION ( 'NONE',  ( -1.000000000000000000, -0.000000000000000000, -0.000000000000000000 ) ) ;
#3738 = DIRECTION ( 'NONE',  ( 0.000000000000000000, 0.000000000000000000, 1.000000000000000000 ) ) ;
#3739 = CARTESIAN_POINT ( 'NONE',  ( -5.656854249492381470, -23.56249999999999289, 5.656854249492379694 ) ) ;
#3740 = CARTESIAN_POINT ( 'NONE',  ( 40.60998584173464820, -26.59100105118786317, 36.33122594000368366 ) ) ;
#3741 = STYLED_ITEM ( 'NONE', ( #69471 ), #19502 ) ;
#3742 = ADVANCED_FACE ( 'NONE', ( #49661 ), #1675, .T. ) ;
#3743 = AXIS2_PLACEMENT_3D ( 'NONE', #61742, #78419, #44479 ) ;
#3744 = PRODUCT_DEFINITION_SHAPE ( 'NONE', 'NONE',  #106804 ) ;
#3745 = CARTESIAN_POINT ( 'NONE',  ( -7.500000000000000000, 4.330127018922188320, -0.9999999999999904521 ) ) ;
#3746 = ORIENTED_EDGE ( 'NONE', *, *, #94758, .F. ) ;
#3747 = CARTESIAN_POINT ( 'NONE',  ( 84.56613401024672783, -39.39959700902200979, 181.6695324457707557 ) ) ;
#3748 = CARTESIAN_POINT ( 'NONE',  ( 8.000000000000000000, 9.797174393178825657E-16, -11.12471428571428689 ) ) ;
#3749 = ORIENTED_EDGE ( 'NONE', *, *, #105871, .F. ) ;
#3750 = CARTESIAN_POINT ( 'NONE',  ( -84.82029566994467018, -37.82138604335175103, 44.26793484215674113 ) ) ;
#3751 = CARTESIAN_POINT ( 'NONE',  ( 6.162888688655344893, 3.752776749732562589, -6.500000000000000888 ) ) ;
#3752 = CARTESIAN_POINT ( 'NONE',  ( -9.891797161801507698, -3.000000000000002665, -73.72381496649796873 ) ) ;
#3753 = DIRECTION ( 'NONE',  ( -1.000000000000000000, 0.000000000000000000, 0.000000000000000000 ) ) ;
#3754 = CARTESIAN_POINT ( 'NONE',  ( -4.429919089265682786, -21.58035052029104151, -38.54841997176323787 ) ) ;
#3755 = B_SPLINE_CURVE_WITH_KNOTS ( 'NONE', 3,
 ( #61787, #31019, #30474, #38053, #78999, #6158, #55755, #39091, #36988, #13721, #55239, #78468, #4589, #63898, #37524, #88687, #70911, #71971, #70388, #88163, #103286, #29434, #29947, #14247, #62831, #47153, #69856, #62310, #95201, #79526, #95722, #80047, #45063, #96787, #77946, #21861, #22918, #28913, #94682, #21334, #13186, #54703, #87636, #46630, #5640, #72495, #56287, #32602, #16932, #64939, #48732, #25035, #32064, #56832, #57890, #89756, #14783, #41722, #15852, #97295, #15321, #33128, #73540, #23451, #81623, #8818, #99402, #25586, #106445, #33650, #23990, #49267, #48208, #97832, #7748, #90277, #74607, #58445, #65474, #89224, #80576, #57356, #64426, #40658, #81111, #16378 ),
 .UNSPECIFIED., .F., .F.,
 ( 4, 2, 2, 2, 2, 2, 2, 2, 2, 2, 2, 2, 2, 2, 2, 2, 2, 2, 2, 2, 2, 2, 2, 2, 2, 2, 2, 2, 2, 2, 2, 2, 2, 2, 2, 2, 2, 2, 2, 2, 2, 2, 4 ),
 ( 0.02397150411713972612, 0.02592718538678167456, 0.02788286665642362300, 0.02983854792606556797, 0.03081638856088654219, 0.03179422919570751294, 0.03374991046534946137, 0.03570559173499140287, 0.03766127300463335131, 0.03863911363945431859, 0.03961695427427529281, 0.04059479490909626009, 0.04157263554391722737, 0.04352831681355916194, 0.04450615744838013615, 0.04548399808320111037, 0.04743967935284304493, 0.04939536062248497950, 0.05135104189212691406, 0.05232888252694787440, 0.05330672316176883474, 0.05428456379658980202, 0.05526240443141076236, 0.05721808570105269692, 0.05819592633587366420, 0.05917376697069462455, 0.06112944824033656605, 0.06308512950997849367, 0.06504081077962042823, 0.06699649204926236279, 0.06895217331890429735, 0.06993001395372527851, 0.07090785458854624579, 0.07286353585818819423, 0.07481921712783012879, 0.07677489839747206335, 0.07873057966711399791, 0.07970842030193497907, 0.08068626093675593247, 0.08264194220639786703, 0.08361978284121884819, 0.08459762347603982935, 0.08655330474568176391 ),
 .UNSPECIFIED. ) ;
#3756 = AXIS2_PLACEMENT_3D ( 'NONE', #79920, #6028, #93995 ) ;
#3757 = CARTESIAN_POINT ( 'NONE',  ( 21.33042875005117267, -59.99999999999998579, 40.41048302378931822 ) ) ;
#3758 =( GEOMETRIC_REPRESENTATION_CONTEXT ( 3 ) GLOBAL_UNCERTAINTY_ASSIGNED_CONTEXT ( ( #57126 ) ) GLOBAL_UNIT_ASSIGNED_CONTEXT ( ( #84072, #9103, #100777 ) ) REPRESENTATION_CONTEXT ( 'NONE', 'WORKASPACE' ) );
#3759 = CARTESIAN_POINT ( 'NONE',  ( -87.14767027655014431, -37.99999999998310329, 189.0874028505847662 ) ) ;
#3760 = CARTESIAN_POINT ( 'NONE',  ( 51.37606068035684359, -29.89807750398198394, 48.95549095964486241 ) ) ;
#3762 = CARTESIAN_POINT ( 'NONE',  ( -11.44045018991158003, 13.03826302799688186, 10.01684603989913747 ) ) ;
#3761 = FACE_OUTER_BOUND ( 'NONE', #78513, .T. ) ;
#3763 = CARTESIAN_POINT ( 'NONE',  ( 3.010187908141165103, 299.5653876365747692, -10.00571708631404810 ) ) ;
#3764 = LINE ( 'NONE', #42609, #44597 ) ;
#3765 = SURFACE_STYLE_FILL_AREA ( #93303 ) ;
#3766 = CARTESIAN_POINT ( 'NONE',  ( -9.819056950928635175, 294.6481068335448299, 1.893705519456528652 ) ) ;
#3767 = CARTESIAN_POINT ( 'NONE',  ( 6.169949891408088583, 6.308465495018137581, -2.073417244832098216 ) ) ;
#3768 = ORIENTED_EDGE ( 'NONE', *, *, #2418, .T. ) ;
#3769 = CARTESIAN_POINT ( 'NONE',  ( 6.500000000000007105, -3.752776749732581685, -0.7999999999999977129 ) ) ;
#3770 = CARTESIAN_POINT ( 'NONE',  ( -17.49999999999997513, 51.99872764530893932, 60.15967750826234806 ) ) ;
#3771 = EDGE_LOOP ( 'NONE', ( #80434, #74263 ) ) ;
#3772 = CARTESIAN_POINT ( 'NONE',  ( -14.25073637597874665, 0.6890215015240969132, 14.98521214194409445 ) ) ;
#3773 =( NAMED_UNIT ( * ) SI_UNIT ( $, .STERADIAN. ) SOLID_ANGLE_UNIT ( ) );
#3776 = EDGE_CURVE ( 'NONE', #106154, #95649, #42564, .T. ) ;
#3775 = CARTESIAN_POINT ( 'NONE',  ( 3.088936762904795241, -21.77034166220828837, -30.49860928398698690 ) ) ;
#3774 = CARTESIAN_POINT ( 'NONE',  ( 9.645512969475877441, 253.0110315067572913, -2.645801731561389314 ) ) ;
#3777 = VERTEX_POINT ( 'NONE', #74463 ) ;
#3778 = DIRECTION ( 'NONE',  ( 0.000000000000000000, 0.000000000000000000, -1.000000000000000000 ) ) ;
#3779 = FILL_AREA_STYLE ('',( #77667 ) ) ;
#3780 = ORIENTED_EDGE ( 'NONE', *, *, #59664, .F. ) ;
#3781 = CARTESIAN_POINT ( 'NONE',  ( 30.42742517972242666, 7.740625494265016115, -41.86256052107409431 ) ) ;
#3782 = FACE_OUTER_BOUND ( 'NONE', #91838, .T. ) ;
#3783 = CARTESIAN_POINT ( 'NONE',  ( -92.23621273581470348, -60.00000000000000000, 2.391921308898584453 ) ) ;
#3784 = ORIENTED_EDGE ( 'NONE', *, *, #54002, .F. ) ;
#3785 = CARTESIAN_POINT ( 'NONE',  ( -1.797870618338381465, 41.33266196706689755, -58.72278032361812450 ) ) ;
#3786 = DIRECTION ( 'NONE',  ( 1.000000000000000000, 0.000000000000000000, 0.000000000000000000 ) ) ;
#3787 = CARTESIAN_POINT ( 'NONE',  ( -3.433097520132042835, -0.8249796456130259470, 103.8029795887030815 ) ) ;
#3789 = SURFACE_STYLE_USAGE ( .BOTH. , #69591 ) ;
#3788 = FACE_OUTER_BOUND ( 'NONE', #87584, .T. ) ;
#3790 = CARTESIAN_POINT ( 'NONE',  ( -82.17221523199479805, -46.46580854769393909, 173.2050682668972854 ) ) ;
#3791 = EDGE_LOOP ( 'NONE', ( #104575, #33041, #72543, #65147 ) ) ;
#3792 = DIRECTION ( 'NONE',  ( 0.000000000000000000, -1.000000000000000000, 0.000000000000000000 ) ) ;
#3793 = ORIENTED_EDGE ( 'NONE', *, *, #85701, .T. ) ;
#3794 = AXIS2_PLACEMENT_3D ( 'NONE', #9552, #27400, #67812 ) ;
#3795 = ORIENTED_EDGE ( 'NONE', *, *, #13580, .F. ) ;
#3796 = CARTESIAN_POINT ( 'NONE',  ( -14.22021666642130455, -5.000000000000000000, 8.714242330525310720 ) ) ;
#3797 = EDGE_CURVE ( 'NONE', #57829, #3104, #30563, .T. ) ;
#3798 =( NAMED_UNIT ( * ) PLANE_ANGLE_UNIT ( ) SI_UNIT ( $, .RADIAN. ) );
#3799 = ORIENTED_EDGE ( 'NONE', *, *, #32312, .T. ) ;
#3800 = CARTESIAN_POINT ( 'NONE',  ( -91.04381008827128596, -57.66401771476134996, -20.86613467659797649 ) ) ;
#3801 = CARTESIAN_POINT ( 'NONE',  ( 7.212994264445062420, -12.01711344340039567, 3.463766307298584923 ) ) ;
#3802 = CARTESIAN_POINT ( 'NONE',  ( 28.17977184163764193, 5.000000000000003553, 0.000000000000000000 ) ) ;
#3803 = CARTESIAN_POINT ( 'NONE',  ( -9.989113211954167681, 101.0270072645100754, 0.5334031035449037228 ) ) ;
#3804 = SURFACE_STYLE_FILL_AREA ( #77695 ) ;
#3805 = CARTESIAN_POINT ( 'NONE',  ( -4.582575694955840717, 15.00000000000000000, -10.00000000000000000 ) ) ;
#3806 = CIRCLE ( 'NONE', #51990, 4.000000000000003553 ) ;
#3807 = CARTESIAN_POINT ( 'NONE',  ( 93.17370000506844008, -59.99999999999994316, -17.95777172718301173 ) ) ;
#3808 = EDGE_CURVE ( 'NONE', #18205, #51545, #103887, .T. ) ;
#3809 = AXIS2_PLACEMENT_3D ( 'NONE', #79098, #5221, #61344 ) ;
#3810 = CARTESIAN_POINT ( 'NONE',  ( -94.89844962927027439, -60.00000000000001421, 205.0338773334991060 ) ) ;
#3811 = CARTESIAN_POINT ( 'NONE',  ( -54.48342840945926469, -56.85295987972201459, 66.24415397588745691 ) ) ;
#3812 = ORIENTED_EDGE ( 'NONE', *, *, #32330, .T. ) ;
#3813 = ORIENTED_EDGE ( 'NONE', *, *, #37842, .F. ) ;
#3814 = CARTESIAN_POINT ( 'NONE',  ( -102.9797039820129072, -45.26540897849420020, 185.6133583916170267 ) ) ;
#3815 = LINE ( 'NONE', #36753, #62674 ) ;
#3816 = CARTESIAN_POINT ( 'NONE',  ( -5.455379837882870397, 51.31468677425149849, 8.531152949374572358 ) ) ;
#3817 = EDGE_LOOP ( 'NONE', ( #102248, #67837, #10668 ) ) ;
#3818 = CARTESIAN_POINT ( 'NONE',  ( 19.49389532278797432, 49.99942041210562849, 60.03759455525020883 ) ) ;
#3819 =( NAMED_UNIT ( * ) SI_UNIT ( $, .STERADIAN. ) SOLID_ANGLE_UNIT ( ) );
#3820 = CARTESIAN_POINT ( 'NONE',  ( 33.00000000000000000, 450.0000000000002274, 13.20242257375370976 ) ) ;
#3821 = CARTESIAN_POINT ( 'NONE',  ( 2.977408999572650927, -16.25000000204838813, -7.188101187500001821 ) ) ;
#3822 = EDGE_CURVE ( 'NONE', #34804, #14145, #76595, .T. ) ;
#3823 = CARTESIAN_POINT ( 'NONE',  ( -4.359081798055807866, -66.52598855954795454, 13.14323235564549819 ) ) ;
#3824 = CARTESIAN_POINT ( 'NONE',  ( 16.08349330513380337, 1.593028355512270962E-15, 0.000000000000000000 ) ) ;
#3825 = DIRECTION ( 'NONE',  ( 1.000000000000000000, 1.224606353822377258E-16, 0.000000000000000000 ) ) ;
#3826 = CARTESIAN_POINT ( 'NONE',  ( -22.20318009218133071, 295.0333587257888439, 9.975590323731541531 ) ) ;
#3827 = CARTESIAN_POINT ( 'NONE',  ( -5.290067270632214047, 53.47475093287474124, -8.531152949374821048 ) ) ;
#3828 = CARTESIAN_POINT ( 'NONE',  ( -9.755167981113400444, 8.162422641044738469, 0.000000000000000000 ) ) ;
#3829 = CARTESIAN_POINT ( 'NONE',  ( -16.32471966984383371, 45.71573795642331106, -6.626903219538490930 ) ) ;
#3830 = CARTESIAN_POINT ( 'NONE',  ( -7.500000000000002665, 1.559114133231479071, -21.99325844590496004 ) ) ;
#3831 = UNCERTAINTY_MEASURE_WITH_UNIT (LENGTH_MEASURE( 1.000000000000000082E-05 ), #29524, 'distance_accuracy_value', 'NONE');
#3832 = CARTESIAN_POINT ( 'NONE',  ( -27.39369750312375729, -56.87079340815250106, 35.32494246014085348 ) ) ;
#3833 = COLOUR_RGB ( '', 0.40784314, 0.44705882, 0.49803922) ;
#3834 = CARTESIAN_POINT ( 'NONE',  ( 32.87517070013015541, 485.0717976019059847, 1.466424316699966202 ) ) ;
#3835 = CARTESIAN_POINT ( 'NONE',  ( 47.01967600138543446, -39.52544382475996798, 46.22899997382759096 ) ) ;
#3836 = EDGE_LOOP ( 'NONE', ( #20379, #94806 ) ) ;
#3837 = AXIS2_PLACEMENT_3D ( 'NONE', #75170, #8850, #41754 ) ;
#3838 = FACE_OUTER_BOUND ( 'NONE', #53178, .T. ) ;
#3839 = CARTESIAN_POINT ( 'NONE',  ( -0.7852806286178579676, 46.11106221562390317, 16.51405864586197225 ) ) ;
#3840 = VECTOR ( 'NONE', #104714, 1000.000000000000000 ) ;
#3841 = CARTESIAN_POINT ( 'NONE',  ( -91.91261139602251262, -38.50135474963098403, 200.9741384565720637 ) ) ;
#3842 = ORIENTED_EDGE ( 'NONE', *, *, #34582, .T. ) ;
#3843 = DIRECTION ( 'NONE',  ( 0.000000000000000000, 0.000000000000000000, 1.000000000000000000 ) ) ;
#3844 = CARTESIAN_POINT ( 'NONE',  ( 13.45742156688652713, 5.393973166499471006, -6.521729985601480095 ) ) ;
#3845 = CARTESIAN_POINT ( 'NONE',  ( -49.07509721567202376, 8.836758769845310724, -14.91787708872438856 ) ) ;
#3846 = PRESENTATION_STYLE_ASSIGNMENT (( #62614 ) ) ;
#3847 = CARTESIAN_POINT ( 'NONE',  ( 4.872636759907720716, 41.00341855746686548, -70.74912513459382524 ) ) ;
#3848 = CARTESIAN_POINT ( 'NONE',  ( 0.000000000000000000, 0.000000000000000000, 8.000000000000000000 ) ) ;
#3849 = CARTESIAN_POINT ( 'NONE',  ( 5.000000000000000000, -51.57174003072816504, 8.340209667212416633 ) ) ;
#3851 = VECTOR ( 'NONE', #53716, 1000.000000000000000 ) ;
#3850 = CARTESIAN_POINT ( 'NONE',  ( 0.000000000000000000, 0.000000000000000000, -6.123524522925831270 ) ) ;
#3852 = CARTESIAN_POINT ( 'NONE',  ( 103.5957000756554578, -60.00000000000001421, 200.2558930352217317 ) ) ;
#3853 = CARTESIAN_POINT ( 'NONE',  ( -6.928203230275508773, -65.00000000000000000, 4.000000000000002665 ) ) ;
#3854 = VERTEX_POINT ( 'NONE', #10267 ) ;
#3855 = ADVANCED_FACE ( 'NONE', ( #101937 ), #12387, .F. ) ;
#3856 = CARTESIAN_POINT ( 'NONE',  ( 7.619753052866895970, 33.17451502807172403, -2.447276542590444137 ) ) ;
#3857 = CARTESIAN_POINT ( 'NONE',  ( -81.34740007214244883, -30.00000000000000711, -10.45134090017297446 ) ) ;
#3858 = ORIENTED_EDGE ( 'NONE', *, *, #61215, .F. ) ;
#3860 = CARTESIAN_POINT ( 'NONE',  ( 32.13020926079881434, 464.8240734303054182, 14.61769217561763945 ) ) ;
#3859 = PRESENTATION_STYLE_ASSIGNMENT (( #19553 ) ) ;
#3861 = DIRECTION ( 'NONE',  ( 0.5735764363510490460, 0.8191520442889896891, 0.000000000000000000 ) ) ;
#3862 = CARTESIAN_POINT ( 'NONE',  ( 46.02200000000003399, 6.123233995736772199E-16, -5.000000000000004441 ) ) ;
#3863 = CARTESIAN_POINT ( 'NONE',  ( 2.977408999572651815, -15.31250000204838457, 7.188101187500000933 ) ) ;
#3864 = CARTESIAN_POINT ( 'NONE',  ( 6.043427762770655853, -5.000000000000002665, -95.48543666094731464 ) ) ;
#3865 = EDGE_CURVE ( 'NONE', #23643, #26151, #77064, .T. ) ;
#3866 = EDGE_CURVE ( 'NONE', #91921, #17636, #30585, .T. ) ;
#3867 = LINE ( 'NONE', #46444, #19090 ) ;
#3869 = VERTEX_POINT ( 'NONE', #44790 ) ;
#3868 = CARTESIAN_POINT ( 'NONE',  ( -32.64206520361308606, 464.2415374745227155, 8.403253426436839035 ) ) ;
#3870 = CARTESIAN_POINT ( 'NONE',  ( 83.58220805307611556, -35.98891138001182810, 169.8156018569172545 ) ) ;
#3871 = DIRECTION ( 'NONE',  ( 0.000000000000000000, 0.000000000000000000, 1.000000000000000000 ) ) ;
#3872 = DIRECTION ( 'NONE',  ( -1.000000000000000000, -1.224606353822377258E-16, -0.000000000000000000 ) ) ;
#3873 = ORIENTED_EDGE ( 'NONE', *, *, #76722, .F. ) ;
#3874 = VECTOR ( 'NONE', #73356, 1000.000000000000000 ) ;
#3875 = CARTESIAN_POINT ( 'NONE',  ( -21.24460900603666857, 302.9489078580693331, -9.979273875210839861 ) ) ;
#3876 = SURFACE_STYLE_USAGE ( .BOTH. , #45405 ) ;
#3877 = DIRECTION ( 'NONE',  ( 1.000000000000000000, 0.000000000000000000, 0.000000000000000000 ) ) ;
#3878 = AXIS2_PLACEMENT_3D ( 'NONE', #4173, #23030, #79637 ) ;
#3879 = DIRECTION ( 'NONE',  ( 0.000000000000000000, 0.000000000000000000, -1.000000000000000000 ) ) ;
#3880 = CARTESIAN_POINT ( 'NONE',  ( -3.312116827214752676E-14, 12.91535575336970965, 51.75000000000017764 ) ) ;
#3881 = EDGE_CURVE ( 'NONE', #55300, #30328, #51787, .T. ) ;
#3882 = VERTEX_POINT ( 'NONE', #36725 ) ;
#3883 = CARTESIAN_POINT ( 'NONE',  ( -4.284822031654912600, -48.90716638558775031, 104.4267991316945228 ) ) ;
#3884 = CARTESIAN_POINT ( 'NONE',  ( 74.56127108291157413, 6.975173280561618775E-15, 0.000000000000000000 ) ) ;
#3886 = ADVANCED_FACE ( 'NONE', ( #11316 ), #3254, .F. ) ;
#3885 = CARTESIAN_POINT ( 'NONE',  ( 6.249999999999998224, 8.000000000000000000, 0.000000000000000000 ) ) ;
#3888 = CARTESIAN_POINT ( 'NONE',  ( 0.000000000000000000, 0.000000000000000000, 0.000000000000000000 ) ) ;
#3887 = CARTESIAN_POINT ( 'NONE',  ( 22.33349330513380693, 1.593028355512270962E-15, 0.000000000000000000 ) ) ;
#3889 = CARTESIAN_POINT ( 'NONE',  ( 5.082755093536325930, -26.46875000204838813, -5.082755093536325042 ) ) ;
#3890 = CARTESIAN_POINT ( 'NONE',  ( 64.78349330513380266, 6.975173280561618775E-15, 0.000000000000000000 ) ) ;
#3891 = CARTESIAN_POINT ( 'NONE',  ( 2.583982984169515440, -5.000000000000000000, -9.743117168495876612 ) ) ;
#3892 = CARTESIAN_POINT ( 'NONE',  ( 7.360438360658586809, -5.000000000000000000, -75.39006186636561324 ) ) ;
#3893 = CONTEXT_DEPENDENT_SHAPE_REPRESENTATION ( #57641, #37373 ) ;
#3894 = ORIENTED_EDGE ( 'NONE', *, *, #39756, .T. ) ;
#3895 = CARTESIAN_POINT ( 'NONE',  ( -36.12201691787056035, 490.9181190026608306, 12.43842860963000696 ) ) ;
#3896 = CARTESIAN_POINT ( 'NONE',  ( -7.989277284034971949, 50.32447066040694494, -4.999999999999999112 ) ) ;
#3897 =( BOUNDED_SURFACE ( )  B_SPLINE_SURFACE ( 3, 2, ( 
 ( #45994, #46513, #56161 ),
 ( #71313, #6568, #6039 ),
 ( #55117, #30896, #72375 ),
 ( #30353, #70794, #79409 ) ),
 .UNSPECIFIED., .F., .F., .F. ) 
 B_SPLINE_SURFACE_WITH_KNOTS ( ( 4, 4 ),
 ( 3, 3 ),
 ( -1.821459649775647449E-17, 0.0004290382097840233990 ),
 ( 0.000000000000000000, 1.000000000000000000 ),
 .UNSPECIFIED. ) 
 GEOMETRIC_REPRESENTATION_ITEM ( )  RATIONAL_B_SPLINE_SURFACE ( (
 ( 1.000000000000000000, 0.7888522786294254185, 1.000000000000000000),
 ( 1.000000000000000000, 0.7909287578650892048, 1.000000000000000000),
 ( 1.000000000000000000, 0.7929954621607017140, 1.000000000000000000),
 ( 1.000000000000000000, 0.7950530193019101910, 1.000000000000000000) ) ) 
 REPRESENTATION_ITEM ( '' )  SURFACE ( )  );
#3898 = AXIS2_PLACEMENT_3D ( 'NONE', #21541, #54376, #80797 ) ;
#3899 = DIRECTION ( 'NONE',  ( 0.000000000000000000, -1.000000000000000000, 0.000000000000000000 ) ) ;
#3900 = PRESENTATION_LAYER_ASSIGNMENT (  '', '', ( #74473 ) ) ;
#3901 = VERTEX_POINT ( 'NONE', #4311 ) ;
#3902 = CARTESIAN_POINT ( 'NONE',  ( -7.315365623647276827, 52.17029336129217398, -2.633652021638295704 ) ) ;
#3903 = CARTESIAN_POINT ( 'NONE',  ( 4.707696486722537266, 48.00000000000000000, -99.43546650846083423 ) ) ;
#3904 = CIRCLE ( 'NONE', #77970, 2.999999999999999112 ) ;
#3905 = VERTEX_POINT ( 'NONE', #69064 ) ;
#3906 = CARTESIAN_POINT ( 'NONE',  ( -27.92784172790835839, 34.23327901736961820, 9.751711673318832041 ) ) ;
#3907 = CARTESIAN_POINT ( 'NONE',  ( -0.2984172751366608867, 7.825053155909972524, -51.71602382706492307 ) ) ;
#3908 = CARTESIAN_POINT ( 'NONE',  ( 9.645512969475854348, 101.9889684932427514, -2.645801731561389758 ) ) ;
#3909 = UNCERTAINTY_MEASURE_WITH_UNIT (LENGTH_MEASURE( 1.000000000000000082E-05 ), #80965, 'distance_accuracy_value', 'NONE');
#3910 = CARTESIAN_POINT ( 'NONE',  ( -108.5746306176662301, -59.99999999999999289, 194.5749993497246635 ) ) ;
#3911 = CARTESIAN_POINT ( 'NONE',  ( 19.50000000000126832, 49.99999999999980815, 59.82664205501161092 ) ) ;
#3912 = CARTESIAN_POINT ( 'NONE',  ( 19.38370409691060203, 304.7210516941073024, -9.027791792081334421 ) ) ;
#3913 = CARTESIAN_POINT ( 'NONE',  ( 44.17836536378482748, 435.2619773020558682, 14.65562696767865170 ) ) ;
#3914 = CARTESIAN_POINT ( 'NONE',  ( 17.08457507770788908, 34.19635311626529983, -24.27368305446641727 ) ) ;
#3915 = B_SPLINE_CURVE_WITH_KNOTS ( 'NONE', 3,
 ( #96102, #6535, #87488, #71281, #23289, #95571, #62166, #47530 ),
 .UNSPECIFIED., .F., .F.,
 ( 4, 2, 2, 4 ),
 ( 0.000000000000000000, 0.5000000000000000000, 0.7500000000000000000, 1.000000000000000000 ),
 .UNSPECIFIED. ) ;
#3916 = CARTESIAN_POINT ( 'NONE',  ( -84.96410193910523390, -32.32224907966426741, 177.2623289152436996 ) ) ;
#3917 = CARTESIAN_POINT ( 'NONE',  ( 42.97360691268208654, 41.50767547277785496, -51.42105803120703911 ) ) ;
#3918 = ORIENTED_EDGE ( 'NONE', *, *, #93636, .T. ) ;
#3919 = CARTESIAN_POINT ( 'NONE',  ( -9.954785814282052669, 46.18621183893549897, -12.94079623093657183 ) ) ;
#3920 = EDGE_CURVE ( 'NONE', #77684, #98423, #4778, .T. ) ;
#3921 = CARTESIAN_POINT ( 'NONE',  ( 1.000000000000000222, -10.50453238069598960, -12.19598953690542231 ) ) ;
#3922 = CARTESIAN_POINT ( 'NONE',  ( -82.46448073435685444, -37.83313065937878861, 8.731117919795149618 ) ) ;
#3923 = CARTESIAN_POINT ( 'NONE',  ( -3.684569285721631005, -8.676863831078836853, -12.27927943165845193 ) ) ;
#3924 = CARTESIAN_POINT ( 'NONE',  ( -2.983112692022612311, 50.82233998752811743, -5.000000000000000888 ) ) ;
#3925 = CARTESIAN_POINT ( 'NONE',  ( 0.000000000000000000, 6.123233995736770227E-16, -5.000000000000002665 ) ) ;
#3926 = CARTESIAN_POINT ( 'NONE',  ( 10.04205104292330475, 18.64316884715076839, 37.36680950592799633 ) ) ;
#3927 = EDGE_CURVE ( 'NONE', #21000, #104615, #20305, .T. ) ;
#3928 = CARTESIAN_POINT ( 'NONE',  ( 75.56757797150578426, -14.21045842199434439, 141.5459454228812319 ) ) ;
#3929 = CARTESIAN_POINT ( 'NONE',  ( 0.000000000000000000, 60.33964880548970200, -13.06657876680918662 ) ) ;
#3930 = EDGE_CURVE ( 'NONE', #54691, #54576, #96518, .T. ) ;
#3931 = CARTESIAN_POINT ( 'NONE',  ( -94.49493096136262693, -59.99999999999997158, -13.89135613746328701 ) ) ;
#3932 = CARTESIAN_POINT ( 'NONE',  ( -64.47854645191701195, -42.96210629927422531, 86.48441421252113059 ) ) ;
#3933 = ORIENTED_EDGE ( 'NONE', *, *, #43928, .F. ) ;
#3934 = CARTESIAN_POINT ( 'NONE',  ( 111.5326445490954228, -59.99999999999995737, 193.8609935400126005 ) ) ;
#3935 = CARTESIAN_POINT ( 'NONE',  ( 19.58390667205444657, -59.99999999998016165, 42.52723830633056679 ) ) ;
#3936 = EDGE_LOOP ( 'NONE', ( #51030, #14680, #30824, #22393 ) ) ;
#3937 = CARTESIAN_POINT ( 'NONE',  ( 13.42014116845449934, -55.04332197544540151, 30.98782490008220236 ) ) ;
#3938 = CARTESIAN_POINT ( 'NONE',  ( 2.977408999572652260, -22.81250000204838813, 7.188101187500000044 ) ) ;
#3939 = AXIS2_PLACEMENT_3D ( 'NONE', #970, #66821, #9622 ) ;
#3940 = FACE_BOUND ( 'NONE', #47503, .T. ) ;
#3941 = ORIENTED_EDGE ( 'NONE', *, *, #87900, .F. ) ;
#3942 = LINE ( 'NONE', #19640, #81969 ) ;
#3943 = ORIENTED_EDGE ( 'NONE', *, *, #25237, .T. ) ;
#3944 = DIRECTION ( 'NONE',  ( 0.000000000000000000, -1.000000000000000000, 0.000000000000000000 ) ) ;
#3945 = AXIS2_PLACEMENT_3D ( 'NONE', #41279, #83864, #82265 ) ;
#3946 = CARTESIAN_POINT ( 'NONE',  ( -44.37565758691186346, -59.99999999999997868, -38.94428251963324072 ) ) ;
#3947 = CARTESIAN_POINT ( 'NONE',  ( -10.45131719755852728, 43.22378321881971175, 15.40779740156164479 ) ) ;
#3948 = CARTESIAN_POINT ( 'NONE',  ( -1.320432766682874540E-15, -31.90625000204838813, 7.188101187500000044 ) ) ;
#3949 = EDGE_CURVE ( 'NONE', #45750, #44463, #39199, .T. ) ;
#3950 = DIRECTION ( 'NONE',  ( -1.000000000000000000, -1.224606353822377258E-16, -0.000000000000000000 ) ) ;
#3951 = AXIS2_PLACEMENT_3D ( 'NONE', #9451, #90393, #49382 ) ;
#3952 = DIRECTION ( 'NONE',  ( -1.000000000000000000, -1.224606353822377258E-16, -0.000000000000000000 ) ) ;
#3953 = CARTESIAN_POINT ( 'NONE',  ( 1.469576158976823356E-15, 50.00000000000000000, -73.00000000000001421 ) ) ;
#3954 = CARTESIAN_POINT ( 'NONE',  ( -7.619701877737479201, 108.1744215953277006, -2.447562251315980486 ) ) ;
#3955 = CARTESIAN_POINT ( 'NONE',  ( 39.36202273480931524, 437.3280700035287509, 5.163426856674600884 ) ) ;
#3956 = ORIENTED_EDGE ( 'NONE', *, *, #7199, .F. ) ;
#3957 = CARTESIAN_POINT ( 'NONE',  ( 4.188755055078403622, -1.571875576994826718, 102.8981131900555113 ) ) ;
#3958 = CIRCLE ( 'NONE', #15953, 5.000000000000001776 ) ;
#3960 = CARTESIAN_POINT ( 'NONE',  ( 34.65411374088593988, -18.71485586463119333, 31.05683867045650715 ) ) ;
#3959 = CARTESIAN_POINT ( 'NONE',  ( -3.352941176470584761, -48.79941684889506348, 104.5794940929807524 ) ) ;
#3961 = CARTESIAN_POINT ( 'NONE',  ( 15.50035291838412199, -4.285714285712356464, 20.16952962162429941 ) ) ;
#3962 = ORIENTED_EDGE ( 'NONE', *, *, #29073, .F. ) ;
#3963 = CARTESIAN_POINT ( 'NONE',  ( 36.69878522478096983, 484.6513904560040373, -2.872853880322673970 ) ) ;
#3965 = DIRECTION ( 'NONE',  ( 0.5735764363510462704, 0.8191520442889915765, 0.000000000000000000 ) ) ;
#3964 = DIRECTION ( 'NONE',  ( 0.000000000000000000, 0.000000000000000000, 1.000000000000000000 ) ) ;
#3966 = DIRECTION ( 'NONE',  ( 0.000000000000000000, -1.000000000000000000, 0.000000000000000000 ) ) ;
#3967 = CARTESIAN_POINT ( 'NONE',  ( -43.98494780545747318, 485.1299400072931007, -0.2561545286475674366 ) ) ;
#3968 =( REPRESENTATION_RELATIONSHIP ('NONE','NONE', #69581, #70207 ) REPRESENTATION_RELATIONSHIP_WITH_TRANSFORMATION ( #100983 )SHAPE_REPRESENTATION_RELATIONSHIP( ) );
#3969 = CARTESIAN_POINT ( 'NONE',  ( -7.500000000000001776, -3.000000000000000000, -36.97043916959987087 ) ) ;
#3970 = CARTESIAN_POINT ( 'NONE',  ( 0.000000000000000000, 2.999999999999993339, 0.000000000000000000 ) ) ;
#3971 = CYLINDRICAL_SURFACE ( 'NONE', #82703, 5.000000000000002665 ) ;
#3972 =( LENGTH_UNIT ( ) NAMED_UNIT ( * ) SI_UNIT ( .MILLI., .METRE. ) );
#3973 = EDGE_LOOP ( 'NONE', ( #75321, #23575, #17516, #4423 ) ) ;
#3974 = CARTESIAN_POINT ( 'NONE',  ( 92.01456011641386112, -59.99999999999999289, 18.73852019385518020 ) ) ;
#3975 = DIRECTION ( 'NONE',  ( 0.000000000000000000, -1.000000000000000000, 0.000000000000000000 ) ) ;
#3976 = CYLINDRICAL_SURFACE ( 'NONE', #16992, 1.250000000000001110 ) ;
#3977 = DIRECTION ( 'NONE',  ( -1.000000000000000000, -1.224606353822377258E-16, -0.000000000000000000 ) ) ;
#3978 = VECTOR ( 'NONE', #63858, 1000.000000000000000 ) ;
#3979 = CARTESIAN_POINT ( 'NONE',  ( -6.661998917891360783, 40.29425637337637767, -71.19925390475410154 ) ) ;
#3980 = DIRECTION ( 'NONE',  ( 1.000000000000000000, 0.000000000000000000, 0.000000000000000000 ) ) ;
#3981 = ORIENTED_EDGE ( 'NONE', *, *, #106268, .F. ) ;
#3982 = EDGE_CURVE ( 'NONE', #34973, #25211, #39351, .T. ) ;
#3983 =( GEOMETRIC_REPRESENTATION_CONTEXT ( 3 ) GLOBAL_UNCERTAINTY_ASSIGNED_CONTEXT ( ( #1733 ) ) GLOBAL_UNIT_ASSIGNED_CONTEXT ( ( #70336, #36937, #3478 ) ) REPRESENTATION_CONTEXT ( 'NONE', 'WORKASPACE' ) );
#3984 = CARTESIAN_POINT ( 'NONE',  ( -104.9152107932271463, -30.00000000010609469, 126.1345714984008737 ) ) ;
#3985 = VERTEX_POINT ( 'NONE', #88423 ) ;
#3986 = DIRECTION ( 'NONE',  ( 0.000000000000000000, 0.000000000000000000, -1.000000000000000000 ) ) ;
#3987 = CARTESIAN_POINT ( 'NONE',  ( 1.152188841818234133E-13, -1.200000000000000030E-05, 50.50000000000000000 ) ) ;
#3988 = CARTESIAN_POINT ( 'NONE',  ( 6.162888688655347558, 7.505553499465140277, 0.000000000000000000 ) ) ;
#3989 = CARTESIAN_POINT ( 'NONE',  ( 16.10335319434522461, 21.83248469006533199, -0.8773453446276189283 ) ) ;
#3990 = CARTESIAN_POINT ( 'NONE',  ( 84.33012706832269600, -45.28231600066910545, -10.05877812763055523 ) ) ;
#3991 = CIRCLE ( 'NONE', #86690, 0.9999999999999990008 ) ;
#3992 = CARTESIAN_POINT ( 'NONE',  ( 7.188101187499999156, -28.62500000204838457, 2.977408999572654924 ) ) ;
#3993 = CARTESIAN_POINT ( 'NONE',  ( -17.08308936354170982, 34.91790941067561249, 21.80698433968612449 ) ) ;
#3994 = CARTESIAN_POINT ( 'NONE',  ( 105.5353273971932140, 5.000000000000020428, 0.000000000000000000 ) ) ;
#3995 = ORIENTED_EDGE ( 'NONE', *, *, #28861, .F. ) ;
#3996 = ADVANCED_FACE ( 'NONE', ( #14495 ), #54964, .F. ) ;
#3997 = ORIENTED_EDGE ( 'NONE', *, *, #42575, .F. ) ;
#3998 = CARTESIAN_POINT ( 'NONE',  ( 49.22180010227521052, 7.740565218139805914, -15.98496799241697808 ) ) ;
#4000 = ORIENTED_EDGE ( 'NONE', *, *, #2893, .F. ) ;
#3999 = FACE_OUTER_BOUND ( 'NONE', #30085, .T. ) ;
#4001 = CARTESIAN_POINT ( 'NONE',  ( 78.28673168894357559, -60.30906236363500028, 158.4437153918191825 ) ) ;
#4002 = VERTEX_POINT ( 'NONE', #30197 ) ;
#4003 = CARTESIAN_POINT ( 'NONE',  ( 6.162708901257258454, -50.04180103047903572, 39.57312441009716508 ) ) ;
#4004 = CARTESIAN_POINT ( 'NONE',  ( -7.188101187500000933, -20.00000000204838457, -2.977408999572651371 ) ) ;
#4005 = CARTESIAN_POINT ( 'NONE',  ( -106.5151323516585649, -57.65184864013982491, 200.5412705504392079 ) ) ;
#4006 = VERTEX_POINT ( 'NONE', #23169 ) ;
#4007 = CARTESIAN_POINT ( 'NONE',  ( -5.093082057083965886, -12.44446206421571866, -3.176439207277719223 ) ) ;
#4008 = CARTESIAN_POINT ( 'NONE',  ( -9.948688207305195874, 81.12976850509815563, -1.044946705213431137 ) ) ;
#4009 = ADVANCED_FACE ( 'NONE', ( #71161 ), #62557, .T. ) ;
#4010 = CARTESIAN_POINT ( 'NONE',  ( 49.07662235626771263, 14.00107037724277248, -14.92012541985465646 ) ) ;
#4011 = CARTESIAN_POINT ( 'NONE',  ( 7.999999999999998224, -17.28125000409677270, 3.313708498984766493 ) ) ;
#4012 = CARTESIAN_POINT ( 'NONE',  ( -42.05067302585612055, -27.18224454527997480, 37.40642595164874962 ) ) ;
#4013 = CARTESIAN_POINT ( 'NONE',  ( 0.000000000000000000, 0.000000000000000000, 0.000000000000000000 ) ) ;
#4014 = CIRCLE ( 'NONE', #86718, 7.000000000000006217 ) ;
#4015 = DIRECTION ( 'NONE',  ( -1.000000000000000000, -1.224606353822377258E-16, -0.000000000000000000 ) ) ;
#4016 = EDGE_CURVE ( 'NONE', #9392, #61254, #104056, .T. ) ;
#4017 = CARTESIAN_POINT ( 'NONE',  ( 5.025684061874351016, -6.606954474312070502, -14.98089720656572688 ) ) ;
#4018 = DIRECTION ( 'NONE',  ( 0.000000000000000000, 1.000000000000000000, 0.000000000000000000 ) ) ;
#4019 = CIRCLE ( 'NONE', #64309, 5.000000000000001776 ) ;
#4020 = CARTESIAN_POINT ( 'NONE',  ( 61.88291765283142354, 546.5234784715379419, 200.1325441657795068 ) ) ;
#4021 = FACE_OUTER_BOUND ( 'NONE', #99597, .T. ) ;
#4022 = VERTEX_POINT ( 'NONE', #21588 ) ;
#4023 = CARTESIAN_POINT ( 'NONE',  ( -1.081074338060140638, -50.02734650443385789, 40.96720160546766465 ) ) ;
#4024 = CARTESIAN_POINT ( 'NONE',  ( 10.68521086147759647, -5.000000000000001776, -12.55427425704376887 ) ) ;
#4025 = CARTESIAN_POINT ( 'NONE',  ( 1.106009303435988578, 12.12314782375359101, 49.90128369131649322 ) ) ;
#4026 = CARTESIAN_POINT ( 'NONE',  ( -32.75612034570598041, -24.60049146598317904, -37.04625446625190222 ) ) ;
#4027 = CARTESIAN_POINT ( 'NONE',  ( -59.21483274588983647, -29.99999999999999645, 65.04807226357009142 ) ) ;
#4028 = CARTESIAN_POINT ( 'NONE',  ( 22.19860641359351305, 28.18788469371686745, -31.21259335822235315 ) ) ;
#4029 = ORIENTED_EDGE ( 'NONE', *, *, #33718, .F. ) ;
#4030 = CARTESIAN_POINT ( 'NONE',  ( 0.000000000000000000, 79.50000000000000000, 65.00000000000000000 ) ) ;
#4031 = COLOUR_RGB ( '', 0.66274510, 0.83137255, 0.94901961) ;
#4032 = CARTESIAN_POINT ( 'NONE',  ( 78.02157272649068886, -57.51171903303600885, 196.6038749271185111 ) ) ;
#4033 = DIRECTION ( 'NONE',  ( 0.000000000000000000, -1.000000000000000000, 0.000000000000000000 ) ) ;
#4034 = DIRECTION ( 'NONE',  ( 0.000000000000000000, 0.000000000000000000, 1.000000000000000000 ) ) ;
#4035 = DIRECTION ( 'NONE',  ( -1.000000000000000000, -1.224606353822377258E-16, -0.000000000000000000 ) ) ;
#4036 = DIRECTION ( 'NONE',  ( -1.000000000000000000, -1.224606353822377258E-16, -0.000000000000000000 ) ) ;
#4037 = CARTESIAN_POINT ( 'NONE',  ( -69.29604869819449675, -60.00000000000000711, 137.6211246123437206 ) ) ;
#4038 =( LENGTH_UNIT ( ) NAMED_UNIT ( * ) SI_UNIT ( .MILLI., .METRE. ) );
#4039 = SURFACE_STYLE_USAGE ( .BOTH. , #36453 ) ;
#4040 = CARTESIAN_POINT ( 'NONE',  ( -86.04699626542492297, -31.95447380513247282, 184.0172807620984656 ) ) ;
#4042 = VERTEX_POINT ( 'NONE', #80301 ) ;
#4041 = CIRCLE ( 'NONE', #14334, 4.000000000000000000 ) ;
#4043 = CARTESIAN_POINT ( 'NONE',  ( -41.94726657799440517, 461.2497493223742708, 3.266452559861955596 ) ) ;
#4044 = CARTESIAN_POINT ( 'NONE',  ( -1.981107828036278606, -22.06778036923262931, 27.56548919790143870 ) ) ;
#4045 = CARTESIAN_POINT ( 'NONE',  ( -7.054523059426880849, 41.71556238290650498, -59.55896278357374740 ) ) ;
#4046 = DIRECTION ( 'NONE',  ( 0.000000000000000000, 0.000000000000000000, 1.000000000000000000 ) ) ;
#4047 = AXIS2_PLACEMENT_3D ( 'NONE', #84903, #82769, #59576 ) ;
#4048 = DIRECTION ( 'NONE',  ( -1.000000000000000000, -1.224606353822377258E-16, -0.000000000000000000 ) ) ;
#4049 = ADVANCED_FACE ( 'NONE', ( #87893 ), #21073, .T. ) ;
#4050 = CARTESIAN_POINT ( 'NONE',  ( -34.66390255139928200, 326.6599121232922016, -4.408687661176519335 ) ) ;
#4051 = AXIS2_PLACEMENT_3D ( 'NONE', #100580, #82808, #26741 ) ;
#4052 = FACE_OUTER_BOUND ( 'NONE', #78060, .T. ) ;
#4053 = CARTESIAN_POINT ( 'NONE',  ( 31.14131030317610538, 1.482358050883964840E-15, 0.000000000000000000 ) ) ;
#4054 = CARTESIAN_POINT ( 'NONE',  ( -43.47770857297121694, 484.8227827122652229, 4.253339224812703101 ) ) ;
#4055 = AXIS2_PLACEMENT_3D ( 'NONE', #10868, #3872, #52945 ) ;
#4056 = ORIENTED_EDGE ( 'NONE', *, *, #100828, .T. ) ;
#4057 = CARTESIAN_POINT ( 'NONE',  ( 17.59424591481818823, 50.00000000000000711, 62.71031934002806452 ) ) ;
#4058 = DIRECTION ( 'NONE',  ( 1.000000000000000000, 1.224606353822377258E-16, 0.000000000000000000 ) ) ;
#4059 = ADVANCED_FACE ( 'NONE', ( #97028 ), #28923, .T. ) ;
#4060 = CARTESIAN_POINT ( 'NONE',  ( -6.601913983200961233, -4.285714285712858285, -24.56594385547797543 ) ) ;
#4061 = CARTESIAN_POINT ( 'NONE',  ( 9.647447593234698360, 53.40512216555158176, -3.402356764703239111 ) ) ;
#4062 = ADVANCED_FACE ( 'NONE', ( #72229 ), #37247, .T. ) ;
#4063 = CARTESIAN_POINT ( 'NONE',  ( 90.56091889802806350, -29.99999999999993960, 34.47026654395114775 ) ) ;
#4064 = CARTESIAN_POINT ( 'NONE',  ( -79.63233721077718030, -32.55990623632270342, 136.6957858042794385 ) ) ;
#4065 = ORIENTED_EDGE ( 'NONE', *, *, #33055, .F. ) ;
#4066 = DIRECTION ( 'NONE',  ( -1.000000000000000000, -0.000000000000000000, -0.000000000000000000 ) ) ;
#4067 = FACE_OUTER_BOUND ( 'NONE', #6089, .T. ) ;
#4068 = CARTESIAN_POINT ( 'NONE',  ( 30.89728992616315750, -57.68649126897638268, 45.79953151277155143 ) ) ;
#4069 = CARTESIAN_POINT ( 'NONE',  ( 58.26690781281054399, 50.00000000000000711, 24.09029710667956081 ) ) ;
#4070 = CARTESIAN_POINT ( 'NONE',  ( 41.12303835364165394, 320.9630341345189777, 4.352592110578689777 ) ) ;
#4071 = CARTESIAN_POINT ( 'NONE',  ( 25.59999999999999787, 1.533819458162526451E-15, 0.000000000000000000 ) ) ;
#4072 = ORIENTED_EDGE ( 'NONE', *, *, #96963, .T. ) ;
#4073 = CYLINDRICAL_SURFACE ( 'NONE', #89190, 5.000000000000002665 ) ;
#4074 = CARTESIAN_POINT ( 'NONE',  ( 31.33064812253037701, 438.2812499056968818, 22.63898674761892948 ) ) ;
#4075 = CARTESIAN_POINT ( 'NONE',  ( -1.320432766682874540E-15, -24.03125000204838457, 7.188101187500000044 ) ) ;
#4076 = EDGE_CURVE ( 'NONE', #95902, #48016, #103017, .T. ) ;
#4077 = ORIENTED_EDGE ( 'NONE', *, *, #103276, .T. ) ;
#4078 = DIRECTION ( 'NONE',  ( -1.000000000000000000, -0.000000000000000000, -0.000000000000000000 ) ) ;
#4079 = CARTESIAN_POINT ( 'NONE',  ( 6.241999248351493002, 41.80321055404989039, -70.33316251798440533 ) ) ;
#4080 = LINE ( 'NONE', #39113, #39339 ) ;
#4081 = CARTESIAN_POINT ( 'NONE',  ( 1.000000000000000222, -5.000000000000000000, -14.14213562373095101 ) ) ;
#4083 = B_SPLINE_CURVE_WITH_KNOTS ( 'NONE', 3,
 ( #21348, #101824, #5136, #85119 ),
 .UNSPECIFIED., .F., .F.,
 ( 4, 4 ),
 ( 0.000000000000000000, 1.000000000000000000 ),
 .UNSPECIFIED. ) ;
#4082 = PRESENTATION_LAYER_ASSIGNMENT (  '', '', ( #29973 ) ) ;
#4084 = B_SPLINE_CURVE_WITH_KNOTS ( 'NONE', 3,
 ( #62873, #95761, #104365, #79566, #55276, #30517, #63414, #11634, #20868, #37026, #77454, #3567, #36504, #28952, #45102, #69371, #77982, #4098, #61824, #94720 ),
 .UNSPECIFIED., .F., .F.,
 ( 4, 2, 2, 2, 2, 2, 2, 2, 2, 4 ),
 ( 0.007074730525056170845, 0.007326744003114083262, 0.007578757481171995679, 0.008082784437287823115, 0.008586811393403649684, 0.009090838349519476252, 0.009594865305635304556, 0.01009889226175113112, 0.01060291921786695943, 0.01110694617398278600 ),
 .UNSPECIFIED. ) ;
#4085 = FILL_AREA_STYLE ('',( #93087 ) ) ;
#4086 = EDGE_LOOP ( 'NONE', ( #40381, #17061, #81597, #89946, #27974 ) ) ;
#4087 = CARTESIAN_POINT ( 'NONE',  ( 83.46915560824537295, -60.00000000000000000, -25.72054130885968704 ) ) ;
#4089 = CARTESIAN_POINT ( 'NONE',  ( 26.98664971853731487, -46.43314927939716341, 33.41725387913556489 ) ) ;
#4088 = CARTESIAN_POINT ( 'NONE',  ( -73.20747738243755975, -14.21045842199437992, 129.5005664428163641 ) ) ;
#4090 = CARTESIAN_POINT ( 'NONE',  ( 23.61990465140407380, 60.76237703744687479, 11.80995232570204401 ) ) ;
#4091 = VERTEX_POINT ( 'NONE', #22110 ) ;
#4092 = CARTESIAN_POINT ( 'NONE',  ( -38.45575393299976241, -46.43411444215534090, 38.95968530998309376 ) ) ;
#4093 = UNCERTAINTY_MEASURE_WITH_UNIT (LENGTH_MEASURE( 1.000000000000000082E-05 ), #55373, 'distance_accuracy_value', 'NONE');
#4094 = ORIENTED_EDGE ( 'NONE', *, *, #7312, .F. ) ;
#4095 = CARTESIAN_POINT ( 'NONE',  ( -22.67073868809949033, -4.285714285714295357, 11.17734400176826526 ) ) ;
#4096 = DIRECTION ( 'NONE',  ( 0.000000000000000000, 0.000000000000000000, 1.000000000000000000 ) ) ;
#4097 = CARTESIAN_POINT ( 'NONE',  ( -44.17588657941835351, 463.1658906400270439, 6.343983253503433950 ) ) ;
#4098 = CARTESIAN_POINT ( 'NONE',  ( -0.3381277199951053247, 52.16423866172722512, -7.785256431692882728 ) ) ;
#4099 = CARTESIAN_POINT ( 'NONE',  ( 6.943926999490791729, -64.46699007373854329, -3.973092371898547803 ) ) ;
#4100 =( NAMED_UNIT ( * ) SI_UNIT ( $, .STERADIAN. ) SOLID_ANGLE_UNIT ( ) );
#4101 = EDGE_LOOP ( 'NONE', ( #11753, #78760, #16712, #101804 ) ) ;
#4102 = CARTESIAN_POINT ( 'NONE',  ( -67.77671069964115702, -38.33437092114629507, 124.5516907683609418 ) ) ;
#4103 =( LENGTH_UNIT ( ) NAMED_UNIT ( * ) SI_UNIT ( .MILLI., .METRE. ) );
#4104 = CARTESIAN_POINT ( 'NONE',  ( 99.43643474579640440, -30.00000000000000000, 187.6780440051967958 ) ) ;
#4105 = CARTESIAN_POINT ( 'NONE',  ( 42.29310172631443976, 39.52350749398639351, -49.90450179939642084 ) ) ;
#4106 = STYLED_ITEM ( 'NONE', ( #89358 ), #85004 ) ;
#4107 = CARTESIAN_POINT ( 'NONE',  ( -4.813668318631095566, -83.20486770173317836, 3.583991016754781711 ) ) ;
#4108 = CARTESIAN_POINT ( 'NONE',  ( 76.98249430118629277, -30.00000000000000000, -16.66152498815789684 ) ) ;
#4109 = CONICAL_SURFACE ( 'NONE', #62621, 4.000000000000002665, 0.9599310885968824758 ) ;
#4110 = CARTESIAN_POINT ( 'NONE',  ( 64.78349330513380266, 6.975173280561618775E-15, 0.000000000000000000 ) ) ;
#4111 = VERTEX_POINT ( 'NONE', #104586 ) ;
#4112 = ORIENTED_EDGE ( 'NONE', *, *, #78990, .T. ) ;
#4113 = ORIENTED_EDGE ( 'NONE', *, *, #28865, .T. ) ;
#4114 = CARTESIAN_POINT ( 'NONE',  ( 0.000000000000000000, 5.629165124598848102, -3.250000000000007105 ) ) ;
#4115 = CARTESIAN_POINT ( 'NONE',  ( 1.347111479062088996E-15, -4.000000000000003553, 100.9999999999999858 ) ) ;
#4116 = CARTESIAN_POINT ( 'NONE',  ( -45.40857618788439254, 438.4254554321796036, 6.241827246365757809 ) ) ;
#4117 = CARTESIAN_POINT ( 'NONE',  ( 9.999999999999998224, 15.00000000000000000, 4.582575694955846934 ) ) ;
#4118 = CARTESIAN_POINT ( 'NONE',  ( -7.800703710507056243, -88.58595692657942777, 1.791736796405269061 ) ) ;
#4119 = CARTESIAN_POINT ( 'NONE',  ( 25.60851123651794836, 48.00000000000000000, -75.29411764705879762 ) ) ;
#4120 = EDGE_LOOP ( 'NONE', ( #40129, #23758, #8743, #4072 ) ) ;
#4122 = EDGE_CURVE ( 'NONE', #54910, #33830, #73652, .T. ) ;
#4121 = CARTESIAN_POINT ( 'NONE',  ( 42.87890296919691480, 485.5827577773664530, 6.686241925529814445 ) ) ;
#4123 = ORIENTED_EDGE ( 'NONE', *, *, #101926, .T. ) ;
#4124 = CARTESIAN_POINT ( 'NONE',  ( -5.477578620271507326, -61.83498560983895231, -2.459398706554657199 ) ) ;
#4125 = DIRECTION ( 'NONE',  ( 0.6621791990579487530, 0.000000000000000000, -0.7493455199939301759 ) ) ;
#4126 = CARTESIAN_POINT ( 'NONE',  ( 5.656854249492378806, -11.37500000409677092, 5.656854249492381470 ) ) ;
#4127 = CARTESIAN_POINT ( 'NONE',  ( 24.43287555171192693, 295.5625495699969747, 10.08955056188434796 ) ) ;
#4128 = CARTESIAN_POINT ( 'NONE',  ( 6.463481858019718196, -4.600809706232205087, -5.711197301637625401 ) ) ;
#4129 = CARTESIAN_POINT ( 'NONE',  ( 63.59325793215686673, -46.43410071035751230, 85.67174166192037887 ) ) ;
#4130 = B_SPLINE_CURVE_WITH_KNOTS ( 'NONE', 3,
 ( #47060, #37964, #62741, #21248 ),
 .UNSPECIFIED., .F., .F.,
 ( 4, 4 ),
 ( 0.000000000000000000, 1.000000000000000000 ),
 .UNSPECIFIED. ) ;
#4131 = CIRCLE ( 'NONE', #45477, 15.00000000000001243 ) ;
#4132 = ORIENTED_EDGE ( 'NONE', *, *, #19874, .T. ) ;
#4133 = LINE ( 'NONE', #102829, #103012 ) ;
#4134 = CARTESIAN_POINT ( 'NONE',  ( -64.54403517473807028, -37.84143551314759435, -32.95252873240283975 ) ) ;
#4135 = LINE ( 'NONE', #30551, #97119 ) ;
#4136 = VECTOR ( 'NONE', #72568, 1000.000000000000000 ) ;
#4137 = EDGE_CURVE ( 'NONE', #51789, #56343, #47409, .T. ) ;
#4138 = CARTESIAN_POINT ( 'NONE',  ( -6.573529411764777564, 40.00000000000032685, -71.39502911389392636 ) ) ;
#4139 =( GEOMETRIC_REPRESENTATION_CONTEXT ( 3 ) GLOBAL_UNCERTAINTY_ASSIGNED_CONTEXT ( ( #57512 ) ) GLOBAL_UNIT_ASSIGNED_CONTEXT ( ( #104150, #65820, #24854 ) ) REPRESENTATION_CONTEXT ( 'NONE', 'WORKASPACE' ) );
#4141 = ORIENTED_EDGE ( 'NONE', *, *, #87040, .T. ) ;
#4140 = AXIS2_PLACEMENT_3D ( 'NONE', #37323, #70184, #103090 ) ;
#4142 =( LENGTH_UNIT ( ) NAMED_UNIT ( * ) SI_UNIT ( .MILLI., .METRE. ) );
#4143 = DIRECTION ( 'NONE',  ( 0.000000000000000000, 0.000000000000000000, 1.000000000000000000 ) ) ;
#4144 =( NAMED_UNIT ( * ) SI_UNIT ( $, .STERADIAN. ) SOLID_ANGLE_UNIT ( ) );
#4145 = DIRECTION ( 'NONE',  ( 0.000000000000000000, -1.000000000000000000, 0.000000000000000000 ) ) ;
#4146 = CARTESIAN_POINT ( 'NONE',  ( 8.349999999999999645, -4.171999999999999709, 5.616230220889763424E-16 ) ) ;
#4147 = FACE_OUTER_BOUND ( 'NONE', #67341, .T. ) ;
#4148 = CARTESIAN_POINT ( 'NONE',  ( 86.32370369321748171, -31.85974275469703088, 185.2292116863652609 ) ) ;
#4149 = ADVANCED_FACE ( 'NONE', ( #86842 ), #13374, .T. ) ;
#4150 = CARTESIAN_POINT ( 'NONE',  ( -5.292102851260739094, 18.18885909246420596, -37.58867055452670769 ) ) ;
#4151 = EDGE_CURVE ( 'NONE', #10937, #90401, #27218, .T. ) ;
#4152 = CARTESIAN_POINT ( 'NONE',  ( -9.252395038628018042, 11.88928468659940307, 0.000000000000000000 ) ) ;
#4153 = VERTEX_POINT ( 'NONE', #64670 ) ;
#4154 = CARTESIAN_POINT ( 'NONE',  ( -10.00000000000000355, 30.00000000000000000, 0.000000000000000000 ) ) ;
#4155 = DIRECTION ( 'NONE',  ( 0.000000000000000000, 0.000000000000000000, 1.000000000000000000 ) ) ;
#4156 = DIRECTION ( 'NONE',  ( 0.000000000000000000, 0.000000000000000000, -1.000000000000000000 ) ) ;
#4157 = CARTESIAN_POINT ( 'NONE',  ( 0.000000000000000000, 6.123233995736770227E-16, -5.000000000000002665 ) ) ;
#4158 = CARTESIAN_POINT ( 'NONE',  ( -99.16808899320049875, -30.00000000000000355, 146.3606151617508431 ) ) ;
#4159 = AXIS2_PLACEMENT_3D ( 'NONE', #99423, #50345, #25602 ) ;
#4160 = CARTESIAN_POINT ( 'NONE',  ( -0.5204879950542349309, -7.205049615410642261, -0.5609245978742314342 ) ) ;
#4161 = CARTESIAN_POINT ( 'NONE',  ( 19.23758136976156052, -57.67182727287845267, 42.11656184680051496 ) ) ;
#4163 = CARTESIAN_POINT ( 'NONE',  ( 12.08334041755991706, 304.5866437775407007, -10.05636128505472549 ) ) ;
#4162 = CARTESIAN_POINT ( 'NONE',  ( -0.08435185965673104580, 25.16821295365207334, -40.75000000000000711 ) ) ;
#4164 = DIRECTION ( 'NONE',  ( -1.000000000000000000, 0.000000000000000000, 0.000000000000000000 ) ) ;
#4165 = CARTESIAN_POINT ( 'NONE',  ( -17.81569236505151466, 50.00000000000000000, 62.15697636927347247 ) ) ;
#4166 = CARTESIAN_POINT ( 'NONE',  ( -42.75202416090640156, 486.5826644064231914, 6.942705799449254478 ) ) ;
#4167 = LINE ( 'NONE', #73106, #78661 ) ;
#4168 = AXIS2_PLACEMENT_3D ( 'NONE', #93317, #18935, #84691 ) ;
#4169 = FACE_OUTER_BOUND ( 'NONE', #104137, .T. ) ;
#4170 = DIRECTION ( 'NONE',  ( -0.000000000000000000, -0.000000000000000000, -1.000000000000000000 ) ) ;
#4171 = VERTEX_POINT ( 'NONE', #98091 ) ;
#4172 = CARTESIAN_POINT ( 'NONE',  ( 39.80120353649597575, 485.6913716985618521, -4.529092486720104560 ) ) ;
#4173 = CARTESIAN_POINT ( 'NONE',  ( 55.00571552735602410, 6.975173280561618775E-15, 0.000000000000000000 ) ) ;
#4174 = CARTESIAN_POINT ( 'NONE',  ( -18.16430329042714931, -53.40190210536660231, 33.13507712519638204 ) ) ;
#4176 = CARTESIAN_POINT ( 'NONE',  ( 41.14934085771739092, 484.9010050731022829, -3.779718508949024169 ) ) ;
#4175 = CARTESIAN_POINT ( 'NONE',  ( -6.900000000000000355, 8.450062914116737647E-16, -0.7702282920306786629 ) ) ;
#4177 = EDGE_LOOP ( 'NONE', ( #61258, #17732 ) ) ;
#4178 = DIRECTION ( 'NONE',  ( -1.000000000000000000, -1.224606353822377258E-16, -0.000000000000000000 ) ) ;
#4179 = ORIENTED_EDGE ( 'NONE', *, *, #58104, .F. ) ;
#4180 = CARTESIAN_POINT ( 'NONE',  ( 15.50079525336341391, 2.626985771264193747, -0.7904007780842380315 ) ) ;
#4181 = LINE ( 'NONE', #53268, #57851 ) ;
#4182 = EDGE_LOOP ( 'NONE', ( #77702, #62178, #72671, #28091, #74221 ) ) ;
#4183 = PRESENTATION_STYLE_ASSIGNMENT (( #71554 ) ) ;
#4184 = CARTESIAN_POINT ( 'NONE',  ( 0.000000000000000000, 0.000000000000000000, -0.9215586320570148260 ) ) ;
#4185 = CARTESIAN_POINT ( 'NONE',  ( 101.2091753172953190, -45.28154215804822513, 190.9441895052663938 ) ) ;
#4187 = CARTESIAN_POINT ( 'NONE',  ( 0.000000000000000000, 0.000000000000000000, 5.000000000000000888 ) ) ;
#4186 = CARTESIAN_POINT ( 'NONE',  ( 46.25537882904671250, -37.26716345494458693, 44.48526200656858265 ) ) ;
#4188 = ORIENTED_EDGE ( 'NONE', *, *, #2146, .T. ) ;
#4189 = AXIS2_PLACEMENT_3D ( 'NONE', #26872, #85071, #11154 ) ;
#4190 = ORIENTED_EDGE ( 'NONE', *, *, #5905, .F. ) ;
#4191 = EDGE_CURVE ( 'NONE', #62746, #32321, #21589, .T. ) ;
#4192 = VERTEX_POINT ( 'NONE', #950 ) ;
#4194 =( BOUNDED_SURFACE ( )  B_SPLINE_SURFACE ( 2, 3, ( 
 ( #48594, #49121, #23302, #40519, #32986, #73397 ),
 ( #8678, #72356, #97154, #106296, #32459, #65331 ),
 ( #80435, #82022, #57743, #41580, #98219, #33510 ) ),
 .UNSPECIFIED., .F., .F., .F. ) 
 B_SPLINE_SURFACE_WITH_KNOTS ( ( 3, 3 ),
 ( 4, 2, 4 ),
 ( 0.000000000000000000, 1.000000000000000000 ),
 ( 0.07468083296558609974, 0.1199308329655860983, 0.1241808329655861021 ),
 .UNSPECIFIED. ) 
 GEOMETRIC_REPRESENTATION_ITEM ( )  RATIONAL_B_SPLINE_SURFACE ( (
 ( 1.000000000000000000, 1.000000000000000000, 1.000000000000000000, 1.000000000000000000, 1.000000000000000000, 1.000000000000000000),
 ( 1.857142857142858317, 1.857142857142858317, 1.857142857142858317, 1.857142857142858317, 1.857142857142858317, 1.857142857142858317),
 ( 1.000000000000000000, 1.000000000000000000, 1.000000000000000000, 1.000000000000000000, 1.000000000000000000, 1.000000000000000000) ) ) 
 REPRESENTATION_ITEM ( '' )  SURFACE ( )  );
#4193 = CARTESIAN_POINT ( 'NONE',  ( 23.39524124133658844, 305.8619436084897529, 9.157947684428933144 ) ) ;
#4195 = EDGE_CURVE ( 'NONE', #50869, #52643, #85711, .T. ) ;
#4196 = CARTESIAN_POINT ( 'NONE',  ( -16.75187969033554936, 34.99134772383131065, -21.80698433968595751 ) ) ;
#4197 = CARTESIAN_POINT ( 'NONE',  ( -14.29190075645216318, 6.456385560668112866, -7.561819230143454362 ) ) ;
#4198 = VERTEX_POINT ( 'NONE', #16647 ) ;
#4199 = AXIS2_PLACEMENT_3D ( 'NONE', #82805, #62524, #15409 ) ;
#4200 = CARTESIAN_POINT ( 'NONE',  ( 0.000000000000000000, 0.000000000000000000, 0.000000000000000000 ) ) ;
#4201 = CARTESIAN_POINT ( 'NONE',  ( -6.602502349679192584, 41.80321055419442899, -70.07543150438399948 ) ) ;
#4202 = CIRCLE ( 'NONE', #66244, 9.999999999999998224 ) ;
#4203 = CARTESIAN_POINT ( 'NONE',  ( -95.16212988580207366, -60.00000000004876455, 30.21691017251174216 ) ) ;
#4204 = DIRECTION ( 'NONE',  ( 0.000000000000000000, -1.000000000000000000, 0.000000000000000000 ) ) ;
#4205 = CARTESIAN_POINT ( 'NONE',  ( 81.11166217577948601, -59.99999999999026556, -30.02696344982326337 ) ) ;
#4206 = CARTESIAN_POINT ( 'NONE',  ( -6.524042246343456419, -4.999999999999999112, 15.07235311481336559 ) ) ;
#4207 = CARTESIAN_POINT ( 'NONE',  ( -6.670526998832738919, 41.45458147225290446, -58.55660974155367171 ) ) ;
#4209 = CARTESIAN_POINT ( 'NONE',  ( 7.030933152283679100, -25.54832196774594522, 28.13802627504265885 ) ) ;
#4208 = CARTESIAN_POINT ( 'NONE',  ( -101.4323841882945771, -14.21045842199443499, 121.1831906623697677 ) ) ;
#4210 =( LENGTH_UNIT ( ) NAMED_UNIT ( * ) SI_UNIT ( .MILLI., .METRE. ) );
#4211 = CARTESIAN_POINT ( 'NONE',  ( -48.21680793553016287, -53.36514319048075805, 52.27612587481558393 ) ) ;
#4212 = ORIENTED_EDGE ( 'NONE', *, *, #48194, .F. ) ;
#4213 = CARTESIAN_POINT ( 'NONE',  ( -3.177887466246608117, 20.29553532598250598, 6.239201926316404467 ) ) ;
#4214 = ORIENTED_EDGE ( 'NONE', *, *, #66504, .T. ) ;
#4215 = DIRECTION ( 'NONE',  ( -1.000000000000000000, -1.224606353822377258E-16, -0.000000000000000000 ) ) ;
#4216 = DIRECTION ( 'NONE',  ( 0.000000000000000000, 1.000000000000000000, 0.000000000000000000 ) ) ;
#4217 = CARTESIAN_POINT ( 'NONE',  ( 5.858881034796412202, -6.214136759970199542, 1.317748741875969243 ) ) ;
#4218 = ORIENTED_EDGE ( 'NONE', *, *, #29825, .T. ) ;
#4219 = CARTESIAN_POINT ( 'NONE',  ( -6.835098440474090431, -6.776903958348333035, 13.91313563306597700 ) ) ;
#4220 = ORIENTED_EDGE ( 'NONE', *, *, #21653, .T. ) ;
#4221 = CARTESIAN_POINT ( 'NONE',  ( 89.33888981624761527, -30.00000000000353850, -13.70441906546611044 ) ) ;
#4222 = DIRECTION ( 'NONE',  ( 0.000000000000000000, -1.000000000000000000, 0.000000000000000000 ) ) ;
#4223 = CARTESIAN_POINT ( 'NONE',  ( 6.883638421508285532, 41.77293051532582524, -59.38142182129858071 ) ) ;
#4224 = CARTESIAN_POINT ( 'NONE',  ( -29.83308852624522345, 41.99999999999999289, 51.76085035109112198 ) ) ;
#4225 = CARTESIAN_POINT ( 'NONE',  ( 101.2094742396540425, -30.00000000000000000, 175.1259804473514521 ) ) ;
#4226 = LINE ( 'NONE', #29600, #51798 ) ;
#4227 = ORIENTED_EDGE ( 'NONE', *, *, #100714, .T. ) ;
#4228 = AXIS2_PLACEMENT_3D ( 'NONE', #67235, #59674, #59139 ) ;
#4229 = ORIENTED_EDGE ( 'NONE', *, *, #19401, .T. ) ;
#4230 = ORIENTED_EDGE ( 'NONE', *, *, #1342, .F. ) ;
#4231 = CARTESIAN_POINT ( 'NONE',  ( 54.29581107121828865, -29.09449404548636409, 54.75117451817219205 ) ) ;
#4232 = CARTESIAN_POINT ( 'NONE',  ( -46.00000000000000000, 436.1162229055561852, 10.84634507115767477 ) ) ;
#4233 = CARTESIAN_POINT ( 'NONE',  ( -46.00000000000000711, 460.8553455089887052, 7.925197340742291985 ) ) ;
#4234 = VERTEX_POINT ( 'NONE', #33928 ) ;
#4236 = EDGE_CURVE ( 'NONE', #67515, #56640, #44350, .T. ) ;
#4235 = CARTESIAN_POINT ( 'NONE',  ( -87.51990533283513685, -38.36637924240768172, -20.20941912294309262 ) ) ;
#4237 = VERTEX_POINT ( 'NONE', #24241 ) ;
#4238 = DIRECTION ( 'NONE',  ( -1.000000000000000000, -1.224606353822377258E-16, -0.000000000000000000 ) ) ;
#4239 = CARTESIAN_POINT ( 'NONE',  ( 105.2106280407045631, -38.39002650047679310, 197.2706458416391797 ) ) ;
#4240 = CARTESIAN_POINT ( 'NONE',  ( 10.82293865544385980, 16.07063780477403370, 9.522976597001717280 ) ) ;
#4241 = CONICAL_SURFACE ( 'NONE', #30052, 4.172000000000001485, 0.9599310885968750373 ) ;
#4242 = CARTESIAN_POINT ( 'NONE',  ( 83.97326503874400316, -45.28715381657895733, 3.105619776616419969 ) ) ;
#4243 = CARTESIAN_POINT ( 'NONE',  ( 5.975663821525200703, -4.257391242883789673, 5.625982059626458032 ) ) ;
#4244 = CIRCLE ( 'NONE', #104159, 5.000000000000002665 ) ;
#4245 = CARTESIAN_POINT ( 'NONE',  ( 33.16832779733599068, 391.0018465421582619, 25.58625501838764649 ) ) ;
#4246 = FACE_OUTER_BOUND ( 'NONE', #52682, .T. ) ;
#4247 = STYLED_ITEM ( 'NONE', ( #26921 ), #41549 ) ;
#4248 = DIRECTION ( 'NONE',  ( -1.000000000000000000, -1.224606353822377258E-16, -0.000000000000000000 ) ) ;
#4249 = STYLED_ITEM ( 'NONE', ( #59422 ), #85702 ) ;
#4250 = COLOUR_RGB ( '', 0.31764706, 0.68627451, 0.89019608) ;
#4251 = CARTESIAN_POINT ( 'NONE',  ( -14.29190075645648683, 6.456385560661901835, 7.561819230138081771 ) ) ;
#4252 = DIRECTION ( 'NONE',  ( 0.000000000000000000, 0.000000000000000000, 1.000000000000000000 ) ) ;
#4253 = ORIENTED_EDGE ( 'NONE', *, *, #63596, .T. ) ;
#4254 = EDGE_CURVE ( 'NONE', #98888, #54301, #40852, .T. ) ;
#4255 = SURFACE_STYLE_FILL_AREA ( #19954 ) ;
#4256 = CARTESIAN_POINT ( 'NONE',  ( 0.000000000000000000, 0.000000000000000000, -3.764187203485586330 ) ) ;
#4257 = CARTESIAN_POINT ( 'NONE',  ( 7.500000000000006217, 152.0000000000000000, 0.000000000000000000 ) ) ;
#4258 = ORIENTED_EDGE ( 'NONE', *, *, #21466, .F. ) ;
#4259 = CARTESIAN_POINT ( 'NONE',  ( -28.47185190024522683, 309.2877488384496019, -7.987972226861596248 ) ) ;
#4260 = CARTESIAN_POINT ( 'NONE',  ( -38.95921387178869821, 313.4153382223458948, 6.403111246584953342 ) ) ;
#4261 = DIRECTION ( 'NONE',  ( 0.000000000000000000, 0.000000000000000000, 1.000000000000000000 ) ) ;
#4262 = SURFACE_STYLE_USAGE ( .BOTH. , #54366 ) ;
#4263 = CARTESIAN_POINT ( 'NONE',  ( 5.656854249492380582, -19.81249999999999289, -5.656854249492379694 ) ) ;
#4264 = CARTESIAN_POINT ( 'NONE',  ( -40.30924518282468227, -28.68040258788349561, 47.69910574250469182 ) ) ;
#4265 = CARTESIAN_POINT ( 'NONE',  ( -14.11571568429507018, 5.211159435679596719, 3.514002131789491390 ) ) ;
#4266 = ORIENTED_EDGE ( 'NONE', *, *, #15158, .F. ) ;
#4267 = CARTESIAN_POINT ( 'NONE',  ( 83.89774654829980705, -46.54964297292601572, 184.2018487009828789 ) ) ;
#4268 = CARTESIAN_POINT ( 'NONE',  ( -38.78825536228157489, 27.29347880557803308, 12.52013247353241177 ) ) ;
#4269 = EDGE_CURVE ( 'NONE', #712, #17802, #57090, .T. ) ;
#4270 = CARTESIAN_POINT ( 'NONE',  ( 45.36923076923077502, 1.411358822780289120E-15, 0.000000000000000000 ) ) ;
#4271 = ORIENTED_EDGE ( 'NONE', *, *, #55132, .T. ) ;
#4272 = CARTESIAN_POINT ( 'NONE',  ( -95.59733413037783123, -37.82076376832549158, 111.4287389431865734 ) ) ;
#4273 = CARTESIAN_POINT ( 'NONE',  ( 5.947762761376473861, 2.501851166488373579, -6.500000000000000000 ) ) ;
#4274 = CARTESIAN_POINT ( 'NONE',  ( 14.61924042696704440, -5.000000000000005329, -89.34162378225812517 ) ) ;
#4275 = CARTESIAN_POINT ( 'NONE',  ( -30.93381850223239482, 8.838939540955959018, 40.91347331214245031 ) ) ;
#4276 = AXIS2_PLACEMENT_3D ( 'NONE', #58801, #2121, #25392 ) ;
#4277 = EDGE_CURVE ( 'NONE', #61560, #22182, #94749, .T. ) ;
#4278 = CARTESIAN_POINT ( 'NONE',  ( -43.50377727019363761, 435.9167426301696651, 18.24083946424746117 ) ) ;
#4279 = CARTESIAN_POINT ( 'NONE',  ( 15.20944265188900424, -22.80677179166491797, 35.96349324364335587 ) ) ;
#4280 = CARTESIAN_POINT ( 'NONE',  ( 33.62703971678629955, -23.41653139858035360, 33.03092013152653550 ) ) ;
#4281 = EDGE_CURVE ( 'NONE', #68880, #20574, #54712, .T. ) ;
#4283 = CARTESIAN_POINT ( 'NONE',  ( -11.67857513420520554, 18.91569503322274315, 8.075412257376374470 ) ) ;
#4282 = FACE_OUTER_BOUND ( 'NONE', #88766, .T. ) ;
#4284 = EDGE_CURVE ( 'NONE', #41649, #68317, #63775, .T. ) ;
#4285 = CARTESIAN_POINT ( 'NONE',  ( 2.922700453347648608, 295.7443989525935422, -10.00347189219364097 ) ) ;
#4286 = CARTESIAN_POINT ( 'NONE',  ( -16.48462266119839015, 43.81152415571271064, -4.165346518886126503 ) ) ;
#4287 = EDGE_CURVE ( 'NONE', #39378, #59650, #82283, .T. ) ;
#4288 = CARTESIAN_POINT ( 'NONE',  ( -19.30606845287076823, 294.6887117073658260, 1.902827613119838501 ) ) ;
#4289 = DIRECTION ( 'NONE',  ( 0.5735764363510442720, -0.8191520442889930198, 1.003171929053526349E-16 ) ) ;
#4290 = ORIENTED_EDGE ( 'NONE', *, *, #2571, .F. ) ;
#4291 = FACE_OUTER_BOUND ( 'NONE', #73788, .T. ) ;
#4292 = ORIENTED_EDGE ( 'NONE', *, *, #79181, .F. ) ;
#4293 = CARTESIAN_POINT ( 'NONE',  ( -9.517455598866080280, -3.342537638539781586, 14.84703453944758955 ) ) ;
#4294 = CARTESIAN_POINT ( 'NONE',  ( 87.04245038058458306, -2.002967142162725287E-29, 5.000000000000011546 ) ) ;
#4295 = CARTESIAN_POINT ( 'NONE',  ( 5.476751506168961114, -61.83642877133009108, -2.461144630687909451 ) ) ;
#4297 = CARTESIAN_POINT ( 'NONE',  ( 1.581782531941442027, -47.40884548514188168, -34.79113668873367260 ) ) ;
#4296 = CARTESIAN_POINT ( 'NONE',  ( 9.918579450955592236, 253.7930391296868606, 1.297207292923829636 ) ) ;
#4298 = ORIENTED_EDGE ( 'NONE', *, *, #76053, .T. ) ;
#4299 = CARTESIAN_POINT ( 'NONE',  ( 28.35336936217584025, 36.33375255386920344, 8.699746290353250089 ) ) ;
#4300 = CARTESIAN_POINT ( 'NONE',  ( -44.51476414391957803, 462.1216152431910018, 5.766699157894676908 ) ) ;
#4301 = ORIENTED_EDGE ( 'NONE', *, *, #58791, .T. ) ;
#4302 = CARTESIAN_POINT ( 'NONE',  ( 6.445370176741822554, 4.584736124523701939, 5.738941594274445279 ) ) ;
#4303 = DIRECTION ( 'NONE',  ( 0.000000000000000000, 0.000000000000000000, 1.000000000000000000 ) ) ;
#4304 = CARTESIAN_POINT ( 'NONE',  ( -91.96777462086218691, -60.00000000000000000, 17.71638642338550795 ) ) ;
#4305 = EDGE_LOOP ( 'NONE', ( #60907, #86496 ) ) ;
#4306 = DIRECTION ( 'NONE',  ( -1.000000000000000000, -1.224606353822377258E-16, -0.000000000000000000 ) ) ;
#4307 = LINE ( 'NONE', #62554, #66069 ) ;
#4308 = DIRECTION ( 'NONE',  ( 1.000000000000000000, 1.224606353822377258E-16, 0.000000000000000000 ) ) ;
#4309 = CARTESIAN_POINT ( 'NONE',  ( -9.537291425704607306, 27.35595622667227289, 3.012810007365996245 ) ) ;
#4311 = CARTESIAN_POINT ( 'NONE',  ( 91.37578371391791165, -2.002967142162725287E-29, 5.000000000000011546 ) ) ;
#4310 = CARTESIAN_POINT ( 'NONE',  ( -3.313708498984741180, -27.03124999999998934, -8.000000000000019540 ) ) ;
#4312 = CARTESIAN_POINT ( 'NONE',  ( -80.97806908835234196, -53.42006643256369358, 173.1435725716072227 ) ) ;
#4313 = ORIENTED_EDGE ( 'NONE', *, *, #49773, .T. ) ;
#4314 = CIRCLE ( 'NONE', #14605, 3.309500000000007880 ) ;
#4315 = CARTESIAN_POINT ( 'NONE',  ( -17.01584901091793967, 0.000000000000000000, -1.113195845621204993 ) ) ;
#4316 = VERTEX_POINT ( 'NONE', #3125 ) ;
#4317 = VECTOR ( 'NONE', #9159, 1000.000000000000114 ) ;
#4318 = ORIENTED_EDGE ( 'NONE', *, *, #75224, .T. ) ;
#4319 = CARTESIAN_POINT ( 'NONE',  ( -8.354779502917955014, -5.000000000000000000, -14.10835818931678176 ) ) ;
#4320 = ADVANCED_FACE ( 'NONE', ( #101296 ), #90927, .F. ) ;
#4321 = CARTESIAN_POINT ( 'NONE',  ( -2.900817060773052347, -70.21372430060392844, 13.30197803733283379 ) ) ;
#4322 = PRESENTATION_STYLE_ASSIGNMENT (( #37790 ) ) ;
#4323 = VERTEX_POINT ( 'NONE', #27445 ) ;
#4324 = CARTESIAN_POINT ( 'NONE',  ( -21.98976603507239247, 28.09591002020466632, 31.66807300705238504 ) ) ;
#4325 = CARTESIAN_POINT ( 'NONE',  ( -53.00838388237266940, -57.67116150918030115, -39.31046371713402721 ) ) ;
#4326 = CARTESIAN_POINT ( 'NONE',  ( 7.002990960197235104, -11.05266818383458016, 3.868040364119523566 ) ) ;
#4327 = CARTESIAN_POINT ( 'NONE',  ( 44.13780905824104650, 464.3951235510549509, 9.689956794375980564 ) ) ;
#4328 = CARTESIAN_POINT ( 'NONE',  ( 24.23713502960781341, 27.31419257049584104, 32.69873751732569644 ) ) ;
#4329 =( NAMED_UNIT ( * ) SI_UNIT ( $, .STERADIAN. ) SOLID_ANGLE_UNIT ( ) );
#4330 = CARTESIAN_POINT ( 'NONE',  ( -17.37733725250675221, 36.93507598878604625, -21.96268678933289920 ) ) ;
#4331 = EDGE_CURVE ( 'NONE', #87056, #65902, #19364, .T. ) ;
#4332 = CARTESIAN_POINT ( 'NONE',  ( 93.93995408072316877, -60.00000000000007816, -15.95669063232190155 ) ) ;
#4333 = CARTESIAN_POINT ( 'NONE',  ( -74.93456164446882894, -30.00000000000001421, 156.1801137937684985 ) ) ;
#4334 = CARTESIAN_POINT ( 'NONE',  ( -58.48862033019764084, -18.66108675706986730, 59.20230775497523013 ) ) ;
#4335 = ORIENTED_EDGE ( 'NONE', *, *, #86266, .T. ) ;
#4336 = CARTESIAN_POINT ( 'NONE',  ( 71.63333333333333997, -3.309500000000000774, 4.475777889183797681E-16 ) ) ;
#4337 = VERTEX_POINT ( 'NONE', #20433 ) ;
#4338 = CARTESIAN_POINT ( 'NONE',  ( -99.23041091440894945, -37.78869810946568464, 191.6572301050025260 ) ) ;
#4339 = CARTESIAN_POINT ( 'NONE',  ( 0.000000000000000000, 2.000000000000000000, 0.000000000000000000 ) ) ;
#4340 = CARTESIAN_POINT ( 'NONE',  ( -1.220556079094060831, 51.58127574836134244, 9.313543911585616897 ) ) ;
#4341 = ORIENTED_EDGE ( 'NONE', *, *, #82819, .F. ) ;
#4342 = CARTESIAN_POINT ( 'NONE',  ( 19.12649177053515714, 49.70304845705965846, 61.69455185923964535 ) ) ;
#4343 = CARTESIAN_POINT ( 'NONE',  ( -23.93160351366482885, -59.99999999999998579, 40.89972924297317292 ) ) ;
#4344 = CARTESIAN_POINT ( 'NONE',  ( 37.40740465628558553, 25.81286408686213463, -10.95617127781081024 ) ) ;
#4345 = CARTESIAN_POINT ( 'NONE',  ( -5.082755093536325042, -14.46875000204838457, -5.082755093536325930 ) ) ;
#4346 = CARTESIAN_POINT ( 'NONE',  ( -3.954440898799530313, -67.58589629217112815, 13.13255854702942926 ) ) ;
#4347 = DIRECTION ( 'NONE',  ( 0.000000000000000000, 1.000000000000000000, 0.000000000000000000 ) ) ;
#4348 = STYLED_ITEM ( 'NONE', ( #38521 ), #99162 ) ;
#4349 = CARTESIAN_POINT ( 'NONE',  ( 7.934883677559678716, -81.13160822062448574, 1.051380792122687202 ) ) ;
#4350 = CARTESIAN_POINT ( 'NONE',  ( -29.50756122520733271, 297.9063904818165724, 10.61050061783298126 ) ) ;
#4351 = CARTESIAN_POINT ( 'NONE',  ( 0.000000000000000000, 0.000000000000000000, 0.000000000000000000 ) ) ;
#4352 = CARTESIAN_POINT ( 'NONE',  ( -23.21751746555280249, -1.200000000000000030E-05, -31.95617127781034839 ) ) ;
#4353 = CARTESIAN_POINT ( 'NONE',  ( -5.347321875081102682, 33.30354557871893206, -51.19160682728892908 ) ) ;
#4354 = CARTESIAN_POINT ( 'NONE',  ( -28.82410583165911078, -60.34270495868832285, 36.38275433194883135 ) ) ;
#4355 = ORIENTED_EDGE ( 'NONE', *, *, #51750, .F. ) ;
#4356 = CARTESIAN_POINT ( 'NONE',  ( 48.50248592037799966, -25.67881720222466413, 44.08540501476609563 ) ) ;
#4357 = DIRECTION ( 'NONE',  ( -0.000000000000000000, -0.000000000000000000, -1.000000000000000000 ) ) ;
#4358 = CARTESIAN_POINT ( 'NONE',  ( 7.898269865231972275, 11.02838903529590731, -0.02849990174189836675 ) ) ;
#4360 = EDGE_CURVE ( 'NONE', #77575, #24576, #11605, .T. ) ;
#4359 = CARTESIAN_POINT ( 'NONE',  ( -86.84248034292065199, -38.60144547145630867, 199.4726879763670411 ) ) ;
#4361 = ORIENTED_EDGE ( 'NONE', *, *, #75414, .T. ) ;
#4362 = CARTESIAN_POINT ( 'NONE',  ( 90.78374300502272831, -38.34267589133914100, 5.711982823473677584 ) ) ;
#4363 = CARTESIAN_POINT ( 'NONE',  ( 14.21497376764425091, 4.168734049602408120, -4.751813484541924204 ) ) ;
#4364 = CARTESIAN_POINT ( 'NONE',  ( -18.93411340542660426, 49.15937788526225205, 62.07943494194688583 ) ) ;
#4365 = CARTESIAN_POINT ( 'NONE',  ( 17.50000000000002842, 50.00000000000000000, -500000.0000000000582 ) ) ;
#4366 = CARTESIAN_POINT ( 'NONE',  ( 6.716520184430065044, 41.04202977371297578, -70.96212004294623910 ) ) ;
#4367 = CARTESIAN_POINT ( 'NONE',  ( 3.313708498984780260, -25.90625000409676915, -7.999999999999981348 ) ) ;
#4368 = DIRECTION ( 'NONE',  ( -1.000000000000000000, -1.224606353822377258E-16, -0.000000000000000000 ) ) ;
#4369 = CARTESIAN_POINT ( 'NONE',  ( 33.05096523792742147, 434.2951806504310639, 15.74562047622584871 ) ) ;
#4370 = CARTESIAN_POINT ( 'NONE',  ( 112.1326292210085853, -59.99999999999997868, 177.2482590370370588 ) ) ;
#4371 = CARTESIAN_POINT ( 'NONE',  ( -7.618844049274131613, -68.17235898929459381, 2.450177051822849172 ) ) ;
#4372 = ORIENTED_EDGE ( 'NONE', *, *, #99851, .F. ) ;
#4373 = EDGE_CURVE ( 'NONE', #87124, #26304, #48275, .T. ) ;
#4374 = DIRECTION ( 'NONE',  ( -1.000000000000000000, -1.224606353822377258E-16, -0.000000000000000000 ) ) ;
#4375 = AXIS2_PLACEMENT_3D ( 'NONE', #36784, #2771, #68598 ) ;
#4376 = CARTESIAN_POINT ( 'NONE',  ( -80.80298817501201825, -30.00000000000003197, 8.170653238303200894 ) ) ;
#4377 = ORIENTED_EDGE ( 'NONE', *, *, #40482, .T. ) ;
#4379 = CARTESIAN_POINT ( 'NONE',  ( 5.075566108724593128, -4.332661967060489339, -17.09624963492156269 ) ) ;
#4378 = CARTESIAN_POINT ( 'NONE',  ( -81.36991943370300362, -38.84403975064132908, 195.1307900073841211 ) ) ;
#4380 = CARTESIAN_POINT ( 'NONE',  ( 12.49999999999999289, -3.156328017129524266, -14.15649578910353412 ) ) ;
#4381 = CARTESIAN_POINT ( 'NONE',  ( -1.047197551196596521, -3.000000000000000888, -8.000000000000003553 ) ) ;
#4382 = CARTESIAN_POINT ( 'NONE',  ( 42.20041562234358423, 435.2369744135583574, 7.788607701745475786 ) ) ;
#4383 = CARTESIAN_POINT ( 'NONE',  ( 5.082755093536325930, -14.84375000204838457, -5.082755093536325042 ) ) ;
#4384 = CIRCLE ( 'NONE', #37137, 5.000000000000002665 ) ;
#4385 = CARTESIAN_POINT ( 'NONE',  ( -7.996668422906947349, -3.000000000000002665, -91.14546720082398679 ) ) ;
#4386 = COLOUR_RGB ( '', 0.08235294, 0.09019608, 0.10196078) ;
#4387 = AXIS2_PLACEMENT_3D ( 'NONE', #77555, #45205, #11731 ) ;
#4388 = CARTESIAN_POINT ( 'NONE',  ( 30.80732993440513567, 13.24159032961889437, -41.41050123719151088 ) ) ;
#4389 = AXIS2_PLACEMENT_3D ( 'NONE', #82025, #33513, #41055 ) ;
#4391 = VERTEX_POINT ( 'NONE', #26909 ) ;
#4390 = CARTESIAN_POINT ( 'NONE',  ( -32.43176025746394231, 464.5282231482061661, 9.485014939603443551 ) ) ;
#4392 = CARTESIAN_POINT ( 'NONE',  ( 80.86826994178642281, -56.92707617347908666, 177.6008734011382160 ) ) ;
#4393 = CARTESIAN_POINT ( 'NONE',  ( 7.849088119671323582, 81.59499423012449881, 1.301042606982605321E-15 ) ) ;
#4394 = CONICAL_SURFACE ( 'NONE', #91998, 4.000000000000001776, 0.9599310885968808105 ) ;
#4395 = DIRECTION ( 'NONE',  ( 0.000000000000000000, 0.000000000000000000, -1.000000000000000000 ) ) ;
#4396 = ORIENTED_EDGE ( 'NONE', *, *, #95242, .T. ) ;
#4397 = CARTESIAN_POINT ( 'NONE',  ( -33.19020058218139013, 314.4820628366123856, -7.226409737576505066 ) ) ;
#4398 = CARTESIAN_POINT ( 'NONE',  ( -47.29141116144595003, 18.29911311166173959, 14.59113362281949655 ) ) ;
#4399 = LINE ( 'NONE', #12471, #85192 ) ;
#4400 = CONICAL_SURFACE ( 'NONE', #106005, 4.172000000000009479, 0.9599310885968813656 ) ;
#4401 = CARTESIAN_POINT ( 'NONE',  ( -4.595881407952570719, 251.0662543320131874, -3.857520671226069897 ) ) ;
#4402 = CARTESIAN_POINT ( 'NONE',  ( -20.70020626257101526, 302.9146223833919294, 9.950651519756169350 ) ) ;
#4403 = EDGE_CURVE ( 'NONE', #64826, #93842, #88234, .T. ) ;
#4404 = ORIENTED_EDGE ( 'NONE', *, *, #78238, .F. ) ;
#4405 = PRODUCT_CONTEXT ( 'NONE', #102408, 'mechanical' ) ;
#4406 = CARTESIAN_POINT ( 'NONE',  ( -80.64775485730676508, -30.00000000000000355, -12.74855559745246225 ) ) ;
#4407 = CARTESIAN_POINT ( 'NONE',  ( -5.000000000000000000, -46.95680582063142339, 6.322184883410053580 ) ) ;
#4408 = CARTESIAN_POINT ( 'NONE',  ( 0.000000000000000000, 4.898587196589412829E-16, -4.000000000000000000 ) ) ;
#4409 = EDGE_CURVE ( 'NONE', #21060, #4006, #29052, .T. ) ;
#4410 = CARTESIAN_POINT ( 'NONE',  ( 0.000000000000000000, 0.000000000000000000, 0.000000000000000000 ) ) ;
#4411 = CARTESIAN_POINT ( 'NONE',  ( -2.977408999572650039, -20.18750000204838457, -7.188101187500001821 ) ) ;
#4412 = DIRECTION ( 'NONE',  ( 1.000000000000000000, 0.000000000000000000, 0.000000000000000000 ) ) ;
#4413 = DIRECTION ( 'NONE',  ( 0.000000000000000000, 0.000000000000000000, 1.000000000000000000 ) ) ;
#4414 = CARTESIAN_POINT ( 'NONE',  ( 20.11650669486618881, 4.898587196589413815E-16, -4.000000000000000888 ) ) ;
#4415 = ITEM_DEFINED_TRANSFORMATION ( 'NONE', 'NONE', #28333,  #10728 ) ;
#4416 = VERTEX_POINT ( 'NONE', #103931 ) ;
#4417 = EDGE_CURVE ( 'NONE', #28073, #21338, #103411, .T. ) ;
#4418 = CARTESIAN_POINT ( 'NONE',  ( -35.44924304867188880, 490.5768697630985571, 12.28200392830173726 ) ) ;
#4419 = LINE ( 'NONE', #37357, #37548 ) ;
#4420 = AXIS2_PLACEMENT_3D ( 'NONE', #13735, #95736, #15338 ) ;
#4421 = CARTESIAN_POINT ( 'NONE',  ( -9.832775749609577787, 7.875845744895693556, 0.000000000000000000 ) ) ;
#4422 =( NAMED_UNIT ( * ) PLANE_ANGLE_UNIT ( ) SI_UNIT ( $, .RADIAN. ) );
#4423 = ORIENTED_EDGE ( 'NONE', *, *, #5283, .F. ) ;
#4424 = LINE ( 'NONE', #37362, #84292 ) ;
#4425 = CARTESIAN_POINT ( 'NONE',  ( 7.717304146821367894, 50.00000000000000000, -95.65871486498016907 ) ) ;
#4426 = ORIENTED_EDGE ( 'NONE', *, *, #66495, .F. ) ;
#4427 = CARTESIAN_POINT ( 'NONE',  ( -28.31493636581005546, 34.24499175938969842, 8.451752357833321128 ) ) ;
#4428 = CARTESIAN_POINT ( 'NONE',  ( 8.559508646656407649, -1.200000000000000030E-05, 2.781152949374444461 ) ) ;
#4429 = CARTESIAN_POINT ( 'NONE',  ( 9.989285784994811124, 101.0265757255430117, 0.5301777604595964144 ) ) ;
#4430 = CARTESIAN_POINT ( 'NONE',  ( -102.6181093806218456, -60.00000000000000711, 200.8243356994102271 ) ) ;
#4431 = SURFACE_STYLE_USAGE ( .BOTH. , #30321 ) ;
#4432 = DIRECTION ( 'NONE',  ( 0.000000000000000000, 0.000000000000000000, 1.000000000000000000 ) ) ;
#4433 = CYLINDRICAL_SURFACE ( 'NONE', #28858, 15.00000000000001243 ) ;
#4434 = FILL_AREA_STYLE_COLOUR ( '', #50862 ) ;
#4435 = CARTESIAN_POINT ( 'NONE',  ( -82.00017004842651147, -60.72289651137820954, 187.9292513951569674 ) ) ;
#4436 = STYLED_ITEM ( 'NONE', ( #31381 ), #65343 ) ;
#4437 = CARTESIAN_POINT ( 'NONE',  ( 26.15549530965961011, 43.57015600928786370, -74.54213887132672767 ) ) ;
#4438 = EDGE_LOOP ( 'NONE', ( #105282, #97923, #82329, #52310, #58613 ) ) ;
#4439 = FACE_OUTER_BOUND ( 'NONE', #3661, .T. ) ;
#4440 = EDGE_CURVE ( 'NONE', #20019, #32527, #94329, .T. ) ;
#4442 = DIRECTION ( 'NONE',  ( 0.000000000000000000, -1.000000000000000000, 0.000000000000000000 ) ) ;
#4441 = CIRCLE ( 'NONE', #14750, 66.00000000000000000 ) ;
#4443 = CARTESIAN_POINT ( 'NONE',  ( -84.42099871513350706, -45.26547612325662584, 28.59035868857876039 ) ) ;
#4444 = FACE_OUTER_BOUND ( 'NONE', #55660, .T. ) ;
#4445 = COLOUR_RGB ( '', 0.72549020, 0.75294118, 0.79215686) ;
#4446 = CARTESIAN_POINT ( 'NONE',  ( 9.609486011791064541, 143.0915023496501419, -5.000000000000000888 ) ) ;
#4447 = CARTESIAN_POINT ( 'NONE',  ( -6.269955739554010421, -4.268932597852962196, -6.443844059477448205 ) ) ;
#4448 = CARTESIAN_POINT ( 'NONE',  ( -23.57730434129643626, 18.64316884713158728, -30.67950393661452679 ) ) ;
#4449 = ADVANCED_FACE ( 'NONE', ( #22527 ), #47645, .T. ) ;
#4450 = CARTESIAN_POINT ( 'NONE',  ( 107.5269304809499431, -60.00000000000002132, 200.1385401206229062 ) ) ;
#4451 = CARTESIAN_POINT ( 'NONE',  ( -39.18206537991729022, 57.18445727710330573, -19.59103268995865221 ) ) ;
#4452 = CARTESIAN_POINT ( 'NONE',  ( -95.66383100604464573, -60.00000000000002132, 35.18327952992021324 ) ) ;
#4453 = CARTESIAN_POINT ( 'NONE',  ( -62.37994538018725166, -60.34609847077623357, 89.28735657275996118 ) ) ;
#4454 = AXIS2_PLACEMENT_3D ( 'NONE', #949, #50581, #34468 ) ;
#4455 = ORIENTED_EDGE ( 'NONE', *, *, #79542, .F. ) ;
#4456 = CARTESIAN_POINT ( 'NONE',  ( 102.0109750195309175, -30.00000000000007816, 198.2012210982776708 ) ) ;
#4457 = CARTESIAN_POINT ( 'NONE',  ( 56.10215434529457923, 39.42619182473122663, -33.37226973483742398 ) ) ;
#4458 = CARTESIAN_POINT ( 'NONE',  ( 78.54918379967675435, -59.99999999999753442, 198.2828222273666086 ) ) ;
#4459 = AXIS2_PLACEMENT_3D ( 'NONE', #79437, #5549, #96694 ) ;
#4461 = EDGE_LOOP ( 'NONE', ( #44124, #96132, #37187, #39749 ) ) ;
#4460 = CIRCLE ( 'NONE', #45815, 4.000000000000007105 ) ;
#4462 = CARTESIAN_POINT ( 'NONE',  ( -33.83651168700076539, 463.7543666047556599, 7.167145050625423508 ) ) ;
#4464 = VECTOR ( 'NONE', #43185, 1000.000000000000000 ) ;
#4463 = CARTESIAN_POINT ( 'NONE',  ( -5.082755093536325042, -21.96875000204838457, -5.082755093536325930 ) ) ;
#4465 = ADVANCED_FACE ( 'NONE', ( #45708 ), #47284, .F. ) ;
#4466 = VERTEX_POINT ( 'NONE', #55370 ) ;
#4467 = PRODUCT_DEFINITION_SHAPE ( 'NONE', 'NONE',  #106791 ) ;
#4468 = CARTESIAN_POINT ( 'NONE',  ( 32.61650669486618881, 1.474610560812782335E-15, 0.000000000000000000 ) ) ;
#4469 = ORIENTED_EDGE ( 'NONE', *, *, #21854, .T. ) ;
#4470 = CARTESIAN_POINT ( 'NONE',  ( -6.821717117272705799, 41.99999999999999289, -69.36621149908677353 ) ) ;
#4471 = FILL_AREA_STYLE ('',( #12019 ) ) ;
#4472 = CARTESIAN_POINT ( 'NONE',  ( -51.23217687371317197, -59.99999999999998579, -37.66347443025715336 ) ) ;
#4473 = CARTESIAN_POINT ( 'NONE',  ( 36.71696399481749751, 413.9589844344937433, 6.177452124062001282 ) ) ;
#4474 = CARTESIAN_POINT ( 'NONE',  ( -7.188101187500001821, -33.87500000204838813, -2.977408999572651371 ) ) ;
#4475 = CARTESIAN_POINT ( 'NONE',  ( -5.000000000000000000, 0.000000000000000000, -0.02540000000000007530 ) ) ;
#4476 = CIRCLE ( 'NONE', #64762, 5.000000000000001776 ) ;
#4477 = DIRECTION ( 'NONE',  ( -1.000000000000000000, -1.224606353822377258E-16, -0.000000000000000000 ) ) ;
#4478 = CARTESIAN_POINT ( 'NONE',  ( 1.000000000000000000, -67.35888985745027924, 11.51944599225194210 ) ) ;
#4479 = CARTESIAN_POINT ( 'NONE',  ( 5.036189802311931807, 48.00000000000000000, -93.73786388412125348 ) ) ;
#4480 = DIRECTION ( 'NONE',  ( 0.000000000000000000, 0.000000000000000000, 1.000000000000000000 ) ) ;
#4481 = DIRECTION ( 'NONE',  ( 1.000000000000000000, 0.000000000000000000, 0.000000000000000000 ) ) ;
#4482 = ADVANCED_FACE ( 'NONE', ( #6288 ), #54294, .T. ) ;
#4483 = DIRECTION ( 'NONE',  ( 0.000000000000000000, 0.000000000000000000, 1.000000000000000000 ) ) ;
#4484 = EDGE_LOOP ( 'NONE', ( #53982, #14772, #1782, #13671, #12838 ) ) ;
#4485 = CARTESIAN_POINT ( 'NONE',  ( -8.559508646656389885, 53.96349637827586321, -1.531152949374502859 ) ) ;
#4486 = CARTESIAN_POINT ( 'NONE',  ( 4.980618096941269002, -3.539029780453324392, 103.2912570477108716 ) ) ;
#4487 = AXIS2_PLACEMENT_3D ( 'NONE', #23117, #21531, #79202 ) ;
#4489 = CARTESIAN_POINT ( 'NONE',  ( 38.04275141536665927, -60.26973243953698045, 41.50661353697247336 ) ) ;
#4488 = CARTESIAN_POINT ( 'NONE',  ( -3.358578016107393260, -49.02765317499757458, 104.2746939430699342 ) ) ;
#4490 = ORIENTED_EDGE ( 'NONE', *, *, #40700, .T. ) ;
#4491 = CARTESIAN_POINT ( 'NONE',  ( -1.308996938995744541, 48.00000000000000711, -95.00000000000001421 ) ) ;
#4493 = CARTESIAN_POINT ( 'NONE',  ( 0.000000000000000000, 6.928203230275505220, 4.000000000000006217 ) ) ;
#4492 = DIRECTION ( 'NONE',  ( -1.000000000000000000, -1.224606353822377258E-16, -0.000000000000000000 ) ) ;
#4494 = CARTESIAN_POINT ( 'NONE',  ( -12.50000000000000178, -3.000000000000000888, -35.13068384735336736 ) ) ;
#4495 = CARTESIAN_POINT ( 'NONE',  ( 5.656854249492380582, -23.00000000409677270, -5.656854249492379694 ) ) ;
#4496 = CARTESIAN_POINT ( 'NONE',  ( -9.500000000000007105, -5.000000000000000000, -52.94236561372732552 ) ) ;
#4497 = CARTESIAN_POINT ( 'NONE',  ( 63.56127108291158123, -4.000000000000000000, 4.898587196589421703E-16 ) ) ;
#4498 = CARTESIAN_POINT ( 'NONE',  ( 42.98746414932995208, 3.851859888774471706E-31, 5.000000000000001776 ) ) ;
#4499 = EDGE_LOOP ( 'NONE', ( #52468, #26034, #25246, #97272, #36737, #95599 ) ) ;
#4500 = CARTESIAN_POINT ( 'NONE',  ( 91.87991718087357640, -60.00000000000000711, 9.797106062246539793 ) ) ;
#4501 = CARTESIAN_POINT ( 'NONE',  ( 28.02682550970785513, 34.39574914770449965, -7.958842414421645195 ) ) ;
#4502 = LINE ( 'NONE', #29871, #97892 ) ;
#4503 = AXIS2_PLACEMENT_3D ( 'NONE', #16811, #65885, #64827 ) ;
#4504 = CARTESIAN_POINT ( 'NONE',  ( -4.881098102818297590, 41.14559805159954919, -70.72437845145068991 ) ) ;
#4505 = DIRECTION ( 'NONE',  ( 0.000000000000000000, 0.000000000000000000, -1.000000000000000000 ) ) ;
#4506 = ORIENTED_EDGE ( 'NONE', *, *, #103491, .F. ) ;
#4507 = CARTESIAN_POINT ( 'NONE',  ( -87.30396544109028412, -29.99999999998607336, 198.3586875667010645 ) ) ;
#4508 = VERTEX_POINT ( 'NONE', #78592 ) ;
#4509 = DIRECTION ( 'NONE',  ( 1.150791560227848051E-16, -0.3420201433256733758, 0.9396926207859066515 ) ) ;
#4510 = CARTESIAN_POINT ( 'NONE',  ( 6.394343112843833943, 7.552705921139272860, 1.203258575478541822E-16 ) ) ;
#4511 = CARTESIAN_POINT ( 'NONE',  ( 14.81542429969936592, 22.88666905516098282, 2.089502384928102252 ) ) ;
#4512 = DIRECTION ( 'NONE',  ( 0.000000000000000000, 0.000000000000000000, 1.000000000000000000 ) ) ;
#4513 = CARTESIAN_POINT ( 'NONE',  ( -7.188101187500002709, -33.68750000204839523, 2.977408999572648707 ) ) ;
#4514 = CARTESIAN_POINT ( 'NONE',  ( -17.98970702557545920, 45.00000000000000711, 62.57427701062805170 ) ) ;
#4515 = CARTESIAN_POINT ( 'NONE',  ( 32.22120753352783140, 464.6691781026584636, 10.60621122532586291 ) ) ;
#4516 =( NAMED_UNIT ( * ) SI_UNIT ( $, .STERADIAN. ) SOLID_ANGLE_UNIT ( ) );
#4517 = VERTEX_POINT ( 'NONE', #13318 ) ;
#4519 = EDGE_LOOP ( 'NONE', ( #32835, #72333, #11848, #25311 ) ) ;
#4518 = SURFACE_STYLE_FILL_AREA ( #86535 ) ;
#4520 = CARTESIAN_POINT ( 'NONE',  ( 79.94750706239578619, -25.61877512049329297, 131.8648424581376730 ) ) ;
#4521 = AXIS2_PLACEMENT_3D ( 'NONE', #66192, #16045, #48927 ) ;
#4522 = CARTESIAN_POINT ( 'NONE',  ( 15.37029426978700641, 3.165964433755443785, 3.249157221777043691 ) ) ;
#4523 = ORIENTED_EDGE ( 'NONE', *, *, #28462, .T. ) ;
#4524 = CARTESIAN_POINT ( 'NONE',  ( -12.50000000000000533, 34.36268320169224921, -53.42085938171843651 ) ) ;
#4525 = CARTESIAN_POINT ( 'NONE',  ( -1.320432766682874540E-15, -19.53125000204838457, 7.188101187500000044 ) ) ;
#4526 =( BOUNDED_CURVE ( )  B_SPLINE_CURVE ( 2, ( #88091, #14171, #47075 ),
 .UNSPECIFIED., .F., .F. ) 
 B_SPLINE_CURVE_WITH_KNOTS ( ( 3, 3 ),
 ( 0.000000000000000000, 1.000000000000000000 ),
 .UNSPECIFIED. ) 
 CURVE ( )  GEOMETRIC_REPRESENTATION_ITEM ( )  RATIONAL_B_SPLINE_CURVE ( ( 1.000000000000000000, 1.857142857142858317, 1.000000000000000000 ) ) 
 REPRESENTATION_ITEM ( '' )  );
#4527 = CARTESIAN_POINT ( 'NONE',  ( -108.9175987578229297, -57.66477069964600588, 197.8260142395344303 ) ) ;
#4528 = EDGE_CURVE ( 'NONE', #37991, #7878, #4641, .T. ) ;
#4529 = AXIS2_PLACEMENT_3D ( 'NONE', #7434, #32286, #47895 ) ;
#4530 = ORIENTED_EDGE ( 'NONE', *, *, #27446, .T. ) ;
#4531 = EDGE_CURVE ( 'NONE', #9380, #74189, #58037, .T. ) ;
#4532 = B_SPLINE_CURVE_WITH_KNOTS ( 'NONE', 3,
 ( #7905, #32756, #96931, #80733, #74238, #89901, #72649, #73161, #31689, #315, #106063, #23602, #33280, #64575, #97441, #99033, #56985, #25198, #89384, #99573, #17623, #66691 ),
 .UNSPECIFIED., .F., .F.,
 ( 4, 2, 2, 2, 2, 2, 2, 2, 2, 2, 4 ),
 ( 0.003183879630746418773, 0.003435849579571543036, 0.003687819528396666865, 0.004191759426046917127, 0.004695699323697167388, 0.005199639221347416781, 0.006207519016647917304, 0.006459488965473041133, 0.006711458914298166697, 0.006963428863123290527, 0.007215398811948416091 ),
 .UNSPECIFIED. ) ;
#4533 = VECTOR ( 'NONE', #67586, 1000.000000000000341 ) ;
#4534 = CARTESIAN_POINT ( 'NONE',  ( 7.039599551806973388, 41.52217469061105959, -58.93052221769676891 ) ) ;
#4535 = EDGE_CURVE ( 'NONE', #62559, #60854, #25281, .T. ) ;
#4536 = CARTESIAN_POINT ( 'NONE',  ( 49.22174280021646808, 12.91003493663461832, -15.98497293138166597 ) ) ;
#4537 = VECTOR ( 'NONE', #48646, 1000.000000000000000 ) ;
#4538 = CARTESIAN_POINT ( 'NONE',  ( 3.313708498984762052, -18.40625000409676915, -8.000000000000000000 ) ) ;
#4539 = VECTOR ( 'NONE', #47731, 1000.000000000000000 ) ;
#4540 = CARTESIAN_POINT ( 'NONE',  ( -49.56313789510318202, -29.60261757400662574, 45.92228025562707927 ) ) ;
#4541 = STYLED_ITEM ( 'NONE', ( #100191 ), #57681 ) ;
#4542 = CARTESIAN_POINT ( 'NONE',  ( -37.56673239365851913, 25.75719283951025673, 10.95617127780993449 ) ) ;
#4543 = VECTOR ( 'NONE', #18409, 1000.000000000000000 ) ;
#4544 = CARTESIAN_POINT ( 'NONE',  ( -1.000000000000000000, -67.04094093996420156, 11.34959271884451937 ) ) ;
#4545 = B_SPLINE_CURVE_WITH_KNOTS ( 'NONE', 3,
 ( #77954, #63385, #36998, #21342, #20840, #87121, #14257, #21872, #96280, #95732, #13195, #12669, #103813, #4069, #22405, #29957, #37535, #54714, #86071, #53670, #55249, #45600, #30484, #78476, #4600, #70399, #70920, #46639, #87649, #13731, #45072 ),
 .UNSPECIFIED., .F., .F.,
 ( 4, 2, 2, 2, 1, 1, 2, 2, 2, 2, 1, 2, 2, 1, 1, 2, 2, 4 ),
 ( 0.5714977658632183211, 0.6250605451303161697, 0.6786233243974139073, 0.6920140192141883695, 0.7054047140309627206, 0.7321861036645116450, 0.7455767984812859961, 0.7589674932980604583, 0.7857488829316092716, 0.8125302725651581959, 0.8393116621987070092, 0.8660930518322558225, 0.8794837466490301736, 0.8928744414658046358, 0.9196558310993534491, 0.9330465259161280223, 0.9464372207329023734, 1.000000000000000000 ),
 .UNSPECIFIED. ) ;
#4546 = CARTESIAN_POINT ( 'NONE',  ( 5.693345022498909280, -2.999999999999138467, -71.09407784968016131 ) ) ;
#4547 = DIRECTION ( 'NONE',  ( 0.6000000000000013101, 0.000000000000000000, 0.7999999999999990452 ) ) ;
#4548 = CARTESIAN_POINT ( 'NONE',  ( 0.000000000000000000, 0.000000000000000000, -7.424942857142857733 ) ) ;
#4549 = ORIENTED_EDGE ( 'NONE', *, *, #62264, .T. ) ;
#4551 = AXIS2_PLACEMENT_3D ( 'NONE', #34691, #59477, #27133 ) ;
#4550 = CARTESIAN_POINT ( 'NONE',  ( -2.301926985296694372, -49.78450636680690877, 44.63741750628801697 ) ) ;
#4552 = EDGE_CURVE ( 'NONE', #54541, #65774, #78072, .T. ) ;
#4553 = CARTESIAN_POINT ( 'NONE',  ( 11.59420250832448218, -4.918022519855804298, -12.56327219346357893 ) ) ;
#4554 = VECTOR ( 'NONE', #66909, 1000.000000000000000 ) ;
#4555 = CARTESIAN_POINT ( 'NONE',  ( -40.96169049688617747, 435.9986040634732376, 6.367590718067607014 ) ) ;
#4556 = CARTESIAN_POINT ( 'NONE',  ( -61.19724114412970550, -29.40090490056691408, -24.55535741776452596 ) ) ;
#4557 = CARTESIAN_POINT ( 'NONE',  ( -66.40962216726373413, -30.00000000000000000, 84.31724798585034364 ) ) ;
#4558 = CARTESIAN_POINT ( 'NONE',  ( 7.500000000000007994, 40.00000000000000000, -71.41947339647144588 ) ) ;
#4559 = ORIENTED_EDGE ( 'NONE', *, *, #4076, .F. ) ;
#4560 = CIRCLE ( 'NONE', #18359, 0.5000000000000004441 ) ;
#4561 = DIRECTION ( 'NONE',  ( 0.000000000000000000, -1.000000000000000000, 0.000000000000000000 ) ) ;
#4562 = CARTESIAN_POINT ( 'NONE',  ( 75.82261830597555274, -57.55065031891655991, 192.7782113498394381 ) ) ;
#4563 = VECTOR ( 'NONE', #19813, 1000.000000000000000 ) ;
#4564 = DIRECTION ( 'NONE',  ( -1.000000000000000000, -0.000000000000000000, -0.000000000000000000 ) ) ;
#4565 = DIRECTION ( 'NONE',  ( 1.000000000000000000, -0.000000000000000000, -0.000000000000000000 ) ) ;
#4566 = CARTESIAN_POINT ( 'NONE',  ( 37.61650669486618881, 4.000000000000003553, 4.898587196589414801E-16 ) ) ;
#4567 = DIRECTION ( 'NONE',  ( 0.000000000000000000, -1.000000000000000000, 0.000000000000000000 ) ) ;
#4568 = PRODUCT_DEFINITION_SHAPE ( 'NONE', 'NONE',  #12664 ) ;
#4569 = CARTESIAN_POINT ( 'NONE',  ( -50.52593252671915991, -60.00000000000000711, 73.12709640751428708 ) ) ;
#4570 =( NAMED_UNIT ( * ) SI_UNIT ( $, .STERADIAN. ) SOLID_ANGLE_UNIT ( ) );
#4571 = CARTESIAN_POINT ( 'NONE',  ( 0.000000000000000000, 44.00000000000000711, 0.000000000000000000 ) ) ;
#4572 = CARTESIAN_POINT ( 'NONE',  ( 58.76133767613618630, 50.00000000000000000, 23.44026136864407306 ) ) ;
#4573 =( GEOMETRIC_REPRESENTATION_CONTEXT ( 3 ) GLOBAL_UNCERTAINTY_ASSIGNED_CONTEXT ( ( #77447 ) ) GLOBAL_UNIT_ASSIGNED_CONTEXT ( ( #69444, #56812, #104437 ) ) REPRESENTATION_CONTEXT ( 'NONE', 'WORKASPACE' ) );
#4574 = CARTESIAN_POINT ( 'NONE',  ( -85.56608911191202083, -39.28323613089826694, 185.6737815819577406 ) ) ;
#4575 = ORIENTED_EDGE ( 'NONE', *, *, #72345, .F. ) ;
#4576 = CARTESIAN_POINT ( 'NONE',  ( 35.31481630306472397, 361.5983975385465214, 3.569375408695424579 ) ) ;
#4577 = CARTESIAN_POINT ( 'NONE',  ( 2.066990665002553832E-05, -35.99444419889723434, 29.88872399275190972 ) ) ;
#4578 = COLOUR_RGB ( '', 0.66274510, 0.83137255, 0.94901961) ;
#4579 = CARTESIAN_POINT ( 'NONE',  ( -6.883638564027164009, 41.77293021818198326, -59.38142135283953138 ) ) ;
#4580 = CARTESIAN_POINT ( 'NONE',  ( 36.49104508226335497, 491.8392457932880575, 12.58580469730120299 ) ) ;
#4581 = PLANE ( 'NONE',  #93940 ) ;
#4582 = EDGE_CURVE ( 'NONE', #3985, #63587, #68939, .T. ) ;
#4583 = CARTESIAN_POINT ( 'NONE',  ( -31.63278175528669323, 313.0349085595907468, -7.829891971190884981 ) ) ;
#4584 = DIRECTION ( 'NONE',  ( 0.000000000000000000, 1.000000000000000000, 0.000000000000000000 ) ) ;
#4585 = CARTESIAN_POINT ( 'NONE',  ( 6.249999999999998224, 0.000000000000000000, 0.000000000000000000 ) ) ;
#4586 = CARTESIAN_POINT ( 'NONE',  ( 9.830769230769229594, 4.172000000000003261, 5.109226446042759579E-16 ) ) ;
#4587 = ORIENTED_EDGE ( 'NONE', *, *, #84416, .F. ) ;
#4588 = CARTESIAN_POINT ( 'NONE',  ( 18.10339634169226741, 50.00000000000001421, 61.75574722958666740 ) ) ;
#4589 = CARTESIAN_POINT ( 'NONE',  ( 10.88898873136430900, 9.029852970804380874, 10.01842208923438093 ) ) ;
#4590 = EDGE_CURVE ( 'NONE', #10855, #92963, #1119, .T. ) ;
#4591 = EDGE_CURVE ( 'NONE', #87758, #56514, #97969, .T. ) ;
#4592 = CARTESIAN_POINT ( 'NONE',  ( -6.601913983209747983, -4.285714285713511096, 24.56594385547482418 ) ) ;
#4593 = PRESENTATION_STYLE_ASSIGNMENT (( #43984 ) ) ;
#4594 = CARTESIAN_POINT ( 'NONE',  ( 87.30924545702741568, -14.21045842199429998, 28.19131950638903206 ) ) ;
#4595 = CARTESIAN_POINT ( 'NONE',  ( -81.46110316675287777, -22.15507786611714636, 136.5093758021127996 ) ) ;
#4596 = ORIENTED_EDGE ( 'NONE', *, *, #85346, .F. ) ;
#4597 = FACE_OUTER_BOUND ( 'NONE', #96513, .T. ) ;
#4598 =( LENGTH_UNIT ( ) NAMED_UNIT ( * ) SI_UNIT ( .MILLI., .METRE. ) );
#4599 = APPLICATION_CONTEXT ( 'automotive_design' ) ;
#4600 = CARTESIAN_POINT ( 'NONE',  ( 61.03799250145893751, 50.00000000000002132, -15.95017878592576110 ) ) ;
#4601 = UNCERTAINTY_MEASURE_WITH_UNIT (LENGTH_MEASURE( 1.000000000000000082E-05 ), #46399, 'distance_accuracy_value', 'NONE');
#4602 = CIRCLE ( 'NONE', #13197, 0.9999999999999998890 ) ;
#4603 = CARTESIAN_POINT ( 'NONE',  ( 43.46308961903932300, 361.0392705997022631, 12.69300088796138226 ) ) ;
#4604 = CARTESIAN_POINT ( 'NONE',  ( -43.41290683822509067, 487.0833545439620593, 7.569976829064872348 ) ) ;
#4605 = ORIENTED_EDGE ( 'NONE', *, *, #25954, .F. ) ;
#4606 = CIRCLE ( 'NONE', #8042, 4.000000000000000888 ) ;
#4607 = CARTESIAN_POINT ( 'NONE',  ( 5.290067270632157204, 54.20842449845687838, -6.031152949374584793 ) ) ;
#4608 = CARTESIAN_POINT ( 'NONE',  ( 16.32209425763040755, 43.86680992065402052, 4.189051175685120754 ) ) ;
#4609 = CARTESIAN_POINT ( 'NONE',  ( -7.188101187500000044, -22.90625000204838457, -8.802885111219163269E-16 ) ) ;
#4610 = DIRECTION ( 'NONE',  ( 0.000000000000000000, -1.000000000000000000, 0.000000000000000000 ) ) ;
#4611 = ADVANCED_FACE ( 'NONE', ( #73683 ), #8950, .T. ) ;
#4612 = CARTESIAN_POINT ( 'NONE',  ( 6.928203230275509661, -65.00000000000000000, -4.000000000000002665 ) ) ;
#4613 = CARTESIAN_POINT ( 'NONE',  ( 5.892296920977983632, 42.00785640420587441, -69.46301655925690000 ) ) ;
#4614 = CARTESIAN_POINT ( 'NONE',  ( 27.10511071441197117, 36.60571256639528315, 10.05698433968570704 ) ) ;
#4615 = DIRECTION ( 'NONE',  ( -1.000000000000000000, -1.224606353822377258E-16, -0.000000000000000000 ) ) ;
#4616 = EDGE_CURVE ( 'NONE', #2439, #23591, #30352, .T. ) ;
#4617 = CARTESIAN_POINT ( 'NONE',  ( -23.97722388339740007, 27.87827700592711722, -30.95083563548404015 ) ) ;
#4618 = ORIENTED_EDGE ( 'NONE', *, *, #27844, .T. ) ;
#4619 = CARTESIAN_POINT ( 'NONE',  ( 2.216488688100098248, 14.30876692738955924, -12.46553453015539503 ) ) ;
#4620 = AXIS2_PLACEMENT_3D ( 'NONE', #35109, #52851, #59368 ) ;
#4621 = VECTOR ( 'NONE', #12129, 1000.000000000000000 ) ;
#4623 = CARTESIAN_POINT ( 'NONE',  ( 27.94074522160097018, -39.48070956748559723, 32.48135008067870189 ) ) ;
#4622 = CARTESIAN_POINT ( 'NONE',  ( -46.52099778141491271, -60.00000000000009948, 69.35786614446448084 ) ) ;
#4624 = CARTESIAN_POINT ( 'NONE',  ( 6.136456400494866826E-15, 53.37899725327129374, -25.05398456423234066 ) ) ;
#4625 = EDGE_LOOP ( 'NONE', ( #54639, #29857, #44064 ) ) ;
#4626 = EDGE_CURVE ( 'NONE', #85522, #2566, #20145, .T. ) ;
#4627 = ORIENTED_EDGE ( 'NONE', *, *, #39626, .T. ) ;
#4628 = COLOUR_RGB ( '', 0.31764706, 0.68627451, 0.89019608) ;
#4629 = CARTESIAN_POINT ( 'NONE',  ( -12.64023069600374249, -4.285714285714296246, -21.88880945939638778 ) ) ;
#4630 =( GEOMETRIC_REPRESENTATION_CONTEXT ( 3 ) GLOBAL_UNCERTAINTY_ASSIGNED_CONTEXT ( ( #7071 ) ) GLOBAL_UNIT_ASSIGNED_CONTEXT ( ( #3639, #94789, #8394 ) ) REPRESENTATION_CONTEXT ( 'NONE', 'WORKASPACE' ) );
#4631 = CARTESIAN_POINT ( 'NONE',  ( 7.380473217280480114, 40.84000775496618729, -58.87770853468460075 ) ) ;
#4632 = AXIS2_PLACEMENT_3D ( 'NONE', #12934, #20034, #70127 ) ;
#4633 = CARTESIAN_POINT ( 'NONE',  ( 34.47678062874018678, 436.2905755606503817, 4.953078263945744908 ) ) ;
#4634 = EDGE_CURVE ( 'NONE', #36922, #17355, #81761, .T. ) ;
#4635 = CARTESIAN_POINT ( 'NONE',  ( 12.13435171257998846, 2.003356828137956569, 14.86647337586970785 ) ) ;
#4636 = CARTESIAN_POINT ( 'NONE',  ( 0.2578475836320734405, -6.890627091270379090, -1.065083781909172078 ) ) ;
#4637 = ORIENTED_EDGE ( 'NONE', *, *, #3451, .F. ) ;
#4638 = PRESENTATION_STYLE_ASSIGNMENT (( #53705 ) ) ;
#4639 = CARTESIAN_POINT ( 'NONE',  ( 91.77464836895023836, -29.99999999999999289, 98.58162192422200576 ) ) ;
#4640 = CARTESIAN_POINT ( 'NONE',  ( -10.15339062455847774, 12.11279177272005114, 10.55309804651484917 ) ) ;
#4641 = CIRCLE ( 'NONE', #57967, 4.172000000000001485 ) ;
#4642 = CARTESIAN_POINT ( 'NONE',  ( -5.191144708981714651, -82.35969914478735632, 3.015512395308853844 ) ) ;
#4643 = CARTESIAN_POINT ( 'NONE',  ( 81.59421194845130287, -30.00000000000000355, -6.849562237453022284 ) ) ;
#4644 = CARTESIAN_POINT ( 'NONE',  ( 0.000000000000000000, 48.50000000000000000, 0.000000000000000000 ) ) ;
#4645 = ORIENTED_EDGE ( 'NONE', *, *, #49109, .T. ) ;
#4646 = ORIENTED_EDGE ( 'NONE', *, *, #10088, .T. ) ;
#4647 = EDGE_LOOP ( 'NONE', ( #46310, #82931, #51409, #18473 ) ) ;
#4648 = DIRECTION ( 'NONE',  ( 0.000000000000000000, 0.000000000000000000, -1.000000000000000000 ) ) ;
#4649 = DIRECTION ( 'NONE',  ( 0.000000000000000000, -1.000000000000000000, 0.000000000000000000 ) ) ;
#4650 = DIRECTION ( 'NONE',  ( 0.000000000000000000, 1.000000000000000000, -0.000000000000000000 ) ) ;
#4651 = CARTESIAN_POINT ( 'NONE',  ( -43.60048788927255004, 433.3707788411693400, 14.72783989749648370 ) ) ;
#4652 =( LENGTH_UNIT ( ) NAMED_UNIT ( * ) SI_UNIT ( .MILLI., .METRE. ) );
#4653 = CARTESIAN_POINT ( 'NONE',  ( 0.000000000000000000, 25.16329480281783759, 0.000000000000000000 ) ) ;
#4654 = CARTESIAN_POINT ( 'NONE',  ( 0.000000000000000000, 80.00000000000000000, 0.000000000000000000 ) ) ;
#4655 = VERTEX_POINT ( 'NONE', #48341 ) ;
#4656 = CARTESIAN_POINT ( 'NONE',  ( 8.737863884125493641, 48.00000000000000000, -90.03618980230170621 ) ) ;
#4657 = VERTEX_POINT ( 'NONE', #7882 ) ;
#4658 = CARTESIAN_POINT ( 'NONE',  ( -5.475947152006324536, -61.83782269890877359, 2.462898245435129585 ) ) ;
#4659 = CARTESIAN_POINT ( 'NONE',  ( 42.23079339798723453, 461.4509360991310132, 2.027626716395714901 ) ) ;
#4660 = CARTESIAN_POINT ( 'NONE',  ( 41.36650669486618881, 4.000000000000003553, 4.898587196589414801E-16 ) ) ;
#4661 = CARTESIAN_POINT ( 'NONE',  ( 22.33420830224751086, 303.2829233726812959, 10.02965477944128736 ) ) ;
#4662 = AXIS2_PLACEMENT_3D ( 'NONE', #42257, #49278, #75147 ) ;
#4663 = CARTESIAN_POINT ( 'NONE',  ( 9.404048505571516614, 302.6623157415702394, -10.04027336087706246 ) ) ;
#4664 = CARTESIAN_POINT ( 'NONE',  ( 64.22169963983361640, -25.57819097122271756, 76.81871742320117846 ) ) ;
#4665 = ORIENTED_EDGE ( 'NONE', *, *, #37443, .T. ) ;
#4666 = CARTESIAN_POINT ( 'NONE',  ( 16.75187969033515145, 34.25544727262118982, -24.30698433968624883 ) ) ;
#4667 = CIRCLE ( 'NONE', #20259, 7.500000000000003553 ) ;
#4668 = CARTESIAN_POINT ( 'NONE',  ( -46.45064480349970637, -34.72776456001106737, -36.68816489433520189 ) ) ;
#4669 = DIRECTION ( 'NONE',  ( -1.000000000000000000, -1.224606353822377258E-16, -0.000000000000000000 ) ) ;
#4670 = CARTESIAN_POINT ( 'NONE',  ( 62.33904886068935980, 6.975173280561618775E-15, 0.000000000000000000 ) ) ;
#4671 = EDGE_CURVE ( 'NONE', #88549, #34518, #59761, .T. ) ;
#4672 = EDGE_LOOP ( 'NONE', ( #81577, #3302, #69412, #5799 ) ) ;
#4673 = FILL_AREA_STYLE_COLOUR ( '', #28039 ) ;
#4674 = CARTESIAN_POINT ( 'NONE',  ( 7.002641335706727865, 28.94912737319167917, 3.868676264653293284 ) ) ;
#4675 = CARTESIAN_POINT ( 'NONE',  ( 43.03894652950350519, 464.9992092536281802, 11.55502599541015840 ) ) ;
#4676 = ADVANCED_FACE ( 'NONE', ( #41324 ), #80365, .F. ) ;
#4677 = CARTESIAN_POINT ( 'NONE',  ( 0.000000000000000000, 0.000000000000000000, 0.000000000000000000 ) ) ;
#4678 = EDGE_CURVE ( 'NONE', #75707, #32369, #36871, .T. ) ;
#4679 = CARTESIAN_POINT ( 'NONE',  ( -2.576959554038571877E-15, 37.86482112153537116, -10.52123582012687919 ) ) ;
#4680 = CARTESIAN_POINT ( 'NONE',  ( 31.96161004470365086, 465.6201165449652990, 10.43791023679830587 ) ) ;
#4681 = CARTESIAN_POINT ( 'NONE',  ( 85.01337858154622040, -61.07969618245190446, 193.5080867132440687 ) ) ;
#4682 = EDGE_CURVE ( 'NONE', #80415, #83228, #77908, .T. ) ;
#4683 = CARTESIAN_POINT ( 'NONE',  ( -5.307398959431215424, 21.45645744618504480, -40.53500383443203248 ) ) ;
#4684 = MECHANICAL_DESIGN_GEOMETRIC_PRESENTATION_REPRESENTATION (  '', ( #94301 ), #44329 ) ;
#4685 = CARTESIAN_POINT ( 'NONE',  ( -9.692620405620905544, 8.443756516928340616, 4.999999999999841904 ) ) ;
#4686 = CARTESIAN_POINT ( 'NONE',  ( 7.896571385775229324, -6.210020006542475990, 1.305932416347438618 ) ) ;
#4687 = CARTESIAN_POINT ( 'NONE',  ( 13.87389654945780215, -50.52883469042527764, 25.11216171227248850 ) ) ;
#4688 = EDGE_CURVE ( 'NONE', #23419, #51169, #94179, .T. ) ;
#4689 = CARTESIAN_POINT ( 'NONE',  ( 32.99999999999999289, 435.0774731480752280, 11.67986145722082014 ) ) ;
#4690 = EDGE_CURVE ( 'NONE', #63779, #48529, #61465, .T. ) ;
#4691 = CARTESIAN_POINT ( 'NONE',  ( -100.3761925564723754, -29.99999999999999289, 157.7587148953477652 ) ) ;
#4692 = AXIS2_PLACEMENT_3D ( 'NONE', #69455, #3659, #35516 ) ;
#4693 = CARTESIAN_POINT ( 'NONE',  ( 24.34999999999999787, 3.309500000000003439, 0.000000000000000000 ) ) ;
#4694 = CARTESIAN_POINT ( 'NONE',  ( 8.463560105336789263, -57.67125183312073489, 41.60408020090174119 ) ) ;
#4696 = FACE_BOUND ( 'NONE', #66261, .T. ) ;
#4695 = CARTESIAN_POINT ( 'NONE',  ( 12.28614183020320993, 9.928251283239491798, -9.534296537348968315 ) ) ;
#4697 =( BOUNDED_SURFACE ( )  B_SPLINE_SURFACE ( 2, 3, ( 
 ( #36224, #77173, #84201, #60483, #35143, #69093, #68565, #59408, #85817, #61542 ),
 ( #2195, #69620, #12417, #102512, #2735, #18425, #28127, #53433, #101967, #92816 ),
 ( #84732, #77707, #43210, #93363, #51280, #27603, #10297, #61004, #76095, #19516 ) ),
 .UNSPECIFIED., .F., .F., .F. ) 
 B_SPLINE_SURFACE_WITH_KNOTS ( ( 3, 3 ),
 ( 4, 2, 2, 2, 4 ),
 ( 0.000000000000000000, 1.000000000000000000 ),
 ( -0.000000000000000000, 0.001626978433639921992, 0.003253956867279843984, 0.004880935300919765976, 0.006507913734559687968 ),
 .UNSPECIFIED. ) 
 GEOMETRIC_REPRESENTATION_ITEM ( )  RATIONAL_B_SPLINE_SURFACE ( (
 ( 1.000000000000000000, 1.000000000000000000, 1.000000000000000000, 1.000000000000000000, 1.000000000000000000, 1.000000000000000000, 1.000000000000000000, 1.000000000000000000, 1.000000000000000000, 1.000000000000000000),
 ( 1.857142857142858317, 1.857142857142858317, 1.857142857142858317, 1.857142857142858317, 1.857142857142858317, 1.857142857142858317, 1.857142857142858317, 1.857142857142858317, 1.857142857142858317, 1.857142857142858317),
 ( 1.000000000000000000, 1.000000000000000000, 1.000000000000000000, 1.000000000000000000, 1.000000000000000000, 1.000000000000000000, 1.000000000000000000, 1.000000000000000000, 1.000000000000000000, 1.000000000000000000) ) ) 
 REPRESENTATION_ITEM ( '' )  SURFACE ( )  );
#4698 = CARTESIAN_POINT ( 'NONE',  ( -41.16726895037174216, 460.1166845890182344, 2.127318685287579836 ) ) ;
#4699 = CARTESIAN_POINT ( 'NONE',  ( -32.17646412119387378, 464.6980787822280377, 10.84896803612861227 ) ) ;
#4700 = CARTESIAN_POINT ( 'NONE',  ( -46.00000000000000000, 461.9428920847514632, 12.03309428281624172 ) ) ;
#4701 = CIRCLE ( 'NONE', #42561, 12.16579798332631945 ) ;
#4702 = VECTOR ( 'NONE', #84172, 1000.000000000000000 ) ;
#4703 =( BOUNDED_CURVE ( )  B_SPLINE_CURVE ( 2, ( #46827, #21014, #12856, #95923, #45774, #102417, #103473, #54359, #97485 ),
 .UNSPECIFIED., .F., .F. ) 
 B_SPLINE_CURVE_WITH_KNOTS ( ( 3, 2, 2, 2, 3 ),
 ( 0.8970588235294117974, 0.9044117647058823595, 0.9117647058823529216, 0.9191176470588234837, 0.9264705882352941568 ),
 .UNSPECIFIED. ) 
 CURVE ( )  GEOMETRIC_REPRESENTATION_ITEM ( )  RATIONAL_B_SPLINE_CURVE ( ( 1.000000000000000000, 0.9238795325112867385, 1.000000000000000000, 0.9238795325112867385, 1.000000000000000000, 0.9238795325112867385, 1.000000000000000000, 0.9238795325112867385, 1.000000000000000000 ) ) 
 REPRESENTATION_ITEM ( '' )  );
#4704 = CARTESIAN_POINT ( 'NONE',  ( 0.000000000000000000, 0.000000000000000000, -60.00000000000000000 ) ) ;
#4705 = ORIENTED_EDGE ( 'NONE', *, *, #34689, .F. ) ;
#4706 = CARTESIAN_POINT ( 'NONE',  ( 39.83118896912491635, 485.8577528566769388, -4.999724294277989145 ) ) ;
#4707 = CARTESIAN_POINT ( 'NONE',  ( 38.16398975109107994, 438.4461414108280337, 23.47828886419992145 ) ) ;
#4708 = AXIS2_PLACEMENT_3D ( 'NONE', #66378, #47536, #57738 ) ;
#4709 = CARTESIAN_POINT ( 'NONE',  ( -14.66631300009641947, -46.43930650983597985, 31.75654908330537296 ) ) ;
#4711 = CARTESIAN_POINT ( 'NONE',  ( 0.000000000000000000, -1.200000000000000030E-05, -16.25000000000000000 ) ) ;
#4710 = DIRECTION ( 'NONE',  ( 0.000000000000000000, -1.000000000000000000, 0.000000000000000000 ) ) ;
#4712 = EDGE_LOOP ( 'NONE', ( #27252, #30873, #4253, #22693, #23481, #104507 ) ) ;
#4713 = DIRECTION ( 'NONE',  ( -8.881784197001251337E-16, 0.000000000000000000, 1.000000000000000000 ) ) ;
#4714 = EDGE_CURVE ( 'NONE', #99250, #60578, #26567, .T. ) ;
#4715 = DIRECTION ( 'NONE',  ( 0.000000000000000000, 0.000000000000000000, 1.000000000000000000 ) ) ;
#4716 = VECTOR ( 'NONE', #46555, 1000.000000000000000 ) ;
#4717 = CARTESIAN_POINT ( 'NONE',  ( -27.47093694407817210, 296.2799286419132727, -9.692114557244172701 ) ) ;
#4718 = ORIENTED_EDGE ( 'NONE', *, *, #100847, .T. ) ;
#4719 = FACE_OUTER_BOUND ( 'NONE', #90286, .T. ) ;
#4720 = FILL_AREA_STYLE ('',( #21455 ) ) ;
#4722 = CARTESIAN_POINT ( 'NONE',  ( 43.88846153846154152, 1.411358822780289120E-15, 0.000000000000000000 ) ) ;
#4721 = FACE_OUTER_BOUND ( 'NONE', #15881, .T. ) ;
#4723 = MECHANICAL_DESIGN_GEOMETRIC_PRESENTATION_REPRESENTATION (  '', ( #87431 ), #68482 ) ;
#4724 = ORIENTED_EDGE ( 'NONE', *, *, #10691, .T. ) ;
#4725 = VERTEX_POINT ( 'NONE', #84456 ) ;
#4726 = AXIS2_PLACEMENT_3D ( 'NONE', #18404, #41591, #99822 ) ;
#4727 = ORIENTED_EDGE ( 'NONE', *, *, #79110, .F. ) ;
#4728 =( LENGTH_UNIT ( ) NAMED_UNIT ( * ) SI_UNIT ( .MILLI., .METRE. ) );
#4729 = EDGE_CURVE ( 'NONE', #40108, #71499, #92461, .T. ) ;
#4730 = CARTESIAN_POINT ( 'NONE',  ( 4.898587196589412829E-16, -13.81250000409676915, -8.000000000000000000 ) ) ;
#4731 = DIRECTION ( 'NONE',  ( -0.06744659395726224083, -0.6445107564549500401, 0.7616146281272652141 ) ) ;
#4732 = ORIENTED_EDGE ( 'NONE', *, *, #20921, .F. ) ;
#4733 = CARTESIAN_POINT ( 'NONE',  ( -6.762666706417072682, 41.72339003058417006, -70.10115393879142687 ) ) ;
#4734 = CARTESIAN_POINT ( 'NONE',  ( -44.76546953684172792, -60.00000000001929834, -41.27300769871817465 ) ) ;
#4735 = CARTESIAN_POINT ( 'NONE',  ( 43.59756234217316972, 434.3244621007173123, 14.55946156040339368 ) ) ;
#4736 = CARTESIAN_POINT ( 'NONE',  ( 36.34800668462530382, -60.00000000000000000, -42.52793270410367654 ) ) ;
#4737 = DIRECTION ( 'NONE',  ( -0.000000000000000000, -1.000000000000000000, -0.000000000000000000 ) ) ;
#4738 = CARTESIAN_POINT ( 'NONE',  ( -6.492510984469592294, 41.78432685485347520, -59.03546988472429291 ) ) ;
#4740 = CARTESIAN_POINT ( 'NONE',  ( 7.997113486846998853, -18.58630230906148739, 26.97986963482658496 ) ) ;
#4739 = CARTESIAN_POINT ( 'NONE',  ( -103.2297580319645220, -60.00000000000001421, 85.94764253490394879 ) ) ;
#4741 = CARTESIAN_POINT ( 'NONE',  ( 10.11650669486618881, 1.474610560812782335E-15, 0.000000000000000000 ) ) ;
#4742 = VECTOR ( 'NONE', #69101, 1000.000000000000000 ) ;
#4743 = CARTESIAN_POINT ( 'NONE',  ( -47.98399617180434262, -46.44468898856910499, 49.73485108116536679 ) ) ;
#4744 = CARTESIAN_POINT ( 'NONE',  ( -7.054523059426880849, 41.71556238290650498, -59.55896278357374740 ) ) ;
#4745 = ORIENTED_EDGE ( 'NONE', *, *, #9734, .F. ) ;
#4746 = CARTESIAN_POINT ( 'NONE',  ( 0.6187971826122187213, 13.31391316207858644, -49.41005251785713170 ) ) ;
#4747 = FACE_BOUND ( 'NONE', #34920, .T. ) ;
#4748 = EDGE_CURVE ( 'NONE', #23687, #78599, #34869, .T. ) ;
#4749 = CARTESIAN_POINT ( 'NONE',  ( 4.472135954999581386, -10.00000000000000888, -4.000000000000000000 ) ) ;
#4750 = EDGE_LOOP ( 'NONE', ( #48596, #83360, #63962, #13891 ) ) ;
#4751 = CARTESIAN_POINT ( 'NONE',  ( -12.22235868236113809, -5.447693567057124042, 20.16913045786658998 ) ) ;
#4752 = PRESENTATION_LAYER_ASSIGNMENT (  '', '', ( #94301 ) ) ;
#4753 = ORIENTED_EDGE ( 'NONE', *, *, #82521, .T. ) ;
#4754 = CARTESIAN_POINT ( 'NONE',  ( 88.54209716525605245, -30.00000000000043698, -15.94097299020626579 ) ) ;
#4755 = CARTESIAN_POINT ( 'NONE',  ( 3.558939058152283064, -48.93902971889313847, 104.4181685828942250 ) ) ;
#4756 = CARTESIAN_POINT ( 'NONE',  ( -5.000000000000002665, -15.60834397543590590, -6.449723013184157416 ) ) ;
#4757 = CARTESIAN_POINT ( 'NONE',  ( 5.022013495303141006, 18.64316884711713840, 38.36535705883633796 ) ) ;
#4758 = CARTESIAN_POINT ( 'NONE',  ( 97.41881973446541565, -29.99999999999999645, 190.9256256769457138 ) ) ;
#4759 = CARTESIAN_POINT ( 'NONE',  ( 0.000000000000000000, 0.9999999999999943379, -13.99700487351915612 ) ) ;
#4760 = ORIENTED_EDGE ( 'NONE', *, *, #96594, .F. ) ;
#4761 = ORIENTED_EDGE ( 'NONE', *, *, #19686, .T. ) ;
#4762 = EDGE_LOOP ( 'NONE', ( #15905, #3229, #36012, #49748 ) ) ;
#4763 = CARTESIAN_POINT ( 'NONE',  ( 53.74627874984997788, -42.96783881181733022, 59.00685369471283792 ) ) ;
#4764 =( GEOMETRIC_REPRESENTATION_CONTEXT ( 3 ) GLOBAL_UNCERTAINTY_ASSIGNED_CONTEXT ( ( #69890 ) ) GLOBAL_UNIT_ASSIGNED_CONTEXT ( ( #75813, #10013, #42377 ) ) REPRESENTATION_CONTEXT ( 'NONE', 'WORKASPACE' ) );
#4765 = DIRECTION ( 'NONE',  ( 0.000000000000000000, -1.000000000000000000, 0.000000000000000000 ) ) ;
#4766 = AXIS2_PLACEMENT_3D ( 'NONE', #4861, #62061, #61521 ) ;
#4767 = DIRECTION ( 'NONE',  ( 0.000000000000000000, 0.000000000000000000, 1.000000000000000000 ) ) ;
#4768 = ORIENTED_EDGE ( 'NONE', *, *, #81492, .F. ) ;
#4769 = DIRECTION ( 'NONE',  ( -0.5735764363510494901, -0.8191520442889894671, 0.000000000000000000 ) ) ;
#4770 = EDGE_LOOP ( 'NONE', ( #47668, #104722, #83540, #51663, #71167 ) ) ;
#4771 = CARTESIAN_POINT ( 'NONE',  ( 19.29515645702225868, -5.000000000000000000, 6.123233995736768255E-16 ) ) ;
#4772 = CARTESIAN_POINT ( 'NONE',  ( 101.6454106623534130, -38.44960037453935087, 199.8551154696798449 ) ) ;
#4773 = CARTESIAN_POINT ( 'NONE',  ( 11.83113230997336096, 21.33428827753630586, 7.412539468226875705 ) ) ;
#4774 = PRODUCT_RELATED_PRODUCT_CATEGORY ( 'part', '', ( #35204 ) ) ;
#4775 = CARTESIAN_POINT ( 'NONE',  ( 83.74695688753641321, -45.28417006571125825, 7.588987474943079903 ) ) ;
#4776 = CARTESIAN_POINT ( 'NONE',  ( 2.216488688100095583, 14.30876692738956102, -0.5344654698446031915 ) ) ;
#4777 = AXIS2_PLACEMENT_3D ( 'NONE', #39604, #100465, #100999 ) ;
#4778 = CIRCLE ( 'NONE', #30672, 4.000000000000001776 ) ;
#4779 = CARTESIAN_POINT ( 'NONE',  ( 33.12808147879884757, 378.7724976115550817, 24.67513802460110028 ) ) ;
#4780 = AXIS2_PLACEMENT_3D ( 'NONE', #63257, #88582, #96148 ) ;
#4781 = CARTESIAN_POINT ( 'NONE',  ( 3.313708498984780260, -24.40625000409677270, -7.999999999999981348 ) ) ;
#4782 = FACE_OUTER_BOUND ( 'NONE', #21638, .T. ) ;
#4783 =( LENGTH_UNIT ( ) NAMED_UNIT ( * ) SI_UNIT ( .MILLI., .METRE. ) );
#4784 =( NAMED_UNIT ( * ) SI_UNIT ( $, .STERADIAN. ) SOLID_ANGLE_UNIT ( ) );
#4785 = CIRCLE ( 'NONE', #46135, 4.000000000000007105 ) ;
#4786 = ORIENTED_EDGE ( 'NONE', *, *, #17565, .T. ) ;
#4787 = CARTESIAN_POINT ( 'NONE',  ( -35.04731574020232898, 463.2729383095255571, 4.642530231459612189 ) ) ;
#4788 = CARTESIAN_POINT ( 'NONE',  ( -8.559508646656381003, 51.83514083332404709, -1.531152949374265049 ) ) ;
#4789 = VERTEX_POINT ( 'NONE', #19240 ) ;
#4790 = CARTESIAN_POINT ( 'NONE',  ( 44.46823338009918558, 1.482358050883964840E-15, 0.000000000000000000 ) ) ;
#4791 = CARTESIAN_POINT ( 'NONE',  ( -35.76309173223387461, 307.1545808062370497, 12.84636953888385769 ) ) ;
#4792 = CARTESIAN_POINT ( 'NONE',  ( -11.94276309775233003, -4.800907179085195153, -76.87753680762691033 ) ) ;
#4793 = CARTESIAN_POINT ( 'NONE',  ( 0.5805565836007581249, -3.752776749732553263, 6.499999999999999112 ) ) ;
#4794 = CARTESIAN_POINT ( 'NONE',  ( -1.469576158976823947E-15, -18.87499999999999289, 8.000000000000000000 ) ) ;
#4795 = CARTESIAN_POINT ( 'NONE',  ( -41.42724453868126488, -29.06770635680324588, 49.23312051806635736 ) ) ;
#4796 = EDGE_CURVE ( 'NONE', #3475, #79592, #58588, .T. ) ;
#4797 = DIRECTION ( 'NONE',  ( 0.000000000000000000, 1.000000000000000000, -0.000000000000000000 ) ) ;
#4798 = ORIENTED_EDGE ( 'NONE', *, *, #90647, .F. ) ;
#4799 = CARTESIAN_POINT ( 'NONE',  ( 82.86076466567399734, -60.89105270492382260, 190.2892942670303285 ) ) ;
#4801 = TOROIDAL_SURFACE ( 'NONE', #70240, 5.999999999999996447, 4.000000000000000000 ) ;
#4800 = DIRECTION ( 'NONE',  ( -0.000000000000000000, 0.5000000000000009992, 0.8660254037844380415 ) ) ;
#4802 = ORIENTED_EDGE ( 'NONE', *, *, #20430, .T. ) ;
#4803 = CARTESIAN_POINT ( 'NONE',  ( -100.0262352094438114, -60.15499860873356397, 115.3325505367406265 ) ) ;
#4804 = DIRECTION ( 'NONE',  ( 1.000000000000000000, -0.000000000000000000, 1.224646799147353207E-16 ) ) ;
#4805 = CARTESIAN_POINT ( 'NONE',  ( -43.02661387979790675, 465.7449615347597387, 11.43319743843399827 ) ) ;
#4806 = CARTESIAN_POINT ( 'NONE',  ( 3.514268259868478683, -4.333298119783825619, 17.57158721863739004 ) ) ;
#4807 = EDGE_CURVE ( 'NONE', #51545, #71001, #102800, .T. ) ;
#4808 = CARTESIAN_POINT ( 'NONE',  ( -9.343143414270016933, -22.46350855537282953, -38.54324068240695311 ) ) ;
#4809 = EDGE_CURVE ( 'NONE', #42350, #35708, #11068, .T. ) ;
#4810 = FILL_AREA_STYLE ('',( #78159 ) ) ;
#4811 = VECTOR ( 'NONE', #95693, 999.9999999999998863 ) ;
#4812 = FACE_OUTER_BOUND ( 'NONE', #19807, .T. ) ;
#4813 = SURFACE_STYLE_FILL_AREA ( #11823 ) ;
#4814 = CARTESIAN_POINT ( 'NONE',  ( 40.16194943996363520, -26.39549351810784472, 36.06414978926066794 ) ) ;
#4815 = STYLED_ITEM ( 'NONE', ( #22145 ), #1907 ) ;
#4817 = CARTESIAN_POINT ( 'NONE',  ( -11.96408628757766124, 19.58595713499403246, 7.540478412421575349 ) ) ;
#4816 = CARTESIAN_POINT ( 'NONE',  ( 41.57853103384506710, 486.0999730836878143, 12.35226384734806793 ) ) ;
#4818 = CARTESIAN_POINT ( 'NONE',  ( 40.32076386538651747, 316.2483603545517781, 3.170981411441938569 ) ) ;
#4819 = CARTESIAN_POINT ( 'NONE',  ( -13.61497193734505018, 294.5438151431720257, 1.871498990400385809 ) ) ;
#4820 = ADVANCED_FACE ( 'NONE', ( #76879 ), #2994, .T. ) ;
#4821 = VECTOR ( 'NONE', #103032, 1000.000000000000000 ) ;
#4822 = DIRECTION ( 'NONE',  ( -1.000000000000000000, 0.000000000000000000, 0.000000000000000000 ) ) ;
#4823 = AXIS2_PLACEMENT_3D ( 'NONE', #26729, #76292, #59600 ) ;
#4824 = EDGE_LOOP ( 'NONE', ( #60598, #22828, #73724, #90867, #73752, #21383, #92292, #65076, #88661 ) ) ;
#4825 = CARTESIAN_POINT ( 'NONE',  ( -9.755579246370350788, -2.371311999149684269, 15.43086382375051357 ) ) ;
#4826 = CARTESIAN_POINT ( 'NONE',  ( 0.4969600502617477211, 4.995646404165273502, -7.347286611336973472 ) ) ;
#4827 = DIRECTION ( 'NONE',  ( -1.000000000000000000, 0.000000000000000000, 0.000000000000000000 ) ) ;
#4828 =( BOUNDED_SURFACE ( )  B_SPLINE_SURFACE ( 3, 2, ( 
 ( #100168, #43006, #58661 ),
 ( #18764, #100691, #85606 ),
 ( #44071, #76956, #101765 ),
 ( #1994, #34941, #84532 ),
 ( #59731, #51613, #2528 ),
 ( #35478, #6108, #103756 ),
 ( #64884, #69418, #56230 ),
 ( #89168, #15273, #55185 ),
 ( #21808, #71376, #7169 ),
 ( #48155, #96210, #77501 ),
 ( #47623, #39033, #29894 ),
 ( #71915, #88112, #14192 ),
 ( #104278, #79999, #13670 ),
 ( #81056, #64373, #97247 ),
 ( #104817, #23392, #88635 ),
 ( #30419, #63314, #22338 ),
 ( #5585, #3614, #6644 ),
 ( #22866, #11679, #23937 ),
 ( #30965, #46578, #79475 ),
 ( #38512, #56779, #44612 ) ),
 .UNSPECIFIED., .F., .F., .T. ) 
 B_SPLINE_SURFACE_WITH_KNOTS ( ( 4, 2, 2, 2, 2, 2, 2, 2, 2, 4 ),
 ( 3, 3 ),
 ( 0.02241040388483112045, 0.02720928303954221750, 0.02960872261689776602, 0.03080844240557554028, 0.03200816219425331455, 0.03680704134896441160, 0.03740690124330330046, 0.03800676113764218933, 0.03920648092631996706, 0.04160592050367551559 ),
 ( 0.000000000000000000, 1.000000000000000000 ),
 .UNSPECIFIED. ) 
 GEOMETRIC_REPRESENTATION_ITEM ( )  RATIONAL_B_SPLINE_SURFACE ( (
 ( 1.000000000000000000, 0.7071075261733695827, 1.000000000000000000),
 ( 1.000000000000000000, 0.7071101665621289944, 1.000000000000000000),
 ( 1.000000000000000000, 0.7071141823279891714, 1.000000000000000000),
 ( 1.000000000000000000, 0.7071130896529220777, 1.000000000000000000),
 ( 1.000000000000000000, 0.7071116450707854995, 1.000000000000000000),
 ( 1.000000000000000000, 0.7071091581537886084, 1.000000000000000000),
 ( 1.000000000000000000, 0.7071082983977113878, 1.000000000000000000),
 ( 1.000000000000000000, 0.7071070359255379190, 1.000000000000000000),
 ( 1.000000000000000000, 0.7071066027460465309, 1.000000000000000000),
 ( 1.000000000000000000, 0.7071078295206322251, 1.000000000000000000),
 ( 1.000000000000000000, 0.7071068908989407431, 1.000000000000000000),
 ( 1.000000000000000000, 0.7071067684955979482, 1.000000000000000000),
 ( 1.000000000000000000, 0.7071080599920462895, 1.000000000000000000),
 ( 1.000000000000000000, 0.7071121107070883482, 1.000000000000000000),
 ( 1.000000000000000000, 0.7071147513002663532, 1.000000000000000000),
 ( 1.000000000000000000, 0.7071223048250396825, 1.000000000000000000),
 ( 1.000000000000000000, 0.7071265701120853508, 1.000000000000000000),
 ( 1.000000000000000000, 0.7071280438862577178, 1.000000000000000000),
 ( 1.000000000000000000, 0.7071102363992133322, 1.000000000000000000),
 ( 1.000000000000000000, 0.7071067811865472397, 1.000000000000000000) ) ) 
 REPRESENTATION_ITEM ( '' )  SURFACE ( )  );
#4829 = CARTESIAN_POINT ( 'NONE',  ( 3.129901519903563578, -34.58960633113510141, -32.63490336102687195 ) ) ;
#4830 = ORIENTED_EDGE ( 'NONE', *, *, #61343, .F. ) ;
#4831 = CARTESIAN_POINT ( 'NONE',  ( 58.67238219402268840, -1.232595164407830946E-29, 4.000000000000007105 ) ) ;
#4832 = DIRECTION ( 'NONE',  ( -0.5882352941176471894, 0.000000000000000000, 0.8086898285216187476 ) ) ;
#4833 = CONICAL_SURFACE ( 'NONE', #44497, 4.000000000000001776, 0.9599310885968774798 ) ;
#4834 = VECTOR ( 'NONE', #91626, 999.9999999999998863 ) ;
#4835 = ORIENTED_EDGE ( 'NONE', *, *, #6512, .F. ) ;
#4836 = COLOUR_RGB ( '', 0.40784314, 0.44705882, 0.49803922) ;
#4837 = EDGE_CURVE ( 'NONE', #73538, #100365, #41978, .T. ) ;
#4838 = CARTESIAN_POINT ( 'NONE',  ( -43.71297783477830734, 485.1278128289774259, -1.116606130290624721 ) ) ;
#4839 = CARTESIAN_POINT ( 'NONE',  ( -44.13784562318695492, 464.3950638386332344, 9.689741638643303290 ) ) ;
#4840 = CARTESIAN_POINT ( 'NONE',  ( -92.73391705501121862, -59.99999999999999289, -6.016779592986783776 ) ) ;
#4841 = CIRCLE ( 'NONE', #80585, 65.00000000000000000 ) ;
#4842 = VERTEX_POINT ( 'NONE', #18138 ) ;
#4843 = CARTESIAN_POINT ( 'NONE',  ( 7.305752995879768896, 41.99999999999663913, -58.79284008964064157 ) ) ;
#4844 = DIRECTION ( 'NONE',  ( 0.000000000000000000, -1.000000000000000000, 0.000000000000000000 ) ) ;
#4845 = CARTESIAN_POINT ( 'NONE',  ( -9.482993638194541219, 27.55651279746323823, -3.177441187500465336 ) ) ;
#4847 = DIRECTION ( 'NONE',  ( -1.000000000000000000, -1.224606353822377258E-16, -0.000000000000000000 ) ) ;
#4846 = FILL_AREA_STYLE ('',( #79254 ) ) ;
#4848 = B_SPLINE_CURVE_WITH_KNOTS ( 'NONE', 3,
 ( #38338, #20603, #37822, #86362, #77182, #103574, #103056, #94445, #52906, #87409, #28136, #71199, #63122, #53945, #86880, #20054, #46408, #62598, #85826, #104094, #21627, #3292, #12426, #77717, #61014, #30234, #11903, #36233, #54457, #69105, #70153, #69629, #101975, #44830, #3828, #102522, #88984, #6986, #63664, #66705 ),
 .UNSPECIFIED., .F., .F.,
 ( 4, 2, 2, 2, 2, 2, 2, 2, 2, 2, 2, 2, 2, 2, 2, 2, 2, 2, 2, 4 ),
 ( 2.797157557069881010E-17, 0.002121099353757972556, 0.004242198707515917357, 0.008484397415031806958, 0.01696879483006366943, 0.02545319224509545036, 0.03393758966012722783, 0.05090638449019078277, 0.06787517932025434464, 0.08484397415031789957, 0.1018127689803814268, 0.1102971663954131903, 0.1187815638104449539, 0.1272659612254767036, 0.1315081599329925577, 0.1336292592867505125, 0.1346898089636294760, 0.1352200838020689577, 0.1354852212212886986, 0.1357503586405084395 ),
 .UNSPECIFIED. ) ;
#4849 = CARTESIAN_POINT ( 'NONE',  ( -84.46793043747848628, -25.56582313524723915, 161.3502830699509616 ) ) ;
#4850 = ORIENTED_EDGE ( 'NONE', *, *, #74021, .F. ) ;
#4851 = CARTESIAN_POINT ( 'NONE',  ( 0.000000000000000000, -8.673617379884035472E-16, -17.01589776168603407 ) ) ;
#4852 = ORIENTED_EDGE ( 'NONE', *, *, #41546, .F. ) ;
#4853 = ORIENTED_EDGE ( 'NONE', *, *, #70200, .F. ) ;
#4854 = CARTESIAN_POINT ( 'NONE',  ( 13.76503154704518472, -4.999999999999999112, -10.95334723230558716 ) ) ;
#4855 = ADVANCED_FACE ( 'NONE', ( #50465 ), #101097, .T. ) ;
#4856 = CARTESIAN_POINT ( 'NONE',  ( -5.000000000000000000, -14.03284112244674553, 9.638321536846772730 ) ) ;
#4857 = FILL_AREA_STYLE ('',( #86850 ) ) ;
#4858 = EDGE_LOOP ( 'NONE', ( #13622, #5605 ) ) ;
#4859 = CARTESIAN_POINT ( 'NONE',  ( 16.48376536647090873, 45.65789762114239636, -6.657797401561987627 ) ) ;
#4860 = STYLED_ITEM ( 'NONE', ( #97011 ), #44238 ) ;
#4861 = CARTESIAN_POINT ( 'NONE',  ( -46.00000000000000000, 500.0000000000002274, 0.000000000000000000 ) ) ;
#4862 = CARTESIAN_POINT ( 'NONE',  ( -106.6432006776756083, -57.67119647726944009, 107.9924613694791589 ) ) ;
#4863 = CARTESIAN_POINT ( 'NONE',  ( 74.07777777777778283, 3.309500000000014541, 0.000000000000000000 ) ) ;
#4864 = FACE_OUTER_BOUND ( 'NONE', #3259, .T. ) ;
#4865 = CARTESIAN_POINT ( 'NONE',  ( -9.165151389911681434, 104.7328921871708474, -4.000000000000000888 ) ) ;
#4866 = CARTESIAN_POINT ( 'NONE',  ( 89.21410497458975897, -29.99999999999997513, 9.589292377912048693 ) ) ;
#4867 = CARTESIAN_POINT ( 'NONE',  ( -74.38379737572475392, -29.99999999999997513, 152.0617010018234794 ) ) ;
#4868 = CARTESIAN_POINT ( 'NONE',  ( -57.09792055977870007, -29.08279639372222647, 60.54515176239379315 ) ) ;
#4869 = CIRCLE ( 'NONE', #96198, 5.000000000000001776 ) ;
#4870 = ORIENTED_EDGE ( 'NONE', *, *, #31867, .F. ) ;
#4871 = CARTESIAN_POINT ( 'NONE',  ( 43.00000000000000000, 500.0000000000002274, -12.00000000000000711 ) ) ;
#4872 = VERTEX_POINT ( 'NONE', #60726 ) ;
#4873 = CARTESIAN_POINT ( 'NONE',  ( -103.3953119595051788, -60.16512775842720373, 192.1477606830822822 ) ) ;
#4874 = DIRECTION ( 'NONE',  ( 0.000000000000000000, 0.8273160954982761162, -0.5617366626182478395 ) ) ;
#4875 = AXIS2_PLACEMENT_3D ( 'NONE', #93778, #19937, #52779 ) ;
#4876 = ADVANCED_FACE ( 'NONE', ( #59654 ), #8076, .T. ) ;
#4877 = EDGE_LOOP ( 'NONE', ( #40534, #54617, #19042, #93179, #41359, #42500 ) ) ;
#4878 = CARTESIAN_POINT ( 'NONE',  ( 19.44528390683268171, 49.97407526609521256, 60.67034508904624346 ) ) ;
#4879 = CARTESIAN_POINT ( 'NONE',  ( 2.377971214860273304E-07, -59.99999999999998579, 39.63907915656436387 ) ) ;
#4880 = CARTESIAN_POINT ( 'NONE',  ( 37.56673239365899519, 25.75719283951025318, -10.95617127780834998 ) ) ;
#4881 = CARTESIAN_POINT ( 'NONE',  ( 7.188101187500000044, -13.53125000204838457, 0.000000000000000000 ) ) ;
#4882 = CARTESIAN_POINT ( 'NONE',  ( 6.281178480976146616, -3.752776749732557704, 6.500000000000006217 ) ) ;
#4883 = DIRECTION ( 'NONE',  ( 0.000000000000000000, -1.000000000000000000, 0.000000000000000000 ) ) ;
#4884 = CARTESIAN_POINT ( 'NONE',  ( -14.54015256618497176, 142.2617268803927573, 0.000000000000000000 ) ) ;
#4885 = CARTESIAN_POINT ( 'NONE',  ( 69.77518918526168079, -29.99999999999999645, 94.60611941633173672 ) ) ;
#4886 = ADVANCED_FACE ( 'NONE', ( #92534 ), #51102, .T. ) ;
#4887 = DIRECTION ( 'NONE',  ( 0.000000000000000000, -1.000000000000000000, 0.000000000000000000 ) ) ;
#4888 = CARTESIAN_POINT ( 'NONE',  ( -1.011530059480323152, 34.89403417720795630, 27.74769827951694978 ) ) ;
#4889 = CARTESIAN_POINT ( 'NONE',  ( 86.75754961941542831, 1.030564683017419500E-14, 0.000000000000000000 ) ) ;
#4890 = ADVANCED_BREP_SHAPE_REPRESENTATION ( '', ( #55270, #10728 ), #54068 ) ;
#4891 = UNCERTAINTY_MEASURE_WITH_UNIT (LENGTH_MEASURE( 1.000000000000000082E-05 ), #30005, 'distance_accuracy_value', 'NONE');
#4892 = CARTESIAN_POINT ( 'NONE',  ( -28.19790697388618383, -18.63285467839684983, 28.87379585876446697 ) ) ;
#4893 = STYLED_ITEM ( 'NONE', ( #73662 ), #76291 ) ;
#4894 = ORIENTED_EDGE ( 'NONE', *, *, #9741, .F. ) ;
#4895 = ORIENTED_EDGE ( 'NONE', *, *, #40959, .F. ) ;
#4896 = CARTESIAN_POINT ( 'NONE',  ( 47.00367278406724125, -22.23533693108482723, 41.16701144914247834 ) ) ;
#4897 = CARTESIAN_POINT ( 'NONE',  ( 0.000000000000000000, 0.000000000000000000, -0.02540000000000007530 ) ) ;
#4899 = VECTOR ( 'NONE', #72016, 1000.000000000000000 ) ;
#4898 = CARTESIAN_POINT ( 'NONE',  ( -19.99999999999999289, -5.000000000000000000, 25.00000000000000000 ) ) ;
#4900 = CARTESIAN_POINT ( 'NONE',  ( -108.8824160030044652, -38.35653676688028213, 190.5054770832236954 ) ) ;
#4901 = ORIENTED_EDGE ( 'NONE', *, *, #69802, .F. ) ;
#4902 = CARTESIAN_POINT ( 'NONE',  ( 90.63064853328148729, -38.34546238407526175, 14.30285600733137485 ) ) ;
#4903 = CARTESIAN_POINT ( 'NONE',  ( 82.86271956844252884, -60.00000000000014211, 189.8647660441692437 ) ) ;
#4904 = CARTESIAN_POINT ( 'NONE',  ( -49.26505482459800334, 8.072780847947164773, -15.39015249100678240 ) ) ;
#4905 = FILL_AREA_STYLE ('',( #104109 ) ) ;
#4906 = CARTESIAN_POINT ( 'NONE',  ( 6.122251204096708754, 40.00000000294605940, -71.16543156461924013 ) ) ;
#4907 = CARTESIAN_POINT ( 'NONE',  ( 5.656854249492378806, -26.37500000409677270, 5.656854249492381470 ) ) ;
#4908 = CARTESIAN_POINT ( 'NONE',  ( 8.000000000000000000, -17.18750000409676915, 0.000000000000000000 ) ) ;
#4909 = CARTESIAN_POINT ( 'NONE',  ( -30.00000000000000000, 486.5488479675415192, 4.838494452963876036 ) ) ;
#4910 = AXIS2_PLACEMENT_3D ( 'NONE', #20854, #94706, #69360 ) ;
#4911 = CARTESIAN_POINT ( 'NONE',  ( 102.7341935722522805, -60.00000000000002842, 200.7825474415656686 ) ) ;
#4912 = EDGE_CURVE ( 'NONE', #3603, #106390, #1374, .T. ) ;
#4913 = CARTESIAN_POINT ( 'NONE',  ( -15.79195268148549758, 35.06869440440700458, 22.25194163443071460 ) ) ;
#4914 = VERTEX_POINT ( 'NONE', #80059 ) ;
#4915 = CARTESIAN_POINT ( 'NONE',  ( -36.45417852791157998, 303.1973759554606431, -8.097999875148085280 ) ) ;
#4916 = DIRECTION ( 'NONE',  ( 0.000000000000000000, 1.000000000000000000, 0.000000000000000000 ) ) ;
#4917 = FILL_AREA_STYLE_COLOUR ( '', #24632 ) ;
#4918 = EDGE_LOOP ( 'NONE', ( #23708, #66932, #53884 ) ) ;
#4920 = CARTESIAN_POINT ( 'NONE',  ( 31.97895150603505954, 464.8429202049701416, 12.52771109945640582 ) ) ;
#4919 = CARTESIAN_POINT ( 'NONE',  ( -96.94769293072555172, -38.48349360550125198, 201.1369200050914685 ) ) ;
#4921 = DIRECTION ( 'NONE',  ( 0.000000000000000000, 0.000000000000000000, -1.000000000000000000 ) ) ;
#4922 = CARTESIAN_POINT ( 'NONE',  ( 43.47770857297122404, 484.8227827122696567, 4.253339224811428565 ) ) ;
#4923 = VECTOR ( 'NONE', #18019, 1000.000000000000000 ) ;
#4924 = CARTESIAN_POINT ( 'NONE',  ( -5.082755093536326818, -15.59375000204838635, 5.082755093536325042 ) ) ;
#4925 = CIRCLE ( 'NONE', #8368, 4.250000000000000000 ) ;
#4926 = CARTESIAN_POINT ( 'NONE',  ( 0.000000000000000000, -3.000000000000002665, -75.00000000000001421 ) ) ;
#4927 = CIRCLE ( 'NONE', #65188, 5.000000000000000000 ) ;
#4928 = AXIS2_PLACEMENT_3D ( 'NONE', #88509, #13000, #71766 ) ;
#4929 = DIRECTION ( 'NONE',  ( 1.000000000000000000, 1.224606353822377258E-16, 0.000000000000000000 ) ) ;
#4931 = VERTEX_POINT ( 'NONE', #61798 ) ;
#4930 =( LENGTH_UNIT ( ) NAMED_UNIT ( * ) SI_UNIT ( .MILLI., .METRE. ) );
#4932 = CARTESIAN_POINT ( 'NONE',  ( 81.23237909639242105, -56.97435546150522612, 180.4903185276303361 ) ) ;
#4933 = CARTESIAN_POINT ( 'NONE',  ( 9.493007256569747199, 142.3993658332746577, -0.000000000000000000 ) ) ;
#4934 = CARTESIAN_POINT ( 'NONE',  ( -38.07677585881090465, 439.4430026352447385, 23.85998911115680698 ) ) ;
#4935 = ORIENTED_EDGE ( 'NONE', *, *, #59344, .F. ) ;
#4936 = LINE ( 'NONE', #94490, #20461 ) ;
#4937 = CARTESIAN_POINT ( 'NONE',  ( -47.06916318994504422, 18.66170694578063660, 14.79344423761920169 ) ) ;
#4938 = FACE_OUTER_BOUND ( 'NONE', #68012, .T. ) ;
#4939 = SURFACE_SIDE_STYLE ('',( #71249 ) ) ;
#4940 = CARTESIAN_POINT ( 'NONE',  ( 0.7794294244140879124, 13.54093176544609634, 51.48168560154597628 ) ) ;
#4941 = EDGE_CURVE ( 'NONE', #55265, #20019, #5649, .T. ) ;
#4942 = ORIENTED_EDGE ( 'NONE', *, *, #1969, .F. ) ;
#4943 = AXIS2_PLACEMENT_3D ( 'NONE', #69059, #35649, #93853 ) ;
#4944 = CIRCLE ( 'NONE', #44611, 10.00000000000000000 ) ;
#4945 = DIRECTION ( 'NONE',  ( -1.000000000000000000, 0.000000000000000000, 0.000000000000000000 ) ) ;
#4946 = EDGE_CURVE ( 'NONE', #71163, #103692, #4545, .T. ) ;
#4947 = CARTESIAN_POINT ( 'NONE',  ( -1.000000000000000000, -32.16754151679361939, -4.059900122495614383 ) ) ;
#4948 = CARTESIAN_POINT ( 'NONE',  ( -4.999999999999999112, -4.000000000000000000, 35.66025403784438197 ) ) ;
#4950 = CARTESIAN_POINT ( 'NONE',  ( -15.04954976391476151, 5.409063359390556158, -6.531832031858459509 ) ) ;
#4949 = CARTESIAN_POINT ( 'NONE',  ( 5.500000000000641265, 42.00000000000000000, -59.88032989331720302 ) ) ;
#4951 = AXIS2_PLACEMENT_3D ( 'NONE', #31511, #65441, #49234 ) ;
#4952 = CARTESIAN_POINT ( 'NONE',  ( 4.401442555609581635E-16, -20.28125000204838813, -7.188101187500000044 ) ) ;
#4953 = CARTESIAN_POINT ( 'NONE',  ( 39.44615384615384812, -4.171999999999999709, 5.616230220889763424E-16 ) ) ;
#4954 = CARTESIAN_POINT ( 'NONE',  ( 6.145999768513189743, -5.000000000000000000, -7.996316163939230393 ) ) ;
#4955 =( GEOMETRIC_REPRESENTATION_CONTEXT ( 3 ) GLOBAL_UNCERTAINTY_ASSIGNED_CONTEXT ( ( #104360 ) ) GLOBAL_UNIT_ASSIGNED_CONTEXT ( ( #103933, #5256, #80183 ) ) REPRESENTATION_CONTEXT ( 'NONE', 'WORKASPACE' ) );
#4956 = ORIENTED_EDGE ( 'NONE', *, *, #80192, .F. ) ;
#4957 = DIRECTION ( 'NONE',  ( 0.000000000000000000, -0.000000000000000000, 1.000000000000000000 ) ) ;
#4958 = DIRECTION ( 'NONE',  ( -1.000000000000000000, -1.224606353822377258E-16, -0.000000000000000000 ) ) ;
#4959 = CARTESIAN_POINT ( 'NONE',  ( -4.455300429064767975, 9.670763880908177512, -5.000000000000000888 ) ) ;
#4960 = ADVANCED_FACE ( 'NONE', ( #103298 ), #104335, .T. ) ;
#4961 = CARTESIAN_POINT ( 'NONE',  ( 5.799999999999999822, 6.928203230275505220, 4.000000000000007105 ) ) ;
#4962 = ORIENTED_EDGE ( 'NONE', *, *, #104465, .T. ) ;
#4963 = PRESENTATION_LAYER_ASSIGNMENT (  '', '', ( #56600 ) ) ;
#4964 = CARTESIAN_POINT ( 'NONE',  ( -34.29149597887493428, 464.1889238631191006, 18.11295844668995159 ) ) ;
#4965 = ORIENTED_EDGE ( 'NONE', *, *, #69598, .F. ) ;
#4966 = CLOSED_SHELL ( 'NONE', ( #64446, #104900, #55999, #10950, #60829, #69337, #80858, #83078, #49138, #89734, #34147, #92399, #14468, #69279, #22941, #4320, #77794, #31123, #56221, #47110, #41508, #12104, #94571, #103164, #98553, #98155, #102612, #63890, #56626, #63187, #27152, #14239, #75832, #31602, #54738, #92628, #3330, #32117, #26082, #95568, #7639, #72400, #56809, #68174, #48973, #77109, #12866, #6197, #88799, #13340, #71181, #27520, #43912, #6079, #40802, #23803, #88156, #25061, #73906, #73592, #57109, #17146, #32240, #67446, #35718, #70666, #89674, #97498, #103747, #76630, #23436, #23546 ) ) ;
#4967 = LINE ( 'NONE', #70758, #62684 ) ;
#4968 = EDGE_CURVE ( 'NONE', #46481, #29099, #2046, .T. ) ;
#4969 = CARTESIAN_POINT ( 'NONE',  ( -42.30916052715512166, 39.52170759503056985, -49.88302887289012233 ) ) ;
#4970 = FACE_OUTER_BOUND ( 'NONE', #26918, .T. ) ;
#4971 = UNCERTAINTY_MEASURE_WITH_UNIT (LENGTH_MEASURE( 1.000000000000000082E-05 ), #58294, 'distance_accuracy_value', 'NONE');
#4972 = CARTESIAN_POINT ( 'NONE',  ( -98.90204163354637501, -60.00000000000000711, 202.1654228340109967 ) ) ;
#4973 = CYLINDRICAL_SURFACE ( 'NONE', #84155, 5.000000000000002665 ) ;
#4974 = CARTESIAN_POINT ( 'NONE',  ( 3.373304793538787205, 304.8518027749948942, -9.000000000275658607 ) ) ;
#4975 = DIRECTION ( 'NONE',  ( 1.000000000000000000, 0.000000000000000000, 0.000000000000000000 ) ) ;
#4976 = PLANE ( 'NONE',  #12990 ) ;
#4977 = EDGE_CURVE ( 'NONE', #11792, #21079, #85632, .T. ) ;
#4978 = MECHANICAL_DESIGN_GEOMETRIC_PRESENTATION_REPRESENTATION (  '', ( #34266 ), #82506 ) ;
#4979 = CARTESIAN_POINT ( 'NONE',  ( -83.88175480885155366, -42.98347005089964767, 181.2433426847502176 ) ) ;
#4980 = FACE_OUTER_BOUND ( 'NONE', #53912, .T. ) ;
#4981 = ORIENTED_EDGE ( 'NONE', *, *, #75906, .T. ) ;
#4982 = DIRECTION ( 'NONE',  ( 0.000000000000000000, 1.000000000000000000, 0.000000000000000000 ) ) ;
#4983 = EDGE_CURVE ( 'NONE', #38550, #69704, #25365, .T. ) ;
#4984 = CARTESIAN_POINT ( 'NONE',  ( 5.475947152006326313, -68.16217730109124773, 2.462898245435125588 ) ) ;
#4985 = CARTESIAN_POINT ( 'NONE',  ( -83.48701994937339066, -37.82282612950775302, 31.99776073991571934 ) ) ;
#4986 = CARTESIAN_POINT ( 'NONE',  ( 33.95156263172584943, 464.5083255208626838, 6.608064661821377861 ) ) ;
#4987 = FILL_AREA_STYLE_COLOUR ( '', #37801 ) ;
#4988 = CARTESIAN_POINT ( 'NONE',  ( 3.646183794689596969, 129.8030994959483735, -4.999999999999999112 ) ) ;
#4989 = FACE_OUTER_BOUND ( 'NONE', #77943, .T. ) ;
#4990 = CARTESIAN_POINT ( 'NONE',  ( 11.08349330513380160, 1.593028355512270567E-15, 0.000000000000000000 ) ) ;
#4991 = CARTESIAN_POINT ( 'NONE',  ( 79.87681789614374850, -30.00000000000000711, 191.0754539389706395 ) ) ;
#4992 = CARTESIAN_POINT ( 'NONE',  ( -50.10796912846466000, 53.37899725327127953, -25.05398456423234066 ) ) ;
#4993 = CARTESIAN_POINT ( 'NONE',  ( -87.68152309050471160, -14.21045842199426801, 32.26861779447729361 ) ) ;
#4994 = CARTESIAN_POINT ( 'NONE',  ( -66.93347199945957016, -25.58110973058455784, 84.52057819029118946 ) ) ;
#4995 = ORIENTED_EDGE ( 'NONE', *, *, #97134, .F. ) ;
#4996 = CARTESIAN_POINT ( 'NONE',  ( -61.56154494590426651, 38.95379437484910312, -16.50053755318738880 ) ) ;
#4997 = CARTESIAN_POINT ( 'NONE',  ( 49.49803543560198449, -60.00000000002933831, 76.94089586485750942 ) ) ;
#4998 = AXIS2_PLACEMENT_3D ( 'NONE', #76021, #66886, #2119 ) ;
#4999 = ORIENTED_EDGE ( 'NONE', *, *, #68476, .F. ) ;
#5000 = CARTESIAN_POINT ( 'NONE',  ( 0.000000000000000000, -1.200583151104947843, 112.0000000000000000 ) ) ;
#5001 = CARTESIAN_POINT ( 'NONE',  ( 7.188101187499999156, -18.12500000204838457, 2.977408999572654924 ) ) ;
#5002 = DIRECTION ( 'NONE',  ( 1.000000000000000000, 0.000000000000000000, 0.000000000000000000 ) ) ;
#5003 = ORIENTED_EDGE ( 'NONE', *, *, #48024, .F. ) ;
#5004 = CARTESIAN_POINT ( 'NONE',  ( -10.28624191512074226, 46.12099395432516502, 12.90779740155501187 ) ) ;
#5005 = ORIENTED_EDGE ( 'NONE', *, *, #35494, .F. ) ;
#5006 = CYLINDRICAL_SURFACE ( 'NONE', #42450, 15.00000000000001243 ) ;
#5007 = CARTESIAN_POINT ( 'NONE',  ( -39.81879459130762200, 485.8579414158143663, -5.000253522669930284 ) ) ;
#5008 = CARTESIAN_POINT ( 'NONE',  ( -92.63142467325774021, -60.00000000000000000, -3.230052685997783612 ) ) ;
#5009 = CARTESIAN_POINT ( 'NONE',  ( 6.750000000000016875, -11.69134295108991495, 0.000000000000000000 ) ) ;
#5010 = CARTESIAN_POINT ( 'NONE',  ( -7.188101187500001821, -30.87500000204838813, -2.977408999572651371 ) ) ;
#5011 = CARTESIAN_POINT ( 'NONE',  ( 83.88447113947664491, -60.00000000000000000, 191.6821499555289847 ) ) ;
#5012 = CARTESIAN_POINT ( 'NONE',  ( 0.000000000000000000, 0.000000000000000000, 0.000000000000000000 ) ) ;
#5013 = CARTESIAN_POINT ( 'NONE',  ( 5.000000000000000888, -63.35320086162899145, 9.447768536045829890 ) ) ;
#5014 = CARTESIAN_POINT ( 'NONE',  ( 6.145467200821944864, 49.99999999999999289, -77.00333157708759302 ) ) ;
#5015 = EDGE_CURVE ( 'NONE', #89992, #85394, #47496, .T. ) ;
#5016 = CARTESIAN_POINT ( 'NONE',  ( 1.775369994829482681E-15, -3.035766082959412415E-15, 13.99700487351915612 ) ) ;
#5017 = CARTESIAN_POINT ( 'NONE',  ( -42.00953037517896149, 328.3444845812533117, 6.160407614653865771 ) ) ;
#5018 = CARTESIAN_POINT ( 'NONE',  ( 21.42997177938648790, 302.9814582950376689, -9.972298323676696441 ) ) ;
#5019 = AXIS2_PLACEMENT_3D ( 'NONE', #104458, #30607, #19884 ) ;
#5020 = ORIENTED_EDGE ( 'NONE', *, *, #63900, .F. ) ;
#5021 = CARTESIAN_POINT ( 'NONE',  ( 36.84999999999999432, -3.309499999999999886, 0.000000000000000000 ) ) ;
#5022 = CARTESIAN_POINT ( 'NONE',  ( -15.48058112917927431, 42.57620948808565942, -89.21771955211514182 ) ) ;
#5023 = CARTESIAN_POINT ( 'NONE',  ( 33.08419194243336392, -32.55809666592025309, 33.08005832449853756 ) ) ;
#5024 = CARTESIAN_POINT ( 'NONE',  ( 5.820808985959283532, -2.898778190268130493E-12, -21.65942590380460686 ) ) ;
#5025 = EDGE_LOOP ( 'NONE', ( #10965, #75798, #56164, #33809 ) ) ;
#5026 = EDGE_CURVE ( 'NONE', #22245, #35905, #19994, .T. ) ;
#5027 = CARTESIAN_POINT ( 'NONE',  ( -43.51084452654468748, 465.2903130129606666, 9.421687747985890482 ) ) ;
#5028 = CIRCLE ( 'NONE', #49744, 22.55262289886175964 ) ;
#5030 = CARTESIAN_POINT ( 'NONE',  ( -35.57955382936916067, 363.3973965622570859, 2.919629247011395368 ) ) ;
#5029 = LINE ( 'NONE', #13093, #12433 ) ;
#5031 = CARTESIAN_POINT ( 'NONE',  ( 0.000000000000000000, 0.000000000000000000, 0.000000000000000000 ) ) ;
#5032 = DIRECTION ( 'NONE',  ( 0.000000000000000000, 1.000000000000000000, 0.000000000000000000 ) ) ;
#5033 = FILL_AREA_STYLE_COLOUR ( '', #61893 ) ;
#5034 = CARTESIAN_POINT ( 'NONE',  ( -48.55387420720941805, 13.84642135131182883, -16.74239769522730015 ) ) ;
#5035 = DIRECTION ( 'NONE',  ( 0.000000000000000000, 0.000000000000000000, 1.000000000000000000 ) ) ;
#5037 = VERTEX_POINT ( 'NONE', #15863 ) ;
#5036 = STYLED_ITEM ( 'NONE', ( #58042 ), #31536 ) ;
#5038 = CARTESIAN_POINT ( 'NONE',  ( 92.00383831918911426, -59.99999999999999289, 6.129265091283676803 ) ) ;
#5039 = DIRECTION ( 'NONE',  ( 0.000000000000000000, -1.000000000000000000, 0.000000000000000000 ) ) ;
#5040 = CARTESIAN_POINT ( 'NONE',  ( 99.75754961941544252, -5.000000000000000888, 6.123233995736779101E-16 ) ) ;
#5041 = CARTESIAN_POINT ( 'NONE',  ( 15.11650669486618881, 4.898587196589413815E-16, -4.000000000000000888 ) ) ;
#5042 = DIRECTION ( 'NONE',  ( -1.000000000000000000, -1.224606353822377258E-16, -0.000000000000000000 ) ) ;
#5043 = EDGE_LOOP ( 'NONE', ( #5173, #101488, #106168, #47632 ) ) ;
#5044 = CARTESIAN_POINT ( 'NONE',  ( -89.67601645498943697, -30.00000000002656364, 1.152961518554983078 ) ) ;
#5045 = EDGE_LOOP ( 'NONE', ( #83539, #59778, #53353, #38426, #49318 ) ) ;
#5046 = VECTOR ( 'NONE', #42331, 1000.000000000000000 ) ;
#5047 = FACE_OUTER_BOUND ( 'NONE', #32184, .T. ) ;
#5048 = CARTESIAN_POINT ( 'NONE',  ( 6.750000000000016875, -11.69134295108991495, -13.00000000000000000 ) ) ;
#5049 = DIRECTION ( 'NONE',  ( -0.000000000000000000, 1.000000000000000000, -0.000000000000000000 ) ) ;
#5050 = CARTESIAN_POINT ( 'NONE',  ( 15.64030048137924744, 21.26710225494773709, -5.626279437266589412 ) ) ;
#5051 = CARTESIAN_POINT ( 'NONE',  ( 4.401442555609581635E-16, -29.65625000204838813, -7.188101187500000044 ) ) ;
#5052 = LINE ( 'NONE', #54105, #70862 ) ;
#5053 = CARTESIAN_POINT ( 'NONE',  ( 10.28624191512063746, 46.12099395432516502, -12.90779740155508826 ) ) ;
#5054 = CARTESIAN_POINT ( 'NONE',  ( 33.00000000000000000, 464.3970849722209095, 17.41240408234224191 ) ) ;
#5055 = ORIENTED_EDGE ( 'NONE', *, *, #27995, .F. ) ;
#5057 = ORIENTED_EDGE ( 'NONE', *, *, #5071, .T. ) ;
#5056 = DIRECTION ( 'NONE',  ( 0.000000000000000000, 1.000000000000000000, 0.000000000000000000 ) ) ;
#5058 = CARTESIAN_POINT ( 'NONE',  ( 78.61532337604826637, -46.43317018272926333, 144.3717807119670624 ) ) ;
#5059 =( GEOMETRIC_REPRESENTATION_CONTEXT ( 3 ) GLOBAL_UNCERTAINTY_ASSIGNED_CONTEXT ( ( #1921 ) ) GLOBAL_UNIT_ASSIGNED_CONTEXT ( ( #29795, #4422, #78830 ) ) REPRESENTATION_CONTEXT ( 'NONE', 'WORKASPACE' ) );
#5060 = B_SPLINE_CURVE_WITH_KNOTS ( 'NONE', 3,
 ( #86852, #4859, #79267, #5390, #38312, #71173, #104067, #54973, #87904, #1513, #959, #73823, #57623, #25869, #106718, #33940, #66808, #99697, #427, #16118 ),
 .UNSPECIFIED., .F., .F.,
 ( 4, 2, 2, 2, 2, 2, 2, 2, 2, 4 ),
 ( 0.001107850312301166765, 0.001612907343245353377, 0.002117964374189539988, 0.002623021405133726600, 0.003128078436077913211, 0.003380606951550005432, 0.003633135467022097220, 0.004138192497966280796, 0.004643249528910464372, 0.005148306559854647080 ),
 .UNSPECIFIED. ) ;
#5061 = CARTESIAN_POINT ( 'NONE',  ( 15.50532557111870346, 2.637300882400162472, -0.8493220884092024248 ) ) ;
#5062 = EDGE_LOOP ( 'NONE', ( #45012, #53920, #28548, #73690 ) ) ;
#5063 = CARTESIAN_POINT ( 'NONE',  ( -12.50000000000000711, 39.69996554813628364, -64.82567002250831933 ) ) ;
#5064 = CARTESIAN_POINT ( 'NONE',  ( 5.082755093536325930, -21.96875000204838457, -5.082755093536325042 ) ) ;
#5065 = CARTESIAN_POINT ( 'NONE',  ( -87.17917008083185237, -57.58863837343483283, 203.1758066736668980 ) ) ;
#5066 = EDGE_CURVE ( 'NONE', #66517, #45176, #31029, .T. ) ;
#5067 = ORIENTED_EDGE ( 'NONE', *, *, #39618, .F. ) ;
#5068 =( NAMED_UNIT ( * ) PLANE_ANGLE_UNIT ( ) SI_UNIT ( $, .RADIAN. ) );
#5069 = CARTESIAN_POINT ( 'NONE',  ( -4.589357672516648279, -11.06206030977222809, -3.865585121226768894 ) ) ;
#5070 = STYLED_ITEM ( 'NONE', ( #18772 ), #90584 ) ;
#5071 = EDGE_CURVE ( 'NONE', #81125, #40837, #23438, .T. ) ;
#5072 = CARTESIAN_POINT ( 'NONE',  ( -9.537927238823506570, 82.35373142881822162, -3.010735687602428268 ) ) ;
#5073 = CARTESIAN_POINT ( 'NONE',  ( -6.499999999999999112, 3.752776749732556816, -6.064240316920397333 ) ) ;
#5074 = CARTESIAN_POINT ( 'NONE',  ( 5.656854249492380582, -9.500000004096769146, -5.656854249492379694 ) ) ;
#5075 = CARTESIAN_POINT ( 'NONE',  ( -5.978393154364650464, -13.00690510473827644, 32.07137290849176026 ) ) ;
#5076 = AXIS2_PLACEMENT_3D ( 'NONE', #79368, #45953, #70754 ) ;
#5077 = CARTESIAN_POINT ( 'NONE',  ( 9.999999999999996447, 15.00000000000000000, 3.082707893549208045 ) ) ;
#5078 = AXIS2_PLACEMENT_3D ( 'NONE', #65250, #37438, #70833 ) ;
#5079 = LINE ( 'NONE', #46072, #36214 ) ;
#5080 = CARTESIAN_POINT ( 'NONE',  ( 7.500000000000007105, -3.000000000000000000, -68.91429205785459544 ) ) ;
#5081 =( LENGTH_UNIT ( ) NAMED_UNIT ( * ) SI_UNIT ( .MILLI., .METRE. ) );
#5082 = DIRECTION ( 'NONE',  ( -4.567431630836575009E-16, 1.000000000000000000, 6.481467296164994004E-17 ) ) ;
#5083 = CARTESIAN_POINT ( 'NONE',  ( -9.165151389911681434, 30.00000000000000000, -4.000000000000000000 ) ) ;
#5084 = ORIENTED_EDGE ( 'NONE', *, *, #65219, .T. ) ;
#5085 = PRESENTATION_STYLE_ASSIGNMENT (( #38017 ) ) ;
#5086 = CARTESIAN_POINT ( 'NONE',  ( 12.06346645439106524, -4.728929080163736920, -12.59383595214006135 ) ) ;
#5087 = DIRECTION ( 'NONE',  ( -1.000000000000000000, -1.224606353822377258E-16, -0.000000000000000000 ) ) ;
#5088 = CARTESIAN_POINT ( 'NONE',  ( 4.093755603727620596, -17.90092510166400430, -37.94411461619921511 ) ) ;
#5089 = CARTESIAN_POINT ( 'NONE',  ( -82.56376108564677452, -30.00000000000000711, 149.7403354104212951 ) ) ;
#5090 = CARTESIAN_POINT ( 'NONE',  ( 39.83349330513380693, 1.593028355512270567E-15, 0.000000000000000000 ) ) ;
#5091 = ADVANCED_FACE ( 'NONE', ( #33138 ), #24001, .T. ) ;
#5092 = B_SPLINE_CURVE_WITH_KNOTS ( 'NONE', 3,
 ( #50724, #76080, #60471, #11333, #51265, #83115 ),
 .UNSPECIFIED., .F., .F.,
 ( 4, 2, 4 ),
 ( 2.275079091765669941E-15, 0.01116218283128518791, 0.02232436566256810334 ),
 .UNSPECIFIED. ) ;
#5093 = COLOUR_RGB ( '', 0.09019608, 0.27058824, 0.51372549) ;
#5094 = ORIENTED_EDGE ( 'NONE', *, *, #63924, .F. ) ;
#5095 = CARTESIAN_POINT ( 'NONE',  ( -3.514268259821786700, -4.333298119783847824, 17.57158721864471573 ) ) ;
#5096 = CARTESIAN_POINT ( 'NONE',  ( 101.8121882041653805, -57.63159399422936957, 203.3427569746260986 ) ) ;
#5097 = CARTESIAN_POINT ( 'NONE',  ( 0.000000000000000000, 0.000000000000000000, 4.000000000000000888 ) ) ;
#5098 = CIRCLE ( 'NONE', #63620, 7.000000000000011546 ) ;
#5099 = DIRECTION ( 'NONE',  ( 0.000000000000000000, 1.000000000000000000, 0.000000000000000000 ) ) ;
#5100 = DIRECTION ( 'NONE',  ( 0.000000000000000000, 0.000000000000000000, 1.000000000000000000 ) ) ;
#5101 = CARTESIAN_POINT ( 'NONE',  ( -43.00000000000000000, 500.0000000000002274, 0.000000000000000000 ) ) ;
#5102 = CARTESIAN_POINT ( 'NONE',  ( -70.60798716468931957, -60.00000000000000711, 144.8513084279401255 ) ) ;
#5103 = CARTESIAN_POINT ( 'NONE',  ( 12.33349330513380693, 1.593028355512270962E-15, 0.000000000000000000 ) ) ;
#5104 = DIRECTION ( 'NONE',  ( 0.000000000000000000, 1.000000000000000000, 0.000000000000000000 ) ) ;
#5105 = VECTOR ( 'NONE', #65890, 1000.000000000000000 ) ;
#5106 = CARTESIAN_POINT ( 'NONE',  ( 64.91565662643154155, 50.00000000002004441, 6.815324757472883910 ) ) ;
#5107 = CARTESIAN_POINT ( 'NONE',  ( -85.74525919723035372, -39.25732588298068038, 186.2133864294523562 ) ) ;
#5108 = VERTEX_POINT ( 'NONE', #39099 ) ;
#5109 = CARTESIAN_POINT ( 'NONE',  ( 35.65243850163849970, 370.5602105955105117, 3.802963908744633859 ) ) ;
#5110 = CARTESIAN_POINT ( 'NONE',  ( 43.60658154848616874, 484.6917668751715382, 3.660634294265139754 ) ) ;
#5111 = CARTESIAN_POINT ( 'NONE',  ( -6.648507154639723638, 41.85229584295817062, -59.35075352205862487 ) ) ;
#5112 = CARTESIAN_POINT ( 'NONE',  ( 26.84999999999999787, 1.533819458162526451E-15, 0.000000000000000000 ) ) ;
#5113 = CARTESIAN_POINT ( 'NONE',  ( 12.49999999999996092, -3.165118404323130630, -76.70900766830892792 ) ) ;
#5114 = FILL_AREA_STYLE_COLOUR ( '', #80058 ) ;
#5115 = CARTESIAN_POINT ( 'NONE',  ( -82.65297077345887544, -37.77213538829948192, -12.24075959479144515 ) ) ;
#5116 = AXIS2_PLACEMENT_3D ( 'NONE', #31498, #81064, #64378 ) ;
#5117 = PLANE ( 'NONE',  #32177 ) ;
#5118 = CARTESIAN_POINT ( 'NONE',  ( 5.285714285714277594, -50.19912527334259522, 103.1763305333244176 ) ) ;
#5119 = ORIENTED_EDGE ( 'NONE', *, *, #41219, .F. ) ;
#5120 = CARTESIAN_POINT ( 'NONE',  ( 19.50011280463133545, 50.00000000000000000, 59.90639435984937222 ) ) ;
#5121 = CARTESIAN_POINT ( 'NONE',  ( -2.452879891156814374, -7.244083172395190395, -0.1007566405101844587 ) ) ;
#5122 = CARTESIAN_POINT ( 'NONE',  ( 3.088855081073062209E-15, -4.285714285714286476, 25.22241582816893413 ) ) ;
#5123 = CARTESIAN_POINT ( 'NONE',  ( -33.46689243938315883, 485.1693579410822394, 2.982310567416428082 ) ) ;
#5124 = AXIS2_PLACEMENT_3D ( 'NONE', #103324, #66567, #725 ) ;
#5125 = CARTESIAN_POINT ( 'NONE',  ( 82.54285424309888697, -59.99999999999997868, -29.20801037391389698 ) ) ;
#5126 = CARTESIAN_POINT ( 'NONE',  ( -80.01308992809121889, -36.03078623675013858, 142.1897297268717182 ) ) ;
#5127 = ORIENTED_EDGE ( 'NONE', *, *, #59720, .F. ) ;
#5128 = FACE_OUTER_BOUND ( 'NONE', #49651, .T. ) ;
#5129 = DIRECTION ( 'NONE',  ( 0.000000000000000000, -0.9612814585411639801, -0.2755684261031591809 ) ) ;
#5130 = CARTESIAN_POINT ( 'NONE',  ( 85.39890529347994175, -57.56671838092738369, 202.4583528846124807 ) ) ;
#5131 = CARTESIAN_POINT ( 'NONE',  ( 38.31452810505570028, 308.8792753538928082, 1.313130104885508409 ) ) ;
#5132 = VECTOR ( 'NONE', #77409, 1000.000000000000000 ) ;
#5133 = CARTESIAN_POINT ( 'NONE',  ( 0.000000000000000000, 0.000000000000000000, 0.000000000000000000 ) ) ;
#5134 = ORIENTED_EDGE ( 'NONE', *, *, #102202, .F. ) ;
#5135 = PRESENTATION_STYLE_ASSIGNMENT (( #24004 ) ) ;
#5136 = CARTESIAN_POINT ( 'NONE',  ( 7.500000000000007105, 39.99999999999998579, -65.90297133634152260 ) ) ;
#5137 = DIRECTION ( 'NONE',  ( 1.000000000000000000, 1.224606353822377258E-16, 0.000000000000000000 ) ) ;
#5138 = CARTESIAN_POINT ( 'NONE',  ( -2.977408999572650039, -23.18750000204838813, -7.188101187500001821 ) ) ;
#5139 = ORIENTED_EDGE ( 'NONE', *, *, #32645, .F. ) ;
#5140 = LINE ( 'NONE', #96289, #3357 ) ;
#5141 = DIRECTION ( 'NONE',  ( 0.000000000000000000, 0.000000000000000000, 1.000000000000000000 ) ) ;
#5142 = CARTESIAN_POINT ( 'NONE',  ( -44.21332904831282917, 435.2494715644501184, 14.45449769377396976 ) ) ;
#5143 = EDGE_CURVE ( 'NONE', #60348, #84468, #98885, .T. ) ;
#5144 = CARTESIAN_POINT ( 'NONE',  ( 26.35623858825801591, 36.89120352755210774, 9.820590063098430633 ) ) ;
#5145 = CARTESIAN_POINT ( 'NONE',  ( 13.69330508143927538, 1.340359594676612611E-15, 0.000000000000000000 ) ) ;
#5146 = EDGE_CURVE ( 'NONE', #36049, #60190, #75410, .T. ) ;
#5147 = CARTESIAN_POINT ( 'NONE',  ( -37.22806219796889593, 463.3233819687147275, 20.09366234602755696 ) ) ;
#5148 = ORIENTED_EDGE ( 'NONE', *, *, #90673, .T. ) ;
#5149 = CARTESIAN_POINT ( 'NONE',  ( -7.099152841014172211, 41.70084716954765724, -59.82719248405098256 ) ) ;
#5151 = CARTESIAN_POINT ( 'NONE',  ( 28.23832643585050661, -46.43268247453659825, 33.77938694114138940 ) ) ;
#5150 = CARTESIAN_POINT ( 'NONE',  ( -61.00210428163805432, -14.21045842199449005, 86.20094954650318186 ) ) ;
#5152 = STYLED_ITEM ( 'NONE', ( #72058 ), #90915 ) ;
#5153 = DIRECTION ( 'NONE',  ( 1.000000000000000000, -0.000000000000000000, -0.000000000000000000 ) ) ;
#5154 = ORIENTED_EDGE ( 'NONE', *, *, #73734, .F. ) ;
#5155 = EDGE_CURVE ( 'NONE', #87702, #101426, #75054, .T. ) ;
#5156 = UNCERTAINTY_MEASURE_WITH_UNIT (LENGTH_MEASURE( 1.000000000000000082E-05 ), #88552, 'distance_accuracy_value', 'NONE');
#5157 = ORIENTED_EDGE ( 'NONE', *, *, #103851, .F. ) ;
#5158 = CARTESIAN_POINT ( 'NONE',  ( -25.22241582816893413, -4.285714285714295357, 1.650803255657545376 ) ) ;
#5159 = FILL_AREA_STYLE_COLOUR ( '', #16390 ) ;
#5160 = DIRECTION ( 'NONE',  ( 0.000000000000000000, 0.000000000000000000, -1.000000000000000000 ) ) ;
#5161 = DIRECTION ( 'NONE',  ( -1.000000000000000000, 0.000000000000000000, 0.000000000000000000 ) ) ;
#5162 = DIRECTION ( 'NONE',  ( 1.000000000000000000, 0.000000000000000000, 0.000000000000000000 ) ) ;
#5163 = CARTESIAN_POINT ( 'NONE',  ( -16.07816244837682262, 5.101897851420679864, 4.232350007288137483 ) ) ;
#5164 = VERTEX_POINT ( 'NONE', #90826 ) ;
#5165 = DIRECTION ( 'NONE',  ( 0.000000000000000000, 0.000000000000000000, -1.000000000000000000 ) ) ;
#5166 = CARTESIAN_POINT ( 'NONE',  ( 88.35295536199733135, -29.99999999999992539, 187.5720053298597918 ) ) ;
#5167 = CARTESIAN_POINT ( 'NONE',  ( -13.29658299777914365, 24.24203747270784248, -3.158285168994459990 ) ) ;
#5169 = EDGE_CURVE ( 'NONE', #63754, #64539, #14768, .T. ) ;
#5168 = CARTESIAN_POINT ( 'NONE',  ( 7.500000000000001776, -2.571118828324945760, -0.3627527587569074341 ) ) ;
#5170 = CARTESIAN_POINT ( 'NONE',  ( 77.60255351419164072, -29.99999999999999645, -16.19249867753874739 ) ) ;
#5171 =( BOUNDED_CURVE ( )  B_SPLINE_CURVE ( 2, ( #18513, #52986, #60043, #11980, #100463, #85352, #27154, #102599, #19604 ),
 .UNSPECIFIED., .F., .F. ) 
 B_SPLINE_CURVE_WITH_KNOTS ( ( 3, 2, 2, 2, 3 ),
 ( 0.4264705882352941568, 0.4338235294117647745, 0.4411764705882353366, 0.4485294117647059542, 0.4558823529411765163 ),
 .UNSPECIFIED. ) 
 CURVE ( )  GEOMETRIC_REPRESENTATION_ITEM ( )  RATIONAL_B_SPLINE_CURVE ( ( 0.9999999999999994449, 0.9238795325112872936, 1.000000000000000000, 0.9238795325112867385, 1.000000000000000000, 0.9238795325112867385, 1.000000000000000000, 0.9238795325112861834, 1.000000000000000666 ) ) 
 REPRESENTATION_ITEM ( '' )  );
#5172 = CARTESIAN_POINT ( 'NONE',  ( 80.40000000000000568, 1.023464760207051730E-14, 0.000000000000000000 ) ) ;
#5173 = ORIENTED_EDGE ( 'NONE', *, *, #83164, .F. ) ;
#5174 = STYLED_ITEM ( 'NONE', ( #88841 ), #46357 ) ;
#5175 = ORIENTED_EDGE ( 'NONE', *, *, #78369, .T. ) ;
#5176 = ORIENTED_EDGE ( 'NONE', *, *, #104320, .F. ) ;
#5177 = DIRECTION ( 'NONE',  ( -1.000000000000000000, 0.000000000000000000, 0.000000000000000000 ) ) ;
#5178 = DIRECTION ( 'NONE',  ( 0.000000000000000000, -1.000000000000000000, 0.000000000000000000 ) ) ;
#5179 = CARTESIAN_POINT ( 'NONE',  ( -37.56673239365863282, 25.47613764497371847, -13.45617127781024891 ) ) ;
#5180 = CARTESIAN_POINT ( 'NONE',  ( -8.000000000000001776, -16.34375000409677270, 3.313708498984759387 ) ) ;
#5181 = CARTESIAN_POINT ( 'NONE',  ( -6.928203230275508773, -85.00000000000000000, 4.000000000000001776 ) ) ;
#5182 = LINE ( 'NONE', #48266, #98409 ) ;
#5184 = ORIENTED_EDGE ( 'NONE', *, *, #42895, .T. ) ;
#5183 = CIRCLE ( 'NONE', #65451, 4.000000000000001776 ) ;
#5185 = CARTESIAN_POINT ( 'NONE',  ( 42.57704743493908950, 486.1612337113410263, 7.852296464539637810 ) ) ;
#5186 = ORIENTED_EDGE ( 'NONE', *, *, #38471, .F. ) ;
#5187 = B_SPLINE_CURVE_WITH_KNOTS ( 'NONE', 3,
 ( #54266, #30044, #93704, #86163 ),
 .UNSPECIFIED., .F., .F.,
 ( 4, 4 ),
 ( 0.000000000000000000, 0.0002807886668503978950 ),
 .UNSPECIFIED. ) ;
#5188 = CARTESIAN_POINT ( 'NONE',  ( 0.000000000000000000, 0.000000000000000000, 112.0000000000000000 ) ) ;
#5189 = SURFACE_STYLE_USAGE ( .BOTH. , #104392 ) ;
#5190 = CARTESIAN_POINT ( 'NONE',  ( -39.04140135027484604, 485.1684443570406984, -4.294922607834923411 ) ) ;
#5191 = CARTESIAN_POINT ( 'NONE',  ( 4.240583847320349875, 300.6920699671493935, -10.01075340237639466 ) ) ;
#5192 = CARTESIAN_POINT ( 'NONE',  ( 63.47440578363637798, -42.95821100843742357, 83.53516802226259585 ) ) ;
#5193 = VERTEX_POINT ( 'NONE', #63910 ) ;
#5194 = CIRCLE ( 'NONE', #86196, 4.000000000000000000 ) ;
#5195 = CARTESIAN_POINT ( 'NONE',  ( -7.412969763095563103, 41.14559726925956085, -68.91429205793708945 ) ) ;
#5196 = CARTESIAN_POINT ( 'NONE',  ( -65.57582204172831553, -37.93122577949567642, -32.64385588336286759 ) ) ;
#5197 = CARTESIAN_POINT ( 'NONE',  ( 3.840629472727446691E-14, -1.200000000000000030E-05, 29.75000000000000355 ) ) ;
#5198 = VECTOR ( 'NONE', #11222, 999.9999999999998863 ) ;
#5199 = CARTESIAN_POINT ( 'NONE',  ( -6.928203230275510549, 85.00000000000000000, 4.000000000000000000 ) ) ;
#5200 = EDGE_CURVE ( 'NONE', #86888, #37002, #96796, .T. ) ;
#5201 = B_SPLINE_CURVE_WITH_KNOTS ( 'NONE', 3,
 ( #55499, #81375, #46380, #13990, #62573, #39883, #5898, #89496 ),
 .UNSPECIFIED., .F., .F.,
 ( 4, 2, 2, 4 ),
 ( 0.01261646774359793076, 0.01360218180360692891, 0.01458789586361592880, 0.01655932398363392857 ),
 .UNSPECIFIED. ) ;
#5202 = ORIENTED_EDGE ( 'NONE', *, *, #48044, .F. ) ;
#5203 = CIRCLE ( 'NONE', #41371, 3.309500000000001663 ) ;
#5204 = CARTESIAN_POINT ( 'NONE',  ( -61.96882301508342294, -60.00000000000000000, -29.16134989615447282 ) ) ;
#5205 = EDGE_CURVE ( 'NONE', #45709, #31195, #54775, .T. ) ;
#5206 = EDGE_CURVE ( 'NONE', #87241, #99736, #27183, .T. ) ;
#5207 = LINE ( 'NONE', #37071, #46099 ) ;
#5208 = CARTESIAN_POINT ( 'NONE',  ( 8.000000000000000000, -30.68750000409677625, 0.000000000000000000 ) ) ;
#5209 = CARTESIAN_POINT ( 'NONE',  ( 2.241046694639053261, 6.576374040526321352, -6.171384342982665139 ) ) ;
#5210 = CARTESIAN_POINT ( 'NONE',  ( 86.86677769205006427, -24.33857869492717896, 185.9205046572136268 ) ) ;
#5211 = CARTESIAN_POINT ( 'NONE',  ( -5.134976600207776798, -1.158348134558966791, -20.02593271448602863 ) ) ;
#5212 = AXIS2_PLACEMENT_3D ( 'NONE', #12655, #13718, #80043 ) ;
#5213 = CARTESIAN_POINT ( 'NONE',  ( -9.743481593188134227, 8.211523606429958377, 5.000000000000000888 ) ) ;
#5214 = CARTESIAN_POINT ( 'NONE',  ( 33.74163818581530450, -22.91772919730411928, -31.53376869490962520 ) ) ;
#5215 = CARTESIAN_POINT ( 'NONE',  ( 11.62073187254187800, 304.6006958623242440, 8.883628455833934012 ) ) ;
#5216 = CARTESIAN_POINT ( 'NONE',  ( 13.48739679499482058, -52.95995205322599020, 23.24594036347893677 ) ) ;
#5217 = DIRECTION ( 'NONE',  ( 1.000000000000000000, 0.000000000000000000, 0.000000000000000000 ) ) ;
#5218 = CARTESIAN_POINT ( 'NONE',  ( -100.7601573074881856, -30.00000000000000711, 180.6867523902226651 ) ) ;
#5219 = EDGE_CURVE ( 'NONE', #3905, #13645, #22528, .T. ) ;
#5220 = B_SPLINE_CURVE_WITH_KNOTS ( 'NONE', 3,
 ( #94494, #61059, #93953, #20106, #52950, #77765, #86413, #12474, #40477, #23801, #15140, #80397, #8104, #55579, #65818, #90632, #89569, #39959, #48557, #31369, #105222, #56650, #64763, #98181, #5976, #7043, #64246, #88515 ),
 .UNSPECIFIED., .F., .F.,
 ( 4, 2, 2, 2, 2, 2, 2, 2, 2, 2, 2, 2, 2, 4 ),
 ( 0.007040904414468357811, 0.007507994684082224500, 0.007741539818889156543, 0.007975084953696087720, 0.008208630088503018896, 0.008442175223309951806, 0.008909265492923803750, 0.009376355762537657429, 0.009843446032151509373, 0.01077762657137921153, 0.01171180711060691194, 0.01264598764983461410, 0.01358016818906231452, 0.01451434872829001493 ),
 .UNSPECIFIED. ) ;
#5221 = DIRECTION ( 'NONE',  ( 0.000000000000000000, 1.000000000000000000, 0.000000000000000000 ) ) ;
#5222 = CARTESIAN_POINT ( 'NONE',  ( 22.78484890785721007, -57.67311484157481516, 42.64563236796616508 ) ) ;
#5223 = CONICAL_SURFACE ( 'NONE', #13750, 13.50000000000000178, 1.047197551196596077 ) ;
#5225 = DIRECTION ( 'NONE',  ( 0.000000000000000000, 0.000000000000000000, -1.000000000000000000 ) ) ;
#5224 = CARTESIAN_POINT ( 'NONE',  ( 12.04984095491230001, 10.49891318694633036, -9.702198819609494151 ) ) ;
#5226 = EDGE_CURVE ( 'NONE', #54541, #6367, #37223, .T. ) ;
#5227 = FACE_OUTER_BOUND ( 'NONE', #50890, .T. ) ;
#5228 = CARTESIAN_POINT ( 'NONE',  ( -17.96553647165958623, 50.00000000000000000, 61.93371160714927726 ) ) ;
#5229 = CARTESIAN_POINT ( 'NONE',  ( -9.999999999999998224, 15.00000000000000000, 1.785846837348918736E-15 ) ) ;
#5230 = CARTESIAN_POINT ( 'NONE',  ( 26.84999999999999787, 1.533819458162526451E-15, 0.000000000000000000 ) ) ;
#5231 = APPLICATION_CONTEXT ( 'automotive_design' ) ;
#5232 = DIRECTION ( 'NONE',  ( -1.000000000000000000, 0.000000000000000000, 0.000000000000000000 ) ) ;
#5233 = CARTESIAN_POINT ( 'NONE',  ( 1.971262872859045587E-15, -1.023477375540016387, -16.09658290236430389 ) ) ;
#5234 = DIRECTION ( 'NONE',  ( -1.000000000000000000, -0.000000000000000000, -0.000000000000000000 ) ) ;
#5235 = ORIENTED_EDGE ( 'NONE', *, *, #102815, .T. ) ;
#5236 = CARTESIAN_POINT ( 'NONE',  ( 5.839745530781595306, 11.94268483786961710, 3.859993546116442076 ) ) ;
#5237 = DIRECTION ( 'NONE',  ( -1.000000000000000000, -0.000000000000000000, -0.000000000000000000 ) ) ;
#5238 = CARTESIAN_POINT ( 'NONE',  ( -13.66789640398582506, -53.40249338299810233, 32.88025485198195952 ) ) ;
#5240 = CARTESIAN_POINT ( 'NONE',  ( -35.01745854983780504, 439.9565213148654266, 24.34375494391401418 ) ) ;
#5239 = CARTESIAN_POINT ( 'NONE',  ( -106.4066146825508525, -59.99999999999998579, 177.3607894768842357 ) ) ;
#5241 = ORIENTED_EDGE ( 'NONE', *, *, #61476, .T. ) ;
#5242 = AXIS2_PLACEMENT_3D ( 'NONE', #8587, #24803, #89522 ) ;
#5243 = CARTESIAN_POINT ( 'NONE',  ( -7.500000000000007105, -3.000000000000000000, -68.91429205785459544 ) ) ;
#5244 = SURFACE_SIDE_STYLE ('',( #88287 ) ) ;
#5245 = CARTESIAN_POINT ( 'NONE',  ( -7.000000000000000000, -15.93202192939576989, -5.930487099830191511 ) ) ;
#5246 = AXIS2_PLACEMENT_3D ( 'NONE', #45040, #43430, #3503 ) ;
#5247 = EDGE_CURVE ( 'NONE', #48174, #39800, #78535, .T. ) ;
#5248 = CARTESIAN_POINT ( 'NONE',  ( 15.28599664425438931, 3.173649883747179157, -3.309198297947178347 ) ) ;
#5249 = CARTESIAN_POINT ( 'NONE',  ( -24.37088254901632567, 295.3567874699774620, -9.892597027135842325 ) ) ;
#5250 = EDGE_LOOP ( 'NONE', ( #40177, #54221, #49647, #46580 ) ) ;
#5251 = DIRECTION ( 'NONE',  ( 0.000000000000000000, 0.000000000000000000, 1.000000000000000000 ) ) ;
#5252 = AXIS2_PLACEMENT_3D ( 'NONE', #43173, #11308, #84692 ) ;
#5254 = CARTESIAN_POINT ( 'NONE',  ( 44.49963734947851890, 484.8409368627545746, 4.258617019819923577 ) ) ;
#5253 = CARTESIAN_POINT ( 'NONE',  ( 19.83349330513379982, 4.000000000000002665, 0.000000000000000000 ) ) ;
#5255 = CARTESIAN_POINT ( 'NONE',  ( -10.50000000000000711, -5.000000000000000000, -77.33514508527181874 ) ) ;
#5256 =( NAMED_UNIT ( * ) PLANE_ANGLE_UNIT ( ) SI_UNIT ( $, .RADIAN. ) );
#5257 = ORIENTED_EDGE ( 'NONE', *, *, #51467, .T. ) ;
#5258 = ORIENTED_EDGE ( 'NONE', *, *, #11734, .F. ) ;
#5259 = CARTESIAN_POINT ( 'NONE',  ( -26.91057709476854143, 308.9819425013278078, 11.14264308179486918 ) ) ;
#5260 = EDGE_LOOP ( 'NONE', ( #105112, #11609 ) ) ;
#5261 = CIRCLE ( 'NONE', #41367, 9.000000000000000000 ) ;
#5262 = CARTESIAN_POINT ( 'NONE',  ( 32.61650669486618881, 4.898587196589411843E-16, -4.000000000000000888 ) ) ;
#5263 = CARTESIAN_POINT ( 'NONE',  ( 3.313708498984762496, -12.96875000409676915, 7.999999999999998224 ) ) ;
#5264 = VERTEX_POINT ( 'NONE', #8829 ) ;
#5265 = EDGE_CURVE ( 'NONE', #39998, #88814, #74617, .T. ) ;
#5266 = DIRECTION ( 'NONE',  ( 0.000000000000000000, 0.000000000000000000, 1.000000000000000000 ) ) ;
#5267 = CARTESIAN_POINT ( 'NONE',  ( -6.840796741955091242, 41.85687303122205805, -69.25136139280520808 ) ) ;
#5268 = CARTESIAN_POINT ( 'NONE',  ( -93.10945532521039070, -59.99999999999134559, 204.9187477655829923 ) ) ;
#5269 = VECTOR ( 'NONE', #48043, 1000.000000000000000 ) ;
#5270 = CARTESIAN_POINT ( 'NONE',  ( 43.78670674861668743, 485.1174847320907020, -0.7624762964478807303 ) ) ;
#5271 = CARTESIAN_POINT ( 'NONE',  ( 52.96195712877477746, -59.99999999999034372, -39.71698208206965575 ) ) ;
#5272 = LINE ( 'NONE', #22003, #35686 ) ;
#5273 = CARTESIAN_POINT ( 'NONE',  ( -5.363597346086541151, 41.33266196706063056, -58.39526881795520552 ) ) ;
#5275 = CARTESIAN_POINT ( 'NONE',  ( 11.52855662273420201, -56.87783920999704890, 33.40081634995917881 ) ) ;
#5274 = CARTESIAN_POINT ( 'NONE',  ( -111.4777060157506128, -60.00000000000003553, 136.6114436209108760 ) ) ;
#5276 = EDGE_CURVE ( 'NONE', #54991, #60656, #95859, .T. ) ;
#5277 = CARTESIAN_POINT ( 'NONE',  ( -7.313038074512826725, 52.12733562386607389, 2.972571716980497492 ) ) ;
#5278 = EDGE_CURVE ( 'NONE', #29468, #6808, #20078, .T. ) ;
#5279 = CARTESIAN_POINT ( 'NONE',  ( -48.68168605414437167, -60.29016101526869420, 55.32621818811512071 ) ) ;
#5280 = DIRECTION ( 'NONE',  ( 0.000000000000000000, -0.000000000000000000, -1.000000000000000000 ) ) ;
#5281 = VERTEX_POINT ( 'NONE', #69737 ) ;
#5282 = CARTESIAN_POINT ( 'NONE',  ( 40.69645897022265757, 459.9644416451189954, 1.990281397237154692 ) ) ;
#5283 = EDGE_CURVE ( 'NONE', #94655, #112, #102630, .T. ) ;
#5284 = CARTESIAN_POINT ( 'NONE',  ( 81.26467260280679739, 1.016364837396684119E-14, 0.000000000000000000 ) ) ;
#5285 = EDGE_CURVE ( 'NONE', #69907, #74576, #12534, .T. ) ;
#5286 = TOROIDAL_SURFACE ( 'NONE', #82726, 12.00000000000003908, 1.000000000000000000 ) ;
#5287 = DIRECTION ( 'NONE',  ( -0.000000000000000000, 1.000000000000000000, 0.000000000000000000 ) ) ;
#5288 = EDGE_LOOP ( 'NONE', ( #73036, #35357 ) ) ;
#5289 = CARTESIAN_POINT ( 'NONE',  ( -4.470931500626729616, -8.781224379427507998, 13.55547115919427448 ) ) ;
#5290 = VERTEX_POINT ( 'NONE', #21740 ) ;
#5291 = CARTESIAN_POINT ( 'NONE',  ( 103.7884372076644013, -30.00000000000040501, 196.7705344244245111 ) ) ;
#5292 = DIRECTION ( 'NONE',  ( 0.000000000000000000, 0.000000000000000000, 1.000000000000000000 ) ) ;
#5294 = EDGE_CURVE ( 'NONE', #21676, #78587, #86478, .T. ) ;
#5293 = CARTESIAN_POINT ( 'NONE',  ( 6.849721346867525540, 41.84384207023756375, -59.83401400531045056 ) ) ;
#5295 = CARTESIAN_POINT ( 'NONE',  ( -38.36535705883633085, 18.64316884711714195, -5.022013495247519721 ) ) ;
#5296 = CARTESIAN_POINT ( 'NONE',  ( 95.92227023446287149, -29.99999999999999645, 191.2948881066602098 ) ) ;
#5297 = DIRECTION ( 'NONE',  ( 0.000000000000000000, -1.000000000000000000, 0.000000000000000000 ) ) ;
#5298 = ORIENTED_EDGE ( 'NONE', *, *, #54205, .T. ) ;
#5299 = ORIENTED_EDGE ( 'NONE', *, *, #85732, .F. ) ;
#5300 = ORIENTED_EDGE ( 'NONE', *, *, #49935, .F. ) ;
#5301 = LINE ( 'NONE', #93389, #76670 ) ;
#5302 = CARTESIAN_POINT ( 'NONE',  ( -45.99999999999995737, 436.0465585466099014, 12.15788407233835677 ) ) ;
#5303 = VECTOR ( 'NONE', #57715, 1000.000000000000000 ) ;
#5304 = CYLINDRICAL_SURFACE ( 'NONE', #35947, 7.000000000000000000 ) ;
#5305 = ORIENTED_EDGE ( 'NONE', *, *, #73333, .T. ) ;
#5306 = CARTESIAN_POINT ( 'NONE',  ( 0.000000000000000000, 0.000000000000000000, 0.000000000000000000 ) ) ;
#5307 = CIRCLE ( 'NONE', #50021, 0.9999999999999955591 ) ;
#5308 = ORIENTED_EDGE ( 'NONE', *, *, #39887, .T. ) ;
#5309 = DIRECTION ( 'NONE',  ( -1.000000000000000000, 0.000000000000000000, 0.000000000000000000 ) ) ;
#5310 = CARTESIAN_POINT ( 'NONE',  ( 88.55857370903616754, -38.54383131503518456, 200.1465328989446562 ) ) ;
#5311 = CARTESIAN_POINT ( 'NONE',  ( 13.92939803725944259, 2.720116051143699476, 5.535782246604351364 ) ) ;
#5312 = CARTESIAN_POINT ( 'NONE',  ( 84.94965200653656723, -52.70721121321142988, 8.412351094543845775 ) ) ;
#5313 = CARTESIAN_POINT ( 'NONE',  ( 5.600000207755286397, 12.35529564071043040, 7.521652571618187011E-15 ) ) ;
#5314 = DIRECTION ( 'NONE',  ( 0.000000000000000000, 1.000000000000000000, 0.000000000000000000 ) ) ;
#5315 = CARTESIAN_POINT ( 'NONE',  ( -42.64966854229462001, 465.0854819100622422, 13.23715615004961599 ) ) ;
#5316 = CARTESIAN_POINT ( 'NONE',  ( 7.500000000000000000, 4.330127018922189208, -7.422398894150033399 ) ) ;
#5317 = FILL_AREA_STYLE_COLOUR ( '', #93989 ) ;
#5318 = SURFACE_STYLE_USAGE ( .BOTH. , #79723 ) ;
#5319 = ORIENTED_EDGE ( 'NONE', *, *, #48836, .F. ) ;
#5320 = CARTESIAN_POINT ( 'NONE',  ( 5.691929483231186637, 5.629165124598853431, 3.249999999999998668 ) ) ;
#5321 = CARTESIAN_POINT ( 'NONE',  ( -33.50309374949996766, 462.9597815144458650, 5.626781216141202080 ) ) ;
#5322 = CIRCLE ( 'NONE', #19143, 1.000000000000000000 ) ;
#5323 = CARTESIAN_POINT ( 'NONE',  ( -26.02892717936697053, 37.04797716037987243, 9.463389932884222588 ) ) ;
#5324 = VERTEX_POINT ( 'NONE', #78342 ) ;
#5325 = CARTESIAN_POINT ( 'NONE',  ( -3.340000000000000746, 4.090320309152161009E-16, -0.4621369752184079083 ) ) ;
#5326 = CARTESIAN_POINT ( 'NONE',  ( -33.88476750031885842, 303.0319408999416737, 11.82541583672366414 ) ) ;
#5327 = CARTESIAN_POINT ( 'NONE',  ( 24.63846153846153797, 1.411358822780289120E-15, 0.000000000000000000 ) ) ;
#5328 = CARTESIAN_POINT ( 'NONE',  ( 5.656854249492378806, -12.68749999999999467, 5.656854249492381470 ) ) ;
#5329 = CARTESIAN_POINT ( 'NONE',  ( -38.11555372032616873, -36.98165116605179037, 47.45724135341656336 ) ) ;
#5330 =( BOUNDED_SURFACE ( )  B_SPLINE_SURFACE ( 3, 2, ( 
 ( #28114, #21091, #60989 ),
 ( #37800, #102500, #45336 ),
 ( #93876, #20035, #28643 ),
 ( #70129, #70661, #103555 ),
 ( #103035, #61528, #13463 ),
 ( #20582, #53928, #86859 ),
 ( #14515, #49010, #24782 ),
 ( #15062, #30759, #40404 ),
 ( #15594, #105145, #57630 ),
 ( #90021, #55502, #105667 ) ),
 .UNSPECIFIED., .F., .F., .F. ) 
 B_SPLINE_SURFACE_WITH_KNOTS ( ( 4, 2, 2, 2, 4 ),
 ( 3, 3 ),
 ( 0.002450517525418905579, 0.003060732775749475110, 0.003670948026080045074, 0.004891378526741184569, 0.007332239528063463560 ),
 ( 0.000000000000000000, 1.000000000000000000 ),
 .UNSPECIFIED. ) 
 GEOMETRIC_REPRESENTATION_ITEM ( )  RATIONAL_B_SPLINE_SURFACE ( (
 ( 1.000000000000000000, 0.7071067811865475727, 1.000000000000000000),
 ( 1.000000000000000000, 0.7344063550101432858, 1.000000000000000000),
 ( 1.000000000000000000, 0.7590375248711684897, 1.000000000000000000),
 ( 1.000000000000000000, 0.8038331608703419562, 1.000000000000000000),
 ( 1.000000000000000000, 0.8240352460866020579, 1.000000000000000000),
 ( 1.000000000000000000, 0.8791017378333015886, 1.000000000000000000),
 ( 1.000000000000000000, 0.9085032776981116776, 1.000000000000000000),
 ( 1.000000000000000000, 0.9784170511696360650, 1.000000000000000000),
 ( 1.000000000000000000, 0.9996598051696939935, 1.000000000000000000),
 ( 1.000000000000000000, 1.000000000000000000, 1.000000000000000000) ) ) 
 REPRESENTATION_ITEM ( '' )  SURFACE ( )  );
#5331 = ADVANCED_FACE ( 'NONE', ( #79407 ), #20348, .F. ) ;
#5332 = CARTESIAN_POINT ( 'NONE',  ( 28.86650669486618881, 1.474610560812782335E-15, 0.000000000000000000 ) ) ;
#5334 = EDGE_LOOP ( 'NONE', ( #87031, #100414, #14652, #73546, #45242 ) ) ;
#5333 =( BOUNDED_SURFACE ( )  B_SPLINE_SURFACE ( 3, 2, ( 
 ( #51430, #10437, #33684 ),
 ( #43353, #75165, #91379 ),
 ( #17497, #1258, #27206 ),
 ( #67098, #101050, #26153 ),
 ( #82197, #60095, #92960 ),
 ( #74102, #59009, #91898 ),
 ( #19120, #192, #33156 ),
 ( #20188, #60621, #4488 ),
 ( #12035, #86499, #96553 ),
 ( #20730, #12560, #35830 ),
 ( #19659, #37424, #94027 ),
 ( #3959, #47447, #55524 ) ),
 .UNSPECIFIED., .F., .F., .F. ) 
 B_SPLINE_SURFACE_WITH_KNOTS ( ( 4, 2, 2, 2, 2, 4 ),
 ( 3, 3 ),
 ( 6.615801656506548056E-16, 0.0007735885786029156547, 0.001547177157205169729, 0.001933971446506296604, 0.002320765735807423479, 0.003094354314409677661 ),
 ( 0.000000000000000000, 1.000000000000000000 ),
 .UNSPECIFIED. ) 
 GEOMETRIC_REPRESENTATION_ITEM ( )  RATIONAL_B_SPLINE_SURFACE ( (
 ( 1.000000000000000000, 0.9603284238771456760, 1.000000000000000000),
 ( 1.000000000000000000, 0.9628724889916725482, 1.000000000000000000),
 ( 1.000000000000000000, 0.9663306537744362767, 1.000000000000000000),
 ( 1.000000000000000000, 0.9744563874114811064, 1.000000000000000000),
 ( 1.000000000000000000, 0.9789903143386875506, 1.000000000000000000),
 ( 1.000000000000000000, 0.9855527733005724489, 1.000000000000000000),
 ( 1.000000000000000000, 0.9877025284828782059, 1.000000000000000000),
 ( 1.000000000000000000, 0.9916277982505483646, 1.000000000000000000),
 ( 1.000000000000000000, 0.9934221110298375734, 1.000000000000000000),
 ( 1.000000000000000000, 0.9980179737615564317, 1.000000000000000000),
 ( 1.000000000000000000, 1.000016370385808928, 1.000000000000000000),
 ( 1.000000000000000000, 1.000000000000000000, 1.000000000000000000) ) ) 
 REPRESENTATION_ITEM ( '' )  SURFACE ( )  );
#5335 = CARTESIAN_POINT ( 'NONE',  ( 83.99905227920338291, -46.55430364312917391, 184.5977050623376954 ) ) ;
#5337 = EDGE_CURVE ( 'NONE', #16556, #11414, #73431, .T. ) ;
#5336 = CARTESIAN_POINT ( 'NONE',  ( -49.02571528365156439, 7.903708718522313603, 16.36159347772456130 ) ) ;
#5338 = CARTESIAN_POINT ( 'NONE',  ( 4.551587301587302292, -1.200583151104948731, 104.4018401814738155 ) ) ;
#5339 = ORIENTED_EDGE ( 'NONE', *, *, #14456, .T. ) ;
#5340 = CARTESIAN_POINT ( 'NONE',  ( 94.39577478536416777, -57.67124450908064404, -0.09368570482560956147 ) ) ;
#5341 = COLOUR_RGB ( '', 0.66274510, 0.83137255, 0.94901961) ;
#5342 = CARTESIAN_POINT ( 'NONE',  ( 9.165151389911697422, 249.7370448908366143, 4.000000000000004441 ) ) ;
#5343 = PLANE ( 'NONE',  #31462 ) ;
#5344 = CARTESIAN_POINT ( 'NONE',  ( -30.48982775277903201, 7.748378201987720537, 41.81310123456335504 ) ) ;
#5345 = DIRECTION ( 'NONE',  ( 0.000000000000000000, 0.000000000000000000, 1.000000000000000000 ) ) ;
#5346 = VECTOR ( 'NONE', #17120, 1000.000000000000000 ) ;
#5347 = VECTOR ( 'NONE', #23157, 999.9999999999998863 ) ;
#5348 = CARTESIAN_POINT ( 'NONE',  ( -33.00000000000000000, 500.0000000000002274, 0.000000000000000000 ) ) ;
#5349 = AXIS2_PLACEMENT_3D ( 'NONE', #6421, #75953, #9607 ) ;
#5350 = CARTESIAN_POINT ( 'NONE',  ( 2.323340773570302442, -0.2161414388124262287, 102.3935653434436688 ) ) ;
#5351 = CARTESIAN_POINT ( 'NONE',  ( 32.46779435786267243, -22.86540350073456906, 32.67550843060059407 ) ) ;
#5353 = CARTESIAN_POINT ( 'NONE',  ( -44.11331465659100104, 485.7406967462471243, 4.043683577890781145 ) ) ;
#5352 = CARTESIAN_POINT ( 'NONE',  ( 41.57463006680435313, 490.5138385441047149, 10.95471580061642669 ) ) ;
#5354 = MECHANICAL_DESIGN_GEOMETRIC_PRESENTATION_REPRESENTATION (  '', ( #103585 ), #13949 ) ;
#5355 = PRESENTATION_STYLE_ASSIGNMENT (( #6925 ) ) ;
#5356 = CARTESIAN_POINT ( 'NONE',  ( 40.95420997525301487, 387.0967036739339164, 27.26945002580065136 ) ) ;
#5357 = CARTESIAN_POINT ( 'NONE',  ( 38.80611043514134906, 310.3396361600358659, 1.678686578570257604 ) ) ;
#5358 = DIRECTION ( 'NONE',  ( 0.000000000000000000, 1.000000000000000000, 0.000000000000000000 ) ) ;
#5359 = EDGE_CURVE ( 'NONE', #15011, #90051, #85941, .T. ) ;
#5360 = CARTESIAN_POINT ( 'NONE',  ( -102.2638839044604708, -37.99999999999999289, 159.8928815567210791 ) ) ;
#5361 = PRODUCT_DEFINITION_SHAPE ( 'NONE', 'NONE',  #65408 ) ;
#5362 = VERTEX_POINT ( 'NONE', #96133 ) ;
#5363 = CARTESIAN_POINT ( 'NONE',  ( -9.586442202745699248, -3.380526504394860687, 14.88677015134535608 ) ) ;
#5364 = CARTESIAN_POINT ( 'NONE',  ( -3.962208369018801833E-15, 6.732211846623392226, -4.339467034331192075 ) ) ;
#5365 = CARTESIAN_POINT ( 'NONE',  ( 5.909259836070534178, -61.13722795757932715, -1.072443315311459200 ) ) ;
#5367 = CARTESIAN_POINT ( 'NONE',  ( -0.001407372325411601578, -47.40884528607705306, -34.79112416808659702 ) ) ;
#5366 = DIRECTION ( 'NONE',  ( -1.000000000000000000, -1.224606353822377258E-16, -0.000000000000000000 ) ) ;
#5368 = ORIENTED_EDGE ( 'NONE', *, *, #66094, .T. ) ;
#5369 = CARTESIAN_POINT ( 'NONE',  ( 57.19142787028389563, -60.00000000000000000, 91.73163585818134891 ) ) ;
#5370 = ORIENTED_EDGE ( 'NONE', *, *, #84729, .F. ) ;
#5371 = AXIS2_PLACEMENT_3D ( 'NONE', #25603, #9350, #40672 ) ;
#5372 = CARTESIAN_POINT ( 'NONE',  ( 6.169949891409287623, 4.949864754176874548, 4.426582755168845473 ) ) ;
#5373 = CIRCLE ( 'NONE', #84603, 4.000000000000007105 ) ;
#5374 = CARTESIAN_POINT ( 'NONE',  ( 10.59999999999999609, 1.533819458162526451E-15, 0.000000000000000000 ) ) ;
#5375 = CARTESIAN_POINT ( 'NONE',  ( -92.16884015762632032, -60.00000000000000000, -13.23401553576926126 ) ) ;
#5376 = ORIENTED_EDGE ( 'NONE', *, *, #81041, .T. ) ;
#5377 = CARTESIAN_POINT ( 'NONE',  ( 6.362990258380369468, 41.99999999999664624, -58.90232955951054095 ) ) ;
#5378 = CARTESIAN_POINT ( 'NONE',  ( 19.50000000000000000, 12.99999999999999289, -6.999999999999999112 ) ) ;
#5379 = CARTESIAN_POINT ( 'NONE',  ( -10.00004721872059754, 25.99988195318847772, -0.2617599822266526433 ) ) ;
#5381 = DIRECTION ( 'NONE',  ( 0.000000000000000000, -1.000000000000000000, 0.000000000000000000 ) ) ;
#5380 = CARTESIAN_POINT ( 'NONE',  ( 8.572527594031475162E-16, -46.00000000000000000, 105.0000000000000000 ) ) ;
#5382 = CARTESIAN_POINT ( 'NONE',  ( -84.03169659675084802, -29.04760639451814441, 162.8244371882715313 ) ) ;
#5383 = ORIENTED_EDGE ( 'NONE', *, *, #32507, .F. ) ;
#5384 = CARTESIAN_POINT ( 'NONE',  ( -4.418225343294782448, -0.000000000000000000, -16.46939662769500856 ) ) ;
#5385 = ORIENTED_EDGE ( 'NONE', *, *, #29003, .F. ) ;
#5386 = ORIENTED_EDGE ( 'NONE', *, *, #75544, .T. ) ;
#5387 = DIRECTION ( 'NONE',  ( -1.000000000000000000, -1.224606353822377258E-16, -0.000000000000000000 ) ) ;
#5388 = ORIENTED_EDGE ( 'NONE', *, *, #13975, .T. ) ;
#5389 = AXIS2_PLACEMENT_3D ( 'NONE', #12183, #28413, #102265 ) ;
#5390 = CARTESIAN_POINT ( 'NONE',  ( 16.02987949830365011, 45.83140534720696735, -6.508315408883887265 ) ) ;
#5391 = LINE ( 'NONE', #88436, #15143 ) ;
#5392 = CARTESIAN_POINT ( 'NONE',  ( -87.17917008083185237, -57.58863837343483283, 203.1758066736668980 ) ) ;
#5393 = CARTESIAN_POINT ( 'NONE',  ( -4.815811321232738251, -66.80076707697375582, 3.581116321197038932 ) ) ;
#5394 = EDGE_CURVE ( 'NONE', #15029, #87062, #33836, .T. ) ;
#5395 = CARTESIAN_POINT ( 'NONE',  ( -13.63040502537293364, 294.5432906843956289, -2.065628440375496755 ) ) ;
#5396 = FACE_OUTER_BOUND ( 'NONE', #80591, .T. ) ;
#5397 = CARTESIAN_POINT ( 'NONE',  ( 87.76937946118395928, -14.21045842199442433, -6.551255600857777139 ) ) ;
#5398 = EDGE_CURVE ( 'NONE', #63587, #76134, #37309, .T. ) ;
#5399 = CARTESIAN_POINT ( 'NONE',  ( -70.85198506086598513, -59.99999999999993605, 164.3657034848495186 ) ) ;
#5400 = EDGE_CURVE ( 'NONE', #56691, #12868, #73872, .T. ) ;
#5401 = CARTESIAN_POINT ( 'NONE',  ( -55.90002588988700438, -53.38502262911126905, 68.14443619204867275 ) ) ;
#5402 = ORIENTED_EDGE ( 'NONE', *, *, #2241, .F. ) ;
#5403 = DIRECTION ( 'NONE',  ( -1.000000000000000000, -0.000000000000000000, -0.000000000000000000 ) ) ;
#5404 = ORIENTED_EDGE ( 'NONE', *, *, #78889, .T. ) ;
#5405 = CARTESIAN_POINT ( 'NONE',  ( -101.3229872063272126, -52.72700633799254888, 193.0131086346895302 ) ) ;
#5406 = CARTESIAN_POINT ( 'NONE',  ( -1.250645447352602302, 51.63769438765763908, 9.152833739580529482 ) ) ;
#5407 = ORIENTED_EDGE ( 'NONE', *, *, #9730, .T. ) ;
#5408 = CARTESIAN_POINT ( 'NONE',  ( 19.45402185089408320, 49.97988350549956493, 60.58872670499978597 ) ) ;
#5409 = DIRECTION ( 'NONE',  ( -1.000000000000000000, -1.224606353822377258E-16, -0.000000000000000000 ) ) ;
#5410 = CARTESIAN_POINT ( 'NONE',  ( -2.977408999572650039, -10.06250000204838280, -7.188101187500001821 ) ) ;
#5411 = MECHANICAL_DESIGN_GEOMETRIC_PRESENTATION_REPRESENTATION (  '', ( #19247 ), #86429 ) ;
#5412 = ADVANCED_FACE ( 'NONE', ( #65351 ), #81500, .T. ) ;
#5414 = CARTESIAN_POINT ( 'NONE',  ( -40.88293604215247967, 432.5779639752643675, 26.56799667982232549 ) ) ;
#5413 = UNCERTAINTY_MEASURE_WITH_UNIT (LENGTH_MEASURE( 1.000000000000000082E-05 ), #8374, 'distance_accuracy_value', 'NONE');
#5415 = CARTESIAN_POINT ( 'NONE',  ( -9.041223022389656805, 43.82561790570887439, -14.35408047631669248 ) ) ;
#5416 = CARTESIAN_POINT ( 'NONE',  ( 0.000000000000000000, 0.000000000000000000, -3.393184225085859929 ) ) ;
#5417 = DIRECTION ( 'NONE',  ( 0.000000000000000000, 1.000000000000000000, 0.000000000000000000 ) ) ;
#5418 = CARTESIAN_POINT ( 'NONE',  ( -28.36237863811216897, -22.10885024312786129, 29.53413804810376675 ) ) ;
#5419 = ORIENTED_EDGE ( 'NONE', *, *, #88252, .F. ) ;
#5420 = ORIENTED_EDGE ( 'NONE', *, *, #69631, .F. ) ;
#5421 = CARTESIAN_POINT ( 'NONE',  ( 47.61335411246825089, -53.35666067661759371, 51.28262531696475435 ) ) ;
#5422 = DIRECTION ( 'NONE',  ( 1.000000000000000000, 1.224606353822377258E-16, 0.000000000000000000 ) ) ;
#5423 = COLOUR_RGB ( '', 0.09019608, 0.27058824, 0.51372549) ;
#5424 = CARTESIAN_POINT ( 'NONE',  ( -6.769785244694102921, 16.58291839180370175, 1.797443303175164209 ) ) ;
#5425 = AXIS2_PLACEMENT_3D ( 'NONE', #70060, #37736, #37193 ) ;
#5426 = CARTESIAN_POINT ( 'NONE',  ( -110.8605419238568999, -38.35619012346779755, 166.9666919078160277 ) ) ;
#5427 = ORIENTED_EDGE ( 'NONE', *, *, #56694, .T. ) ;
#5428 = CARTESIAN_POINT ( 'NONE',  ( 91.33513191089157601, -38.39909729304942232, -10.01622609513604978 ) ) ;
#5429 = CARTESIAN_POINT ( 'NONE',  ( 82.14211595064963944, -60.00000000000011369, 187.9158604088532911 ) ) ;
#5430 = DIRECTION ( 'NONE',  ( -1.000000000000000000, -1.224606353822377258E-16, -0.000000000000000000 ) ) ;
#5431 = CARTESIAN_POINT ( 'NONE',  ( 30.00000000000000000, 464.1059074601051861, 11.21808947555551761 ) ) ;
#5432 = FACE_OUTER_BOUND ( 'NONE', #12491, .T. ) ;
#5433 = CARTESIAN_POINT ( 'NONE',  ( -31.95432916196071105, 439.7272652150242038, 23.87563020249913848 ) ) ;
#5434 = CARTESIAN_POINT ( 'NONE',  ( -32.21355997171083629, 436.2367427661213242, 19.10635534054698326 ) ) ;
#5435 = CARTESIAN_POINT ( 'NONE',  ( -31.79789196896621561, 436.0544141482667442, 18.02941909552264477 ) ) ;
#5436 = CARTESIAN_POINT ( 'NONE',  ( 4.999999999999065636, -61.61648432250720475, 12.73941221456567163 ) ) ;
#5437 = CARTESIAN_POINT ( 'NONE',  ( 95.33093839319907659, -60.00000000000000711, 202.5686516758067910 ) ) ;
#5438 = DIRECTION ( 'NONE',  ( 0.000000000000000000, 0.000000000000000000, 1.000000000000000000 ) ) ;
#5439 = ORIENTED_EDGE ( 'NONE', *, *, #56234, .T. ) ;
#5440 = CARTESIAN_POINT ( 'NONE',  ( 56.66478156921341025, -18.67503977128396642, 55.37327426273083830 ) ) ;
#5441 = CARTESIAN_POINT ( 'NONE',  ( -31.64006577679478482, 298.9319948211945075, -1.094726330376324164 ) ) ;
#5442 = CARTESIAN_POINT ( 'NONE',  ( 8.000113193197767814, 34.00022638645860695, -0.2613481123984610077 ) ) ;
#5443 = CIRCLE ( 'NONE', #55383, 63.00000000000000000 ) ;
#5444 = ORIENTED_EDGE ( 'NONE', *, *, #32507, .T. ) ;
#5446 = CARTESIAN_POINT ( 'NONE',  ( -9.677640526858340309, -50.98637785014530976, 24.47418066717162333 ) ) ;
#5445 = CARTESIAN_POINT ( 'NONE',  ( -91.30009454865734142, -38.40134775628936836, -10.51120872120718097 ) ) ;
#5447 = FACE_OUTER_BOUND ( 'NONE', #4647, .T. ) ;
#5448 = CARTESIAN_POINT ( 'NONE',  ( 31.37378682588860102, 432.3277640841818084, 23.18600726979659399 ) ) ;
#5449 = CARTESIAN_POINT ( 'NONE',  ( 91.95555555555554861, -4.171999999999998820, 5.616230220889773285E-16 ) ) ;
#5450 = CARTESIAN_POINT ( 'NONE',  ( -5.082755093536325042, -11.46875000204838635, -5.082755093536325930 ) ) ;
#5451 = TOROIDAL_SURFACE ( 'NONE', #63981, 12.00000000000001066, 3.000000000000000000 ) ;
#5452 = CARTESIAN_POINT ( 'NONE',  ( 9.739726766104286781, -3.000000000000002665, -87.61747884499031613 ) ) ;
#5453 = ADVANCED_FACE ( 'NONE', ( #97172 ), #33422, .F. ) ;
#5454 = AXIS2_PLACEMENT_3D ( 'NONE', #33192, #99477, #26190 ) ;
#5456 = EDGE_LOOP ( 'NONE', ( #13635, #53666, #96911, #62829 ) ) ;
#5455 = CARTESIAN_POINT ( 'NONE',  ( -32.85155332502864667, 463.8111683108724037, 7.359358840565868753 ) ) ;
#5457 = CARTESIAN_POINT ( 'NONE',  ( 84.44844196884631060, -29.00443322529857682, 166.8952161098262934 ) ) ;
#5458 = CARTESIAN_POINT ( 'NONE',  ( 9.269852382678077873, 11.68551705847642275, -0.000000000000000000 ) ) ;
#5459 = CARTESIAN_POINT ( 'NONE',  ( 36.31378453431777587, 28.20125269961366854, 12.06226767304767478 ) ) ;
#5460 = ORIENTED_EDGE ( 'NONE', *, *, #18934, .T. ) ;
#5461 = CARTESIAN_POINT ( 'NONE',  ( -31.93762527360473413, 311.0806311593118494, -8.077542931250780711 ) ) ;
#5462 = CARTESIAN_POINT ( 'NONE',  ( 17.76962432240387812, 34.18902918576760186, 23.80189063641344305 ) ) ;
#5463 = DIRECTION ( 'NONE',  ( -0.000000000000000000, -0.000000000000000000, -1.000000000000000000 ) ) ;
#5464 = CARTESIAN_POINT ( 'NONE',  ( 0.000000000000000000, 50.50000000000000000, 0.000000000000000000 ) ) ;
#5465 = DIRECTION ( 'NONE',  ( -1.000000000000000000, -0.000000000000000000, -0.000000000000000000 ) ) ;
#5466 =( BOUNDED_SURFACE ( )  B_SPLINE_SURFACE ( 3, 2, ( 
 ( #28371, #45069, #87646 ),
 ( #54709, #44532, #29954 ),
 ( #101695, #94689, #94132 ),
 ( #95207, #85523, #77420 ) ),
 .UNSPECIFIED., .F., .F., .F. ) 
 B_SPLINE_SURFACE_WITH_KNOTS ( ( 4, 4 ),
 ( 3, 3 ),
 ( 2.125036258071588691E-17, 0.002033478645169251378 ),
 ( 0.000000000000000000, 1.000000000000000000 ),
 .UNSPECIFIED. ) 
 GEOMETRIC_REPRESENTATION_ITEM ( )  RATIONAL_B_SPLINE_SURFACE ( (
 ( 1.000000000000000000, 0.7976994903569333273, 1.000000000000000000),
 ( 1.000000000000000000, 0.8066624588212726321, 1.000000000000000000),
 ( 1.000000000000000000, 0.8158483196103470947, 1.000000000000000000),
 ( 1.000000000000000000, 0.8239349643288683689, 1.000000000000000000) ) ) 
 REPRESENTATION_ITEM ( '' )  SURFACE ( )  );
#5467 = EDGE_CURVE ( 'NONE', #80842, #64161, #21828, .T. ) ;
#5468 = VERTEX_POINT ( 'NONE', #60021 ) ;
#5469 = CARTESIAN_POINT ( 'NONE',  ( -76.42400522962535092, -29.99999999999999645, -17.06061772383467101 ) ) ;
#5470 = CARTESIAN_POINT ( 'NONE',  ( -5.000000000000000888, -40.36500490292060306, -0.7636728796266644137 ) ) ;
#5471 = CARTESIAN_POINT ( 'NONE',  ( 0.000000000000000000, 6.123233995736770227E-16, -5.000000000000002665 ) ) ;
#5472 = CARTESIAN_POINT ( 'NONE',  ( -0.08974973093378038613, -18.03000550220510334, 35.00499666190406600 ) ) ;
#5473 = CARTESIAN_POINT ( 'NONE',  ( -5.082755093536326818, -18.21875000204838457, 5.082755093536325042 ) ) ;
#5474 = CARTESIAN_POINT ( 'NONE',  ( 11.68506151312264585, 302.5966585334010119, -10.05423947740817958 ) ) ;
#5475 = CARTESIAN_POINT ( 'NONE',  ( 13.58349330513380515, 1.593028355512270962E-15, 0.000000000000000000 ) ) ;
#5476 = EDGE_CURVE ( 'NONE', #77149, #70292, #93432, .T. ) ;
#5477 = CONTEXT_DEPENDENT_SHAPE_REPRESENTATION ( #77678, #54548 ) ;
#5478 = ORIENTED_EDGE ( 'NONE', *, *, #65308, .F. ) ;
#5479 = COLOUR_RGB ( '', 0.31764706, 0.68627451, 0.89019608) ;
#5480 = AXIS2_PLACEMENT_3D ( 'NONE', #15270, #72443, #23389 ) ;
#5481 = CARTESIAN_POINT ( 'NONE',  ( 0.000000000000000000, 0.000000000000000000, 0.000000000000000000 ) ) ;
#5482 = CARTESIAN_POINT ( 'NONE',  ( 1.797870618166049539, 41.33266196706049556, -58.72278032362722655 ) ) ;
#5483 = AXIS2_PLACEMENT_3D ( 'NONE', #1026, #48544, #73344 ) ;
#5484 = CARTESIAN_POINT ( 'NONE',  ( -8.308397487264409520, 32.82220968432262964, 0.000000000000000000 ) ) ;
#5485 = EDGE_CURVE ( 'NONE', #53038, #87076, #104833, .T. ) ;
#5486 = LINE ( 'NONE', #61626, #36046 ) ;
#5487 = CARTESIAN_POINT ( 'NONE',  ( -14.36577178753972994, 3.159923610478025058, 4.257245723753212197 ) ) ;
#5488 = B_SPLINE_CURVE_WITH_KNOTS ( 'NONE', 3,
 ( #70972, #30010, #86125, #103350, #37051, #87701, #69917, #46693, #73606, #57954, #105974, #89816, #66060, #73066, #8350, #65000, #49871, #48795, #40188, #7809, #90877, #98937, #15916, #97356, #33190, #32119, #31601, #7281, #751, #56890 ),
 .UNSPECIFIED., .F., .F.,
 ( 4, 2, 2, 2, 2, 2, 2, 2, 2, 2, 2, 2, 2, 2, 4 ),
 ( 0.01451434872829011555, 0.01497952839231836766, 0.01521211822433249199, 0.01544470805634661631, 0.01567729788836074237, 0.01590988772037486496, 0.01637506738440312748, 0.01684024704843139000, 0.01730542671245965253, 0.01823578604051618104, 0.01916614536857271303, 0.02009650469662924155, 0.02102686402468577354, 0.02149204368871403953, 0.02195722335274230899 ),
 .UNSPECIFIED. ) ;
#5489 = EDGE_LOOP ( 'NONE', ( #20882, #40346, #66456, #7647, #64585 ) ) ;
#5490 = CARTESIAN_POINT ( 'NONE',  ( 30.11650669486618881, 1.474610560812782335E-15, 0.000000000000000000 ) ) ;
#5491 = CARTESIAN_POINT ( 'NONE',  ( 45.59999999999999432, 1.533819458162526451E-15, 0.000000000000000000 ) ) ;
#5492 = ORIENTED_EDGE ( 'NONE', *, *, #68893, .T. ) ;
#5494 = CARTESIAN_POINT ( 'NONE',  ( 5.299999999999999822, 5.388445916248354013E-16, 4.400000000000000355 ) ) ;
#5493 = VECTOR ( 'NONE', #38270, 1000.000000000000000 ) ;
#5495 = PRESENTATION_STYLE_ASSIGNMENT (( #71280 ) ) ;
#5496 = CARTESIAN_POINT ( 'NONE',  ( -36.42954435870697694, 40.26420082970585668, -57.71663982892543032 ) ) ;
#5497 = CARTESIAN_POINT ( 'NONE',  ( 6.585304930659546585, 4.021878819315965359, -6.499999999999999112 ) ) ;
#5498 = CARTESIAN_POINT ( 'NONE',  ( -112.1962952311318134, -60.00000000000000000, 169.8889608969054734 ) ) ;
#5499 = CARTESIAN_POINT ( 'NONE',  ( 0.000000000000000000, 1.714505518806294638E-15, -14.00000000000000000 ) ) ;
#5500 = CARTESIAN_POINT ( 'NONE',  ( 43.89279753500678538, 435.4168038201353284, 16.20034641759606586 ) ) ;
#5501 = CARTESIAN_POINT ( 'NONE',  ( -84.23719628859713282, -42.98023119072136211, 182.9348151746076496 ) ) ;
#5502 = ORIENTED_EDGE ( 'NONE', *, *, #38130, .T. ) ;
#5503 = EDGE_CURVE ( 'NONE', #11528, #25938, #21172, .T. ) ;
#5504 = CARTESIAN_POINT ( 'NONE',  ( 43.56300790393845546, 41.43655928470000305, -50.61076563407275586 ) ) ;
#5505 = ORIENTED_EDGE ( 'NONE', *, *, #36927, .F. ) ;
#5506 =( NAMED_UNIT ( * ) SI_UNIT ( $, .STERADIAN. ) SOLID_ANGLE_UNIT ( ) );
#5507 = CARTESIAN_POINT ( 'NONE',  ( 5.727189096784631062, -68.57869875248739788, -1.806430436190349376 ) ) ;
#5508 = CARTESIAN_POINT ( 'NONE',  ( -87.19071514201230855, -60.15150547609031406, 31.77301145132557636 ) ) ;
#5509 = CARTESIAN_POINT ( 'NONE',  ( 35.58361799548379167, 5.000000000000003553, 0.000000000000000000 ) ) ;
#5510 = DIRECTION ( 'NONE',  ( 0.000000000000000000, 0.000000000000000000, 1.000000000000000000 ) ) ;
#5511 = CARTESIAN_POINT ( 'NONE',  ( 2.955796066023817836, 98.65787461558377913, -5.000000000000000888 ) ) ;
#5512 = PLANE ( 'NONE',  #47637 ) ;
#5513 = CARTESIAN_POINT ( 'NONE',  ( 38.36535705883633796, 18.64316884711713840, 5.022013495247446890 ) ) ;
#5514 = CARTESIAN_POINT ( 'NONE',  ( 81.10520000301197285, -14.21045842199436926, 192.6066858413676925 ) ) ;
#5515 = CARTESIAN_POINT ( 'NONE',  ( -97.37795077744138439, -14.21045842199441722, 96.97852642953840530 ) ) ;
#5516 = MECHANICAL_DESIGN_GEOMETRIC_PRESENTATION_REPRESENTATION (  '', ( #41704 ), #26281 ) ;
#5517 = CARTESIAN_POINT ( 'NONE',  ( -66.25603766433088992, -36.00965392168274803, 88.05982369710793023 ) ) ;
#5518 = ORIENTED_EDGE ( 'NONE', *, *, #14262, .F. ) ;
#5519 = CARTESIAN_POINT ( 'NONE',  ( 60.45584459710401859, 39.42448681592218662, 24.06197592465746382 ) ) ;
#5520 = CARTESIAN_POINT ( 'NONE',  ( 74.18019383371068898, -60.00000000000248690, 189.7622998913098229 ) ) ;
#5521 = ORIENTED_EDGE ( 'NONE', *, *, #5155, .T. ) ;
#5522 = DIRECTION ( 'NONE',  ( 0.000000000000000000, -1.000000000000000000, 0.000000000000000000 ) ) ;
#5523 = CARTESIAN_POINT ( 'NONE',  ( 2.977408999572652260, -21.31250000204838813, 7.188101187500000044 ) ) ;
#5524 = ORIENTED_EDGE ( 'NONE', *, *, #23404, .F. ) ;
#5525 = ORIENTED_EDGE ( 'NONE', *, *, #49602, .F. ) ;
#5526 = CARTESIAN_POINT ( 'NONE',  ( 10.91152070480431568, 45.93327767897820024, -13.06343554040043919 ) ) ;
#5527 = CARTESIAN_POINT ( 'NONE',  ( 46.95966155981695778, 18.79500983735056963, -14.95375697514157132 ) ) ;
#5528 = CARTESIAN_POINT ( 'NONE',  ( -92.13623215974652680, -60.00000000000000000, 3.793454175199357792 ) ) ;
#5529 = DIRECTION ( 'NONE',  ( 0.000000000000000000, 0.000000000000000000, 1.000000000000000000 ) ) ;
#5530 = CARTESIAN_POINT ( 'NONE',  ( -5.082755093536326818, -9.218750002048382797, 5.082755093536325042 ) ) ;
#5531 = CARTESIAN_POINT ( 'NONE',  ( 0.000000000000000000, 0.000000000000000000, 0.000000000000000000 ) ) ;
#5532 = EDGE_CURVE ( 'NONE', #88846, #33881, #61381, .T. ) ;
#5533 = CARTESIAN_POINT ( 'NONE',  ( 1.000000000000000000, -40.36147667352812363, -0.7651093971834536100 ) ) ;
#5534 = CARTESIAN_POINT ( 'NONE',  ( 1.308996937480704004, 49.99999999999999289, -75.00000000000001421 ) ) ;
#5535 = EDGE_CURVE ( 'NONE', #76580, #64598, #102716, .T. ) ;
#5536 = CARTESIAN_POINT ( 'NONE',  ( -45.99999999999998579, 438.2690552493292557, 10.57781013089698519 ) ) ;
#5537 = CARTESIAN_POINT ( 'NONE',  ( -41.09810318407317453, 320.7440978425470917, 4.299128587728701767 ) ) ;
#5538 = CARTESIAN_POINT ( 'NONE',  ( 29.11493748322932618, 306.8126351454100700, -9.108972071340021515 ) ) ;
#5539 = VERTEX_POINT ( 'NONE', #5982 ) ;
#5540 = DIRECTION ( 'NONE',  ( 0.000000000000000000, 0.000000000000000000, 1.000000000000000000 ) ) ;
#5541 = CARTESIAN_POINT ( 'NONE',  ( 35.45451790554718485, -32.57629471585633496, 34.20714003089912580 ) ) ;
#5542 = CARTESIAN_POINT ( 'NONE',  ( 2.083846472846741813E-15, -1.734723475976807094E-15, 17.01589776168603407 ) ) ;
#5543 = EDGE_CURVE ( 'NONE', #23499, #100791, #71258, .T. ) ;
#5544 = ORIENTED_EDGE ( 'NONE', *, *, #78358, .T. ) ;
#5545 = DIRECTION ( 'NONE',  ( -0.000000000000000000, 0.000000000000000000, 1.000000000000000000 ) ) ;
#5546 = VERTEX_POINT ( 'NONE', #95543 ) ;
#5548 = CARTESIAN_POINT ( 'NONE',  ( -31.19792890532719198, 414.2215770364159084, 25.44228638033458623 ) ) ;
#5547 = DIRECTION ( 'NONE',  ( -1.000000000000000000, -0.000000000000000000, -0.000000000000000000 ) ) ;
#5549 = DIRECTION ( 'NONE',  ( -1.000000000000000000, 0.000000000000000000, 0.000000000000000000 ) ) ;
#5550 = CARTESIAN_POINT ( 'NONE',  ( 6.643884894376898664, -3.901062859470944222, -6.756839076126442301 ) ) ;
#5551 = DIRECTION ( 'NONE',  ( 0.000000000000000000, 1.000000000000000000, 0.000000000000000000 ) ) ;
#5552 = CARTESIAN_POINT ( 'NONE',  ( -48.15057074821032757, 16.50253122541020190, -14.35535821593460604 ) ) ;
#5553 = CYLINDRICAL_SURFACE ( 'NONE', #29779, 4.000000000000000888 ) ;
#5554 = CARTESIAN_POINT ( 'NONE',  ( 98.00624854155054777, -59.99999999999999289, 68.96488094194445750 ) ) ;
#5555 = CARTESIAN_POINT ( 'NONE',  ( 27.10511071441176867, 34.75829513984540142, -7.556984339686343866 ) ) ;
#5557 = CARTESIAN_POINT ( 'NONE',  ( -43.49681020211324523, 485.4584596168100461, 3.971815216374599888 ) ) ;
#5556 = CONICAL_SURFACE ( 'NONE', #29768, 3.309500000000007880, 0.9599310885968770357 ) ;
#5558 = AXIS2_PLACEMENT_3D ( 'NONE', #1453, #34417, #99632 ) ;
#5559 = DIRECTION ( 'NONE',  ( -1.000000000000000000, -1.224606353822377258E-16, -0.000000000000000000 ) ) ;
#5560 = CARTESIAN_POINT ( 'NONE',  ( -10.49999999997808331, -5.000000000000000000, -12.52300748972991506 ) ) ;
#5561 = ORIENTED_EDGE ( 'NONE', *, *, #37468, .T. ) ;
#5562 = CARTESIAN_POINT ( 'NONE',  ( -89.53105629151139055, -30.00000000001332623, 3.004387943588768373 ) ) ;
#5563 = ORIENTED_EDGE ( 'NONE', *, *, #24288, .F. ) ;
#5564 =( NAMED_UNIT ( * ) PLANE_ANGLE_UNIT ( ) SI_UNIT ( $, .RADIAN. ) );
#5565 = DIRECTION ( 'NONE',  ( 0.000000000000000000, 0.000000000000000000, -1.000000000000000000 ) ) ;
#5566 = CARTESIAN_POINT ( 'NONE',  ( 3.591870599023073485, 23.61213490889384659, 5.000000000000000000 ) ) ;
#5567 = CARTESIAN_POINT ( 'NONE',  ( 14.89114929831721135, 23.12273819885287551, 0.2580741681286142231 ) ) ;
#5568 = AXIS2_PLACEMENT_3D ( 'NONE', #8980, #9504, #58064 ) ;
#5569 = CARTESIAN_POINT ( 'NONE',  ( 5.082755093536325930, -31.34375000204838457, -5.082755093536325042 ) ) ;
#5570 = CARTESIAN_POINT ( 'NONE',  ( 13.58349330513380160, 1.593028355512270567E-15, 0.000000000000000000 ) ) ;
#5571 = LINE ( 'NONE', #104261, #62919 ) ;
#5572 = AXIS2_PLACEMENT_3D ( 'NONE', #68233, #43427, #1879 ) ;
#5573 = ORIENTED_EDGE ( 'NONE', *, *, #69858, .T. ) ;
#5574 = ADVANCED_FACE ( 'NONE', ( #62144 ), #16626, .T. ) ;
#5576 = EDGE_LOOP ( 'NONE', ( #30220, #95488, #4852, #52584, #43115, #100259 ) ) ;
#5575 = DIRECTION ( 'NONE',  ( -1.000000000000000000, 0.000000000000000000, 0.000000000000000000 ) ) ;
#5577 = CARTESIAN_POINT ( 'NONE',  ( 80.03392445538010236, -32.55901999570951233, 138.7251254010801915 ) ) ;
#5578 = B_SPLINE_CURVE_WITH_KNOTS ( 'NONE', 3,
 ( #67265, #93662, #85580, #1967, #60254, #68323, #67784, #100144, #25780, #27374, #50514, #59706, #43512, #100672, #76391, #26835, #26309, #19812, #92583, #11655, #36525, #18738, #19294, #42437, #93121, #52118, #35994, #10595, #68866, #58638, #52649, #77475, #91538, #17651, #78000, #88223 ),
 .UNSPECIFIED., .F., .F.,
 ( 4, 2, 2, 2, 2, 2, 2, 2, 2, 2, 2, 2, 2, 2, 2, 2, 2, 4 ),
 ( 0.01291936762762759330, 0.01372441420841340187, 0.01452946078919920871, 0.01533450736998501727, 0.01613955395077082411, 0.01694460053155663268, 0.01774964711234244125, 0.01855469369312824982, 0.01935974027391405838, 0.02016478685469986348, 0.02096983343548567205, 0.02177488001627148062, 0.02257992659705728572, 0.02338497317784309429, 0.02419001975862890286, 0.02459254304902180888, 0.02499506633941471143, 0.02580011292020051999 ),
 .UNSPECIFIED. ) ;
#5579 = CARTESIAN_POINT ( 'NONE',  ( -38.76857929379224288, 27.37303770309710416, -11.85268573845290696 ) ) ;
#5580 = EDGE_LOOP ( 'NONE', ( #51468, #55203, #82744, #64999, #84871, #98218 ) ) ;
#5581 = CARTESIAN_POINT ( 'NONE',  ( -3.400000000000000355, 4.163799117101001052E-16, -0.4455245229258316120 ) ) ;
#5582 = SURFACE_STYLE_FILL_AREA ( #22335 ) ;
#5583 = CARTESIAN_POINT ( 'NONE',  ( 2.977408999572652260, -17.93750000204838457, 7.188101187500000044 ) ) ;
#5584 = CARTESIAN_POINT ( 'NONE',  ( 11.07233799575516286, 45.30046846812411587, 15.14426123305342387 ) ) ;
#5585 = CARTESIAN_POINT ( 'NONE',  ( 17.71442011948034079, 294.6047081709573945, 1.884973053585294211 ) ) ;
#5586 = EDGE_CURVE ( 'NONE', #55144, #76220, #28725, .T. ) ;
#5587 = EDGE_CURVE ( 'NONE', #38016, #70795, #11956, .T. ) ;
#5588 = VERTEX_POINT ( 'NONE', #20656 ) ;
#5589 = AXIS2_PLACEMENT_3D ( 'NONE', #69479, #30628, #96927 ) ;
#5590 = CARTESIAN_POINT ( 'NONE',  ( -16.64348903516496136, 45.60392139269943357, -6.657797401562710604 ) ) ;
#5591 = EDGE_CURVE ( 'NONE', #3333, #57238, #82057, .T. ) ;
#5592 = CIRCLE ( 'NONE', #65867, 15.14825148316532832 ) ;
#5593 = CARTESIAN_POINT ( 'NONE',  ( -5.190609988845228173, -12.63922286743592593, -3.016375611400007539 ) ) ;
#5594 = CARTESIAN_POINT ( 'NONE',  ( 7.262243063959841649, 41.41224388735756179, -59.17677670479952212 ) ) ;
#5595 = CARTESIAN_POINT ( 'NONE',  ( -29.00000000000000355, 0.000000000000000000, 0.000000000000000000 ) ) ;
#5596 = CARTESIAN_POINT ( 'NONE',  ( 4.898587196589412829E-16, -9.312500004096769146, -8.000000000000000000 ) ) ;
#5597 = CARTESIAN_POINT ( 'NONE',  ( -33.77811757699123518, -23.48828957687707231, 33.07784126555895199 ) ) ;
#5598 = SURFACE_STYLE_FILL_AREA ( #102170 ) ;
#5599 = CARTESIAN_POINT ( 'NONE',  ( -46.00000000000000000, 488.5500823950412155, 3.682191395223604946 ) ) ;
#5600 = EDGE_CURVE ( 'NONE', #37759, #50908, #13545, .T. ) ;
#5601 = CARTESIAN_POINT ( 'NONE',  ( 7.500000000000006217, 31.97088361167178050, -52.67517300286424131 ) ) ;
#5602 = CARTESIAN_POINT ( 'NONE',  ( 39.34999999999999432, 1.533819458162526451E-15, 0.000000000000000000 ) ) ;
#5603 = DIRECTION ( 'NONE',  ( 0.1884548733085491812, 0.000000000000000000, 0.9820818503191365290 ) ) ;
#5604 = CARTESIAN_POINT ( 'NONE',  ( 38.56444062946145834, 27.31873531207203598, 12.97723241238764658 ) ) ;
#5605 = ORIENTED_EDGE ( 'NONE', *, *, #88459, .T. ) ;
#5606 = CARTESIAN_POINT ( 'NONE',  ( 10.28624191511840458, 43.25714326066859172, 15.40779740156149202 ) ) ;
#5607 = DIRECTION ( 'NONE',  ( 0.000000000000000000, -1.000000000000000000, 0.000000000000000000 ) ) ;
#5608 = CARTESIAN_POINT ( 'NONE',  ( 24.83349330513380337, 1.593028355512270567E-15, 0.000000000000000000 ) ) ;
#5609 = CARTESIAN_POINT ( 'NONE',  ( 63.34140952676320069, -30.10174061359070663, -32.02184817817584417 ) ) ;
#5610 = CARTESIAN_POINT ( 'NONE',  ( -84.01570479851304185, -30.00000000000000000, 161.1131640044202129 ) ) ;
#5611 = EDGE_CURVE ( 'NONE', #14056, #31918, #6228, .T. ) ;
#5612 = DIRECTION ( 'NONE',  ( 0.000000000000000000, -1.000000000000000000, 0.000000000000000000 ) ) ;
#5613 = ORIENTED_EDGE ( 'NONE', *, *, #67276, .F. ) ;
#5614 = CARTESIAN_POINT ( 'NONE',  ( 0.000000000000000000, -48.79941684889505638, 112.0000000000000000 ) ) ;
#5615 = CARTESIAN_POINT ( 'NONE',  ( 106.9698911830091816, -57.65429730927083796, 200.0955121608643026 ) ) ;
#5616 = CARTESIAN_POINT ( 'NONE',  ( -3.601501433546143538E-16, 15.58845726811991206, -13.00000000000000000 ) ) ;
#5617 = EDGE_CURVE ( 'NONE', #1532, #98241, #63186, .T. ) ;
#5618 = CARTESIAN_POINT ( 'NONE',  ( 14.29190075645216851, 12.99999999999999289, 0.000000000000000000 ) ) ;
#5619 = CARTESIAN_POINT ( 'NONE',  ( -16.14595037814582312, 20.48432867205941932, 4.554748808009636996 ) ) ;
#5620 = CARTESIAN_POINT ( 'NONE',  ( 52.56483885390523625, 40.83906611471594061, -38.23529411764706509 ) ) ;
#5621 = CARTESIAN_POINT ( 'NONE',  ( -73.50155193450905244, -59.99999999999998579, 167.2054298968465957 ) ) ;
#5622 = EDGE_CURVE ( 'NONE', #25775, #1581, #36818, .T. ) ;
#5623 = CIRCLE ( 'NONE', #11008, 4.000000000000001776 ) ;
#5624 = DIRECTION ( 'NONE',  ( 0.000000000000000000, -1.000000000000000000, 0.000000000000000000 ) ) ;
#5625 = DIRECTION ( 'NONE',  ( 1.000000000000000000, 1.224606353822377258E-16, 0.000000000000000000 ) ) ;
#5626 = CARTESIAN_POINT ( 'NONE',  ( -52.56483885390515098, 49.99999999999999289, -38.23529411764716457 ) ) ;
#5627 = CARTESIAN_POINT ( 'NONE',  ( -84.81894751370330710, -50.19651377637536172, 188.8560073178213941 ) ) ;
#5628 = AXIS2_PLACEMENT_3D ( 'NONE', #94228, #93697, #44082 ) ;
#5629 = ORIENTED_EDGE ( 'NONE', *, *, #28525, .T. ) ;
#5630 = CARTESIAN_POINT ( 'NONE',  ( 31.67567424330222536, 316.9529563565766921, -6.082121426484099480 ) ) ;
#5631 = STYLED_ITEM ( 'NONE', ( #31255 ), #51855 ) ;
#5632 = CARTESIAN_POINT ( 'NONE',  ( 12.48044894998498044, -3.649665456918604001, -76.71620004746286270 ) ) ;
#5633 = SURFACE_STYLE_FILL_AREA ( #64417 ) ;
#5634 = CARTESIAN_POINT ( 'NONE',  ( -84.05617864326320898, -52.72894240072567129, -15.15459004269859911 ) ) ;
#5635 = DIRECTION ( 'NONE',  ( 0.000000000000000000, -1.000000000000000000, 0.000000000000000000 ) ) ;
#5636 = CARTESIAN_POINT ( 'NONE',  ( 0.000000000000000000, 4.000000000000003553, 0.000000000000000000 ) ) ;
#5637 = EDGE_LOOP ( 'NONE', ( #49667, #28021, #32433, #57468 ) ) ;
#5638 = AXIS2_PLACEMENT_3D ( 'NONE', #95639, #48122, #97734 ) ;
#5639 = CARTESIAN_POINT ( 'NONE',  ( 18.45801141833800330, 50.00000000000000000, 61.31179837014410339 ) ) ;
#5640 = CARTESIAN_POINT ( 'NONE',  ( 13.59280763750475884, 24.77127418736844788, 0.3411334247565424582 ) ) ;
#5641 = CARTESIAN_POINT ( 'NONE',  ( -20.16952962162108065, -4.285714285713656757, 15.50035291838862683 ) ) ;
#5642 = DIRECTION ( 'NONE',  ( 0.000000000000000000, 0.000000000000000000, 1.000000000000000000 ) ) ;
#5643 = CARTESIAN_POINT ( 'NONE',  ( 69.60540008574220394, -30.00000000000001421, -29.89027719438221453 ) ) ;
#5644 = CARTESIAN_POINT ( 'NONE',  ( -80.71693047659314857, -32.56228764399944708, 142.8125308610640047 ) ) ;
#5645 = ORIENTED_EDGE ( 'NONE', *, *, #28115, .F. ) ;
#5646 = CARTESIAN_POINT ( 'NONE',  ( 1.295095875561511761E-05, -30.00000000000000000, 37.00000000000000711 ) ) ;
#5647 = FACE_OUTER_BOUND ( 'NONE', #86646, .T. ) ;
#5648 = CARTESIAN_POINT ( 'NONE',  ( 93.62081204623362396, -57.61897985685533286, 204.5015724136271444 ) ) ;
#5649 = LINE ( 'NONE', #62843, #18427 ) ;
#5650 = CARTESIAN_POINT ( 'NONE',  ( 37.43609172732153922, 304.6718852671700120, -7.742307645728699228 ) ) ;
#5651 = CARTESIAN_POINT ( 'NONE',  ( -30.00000000000000355, 461.9728594894708635, 12.10976292102400897 ) ) ;
#5652 = VERTEX_POINT ( 'NONE', #69681 ) ;
#5653 = B_SPLINE_CURVE_WITH_KNOTS ( 'NONE', 3,
 ( #97035, #71168, #63091, #104062 ),
 .UNSPECIFIED., .F., .F.,
 ( 4, 4 ),
 ( 4.336808689942017736E-18, 0.001257843226828393984 ),
 .UNSPECIFIED. ) ;
#5654 = CARTESIAN_POINT ( 'NONE',  ( 7.500000000000000888, 0.3744244963005072258, 2.475665546587506316E-15 ) ) ;
#5655 = CARTESIAN_POINT ( 'NONE',  ( 41.50820411079202898, 461.5963371455317770, 2.703439750996501800 ) ) ;
#5657 = CARTESIAN_POINT ( 'NONE',  ( -100.9117355037075754, -37.82075919422305077, 146.9395316649864753 ) ) ;
#5656 = CARTESIAN_POINT ( 'NONE',  ( 16.64348903516524203, 43.75610143575153188, 4.157797401561407646 ) ) ;
#5658 = CARTESIAN_POINT ( 'NONE',  ( 5.082755093536324154, -22.34375000204838457, 5.082755093536326818 ) ) ;
#5659 = CARTESIAN_POINT ( 'NONE',  ( 5.656854249492380582, -20.00000000409677270, -5.656854249492379694 ) ) ;
#5660 = PRESENTATION_LAYER_ASSIGNMENT (  '', '', ( #34954 ) ) ;
#5661 = LINE ( 'NONE', #71990, #36097 ) ;
#5662 = CARTESIAN_POINT ( 'NONE',  ( 7.040971602393473638, 41.74416448739698637, -59.82830749617803434 ) ) ;
#5663 = EDGE_CURVE ( 'NONE', #71421, #42859, #35331, .T. ) ;
#5664 = CARTESIAN_POINT ( 'NONE',  ( 0.000000000000000000, 299.9999999999999432, 6.000000000000000888 ) ) ;
#5665 = DIRECTION ( 'NONE',  ( -1.000000000000000000, -1.224606353822377258E-16, -0.000000000000000000 ) ) ;
#5666 =( GEOMETRIC_REPRESENTATION_CONTEXT ( 3 ) GLOBAL_UNCERTAINTY_ASSIGNED_CONTEXT ( ( #63993 ) ) GLOBAL_UNIT_ASSIGNED_CONTEXT ( ( #22994, #73081, #6777 ) ) REPRESENTATION_CONTEXT ( 'NONE', 'WORKASPACE' ) );
#5667 = CARTESIAN_POINT ( 'NONE',  ( -35.22245897681465721, 463.4774333389162848, 19.78759537333588625 ) ) ;
#5668 = ORIENTED_EDGE ( 'NONE', *, *, #80635, .F. ) ;
#5669 = CARTESIAN_POINT ( 'NONE',  ( 0.4053525175236804001, 3.145852061456247739, 6.499999999999998224 ) ) ;
#5670 = VECTOR ( 'NONE', #29501, 1000.000000000000000 ) ;
#5672 = CARTESIAN_POINT ( 'NONE',  ( 24.88419958317715341, -39.47653737364599635, 31.71990145829097685 ) ) ;
#5671 = CARTESIAN_POINT ( 'NONE',  ( -12.46506237085073110, -30.00000000000006395, 37.03826559298295251 ) ) ;
#5673 = CARTESIAN_POINT ( 'NONE',  ( -24.43671627503044164, 25.27466499483696794, 32.24378702798332341 ) ) ;
#5674 = EDGE_CURVE ( 'NONE', #87774, #95890, #46979, .T. ) ;
#5675 = ORIENTED_EDGE ( 'NONE', *, *, #48128, .F. ) ;
#5676 = ORIENTED_EDGE ( 'NONE', *, *, #32257, .F. ) ;
#5677 = DIRECTION ( 'NONE',  ( 0.4165977904505313578, 0.000000000000000000, 0.9090909090909089496 ) ) ;
#5678 = CARTESIAN_POINT ( 'NONE',  ( 9.797174393178825657E-16, 0.000000000000000000, -8.000000000000000000 ) ) ;
#5679 = CARTESIAN_POINT ( 'NONE',  ( 0.000000000000000000, 0.000000000000000000, 0.000000000000000000 ) ) ;
#5680 = CARTESIAN_POINT ( 'NONE',  ( 31.14131030317610538, 6.123233995736772199E-16, -5.000000000000001776 ) ) ;
#5681 = FILL_AREA_STYLE_COLOUR ( '', #71007 ) ;
#5682 = ORIENTED_EDGE ( 'NONE', *, *, #90673, .F. ) ;
#5683 = CARTESIAN_POINT ( 'NONE',  ( 30.90300773556078084, -60.00000000000000000, -40.80305823694001077 ) ) ;
#5684 = CARTESIAN_POINT ( 'NONE',  ( 89.64643850830432825, 5.000000000000021316, 0.000000000000000000 ) ) ;
#5685 = CARTESIAN_POINT ( 'NONE',  ( -11.68076828077231788, 20.99435049431988531, 7.705273641827774966 ) ) ;
#5686 = LINE ( 'NONE', #87685, #4899 ) ;
#5687 = CARTESIAN_POINT ( 'NONE',  ( 81.51344701192068953, -29.99999999999999645, -9.040800538730334068 ) ) ;
#5688 = CARTESIAN_POINT ( 'NONE',  ( 0.000000000000000000, 0.000000000000000000, 4.000000000000000000 ) ) ;
#5689 = ORIENTED_EDGE ( 'NONE', *, *, #57577, .F. ) ;
#5690 = EDGE_CURVE ( 'NONE', #6418, #79581, #32131, .T. ) ;
#5691 = EDGE_LOOP ( 'NONE', ( #56261, #67960, #35808, #75072, #79133 ) ) ;
#5692 = ORIENTED_EDGE ( 'NONE', *, *, #37906, .F. ) ;
#5693 = CARTESIAN_POINT ( 'NONE',  ( 0.000000000000000000, 0.000000000000000000, 0.000000000000000000 ) ) ;
#5694 = DIRECTION ( 'NONE',  ( 0.000000000000000000, 1.000000000000000000, 0.000000000000000000 ) ) ;
#5695 = CARTESIAN_POINT ( 'NONE',  ( -45.49129229133219354, 409.1704227378016299, 8.337099328860718472 ) ) ;
#5696 = DIRECTION ( 'NONE',  ( 0.000000000000000000, -1.000000000000000000, 0.000000000000000000 ) ) ;
#5697 = FILL_AREA_STYLE_COLOUR ( '', #57869 ) ;
#5698 = CARTESIAN_POINT ( 'NONE',  ( 6.683837171061809634, -7.911893696991943337, -3.558927330633863411E-17 ) ) ;
#5699 = EDGE_LOOP ( 'NONE', ( #104620, #52003, #82601, #48326, #24013 ) ) ;
#5700 = CARTESIAN_POINT ( 'NONE',  ( 6.145467200819017428, 48.00000000000000000, -92.99666842291193802 ) ) ;
#5701 = VERTEX_POINT ( 'NONE', #52959 ) ;
#5702 = ADVANCED_FACE ( 'NONE', ( #85886 ), #44889, .T. ) ;
#5703 = DIRECTION ( 'NONE',  ( -1.000000000000000000, -1.224606353822377258E-16, -0.000000000000000000 ) ) ;
#5704 = DIRECTION ( 'NONE',  ( -0.8191520442889884679, 1.003171929053520679E-16, 0.5735764363510509334 ) ) ;
#5705 = CARTESIAN_POINT ( 'NONE',  ( -39.65933660911444036, 485.2174287600329308, -4.382854859800878522 ) ) ;
#5706 = AXIS2_PLACEMENT_3D ( 'NONE', #28518, #79153, #5280 ) ;
#5707 = CARTESIAN_POINT ( 'NONE',  ( -82.68571612615870947, -60.00000000000005684, 189.3854813724193491 ) ) ;
#5708 = CARTESIAN_POINT ( 'NONE',  ( 62.14462952195434298, -53.38719692732349387, 84.99936359579984924 ) ) ;
#5709 =( GEOMETRIC_REPRESENTATION_CONTEXT ( 3 ) GLOBAL_UNCERTAINTY_ASSIGNED_CONTEXT ( ( #26283 ) ) GLOBAL_UNIT_ASSIGNED_CONTEXT ( ( #61897, #102865, #13832 ) ) REPRESENTATION_CONTEXT ( 'NONE', 'WORKASPACE' ) );
#5710 = ORIENTED_EDGE ( 'NONE', *, *, #15452, .F. ) ;
#5711 = CARTESIAN_POINT ( 'NONE',  ( 38.46722833635603678, 463.5298926290464578, 19.68359823307360301 ) ) ;
#5712 = CARTESIAN_POINT ( 'NONE',  ( -65.16315667887181462, -37.89597709104619128, -32.76824749171753837 ) ) ;
#5713 = STYLED_ITEM ( 'NONE', ( #84298 ), #52429 ) ;
#5714 = CARTESIAN_POINT ( 'NONE',  ( 0.000000000000000000, 304.8518027762758038, -10.00000000000000355 ) ) ;
#5715 = CARTESIAN_POINT ( 'NONE',  ( -47.47329288218261922, -57.67116814553164517, -40.40967777935767202 ) ) ;
#5716 = EDGE_CURVE ( 'NONE', #26896, #44023, #30154, .T. ) ;
#5717 = ORIENTED_EDGE ( 'NONE', *, *, #90616, .F. ) ;
#5718 =( NAMED_UNIT ( * ) PLANE_ANGLE_UNIT ( ) SI_UNIT ( $, .RADIAN. ) );
#5719 = DIRECTION ( 'NONE',  ( -0.000000000000000000, -0.000000000000000000, -1.000000000000000000 ) ) ;
#5720 = CARTESIAN_POINT ( 'NONE',  ( 43.15338089903108454, -60.00000000000001421, -33.32712317583224149 ) ) ;
#5721 = COLOUR_RGB ( '', 0.31764706, 0.68627451, 0.89019608) ;
#5722 = CARTESIAN_POINT ( 'NONE',  ( 4.387778976649724167E-15, 34.08768991669519721, 35.82893434829263413 ) ) ;
#5723 = CARTESIAN_POINT ( 'NONE',  ( -5.656854249492379694, -31.62500000409677270, -5.656854249492380582 ) ) ;
#5724 = CARTESIAN_POINT ( 'NONE',  ( -7.137815226412437930, -4.999999999998865796, -4.175893272574592530 ) ) ;
#5725 = CARTESIAN_POINT ( 'NONE',  ( 86.49766297946776206, -46.48553392096007997, 190.2538031942813461 ) ) ;
#5726 = CARTESIAN_POINT ( 'NONE',  ( -5.217392907308656014, 6.510766470966031783, -27.02462356418083544 ) ) ;
#5727 = CARTESIAN_POINT ( 'NONE',  ( -9.880470762086103420, 7.740809968950301823, 5.000000000000000888 ) ) ;
#5728 = VECTOR ( 'NONE', #70470, 1000.000000000000000 ) ;
#5729 = ORIENTED_EDGE ( 'NONE', *, *, #103598, .T. ) ;
#5730 = CARTESIAN_POINT ( 'NONE',  ( 13.87298779988979724, -50.40831034641927033, 28.89736879381397827 ) ) ;
#5731 = CARTESIAN_POINT ( 'NONE',  ( -4.205882352941162416, -5.000000000000000000, -72.69916451482997388 ) ) ;
#5732 = CARTESIAN_POINT ( 'NONE',  ( 25.54149015966096670, -60.00000000000000000, 41.31963070409977234 ) ) ;
#5733 = VECTOR ( 'NONE', #106496, 1000.000000000000000 ) ;
#5734 = CARTESIAN_POINT ( 'NONE',  ( -98.93669197873286691, -30.00000000000000355, 188.9772157868254965 ) ) ;
#5735 = EDGE_CURVE ( 'NONE', #13365, #65096, #6511, .T. ) ;
#5736 = B_SPLINE_CURVE_WITH_KNOTS ( 'NONE', 3,
 ( #53237, #21951, #70484, #5216, #29526, #13813, #62398, #54802, #95290, #38655, #79617, #4687, #21421, #103895, #87734, #103379, #13279, #19851, #38146, #93698, #37621, #5730, #46207, #79093, #20923, #29016, #46725, #71521, #104422, #30569, #52686, #85614, #86160, #11689 ),
 .UNSPECIFIED., .F., .F.,
 ( 4, 2, 2, 2, 2, 2, 2, 2, 2, 2, 2, 2, 2, 2, 2, 2, 4 ),
 ( 0.000000000000000000, 0.0007857361314144349846, 0.001571472262828869969, 0.002357208394243305062, 0.003142944525657739938, 0.003928680657072174814, 0.004714416788486610124, 0.005500152919901044567, 0.006285889051315479877, 0.007071625182729915186, 0.007857361314144349629, 0.008643097445558784939, 0.009428833576973220248, 0.01021456970838765556, 0.01100030583980208913, 0.01178604197121652444, 0.01257177810263095975 ),
 .UNSPECIFIED. ) ;
#5737 = COLOUR_RGB ( '', 0.40784314, 0.44705882, 0.49803922) ;
#5738 = AXIS2_PLACEMENT_3D ( 'NONE', #24706, #23642, #41393 ) ;
#5739 = FACE_OUTER_BOUND ( 'NONE', #16993, .T. ) ;
#5740 = CARTESIAN_POINT ( 'NONE',  ( 40.07782535012948699, -57.69200939151943430, 55.80417300162885397 ) ) ;
#5742 = CARTESIAN_POINT ( 'NONE',  ( 63.81650669486618455, 4.898587196589294500E-16, -4.000000000000007105 ) ) ;
#5741 = CARTESIAN_POINT ( 'NONE',  ( -9.165151389911699198, 249.9999999999999432, 4.000000000000002665 ) ) ;
#5743 = ADVANCED_FACE ( 'NONE', ( #82538 ), #16204, .T. ) ;
#5744 = CARTESIAN_POINT ( 'NONE',  ( -46.50260707299666763, 39.63181819133366446, -46.56948492247389737 ) ) ;
#5745 = CARTESIAN_POINT ( 'NONE',  ( -17.55366314213746648, 50.00000000000000000, 62.90659931622097645 ) ) ;
#5746 = CARTESIAN_POINT ( 'NONE',  ( -41.49004542385903704, 469.3954094756242625, 1.006055279744931807 ) ) ;
#5747 = CARTESIAN_POINT ( 'NONE',  ( 46.00000000000000000, 488.7535717826328892, 4.225312566654727320 ) ) ;
#5748 = FACE_OUTER_BOUND ( 'NONE', #53867, .T. ) ;
#5749 = FILL_AREA_STYLE_COLOUR ( '', #83777 ) ;
#5750 = CARTESIAN_POINT ( 'NONE',  ( -87.19032044583666163, -28.00046754097470725, 187.4561909348103370 ) ) ;
#5751 = ADVANCED_FACE ( 'NONE', ( #31883 ), #82460, .T. ) ;
#5752 = ORIENTED_EDGE ( 'NONE', *, *, #86543, .F. ) ;
#5753 = CARTESIAN_POINT ( 'NONE',  ( 17.50000000000466827, 49.88162284957544301, 62.03084827767128218 ) ) ;
#5754 = CARTESIAN_POINT ( 'NONE',  ( 14.29190075645216851, 12.99999999999999289, 0.000000000000000000 ) ) ;
#5755 = CARTESIAN_POINT ( 'NONE',  ( -11.08525313475499630, -18.58645957121905212, 27.00989044373123349 ) ) ;
#5757 = DIRECTION ( 'NONE',  ( -1.000000000000000000, 0.000000000000000000, 0.000000000000000000 ) ) ;
#5756 = CARTESIAN_POINT ( 'NONE',  ( -86.09965174442223201, -60.00000000000002132, 13.47334620854856624 ) ) ;
#5758 = ORIENTED_EDGE ( 'NONE', *, *, #39102, .F. ) ;
#5759 = CARTESIAN_POINT ( 'NONE',  ( -43.58313552198230667, 464.0053785828559967, 6.081445975066273490 ) ) ;
#5760 = CARTESIAN_POINT ( 'NONE',  ( 14.95236164052716354, 4.204970931308103843, -5.179833178256462389 ) ) ;
#5761 = DIRECTION ( 'NONE',  ( 0.000000000000000000, -1.000000000000000000, 0.000000000000000000 ) ) ;
#5762 = CARTESIAN_POINT ( 'NONE',  ( 0.000000000000000000, -79.93083296558610584, -75.00000000000001421 ) ) ;
#5763 = CARTESIAN_POINT ( 'NONE',  ( 72.09784563428850390, -59.99999999999999289, 155.0115803735216389 ) ) ;
#5764 = CARTESIAN_POINT ( 'NONE',  ( -29.07128654445882887, 296.9339959557834163, -9.548856946219741459 ) ) ;
#5765 = VERTEX_POINT ( 'NONE', #89042 ) ;
#5766 = CARTESIAN_POINT ( 'NONE',  ( 32.15310320217081141, 439.7024266304580919, 23.94087012106558987 ) ) ;
#5767 =( LENGTH_UNIT ( ) NAMED_UNIT ( * ) SI_UNIT ( .MILLI., .METRE. ) );
#5768 = AXIS2_PLACEMENT_3D ( 'NONE', #37422, #79426, #5540 ) ;
#5769 = CARTESIAN_POINT ( 'NONE',  ( 6.701893401236465486, 41.44328394225253476, -70.59544911815949320 ) ) ;
#5770 = CARTESIAN_POINT ( 'NONE',  ( 7.531577814756222656E-15, 44.00000000000000711, -61.50000000000000000 ) ) ;
#5771 = ORIENTED_EDGE ( 'NONE', *, *, #17948, .T. ) ;
#5772 = CIRCLE ( 'NONE', #41958, 4.250000000000000000 ) ;
#5773 = VERTEX_POINT ( 'NONE', #8642 ) ;
#5774 = CARTESIAN_POINT ( 'NONE',  ( -28.48625763317001613, 313.7440504870126574, 12.33904525942641861 ) ) ;
#5775 = AXIS2_PLACEMENT_3D ( 'NONE', #92787, #27576, #9196 ) ;
#5776 = ORIENTED_EDGE ( 'NONE', *, *, #53760, .F. ) ;
#5777 = CARTESIAN_POINT ( 'NONE',  ( 21.92116886295261935, 305.2355041402309439, 9.019527013375345348 ) ) ;
#5778 =( BOUNDED_CURVE ( )  B_SPLINE_CURVE ( 2, ( #104715, #28762, #21196 ),
 .UNSPECIFIED., .F., .F. ) 
 B_SPLINE_CURVE_WITH_KNOTS ( ( 3, 3 ),
 ( 0.000000000000000000, 1.000000000000000000 ),
 .UNSPECIFIED. ) 
 CURVE ( )  GEOMETRIC_REPRESENTATION_ITEM ( )  RATIONAL_B_SPLINE_CURVE ( ( 1.000000000000000000, 1.857142857142858317, 1.000000000000000000 ) ) 
 REPRESENTATION_ITEM ( '' )  );
#5779 = CARTESIAN_POINT ( 'NONE',  ( -8.000000000000000000, 0.000000000000000000, -3.725171428571429022 ) ) ;
#5780 = ORIENTED_EDGE ( 'NONE', *, *, #54250, .F. ) ;
#5781 = EDGE_CURVE ( 'NONE', #43471, #37118, #92772, .T. ) ;
#5782 = FACE_OUTER_BOUND ( 'NONE', #78734, .T. ) ;
#5783 = CARTESIAN_POINT ( 'NONE',  ( 5.000000000000000000, -13.85537367033550638, 10.16084852767000868 ) ) ;
#5784 = CARTESIAN_POINT ( 'NONE',  ( -78.84470549551073759, -60.00000000000486722, 198.6068565147943161 ) ) ;
#5785 = CARTESIAN_POINT ( 'NONE',  ( 44.23653098086412427, 485.2868257420024634, 1.778614644177207049 ) ) ;
#5786 = CARTESIAN_POINT ( 'NONE',  ( 75.21146677271600822, -60.00000000000000000, 182.8225648044053173 ) ) ;
#5787 = SURFACE_STYLE_USAGE ( .BOTH. , #50882 ) ;
#5788 = CARTESIAN_POINT ( 'NONE',  ( 0.1682240322482835559, 26.07813853931757464, -38.24999999999999289 ) ) ;
#5790 = CARTESIAN_POINT ( 'NONE',  ( 11.12509248473755541, -22.06751002638328174, 27.59088369308159017 ) ) ;
#5789 = CARTESIAN_POINT ( 'NONE',  ( -106.1205840060921730, -60.00000000000004263, 102.8126256328862667 ) ) ;
#5792 = EDGE_CURVE ( 'NONE', #52915, #44815, #4944, .T. ) ;
#5791 = DIRECTION ( 'NONE',  ( -1.000000000000000000, 0.000000000000000000, 0.000000000000000000 ) ) ;
#5793 = CARTESIAN_POINT ( 'NONE',  ( -46.33873388880254396, -49.90047875932729227, 48.28660123752720068 ) ) ;
#5794 = CARTESIAN_POINT ( 'NONE',  ( 2.911360389275831295, -70.20793806422989292, 13.30423068689236210 ) ) ;
#5795 = ORIENTED_EDGE ( 'NONE', *, *, #63676, .T. ) ;
#5796 = CARTESIAN_POINT ( 'NONE',  ( 23.09999999999999432, 1.533819458162526451E-15, 0.000000000000000000 ) ) ;
#5797 = CARTESIAN_POINT ( 'NONE',  ( 16.75187969033571989, 36.38380281757302726, 24.30698433968583316 ) ) ;
#5798 = FACE_BOUND ( 'NONE', #4177, .T. ) ;
#5799 = ORIENTED_EDGE ( 'NONE', *, *, #61995, .F. ) ;
#5800 = CARTESIAN_POINT ( 'NONE',  ( -10.91923657161825822, -10.68772801090689839, 18.23046311196159053 ) ) ;
#5801 = ORIENTED_EDGE ( 'NONE', *, *, #75590, .T. ) ;
#5802 = CARTESIAN_POINT ( 'NONE',  ( 108.4933579148305114, -30.00000000000335731, 186.4703362515614629 ) ) ;
#5803 = CARTESIAN_POINT ( 'NONE',  ( 89.64643850830432825, 1.030564683017419500E-14, 0.000000000000000000 ) ) ;
#5804 = CARTESIAN_POINT ( 'NONE',  ( 0.4973051450610682656, -3.866309095671417673, -8.000000000000001776 ) ) ;
#5805 = CARTESIAN_POINT ( 'NONE',  ( 99.09352263291532381, -30.00000000000000000, 188.6044529824486062 ) ) ;
#5806 = AXIS2_PLACEMENT_3D ( 'NONE', #98417, #88220, #47205 ) ;
#5807 = CARTESIAN_POINT ( 'NONE',  ( 7.000000000000000000, 0.000000000000000000, -13.00000000000000000 ) ) ;
#5808 = ORIENTED_EDGE ( 'NONE', *, *, #102858, .T. ) ;
#5809 = EDGE_CURVE ( 'NONE', #39760, #36282, #54555, .T. ) ;
#5810 = AXIS2_PLACEMENT_3D ( 'NONE', #81964, #40996, #97103 ) ;
#5811 = VERTEX_POINT ( 'NONE', #24338 ) ;
#5812 = ORIENTED_EDGE ( 'NONE', *, *, #18093, .F. ) ;
#5814 = CARTESIAN_POINT ( 'NONE',  ( 0.000000000000000000, -30.00000000000000000, 0.000000000000000000 ) ) ;
#5813 = VECTOR ( 'NONE', #101501, 1000.000000000000000 ) ;
#5815 = DIRECTION ( 'NONE',  ( -0.5735764363510494901, -0.8191520442889894671, 0.000000000000000000 ) ) ;
#5816 = CARTESIAN_POINT ( 'NONE',  ( 0.000000000000000000, 0.000000000000000000, 4.000000000000000888 ) ) ;
#5817 = ADVANCED_FACE ( 'NONE', ( #88521 ), #47507, .T. ) ;
#5818 = ORIENTED_EDGE ( 'NONE', *, *, #57618, .T. ) ;
#5819 = CARTESIAN_POINT ( 'NONE',  ( -16.02741078272298481, 4.186345391436172569, -2.546409592408216405 ) ) ;
#5820 = EDGE_LOOP ( 'NONE', ( #74062, #94489, #56019, #35333 ) ) ;
#5821 = DIRECTION ( 'NONE',  ( -1.000000000000000000, 0.000000000000000000, 0.000000000000000000 ) ) ;
#5822 = CARTESIAN_POINT ( 'NONE',  ( 104.6793613277272925, -38.39935806952897224, 197.8364302557836538 ) ) ;
#5823 = DIRECTION ( 'NONE',  ( 1.000000000000000000, 1.224606353822377258E-16, 0.000000000000000000 ) ) ;
#5824 = CARTESIAN_POINT ( 'NONE',  ( 83.26448648960058563, -37.81913187090151496, -6.272588225319124966 ) ) ;
#5826 = CARTESIAN_POINT ( 'NONE',  ( 79.27568089365161086, -37.99999999999995737, 139.8675762540388803 ) ) ;
#5825 = B_SPLINE_CURVE_WITH_KNOTS ( 'NONE', 3,
 ( #22248, #103667, #72359, #79387 ),
 .UNSPECIFIED., .F., .F.,
 ( 4, 4 ),
 ( 0.000000000000000000, 1.000000000000000000 ),
 .UNSPECIFIED. ) ;
#5827 = CARTESIAN_POINT ( 'NONE',  ( 41.13969092038016839, 328.1746007070119617, 10.04740730255401360 ) ) ;
#5828 = CARTESIAN_POINT ( 'NONE',  ( 7.500000000000001776, 4.330127018922189208, -7.564338275809342704 ) ) ;
#5829 = B_SPLINE_CURVE_WITH_KNOTS ( 'NONE', 3,
 ( #247, #56376, #15940, #89311 ),
 .UNSPECIFIED., .F., .F.,
 ( 4, 4 ),
 ( 0.000000000000000000, 0.001704530934785217656 ),
 .UNSPECIFIED. ) ;
#5830 = CARTESIAN_POINT ( 'NONE',  ( 9.609486011791425142, 143.0915023496523020, 5.000000000000000888 ) ) ;
#5831 = ORIENTED_EDGE ( 'NONE', *, *, #88394, .F. ) ;
#5832 = CARTESIAN_POINT ( 'NONE',  ( -12.49955057333833253, -4.332870170146376765, -12.71907580221295220 ) ) ;
#5833 = CARTESIAN_POINT ( 'NONE',  ( 9.500000000000003553, -5.000000000000000000, -68.91429205785459544 ) ) ;
#5834 = CARTESIAN_POINT ( 'NONE',  ( -25.91464401492078906, 37.21125547857348437, 8.416521324649474778 ) ) ;
#5835 = ORIENTED_EDGE ( 'NONE', *, *, #53165, .F. ) ;
#5836 = CARTESIAN_POINT ( 'NONE',  ( 102.0666666666666629, 1.023464760207051730E-14, 0.000000000000000000 ) ) ;
#5837 = CARTESIAN_POINT ( 'NONE',  ( -34.86182526428664374, 302.9466520364554754, 3.792971351233738631 ) ) ;
#5838 = DIRECTION ( 'NONE',  ( 1.000000000000000000, 0.000000000000000000, 0.000000000000000000 ) ) ;
#5839 = CARTESIAN_POINT ( 'NONE',  ( -6.595563215953496614E-15, -5.469921996229793137, 3.525817189091417170 ) ) ;
#5840 = CARTESIAN_POINT ( 'NONE',  ( -8.000000000000001776, -16.15624999999999289, 3.313708498984758943 ) ) ;
#5841 = CARTESIAN_POINT ( 'NONE',  ( -15.49740174064447196, -17.95698503203060170, 35.11441465487863667 ) ) ;
#5842 =( NAMED_UNIT ( * ) SI_UNIT ( $, .STERADIAN. ) SOLID_ANGLE_UNIT ( ) );
#5843 = AXIS2_PLACEMENT_3D ( 'NONE', #8796, #64920, #66505 ) ;
#5844 = EDGE_LOOP ( 'NONE', ( #27007, #45834, #60404, #73727, #86197, #31275 ) ) ;
#5845 = CARTESIAN_POINT ( 'NONE',  ( 85.90364017214238856, -28.44064950339577180, 181.2095016147336537 ) ) ;
#5846 = CARTESIAN_POINT ( 'NONE',  ( 15.59999999999999787, -3.309499999999999886, 4.475777889183790779E-16 ) ) ;
#5847 = LINE ( 'NONE', #21034, #90037 ) ;
#5848 = ORIENTED_EDGE ( 'NONE', *, *, #40738, .T. ) ;
#5849 = TOROIDAL_SURFACE ( 'NONE', #36931, 10.00000000000000000, 5.000000000000000000 ) ;
#5850 = CARTESIAN_POINT ( 'NONE',  ( 94.23549906357385453, -57.67250308052000918, 23.25353176600918559 ) ) ;
#5851 = CARTESIAN_POINT ( 'NONE',  ( 35.05271644150917609, 437.8393516193232244, 4.418594605297464284 ) ) ;
#5852 = CARTESIAN_POINT ( 'NONE',  ( -29.77394335381484680, 8.177826981235281067, 42.10535821593507677 ) ) ;
#5853 = FILL_AREA_STYLE_COLOUR ( '', #63048 ) ;
#5854 = EDGE_CURVE ( 'NONE', #22652, #105826, #68749, .T. ) ;
#5855 = EDGE_CURVE ( 'NONE', #20128, #65067, #23140, .T. ) ;
#5856 = CARTESIAN_POINT ( 'NONE',  ( 7.016496648689620308, -19.12693412541480598, 35.17887506390064800 ) ) ;
#5857 = CARTESIAN_POINT ( 'NONE',  ( -10.00000000000000000, -5.000000000000000000, -2.617993873628155832 ) ) ;
#5858 = DIRECTION ( 'NONE',  ( 0.000000000000000000, 0.000000000000000000, -1.000000000000000000 ) ) ;
#5859 = CARTESIAN_POINT ( 'NONE',  ( -15.05442749816165104, 5.404963020241716265, 6.510488844712470247 ) ) ;
#5860 = EDGE_CURVE ( 'NONE', #55614, #29736, #105103, .T. ) ;
#5861 = CARTESIAN_POINT ( 'NONE',  ( 9.681569006902808638, 294.6516795043963839, -2.504656372061118130 ) ) ;
#5862 = CARTESIAN_POINT ( 'NONE',  ( 9.168149550320974228, 15.99999999372935022, -3.997425403568101387 ) ) ;
#5863 = DIRECTION ( 'NONE',  ( -1.000000000000000000, 0.000000000000000000, 0.000000000000000000 ) ) ;
#5864 = CARTESIAN_POINT ( 'NONE',  ( -83.11375064820144587, -38.00000000000003553, -10.17571340337245545 ) ) ;
#5865 = AXIS2_PLACEMENT_3D ( 'NONE', #43018, #27412, #66760 ) ;
#5866 = EDGE_CURVE ( 'NONE', #47564, #103578, #106546, .T. ) ;
#5867 = ORIENTED_EDGE ( 'NONE', *, *, #75496, .F. ) ;
#5868 = CARTESIAN_POINT ( 'NONE',  ( -7.882737400093250635, 3.052883471114401726, 14.68611362084002714 ) ) ;
#5869 = CARTESIAN_POINT ( 'NONE',  ( -5.290067270632216712, -1.200000000000000030E-05, 8.531152949374556371 ) ) ;
#5870 = CARTESIAN_POINT ( 'NONE',  ( 5.384233811324311780, -61.99782908655225810, 2.655407383564610146 ) ) ;
#5871 = CONICAL_SURFACE ( 'NONE', #41985, 8.900000000000000355, 0.7853981633974418397 ) ;
#5872 = CARTESIAN_POINT ( 'NONE',  ( -59.17052589201637147, -60.22831900904334645, -29.94874486158233751 ) ) ;
#5873 = ORIENTED_EDGE ( 'NONE', *, *, #32065, .T. ) ;
#5874 = VECTOR ( 'NONE', #51324, 1000.000000000000000 ) ;
#5875 = CARTESIAN_POINT ( 'NONE',  ( 0.000000000000000000, 25.16329480281783759, -46.61112130868859538 ) ) ;
#5876 = ORIENTED_EDGE ( 'NONE', *, *, #27936, .F. ) ;
#5877 = FACE_OUTER_BOUND ( 'NONE', #76338, .T. ) ;
#5878 = LINE ( 'NONE', #37240, #47627 ) ;
#5879 = CARTESIAN_POINT ( 'NONE',  ( -90.61290675944017892, -60.00000000000000711, -17.71793535203029180 ) ) ;
#5880 = EDGE_LOOP ( 'NONE', ( #96406, #97052, #13928, #8893, #38450 ) ) ;
#5881 = DIRECTION ( 'NONE',  ( -1.000000000000000000, -1.224606353822377258E-16, -0.000000000000000000 ) ) ;
#5882 = DIRECTION ( 'NONE',  ( 0.000000000000000000, 0.000000000000000000, 1.000000000000000000 ) ) ;
#5884 = DIRECTION ( 'NONE',  ( 1.000000000000000000, 1.224606353822377258E-16, 0.000000000000000000 ) ) ;
#5883 = DIRECTION ( 'NONE',  ( 0.000000000000000000, -0.8047643452609457571, 0.5935944310694981629 ) ) ;
#5885 = CARTESIAN_POINT ( 'NONE',  ( -80.67482880870019812, -49.91654882987682385, 164.5101345921526104 ) ) ;
#5886 = ORIENTED_EDGE ( 'NONE', *, *, #47720, .F. ) ;
#5887 = CARTESIAN_POINT ( 'NONE',  ( -41.32194754023652195, 489.6440166213180873, 10.86036015010107114 ) ) ;
#5888 = VERTEX_POINT ( 'NONE', #96483 ) ;
#5889 = EDGE_LOOP ( 'NONE', ( #14627, #105460 ) ) ;
#5890 = CARTESIAN_POINT ( 'NONE',  ( 13.05035048251043150, -5.000000000000000000, -10.38464894538376448 ) ) ;
#5891 = LINE ( 'NONE', #38823, #58706 ) ;
#5892 = ORIENTED_EDGE ( 'NONE', *, *, #85049, .T. ) ;
#5893 = ADVANCED_FACE ( 'NONE', ( #31243 ), #58368, .T. ) ;
#5894 = VECTOR ( 'NONE', #102528, 1000.000000000000000 ) ;
#5895 = CARTESIAN_POINT ( 'NONE',  ( -34.87911814922733100, 490.1438948620115070, 11.96539694033642398 ) ) ;
#5896 = CARTESIAN_POINT ( 'NONE',  ( -10.00000000000000000, 15.00000000000000178, -3.648665620917535435 ) ) ;
#5897 = CARTESIAN_POINT ( 'NONE',  ( -91.62307993511501536, -57.61497437271354727, 204.2871689995596967 ) ) ;
#5898 = CARTESIAN_POINT ( 'NONE',  ( -9.924744359744972044, 294.6447758367797860, -1.393037881691840951 ) ) ;
#5899 = CARTESIAN_POINT ( 'NONE',  ( -58.13370862442636877, 48.00000000000000711, -29.53088244907756632 ) ) ;
#5900 = DIRECTION ( 'NONE',  ( -0.000000000000000000, 1.000000000000000000, 0.000000000000000000 ) ) ;
#5901 = CARTESIAN_POINT ( 'NONE',  ( 0.1682410636899299150, 27.29656849860388235, -40.74999999999998579 ) ) ;
#5902 = CARTESIAN_POINT ( 'NONE',  ( 84.06490631893382215, -29.99999999999999645, -21.85721834217820714 ) ) ;
#5903 = ADVANCED_FACE ( 'NONE', ( #7978 ), #87633, .T. ) ;
#5905 = EDGE_CURVE ( 'NONE', #101469, #59690, #41128, .T. ) ;
#5904 = CARTESIAN_POINT ( 'NONE',  ( -39.04695011312426800, -60.00000000000001421, 54.77420429098338417 ) ) ;
#5906 = CARTESIAN_POINT ( 'NONE',  ( -52.28272210538586506, -42.97553591916267379, 56.06210961058410192 ) ) ;
#5907 = ORIENTED_EDGE ( 'NONE', *, *, #61015, .F. ) ;
#5908 = CARTESIAN_POINT ( 'NONE',  ( 0.000000000000000000, 0.000000000000000000, -8.000000000000000000 ) ) ;
#5909 = VECTOR ( 'NONE', #33520, 1000.000000000000000 ) ;
#5910 = ORIENTED_EDGE ( 'NONE', *, *, #77334, .T. ) ;
#5911 = AXIS2_PLACEMENT_3D ( 'NONE', #38852, #41887, #96552 ) ;
#5912 = CARTESIAN_POINT ( 'NONE',  ( -103.5726650996749356, -60.16286882071497644, 191.7881775096330443 ) ) ;
#5913 = AXIS2_PLACEMENT_3D ( 'NONE', #36186, #69054, #60963 ) ;
#5914 = CARTESIAN_POINT ( 'NONE',  ( -30.74966693359947811, 13.13370859069518204, -41.50962874632944022 ) ) ;
#5915 = ORIENTED_EDGE ( 'NONE', *, *, #96902, .F. ) ;
#5916 = CARTESIAN_POINT ( 'NONE',  ( 19.45509070582273026, 49.98058642384193462, 60.57852761549106191 ) ) ;
#5917 = COLOUR_RGB ( '', 0.09019608, 0.27058824, 0.51372549) ;
#5918 = CARTESIAN_POINT ( 'NONE',  ( 87.17001200814932815, -38.36464134849014584, -20.67025014127871785 ) ) ;
#5919 = DIRECTION ( 'NONE',  ( 0.000000000000000000, 0.000000000000000000, -1.000000000000000000 ) ) ;
#5920 = CARTESIAN_POINT ( 'NONE',  ( -5.082755093536326818, -9.593750002048384573, 5.082755093536325042 ) ) ;
#5921 =( NAMED_UNIT ( * ) PLANE_ANGLE_UNIT ( ) SI_UNIT ( $, .RADIAN. ) );
#5922 = CARTESIAN_POINT ( 'NONE',  ( 43.51084452654469459, 465.2903130129626561, 9.421687747985401984 ) ) ;
#5923 = CARTESIAN_POINT ( 'NONE',  ( 62.38470394483648818, -29.99999999999999645, 73.04314485712862393 ) ) ;
#5924 = DIRECTION ( 'NONE',  ( 0.000000000000000000, -0.000000000000000000, -1.000000000000000000 ) ) ;
#5925 = CARTESIAN_POINT ( 'NONE',  ( -0.4140825127594466304, 34.19547899467610819, 29.68239057791232938 ) ) ;
#5926 = CARTESIAN_POINT ( 'NONE',  ( -38.23020704518376789, 485.0116943706008783, -3.938850139310159371 ) ) ;
#5927 = UNCERTAINTY_MEASURE_WITH_UNIT (LENGTH_MEASURE( 1.000000000000000082E-05 ), #83278, 'distance_accuracy_value', 'NONE');
#5928 = EDGE_CURVE ( 'NONE', #72570, #54633, #8385, .T. ) ;
#5929 = ORIENTED_EDGE ( 'NONE', *, *, #37624, .F. ) ;
#5930 = ORIENTED_EDGE ( 'NONE', *, *, #76250, .F. ) ;
#5931 = CARTESIAN_POINT ( 'NONE',  ( 50.78782189071710462, -39.51075776922833427, 52.07867872815624111 ) ) ;
#5932 = FACE_OUTER_BOUND ( 'NONE', #31424, .T. ) ;
#5933 = CARTESIAN_POINT ( 'NONE',  ( -6.984126283073809560, 16.97239697123576718, 0.5389771161762291207 ) ) ;
#5934 = CARTESIAN_POINT ( 'NONE',  ( -110.5479244313631710, -38.35611966620975011, 181.9352924883354206 ) ) ;
#5935 = VERTEX_POINT ( 'NONE', #88914 ) ;
#5936 = CARTESIAN_POINT ( 'NONE',  ( 91.21740072965818058, -38.35861323033353187, -0.9391089420829346057 ) ) ;
#5937 = CARTESIAN_POINT ( 'NONE',  ( 11.78141822354596790, 19.16435779204854839, -7.887621174215590614 ) ) ;
#5938 = CARTESIAN_POINT ( 'NONE',  ( -19.35841150692190737, 49.90777322328655430, 61.14767751163149967 ) ) ;
#5939 = SURFACE_STYLE_FILL_AREA ( #88478 ) ;
#5940 =( LENGTH_UNIT ( ) NAMED_UNIT ( * ) SI_UNIT ( .MILLI., .METRE. ) );
#5941 = CARTESIAN_POINT ( 'NONE',  ( -31.78065384406837524, 439.0075755211457249, 23.52222141353437834 ) ) ;
#5942 = CARTESIAN_POINT ( 'NONE',  ( 4.898587196589412829E-16, -25.81250000409677270, -8.000000000000000000 ) ) ;
#5943 = CARTESIAN_POINT ( 'NONE',  ( -36.71473571993598739, 414.8596714204733189, 6.147209701973896934 ) ) ;
#5944 = CARTESIAN_POINT ( 'NONE',  ( -1.469576158976823947E-15, -17.56250000409676915, 8.000000000000000000 ) ) ;
#5945 = SURFACE_SIDE_STYLE ('',( #56069 ) ) ;
#5946 = EDGE_CURVE ( 'NONE', #13798, #49621, #22627, .T. ) ;
#5947 = CARTESIAN_POINT ( 'NONE',  ( 95.21542849279514087, -60.00000000000001421, 202.5699345040212904 ) ) ;
#5948 = AXIS2_PLACEMENT_3D ( 'NONE', #72062, #96360, #251 ) ;
#5949 = CIRCLE ( 'NONE', #33545, 4.000000000000001776 ) ;
#5950 = FACE_OUTER_BOUND ( 'NONE', #18334, .T. ) ;
#5951 = ORIENTED_EDGE ( 'NONE', *, *, #52085, .F. ) ;
#5952 = CARTESIAN_POINT ( 'NONE',  ( 58.95658943640736993, -25.60101595818816023, 63.31392996776931170 ) ) ;
#5953 = CARTESIAN_POINT ( 'NONE',  ( -28.82563007256410970, 306.5180035891726789, -9.177916022869450074 ) ) ;
#5954 = CARTESIAN_POINT ( 'NONE',  ( 29.34999999999999787, 1.533819458162526451E-15, 0.000000000000000000 ) ) ;
#5955 =( GEOMETRIC_REPRESENTATION_CONTEXT ( 3 ) GLOBAL_UNCERTAINTY_ASSIGNED_CONTEXT ( ( #84472 ) ) GLOBAL_UNIT_ASSIGNED_CONTEXT ( ( #56380, #65560, #32693 ) ) REPRESENTATION_CONTEXT ( 'NONE', 'WORKASPACE' ) );
#5956 = VECTOR ( 'NONE', #51193, 1000.000000000000000 ) ;
#5957 =( NAMED_UNIT ( * ) PLANE_ANGLE_UNIT ( ) SI_UNIT ( $, .RADIAN. ) );
#5958 = EDGE_LOOP ( 'NONE', ( #32627, #79300 ) ) ;
#5960 = FACE_OUTER_BOUND ( 'NONE', #96945, .T. ) ;
#5959 = CARTESIAN_POINT ( 'NONE',  ( -91.27412109437786114, -38.35458256084967132, 28.31964854624011352 ) ) ;
#5961 = DIRECTION ( 'NONE',  ( 0.000000000000000000, 0.000000000000000000, 1.000000000000000000 ) ) ;
#5962 = CARTESIAN_POINT ( 'NONE',  ( 25.64256898552931929, 308.3509028655254838, 9.746403327101473835 ) ) ;
#5963 = CARTESIAN_POINT ( 'NONE',  ( -5.082755093536325042, -9.968750002048384573, -5.082755093536325930 ) ) ;
#5964 = CARTESIAN_POINT ( 'NONE',  ( 9.739726766100236688, -3.000000000000002665, -82.38252115499993522 ) ) ;
#5965 = CYLINDRICAL_SURFACE ( 'NONE', #20893, 3.400000000000000355 ) ;
#5966 = ORIENTED_EDGE ( 'NONE', *, *, #104867, .F. ) ;
#5967 = CARTESIAN_POINT ( 'NONE',  ( 84.52692572873411336, -32.42336717775761201, 173.3565263439695343 ) ) ;
#5968 = CARTESIAN_POINT ( 'NONE',  ( -44.22850192779651479, 464.1424782767533088, 8.760746036170912632 ) ) ;
#5969 = CARTESIAN_POINT ( 'NONE',  ( 37.33349330513379982, 1.593028355512270567E-15, 0.000000000000000000 ) ) ;
#5970 = VERTEX_POINT ( 'NONE', #73232 ) ;
#5971 = CARTESIAN_POINT ( 'NONE',  ( -24.51380645006441128, 303.7709942971744113, -9.801562582197524520 ) ) ;
#5972 = CARTESIAN_POINT ( 'NONE',  ( 7.543027128868171616, -4.999999999993999467, -20.22853049137519221 ) ) ;
#5973 = CARTESIAN_POINT ( 'NONE',  ( 0.000000000000000000, 0.000000000000000000, -5.575057142857143155 ) ) ;
#5974 = CARTESIAN_POINT ( 'NONE',  ( -11.99986829839305535, 50.00000000000000711, -83.40936345627086723 ) ) ;
#5975 = CARTESIAN_POINT ( 'NONE',  ( -34.54222097329575547, 42.66635145815377683, -63.01229731539426382 ) ) ;
#5976 = CARTESIAN_POINT ( 'NONE',  ( -29.09375146990846872, 9.378808818926360757, -41.96648843557836983 ) ) ;
#5977 = ORIENTED_EDGE ( 'NONE', *, *, #97486, .T. ) ;
#5978 = EDGE_CURVE ( 'NONE', #100365, #96318, #27697, .T. ) ;
#5979 = VECTOR ( 'NONE', #5815, 1000.000000000000000 ) ;
#5980 = CARTESIAN_POINT ( 'NONE',  ( -81.34045205995600725, -30.00000000000000711, -10.45056096668239043 ) ) ;
#5981 = CARTESIAN_POINT ( 'NONE',  ( 37.88408281519146925, 25.64317620387171814, 10.98673829482864406 ) ) ;
#5982 = CARTESIAN_POINT ( 'NONE',  ( 0.000000000000000000, 3.999999999999996447, 12.00000000000003908 ) ) ;
#5983 = EDGE_CURVE ( 'NONE', #73940, #78785, #11847, .T. ) ;
#5985 = CARTESIAN_POINT ( 'NONE',  ( -10.65671340344253615, 14.86024801717850075, -9.830563606247649133 ) ) ;
#5984 = CARTESIAN_POINT ( 'NONE',  ( -1.246384481104801489, -18.05976919417167537, 35.00911013355869272 ) ) ;
#5986 = EDGE_CURVE ( 'NONE', #87241, #14833, #56574, .T. ) ;
#5987 =( GEOMETRIC_REPRESENTATION_CONTEXT ( 3 ) GLOBAL_UNCERTAINTY_ASSIGNED_CONTEXT ( ( #27201 ) ) GLOBAL_UNIT_ASSIGNED_CONTEXT ( ( #35919, #19737, #28344 ) ) REPRESENTATION_CONTEXT ( 'NONE', 'WORKASPACE' ) );
#5988 = CARTESIAN_POINT ( 'NONE',  ( 7.188101187500001821, -20.56250000204838457, -2.977408999572650483 ) ) ;
#5989 = UNCERTAINTY_MEASURE_WITH_UNIT (LENGTH_MEASURE( 1.000000000000000082E-05 ), #90708, 'distance_accuracy_value', 'NONE');
#5990 = CARTESIAN_POINT ( 'NONE',  ( -28.65204159835574771, 18.70303032895464668, -40.14586416981832429 ) ) ;
#5991 = CONICAL_SURFACE ( 'NONE', #14602, 4.000000000000001776, 0.9599310885968774798 ) ;
#5992 = AXIS2_PLACEMENT_3D ( 'NONE', #9461, #65057, #34324 ) ;
#5993 = DIRECTION ( 'NONE',  ( -1.000000000000000000, -1.224606353822377258E-16, -0.000000000000000000 ) ) ;
#5994 = ORIENTED_EDGE ( 'NONE', *, *, #73101, .T. ) ;
#5995 = EDGE_CURVE ( 'NONE', #17876, #38472, #81855, .T. ) ;
#5996 = EDGE_CURVE ( 'NONE', #70259, #65781, #68709, .T. ) ;
#5997 = CARTESIAN_POINT ( 'NONE',  ( 7.500000000000000000, -1.645076096009009836, -7.030022527230193496 ) ) ;
#5998 = AXIS2_PLACEMENT_3D ( 'NONE', #26334, #58106, #75892 ) ;
#5999 = CARTESIAN_POINT ( 'NONE',  ( -7.856068184142580790, 67.85260481710604097, -5.000000000005080381 ) ) ;
#6000 = SURFACE_STYLE_USAGE ( .BOTH. , #14084 ) ;
#6001 = CARTESIAN_POINT ( 'NONE',  ( 20.00000000000000000, 12.99999999999999289, 7.500000000000000000 ) ) ;
#6002 = ORIENTED_EDGE ( 'NONE', *, *, #11672, .F. ) ;
#6003 = FILL_AREA_STYLE ('',( #97658 ) ) ;
#6004 = DIRECTION ( 'NONE',  ( 0.000000000000000000, -1.000000000000000000, 0.000000000000000000 ) ) ;
#6005 = ORIENTED_EDGE ( 'NONE', *, *, #23686, .T. ) ;
#6006 = DIRECTION ( 'NONE',  ( 0.000000000000000000, -1.000000000000000000, 0.000000000000000000 ) ) ;
#6007 = LINE ( 'NONE', #14093, #97586 ) ;
#6008 = SURFACE_SIDE_STYLE ('',( #38418 ) ) ;
#6009 = UNCERTAINTY_MEASURE_WITH_UNIT (LENGTH_MEASURE( 1.000000000000000082E-05 ), #86345, 'distance_accuracy_value', 'NONE');
#6010 = CARTESIAN_POINT ( 'NONE',  ( -110.2852303711805746, -60.00000000000000000, 145.7623735510408665 ) ) ;
#6011 = FILL_AREA_STYLE ('',( #47003 ) ) ;
#6012 = DIRECTION ( 'NONE',  ( 0.000000000000000000, 0.000000000000000000, 1.000000000000000000 ) ) ;
#6013 = CARTESIAN_POINT ( 'NONE',  ( 6.534102926715305237, 53.62242791884023063, -7.078184780914639873 ) ) ;
#6014 = CARTESIAN_POINT ( 'NONE',  ( 0.000000000000000000, -5.000000000000002665, -73.00000000000001421 ) ) ;
#6015 = CARTESIAN_POINT ( 'NONE',  ( -85.88231755690129887, -21.77401794985988204, 171.2094949271552764 ) ) ;
#6016 = ORIENTED_EDGE ( 'NONE', *, *, #23113, .T. ) ;
#6017 = CARTESIAN_POINT ( 'NONE',  ( 32.93128443270173022, 42.88088526003227940, -65.22696890650703949 ) ) ;
#6018 = CIRCLE ( 'NONE', #26722, 8.000000000000000000 ) ;
#6019 = ORIENTED_EDGE ( 'NONE', *, *, #95117, .T. ) ;
#6020 = CARTESIAN_POINT ( 'NONE',  ( -0.01402285133662556187, -30.00000000000000000, -39.99999948934169680 ) ) ;
#6021 = CARTESIAN_POINT ( 'NONE',  ( 4.472135954999578722, -65.27077220067361907, 4.000000000000002665 ) ) ;
#6022 = PRODUCT_DEFINITION_FORMATION_WITH_SPECIFIED_SOURCE ( 'ANY', '', #94105, .NOT_KNOWN. ) ;
#6023 = CARTESIAN_POINT ( 'NONE',  ( -86.14801153885079543, -60.13788232086688623, 9.933174785324942135 ) ) ;
#6024 = CARTESIAN_POINT ( 'NONE',  ( -11.59898333071130772, 303.6009974801674502, 9.883690217586748261 ) ) ;
#6025 = CARTESIAN_POINT ( 'NONE',  ( -16.14595037866548566, 6.775806037742684751, -6.185188124845088176 ) ) ;
#6026 = CARTESIAN_POINT ( 'NONE',  ( 8.167412539197350441, 39.27912669871957263, 1.228248305376115968E-12 ) ) ;
#6027 = LINE ( 'NONE', #78331, #28760 ) ;
#6028 = DIRECTION ( 'NONE',  ( -1.000000000000000000, -1.224606353822377258E-16, -0.000000000000000000 ) ) ;
#6029 = CARTESIAN_POINT ( 'NONE',  ( 77.72372478688149045, -60.00000000000015632, 197.5639835283903381 ) ) ;
#6030 = EDGE_CURVE ( 'NONE', #30663, #30305, #6921, .T. ) ;
#6031 = CARTESIAN_POINT ( 'NONE',  ( -101.8002770060248139, -59.99999999999998579, 77.51242708015574578 ) ) ;
#6032 = CARTESIAN_POINT ( 'NONE',  ( -64.03467178915637703, -49.91529051540093320, 88.80954775168983417 ) ) ;
#6033 = VERTEX_POINT ( 'NONE', #23673 ) ;
#6034 = CARTESIAN_POINT ( 'NONE',  ( 2.972029323994034744, 39.42457582143072159, 64.99968642937007246 ) ) ;
#6035 = CARTESIAN_POINT ( 'NONE',  ( 62.33054962693324086, -60.00000000003888800, 116.7585282323999110 ) ) ;
#6036 = VERTEX_POINT ( 'NONE', #64638 ) ;
#6037 = CARTESIAN_POINT ( 'NONE',  ( 1.987573926653205314, -25.54829021846704862, 28.14551609985228708 ) ) ;
#6038 = CARTESIAN_POINT ( 'NONE',  ( 2.977408999572652260, -18.31250000204838457, 7.188101187500000044 ) ) ;
#6039 = CARTESIAN_POINT ( 'NONE',  ( 32.90753060622966331, 485.1134061474841701, 5.490696813887106842 ) ) ;
#6040 = ORIENTED_EDGE ( 'NONE', *, *, #42643, .F. ) ;
#6041 = CARTESIAN_POINT ( 'NONE',  ( 3.351411280263732362, -49.00492482622130552, 104.3292055665660456 ) ) ;
#6042 = EDGE_LOOP ( 'NONE', ( #12347, #26136, #28707, #104471 ) ) ;
#6043 = CARTESIAN_POINT ( 'NONE',  ( 11.07117956952415483, 45.30041971330287964, -15.14528042430110766 ) ) ;
#6044 = VECTOR ( 'NONE', #66090, 1000.000000000000000 ) ;
#6045 = CARTESIAN_POINT ( 'NONE',  ( -7.188101187500002709, -29.18750000204839523, 2.977408999572647819 ) ) ;
#6046 = CARTESIAN_POINT ( 'NONE',  ( -92.96207233507917067, -60.00000000000000000, 202.4679484878635378 ) ) ;
#6047 = CARTESIAN_POINT ( 'NONE',  ( 36.64739769383395185, 372.7567539989593115, 4.301078365670656822 ) ) ;
#6048 = CARTESIAN_POINT ( 'NONE',  ( -5.082755093536326818, -27.59375000204838813, 5.082755093536325042 ) ) ;
#6049 = DIRECTION ( 'NONE',  ( -1.000000000000000000, 0.000000000000000000, 0.000000000000000000 ) ) ;
#6050 = CARTESIAN_POINT ( 'NONE',  ( -11.42046787539988983, 14.07301214197669736, 9.944540719455840616 ) ) ;
#6051 = FILL_AREA_STYLE ('',( #14139 ) ) ;
#6052 = CARTESIAN_POINT ( 'NONE',  ( 1.224646799147352665E-15, 48.00000000000000000, -75.00000000000001421 ) ) ;
#6053 = CARTESIAN_POINT ( 'NONE',  ( -7.151217271224854954, 106.7874940044571872, -3.587901469523285591 ) ) ;
#6054 = CARTESIAN_POINT ( 'NONE',  ( -39.23477672781254455, 311.7615262522152761, 2.036766034490009147 ) ) ;
#6055 = CONICAL_SURFACE ( 'NONE', #23338, 3.309500000000001663, 0.9599310885968770357 ) ;
#6056 = CARTESIAN_POINT ( 'NONE',  ( 105.0433157361263596, -60.00000000000000711, 187.5698151985990307 ) ) ;
#6057 = CARTESIAN_POINT ( 'NONE',  ( -37.74004406342657347, -32.59350783026462750, 35.55426695422483618 ) ) ;
#6058 = ORIENTED_EDGE ( 'NONE', *, *, #93557, .T. ) ;
#6059 = CARTESIAN_POINT ( 'NONE',  ( -36.24373624681329176, 462.2822415611975657, 3.475315787151807001 ) ) ;
#6060 = CARTESIAN_POINT ( 'NONE',  ( 34.08083780335558544, -29.09990395782033801, 32.84435087873961834 ) ) ;
#6061 = AXIS2_PLACEMENT_3D ( 'NONE', #65117, #39796, #49454 ) ;
#6062 = CARTESIAN_POINT ( 'NONE',  ( -5.820808985953483727, -9.668376379147026354E-13, -21.65942590380073085 ) ) ;
#6063 = ORIENTED_EDGE ( 'NONE', *, *, #88792, .T. ) ;
#6064 = FACE_OUTER_BOUND ( 'NONE', #23128, .T. ) ;
#6065 = B_SPLINE_CURVE_WITH_KNOTS ( 'NONE', 3,
 ( #46980, #63727, #5472, #38395, #71260, #104154, #63188, #22213, #5984, #55063, #14071, #87993, #47509, #80401, #64255, #41547, #57184, #65824, #106263, #512, #66899, #82539, #8108, #65295, #16206, #25952, #98186, #58812, #90100, #49088, #98703, #81990, #83588, #33477, #73903, #24858, #66350, #41022, #31884, #74433, #42606, #9696, #25403, #99235, #1051, #58263, #23810, #55895, #91187, #16743, #91705, #99783, #74959, #57708, #17822, #105748, #50673, #49633, #17294, #64768, #97643, #42076, #90635, #56655, #81454, #89580, #8643, #7568, #50168, #15673, #83071, #48563, #34026, #40485, #73364, #9162, #24341, #32425, #32954, #76560, #68498, #92206, #76034, #59882, #100309, #59342, #92755, #75504, #67954, #94367, #2130, #2671, #85198, #18912, #20530, #60938, #51214, #27001, #43151, #53367, #85754, #18363, #93828, #35084, #36164, #51757, #34560, #52826, #69556, #101907, #84671, #12359, #19981, #60419, #10755, #93297, #86287, #84140, #43672, #26471, #11827, #100837, #11283, #1598 ),
 .UNSPECIFIED., .F., .F.,
 ( 4, 2, 2, 2, 1, 2, 2, 2, 2, 1, 2, 2, 1, 2, 2, 1, 1, 2, 2, 1, 2, 2, 1, 1, 2, 2, 1, 2, 2, 1, 2, 2, 2, 2, 2, 2, 1, 1, 2, 2, 2, 2, 2, 2, 2, 1, 1, 1, 2, 2, 1, 1, 2, 2, 1, 2, 2, 1, 1, 1, 2, 2, 2, 1, 1, 2, 2, 2, 2, 1, 2, 2, 2, 4 ),
 ( 0.4962367771140062667, 0.4972206896587050839, 0.4982046022034038457, 0.5001724272928014248, 0.5041080774715966939, 0.5119793778291871211, 0.5277219785443679756, 0.5296898036337656102, 0.5316576287231631337, 0.5355932789019584028, 0.5434645792595488301, 0.5592071799747297955, 0.5611750050641273191, 0.5621589176088261919, 0.5626508738811756283, 0.5631428301535250647, 0.5670784803323204448, 0.5749497806899113161, 0.5906923814050930588, 0.5926602064944908044, 0.5936441190391896772, 0.5941360753115390025, 0.5946280315838885500, 0.5985636817626840411, 0.6064349821202751345, 0.6221775828354573212, 0.6241454079248550668, 0.6246373641972045032, 0.6251293204695539396, 0.6261132330142528124, 0.6300488831930485256, 0.6379201835506397300, 0.6536627842658222498, 0.6851479856961874004, 0.6871158107855852570, 0.6876077670579346934, 0.6880997233302842409, 0.6890836358749831136, 0.6930192860537787158, 0.7008905864113700313, 0.7166331871265524400, 0.7205688373053480422, 0.7245044874841436444, 0.7323757878417348488, 0.7481183885569173686, 0.7491023011016164634, 0.7495942573739660109, 0.7498402355101407846, 0.7499632245782281714, 0.7500862136463155583, 0.7520540387357136369, 0.7559896889145101273, 0.7638609892721028860, 0.7796035899872886255, 0.7805875025319877203, 0.7810794588043372677, 0.7813254369405121524, 0.7815714150766870372, 0.7835392401660863371, 0.7874748903448847148, 0.7953461907024816924, 0.8110887914176753144, 0.8130566165070745033, 0.8150244415964736922, 0.8189600917752720699, 0.8268313921328689364, 0.8425739928480624474, 0.8740591942784496915, 0.8779948444572482913, 0.8819304946360466690, 0.8898017949936435356, 0.9055443957088372686, 0.9370295971392248457, 1.000000000000000000 ),
 .UNSPECIFIED. ) ;
#6066 = CARTESIAN_POINT ( 'NONE',  ( -67.90781492711421663, -38.33416998424474542, 125.1147017743826382 ) ) ;
#6067 = AXIS2_PLACEMENT_3D ( 'NONE', #70108, #87365, #5883 ) ;
#6068 = VERTEX_POINT ( 'NONE', #106676 ) ;
#6070 = CARTESIAN_POINT ( 'NONE',  ( -29.45362385905110969, 325.9253963054578662, 15.14270878922920716 ) ) ;
#6069 = CARTESIAN_POINT ( 'NONE',  ( 6.499999999999999112, -3.752776749732586126, -6.064240316920402663 ) ) ;
#6071 = CARTESIAN_POINT ( 'NONE',  ( 15.90885615318885016, 37.20836610827222302, 22.13023378396293239 ) ) ;
#6072 = CARTESIAN_POINT ( 'NONE',  ( 6.281175601187043434, -3.752776749732576356, -6.500000000000000000 ) ) ;
#6073 = AXIS2_PLACEMENT_3D ( 'NONE', #16419, #38599, #14285 ) ;
#6074 = AXIS2_PLACEMENT_3D ( 'NONE', #39483, #32992, #6548 ) ;
#6075 = CYLINDRICAL_SURFACE ( 'NONE', #106139, 4.000000000000000000 ) ;
#6076 = CARTESIAN_POINT ( 'NONE',  ( -42.11386565846122210, 436.0925768526294632, 7.550517934405435838 ) ) ;
#6077 = VECTOR ( 'NONE', #95314, 1000.000000000000000 ) ;
#6079 = ADVANCED_FACE ( 'NONE', ( #65702 ), #75393, .F. ) ;
#6078 = DIRECTION ( 'NONE',  ( -1.000000000000000000, -0.000000000000000000, -0.000000000000000000 ) ) ;
#6080 = DIRECTION ( 'NONE',  ( -1.000000000000000000, -0.000000000000000000, -0.000000000000000000 ) ) ;
#6081 = ADVANCED_FACE ( 'NONE', ( #2012 ), #8512, .T. ) ;
#6082 = CARTESIAN_POINT ( 'NONE',  ( 97.90254053569493919, -60.00000000000000711, 68.32195872189682007 ) ) ;
#6083 = CONICAL_SURFACE ( 'NONE', #71518, 4.172000000000001485, 0.9599310885968750373 ) ;
#6084 = CARTESIAN_POINT ( 'NONE',  ( 0.4042117618284671865, -3.141900367810038119, 6.500000000000000888 ) ) ;
#6085 = AXIS2_PLACEMENT_3D ( 'NONE', #49084, #106258, #48022 ) ;
#6086 =( BOUNDED_SURFACE ( )  B_SPLINE_SURFACE ( 3, 2, ( 
 ( #79839, #54483, #87429 ),
 ( #78774, #53459, #28686 ),
 ( #104112, #37839, #30800 ),
 ( #78255, #12972, #95503 ) ),
 .UNSPECIFIED., .F., .F., .F. ) 
 B_SPLINE_SURFACE_WITH_KNOTS ( ( 4, 4 ),
 ( 3, 3 ),
 ( 7.329206686002009974E-17, 0.002404295360991625784 ),
 ( 0.000000000000000000, 1.000000000000000000 ),
 .UNSPECIFIED. ) 
 GEOMETRIC_REPRESENTATION_ITEM ( )  RATIONAL_B_SPLINE_SURFACE ( (
 ( 1.000000000000000000, 0.8162384603570761454, 1.000000000000000000),
 ( 1.000000000000000000, 0.8104306387031265935, 1.000000000000000000),
 ( 1.000000000000000000, 0.8018372346786888372, 1.000000000000000000),
 ( 1.000000000000000000, 0.7927020107002136218, 1.000000000000000000) ) ) 
 REPRESENTATION_ITEM ( '' )  SURFACE ( )  );
#6087 = DIRECTION ( 'NONE',  ( -1.000000000000000000, -1.224606353822377258E-16, -0.000000000000000000 ) ) ;
#6088 = DIRECTION ( 'NONE',  ( 0.000000000000000000, 0.000000000000000000, 1.000000000000000000 ) ) ;
#6089 = EDGE_LOOP ( 'NONE', ( #106095, #92588, #104698, #22490, #35574 ) ) ;
#6090 = CARTESIAN_POINT ( 'NONE',  ( -86.86330325217545578, -30.00000000000164846, -18.79756195431963661 ) ) ;
#6091 = ORIENTED_EDGE ( 'NONE', *, *, #47129, .T. ) ;
#6092 = DIRECTION ( 'NONE',  ( -1.000000000000000000, -0.000000000000000000, -0.000000000000000000 ) ) ;
#6093 = DIRECTION ( 'NONE',  ( 0.000000000000000000, 0.000000000000000000, -1.000000000000000000 ) ) ;
#6094 = CARTESIAN_POINT ( 'NONE',  ( 82.62819499073798113, -45.27882038833382694, -15.10946084058340411 ) ) ;
#6095 = CARTESIAN_POINT ( 'NONE',  ( -5.082755093536326818, -23.09375000204838457, 5.082755093536325042 ) ) ;
#6096 = DIRECTION ( 'NONE',  ( -1.000000000000000000, -0.000000000000000000, -0.000000000000000000 ) ) ;
#6097 = EDGE_LOOP ( 'NONE', ( #48390, #1585, #34799, #105861, #73605, #45556 ) ) ;
#6099 = ORIENTED_EDGE ( 'NONE', *, *, #19298, .T. ) ;
#6098 = DIRECTION ( 'NONE',  ( 1.000000000000000000, 1.224606353822377258E-16, 0.000000000000000000 ) ) ;
#6100 = CARTESIAN_POINT ( 'NONE',  ( 81.05849975536304441, -32.56051081393310653, 144.8530755112767565 ) ) ;
#6101 = SURFACE_STYLE_USAGE ( .BOTH. , #47090 ) ;
#6102 = VERTEX_POINT ( 'NONE', #17690 ) ;
#6103 = CARTESIAN_POINT ( 'NONE',  ( -12.49999999999999645, 22.75697755191607641, -40.20656553242739051 ) ) ;
#6104 = CARTESIAN_POINT ( 'NONE',  ( 0.000000000000000000, 0.000000000000000000, 0.000000000000000000 ) ) ;
#6105 = CARTESIAN_POINT ( 'NONE',  ( -7.188101187500000933, -15.50000000204838635, -2.977408999572651371 ) ) ;
#6106 = CIRCLE ( 'NONE', #52606, 6.000000000000001776 ) ;
#6107 = CARTESIAN_POINT ( 'NONE',  ( -15.40724846713353813, -57.67135988443339301, 41.78154393163084279 ) ) ;
#6108 = CARTESIAN_POINT ( 'NONE',  ( 8.413831435758774902, 294.6898084274850476, 9.902566404003444234 ) ) ;
#6109 = ORIENTED_EDGE ( 'NONE', *, *, #70359, .T. ) ;
#6110 =( NAMED_UNIT ( * ) PLANE_ANGLE_UNIT ( ) SI_UNIT ( $, .RADIAN. ) );
#6111 = FILL_AREA_STYLE_COLOUR ( '', #26962 ) ;
#6112 = DIRECTION ( 'NONE',  ( -0.000000000000000000, -1.000000000000000000, -0.000000000000000000 ) ) ;
#6113 = CARTESIAN_POINT ( 'NONE',  ( -9.482945380845297478, 82.55666941221069521, 3.177595346755244243 ) ) ;
#6114 = FILL_AREA_STYLE_COLOUR ( '', #53388 ) ;
#6115 = EDGE_LOOP ( 'NONE', ( #75169, #104271, #43693, #51600 ) ) ;
#6116 = CARTESIAN_POINT ( 'NONE',  ( 7.999999999999998224, -11.28125000409677092, 3.313708498984766493 ) ) ;
#6117 = CARTESIAN_POINT ( 'NONE',  ( -28.27173859142850176, -20.85003346561162374, 31.88408023871041408 ) ) ;
#6118 = CARTESIAN_POINT ( 'NONE',  ( -36.47968809679790780, 26.06923311369085638, 11.58333936845124690 ) ) ;
#6119 = CARTESIAN_POINT ( 'NONE',  ( -1.000000000000000000, -56.57158839598558586, 6.200363299246187232 ) ) ;
#6120 = CARTESIAN_POINT ( 'NONE',  ( 7.500000000000007105, 40.95611321456068055, -60.73832539154659571 ) ) ;
#6121 = CARTESIAN_POINT ( 'NONE',  ( 4.898587196589412829E-16, -19.62499999999999289, -8.000000000000000000 ) ) ;
#6122 = AXIS2_PLACEMENT_3D ( 'NONE', #78826, #64775, #46473 ) ;
#6123 = APPLICATION_PROTOCOL_DEFINITION ( 'draft international standard', 'automotive_design', 1998, #6631 ) ;
#6124 = CARTESIAN_POINT ( 'NONE',  ( 38.64291280000707474, 27.44880098965157345, 11.54947501064066806 ) ) ;
#6125 = ORIENTED_EDGE ( 'NONE', *, *, #10434, .T. ) ;
#6126 = CARTESIAN_POINT ( 'NONE',  ( -5.000000000000000888, -46.00000000000000000, 42.58845726811989607 ) ) ;
#6127 = ADVANCED_FACE ( 'NONE', ( #99653 ), #104874, .T. ) ;
#6128 = DIRECTION ( 'NONE',  ( -0.000000000000000000, -1.000000000000000000, -0.000000000000000000 ) ) ;
#6129 = CARTESIAN_POINT ( 'NONE',  ( -46.00000000000000000, 461.7884530655983326, 10.79543072756972677 ) ) ;
#6130 = CARTESIAN_POINT ( 'NONE',  ( -62.79708356444599104, -30.00000000000000000, 74.14398739475227273 ) ) ;
#6131 = ADVANCED_FACE ( 'NONE', ( #41415 ), #74831, .F. ) ;
#6132 = CARTESIAN_POINT ( 'NONE',  ( 5.500000000000007994, 42.00000000000000000, -72.67206406577979294 ) ) ;
#6133 = ORIENTED_EDGE ( 'NONE', *, *, #10812, .T. ) ;
#6134 = CARTESIAN_POINT ( 'NONE',  ( 0.000000000000000000, 1.502314598737159031E-15, -8.000000000000000000 ) ) ;
#6135 = CONICAL_SURFACE ( 'NONE', #54386, 6.500000000000000888, 0.8987552595851637793 ) ;
#6136 = CARTESIAN_POINT ( 'NONE',  ( 104.5422953853447581, -57.64203673969820585, 202.0104448647194602 ) ) ;
#6137 = AXIS2_PLACEMENT_3D ( 'NONE', #88202, #14284, #72007 ) ;
#6138 = CARTESIAN_POINT ( 'NONE',  ( 67.74083062384904963, -34.58965796570005580, -22.72020771579463272 ) ) ;
#6139 = DIRECTION ( 'NONE',  ( -1.000000000000000000, -1.224606353822377258E-16, -0.000000000000000000 ) ) ;
#6140 = CARTESIAN_POINT ( 'NONE',  ( -14.89114929831680811, 23.12273819885389869, 0.2580741681018605682 ) ) ;
#6141 = DIRECTION ( 'NONE',  ( -0.000000000000000000, -1.000000000000000000, -0.000000000000000000 ) ) ;
#6142 = CARTESIAN_POINT ( 'NONE',  ( -73.13094403033801427, -59.99999999999999289, 163.6547797536228472 ) ) ;
#6143 = VECTOR ( 'NONE', #26634, 1000.000000000000000 ) ;
#6144 = CARTESIAN_POINT ( 'NONE',  ( 19.34999999999999787, 1.533819458162526451E-15, 0.000000000000000000 ) ) ;
#6145 = CARTESIAN_POINT ( 'NONE',  ( 58.90678327788049273, 50.00000000002003731, -28.11551192221532247 ) ) ;
#6146 = CARTESIAN_POINT ( 'NONE',  ( -85.38396510212227497, -46.56038326034761354, 188.3815645333082216 ) ) ;
#6147 = ORIENTED_EDGE ( 'NONE', *, *, #103336, .F. ) ;
#6148 = CARTESIAN_POINT ( 'NONE',  ( 36.73963609038971612, 391.1744242912104141, 5.928860386883613387 ) ) ;
#6149 = CIRCLE ( 'NONE', #71596, 15.00000000000001421 ) ;
#6150 = ORIENTED_EDGE ( 'NONE', *, *, #13817, .F. ) ;
#6151 = CARTESIAN_POINT ( 'NONE',  ( -7.896165657598944065, -13.78911131371973653, -1.307894402814546719 ) ) ;
#6152 = CARTESIAN_POINT ( 'NONE',  ( -25.14694300620596579, 305.1179679012358292, -9.724845900475482807 ) ) ;
#6153 = CARTESIAN_POINT ( 'NONE',  ( -84.90132116126285666, -60.19215146778790881, -16.22236961991315596 ) ) ;
#6154 = DIRECTION ( 'NONE',  ( -1.000000000000000000, -1.224606353822377258E-16, -0.000000000000000000 ) ) ;
#6155 = CARTESIAN_POINT ( 'NONE',  ( -43.48483803624229438, 478.3762783859466481, 6.210097532620542538 ) ) ;
#6156 = ORIENTED_EDGE ( 'NONE', *, *, #5476, .F. ) ;
#6157 = SURFACE_SIDE_STYLE ('',( #62308 ) ) ;
#6158 = CARTESIAN_POINT ( 'NONE',  ( 12.52134978615753624, 5.248113740467461596, 8.137638698453219632 ) ) ;
#6159 = CARTESIAN_POINT ( 'NONE',  ( 72.37206225042174879, 4.898587196589294500E-16, -4.000000000000007105 ) ) ;
#6160 = CARTESIAN_POINT ( 'NONE',  ( 9.349999999999997868, -3.309499999999999886, 0.000000000000000000 ) ) ;
#6161 = EDGE_CURVE ( 'NONE', #99731, #3333, #29095, .T. ) ;
#6162 = CARTESIAN_POINT ( 'NONE',  ( 76.02438791174152755, -14.21045842199433729, -24.18563911012876844 ) ) ;
#6163 = CARTESIAN_POINT ( 'NONE',  ( -80.73742772600893147, -29.09286051066668577, 139.3498210207160639 ) ) ;
#6164 = VERTEX_POINT ( 'NONE', #58130 ) ;
#6165 = CARTESIAN_POINT ( 'NONE',  ( 8.180516222381777780, -14.21045842199445630, 34.35482301558341334 ) ) ;
#6166 = DIRECTION ( 'NONE',  ( -1.000000000000000000, 0.000000000000000000, 0.000000000000000000 ) ) ;
#6167 = CARTESIAN_POINT ( 'NONE',  ( 76.35456037190438394, -57.53670657966636526, 193.9177342501030807 ) ) ;
#6168 = FILL_AREA_STYLE ('',( #54181 ) ) ;
#6169 = CARTESIAN_POINT ( 'NONE',  ( 40.95117681093327633, 312.9070568743562717, -5.696314580190224852 ) ) ;
#6170 = FACE_OUTER_BOUND ( 'NONE', #17710, .T. ) ;
#6171 = VERTEX_POINT ( 'NONE', #27415 ) ;
#6172 = DIRECTION ( 'NONE',  ( 0.000000000000000000, 0.000000000000000000, 1.000000000000000000 ) ) ;
#6173 = SURFACE_STYLE_USAGE ( .BOTH. , #87654 ) ;
#6175 = CARTESIAN_POINT ( 'NONE',  ( -105.6705936910478698, -60.15501511360662334, 156.3715117094907612 ) ) ;
#6174 = CARTESIAN_POINT ( 'NONE',  ( -15.73298926836856992, 37.19132885152136936, 22.31337215277960695 ) ) ;
#6176 = CARTESIAN_POINT ( 'NONE',  ( -7.188101187500001821, -20.00000000204838813, -2.977408999572651371 ) ) ;
#6177 = CARTESIAN_POINT ( 'NONE',  ( 8.000000000000000000, -20.18750000409677270, 0.000000000000000000 ) ) ;
#6178 = CIRCLE ( 'NONE', #18228, 4.999999999999999112 ) ;
#6179 = DIRECTION ( 'NONE',  ( 0.000000000000000000, 0.000000000000000000, -1.000000000000000000 ) ) ;
#6180 = CARTESIAN_POINT ( 'NONE',  ( 0.3382058652630261508, 35.06838561256219577, 27.28521124779242157 ) ) ;
#6181 = EDGE_CURVE ( 'NONE', #15530, #17909, #67827, .T. ) ;
#6182 = CARTESIAN_POINT ( 'NONE',  ( 26.49278565071599445, 36.83346926003848409, 9.908164042044147024 ) ) ;
#6183 = CARTESIAN_POINT ( 'NONE',  ( 36.08349330513379982, 1.593028355512270962E-15, 0.000000000000000000 ) ) ;
#6184 = ORIENTED_EDGE ( 'NONE', *, *, #42121, .F. ) ;
#6185 = FACE_OUTER_BOUND ( 'NONE', #66952, .T. ) ;
#6187 = CARTESIAN_POINT ( 'NONE',  ( 25.87815429224528785, -18.61428468264773528, 28.34824171517409752 ) ) ;
#6186 = CARTESIAN_POINT ( 'NONE',  ( -16.61716630718971643, -29.99999999999995026, 37.21284229651715947 ) ) ;
#6188 = CARTESIAN_POINT ( 'NONE',  ( -4.650164881889539359, 52.18144192692520278, -6.194387419916259852 ) ) ;
#6189 = EDGE_LOOP ( 'NONE', ( #47432, #36007, #92113, #39203 ) ) ;
#6190 = UNCERTAINTY_MEASURE_WITH_UNIT (LENGTH_MEASURE( 1.000000000000000082E-05 ), #101582, 'distance_accuracy_value', 'NONE');
#6191 = ORIENTED_EDGE ( 'NONE', *, *, #68616, .F. ) ;
#6192 = CARTESIAN_POINT ( 'NONE',  ( -0.3347025688926246745, 43.19007807389648690, -18.70729546860571446 ) ) ;
#6193 = CARTESIAN_POINT ( 'NONE',  ( 26.08349330513380693, 1.593028355512270962E-15, 0.000000000000000000 ) ) ;
#6194 = CARTESIAN_POINT ( 'NONE',  ( -43.72734063489070877, 464.0947689350268774, 7.873621169220604621 ) ) ;
#6195 = DIRECTION ( 'NONE',  ( 0.000000000000000000, 0.000000000000000000, -1.000000000000000000 ) ) ;
#6196 = EDGE_LOOP ( 'NONE', ( #92985, #66074, #93610, #77410, #27761 ) ) ;
#6197 = ADVANCED_FACE ( 'NONE', ( #59749 ), #63618, .T. ) ;
#6198 = CARTESIAN_POINT ( 'NONE',  ( 14.21314216640385908, -60.00000000000000711, -42.20886373635748612 ) ) ;
#6199 = AXIS2_PLACEMENT_3D ( 'NONE', #59354, #61486, #84149 ) ;
#6200 = CARTESIAN_POINT ( 'NONE',  ( 22.10772461237692355, 26.03542649978865953, -31.35794278042768113 ) ) ;
#6201 = DIRECTION ( 'NONE',  ( -1.000000000000000000, -1.224606353822377258E-16, -0.000000000000000000 ) ) ;
#6202 = CARTESIAN_POINT ( 'NONE',  ( -1.590636543681222870, -4.999999999999999112, -97.00013170161253129 ) ) ;
#6203 = EDGE_CURVE ( 'NONE', #59582, #48784, #1595, .T. ) ;
#6204 = CARTESIAN_POINT ( 'NONE',  ( 6.500000000000000000, -0.6456425506958757277, 3.147574431996980060E-15 ) ) ;
#6205 = VERTEX_POINT ( 'NONE', #2548 ) ;
#6206 = ORIENTED_EDGE ( 'NONE', *, *, #12314, .F. ) ;
#6207 = ORIENTED_EDGE ( 'NONE', *, *, #48723, .F. ) ;
#6208 = CARTESIAN_POINT ( 'NONE',  ( 0.6406553905574651209, 54.23511180506763196, 7.923516270499307623 ) ) ;
#6209 = PLANE ( 'NONE',  #26981 ) ;
#6210 = CARTESIAN_POINT ( 'NONE',  ( 31.84110979627772409, 331.2976162219903244, 16.86535362664712068 ) ) ;
#6211 = CONICAL_SURFACE ( 'NONE', #20062, 4.000000000000001776, 0.9599310885968808105 ) ;
#6212 = CARTESIAN_POINT ( 'NONE',  ( 33.00000000000000000, 489.5971041675262541, 10.80646835458729349 ) ) ;
#6213 = DIRECTION ( 'NONE',  ( 0.000000000000000000, 0.000000000000000000, 1.000000000000000000 ) ) ;
#6214 = ADVANCED_FACE ( 'NONE', ( #99107 ), #58441, .T. ) ;
#6215 = CARTESIAN_POINT ( 'NONE',  ( -46.00000000000000000, 488.2691388621310011, 2.804837155779786428 ) ) ;
#6216 = CARTESIAN_POINT ( 'NONE',  ( 0.000000000000000000, 43.34115912517999902, 57.50357696970298349 ) ) ;
#6217 = ORIENTED_EDGE ( 'NONE', *, *, #53256, .T. ) ;
#6218 = CARTESIAN_POINT ( 'NONE',  ( -8.737863884121635394, 48.00000000000000000, -90.03618980231102853 ) ) ;
#6219 = ORIENTED_EDGE ( 'NONE', *, *, #93016, .F. ) ;
#6220 = FACE_OUTER_BOUND ( 'NONE', #95538, .T. ) ;
#6221 = CARTESIAN_POINT ( 'NONE',  ( -39.65885301127526930, 485.6927826267795467, -4.533530942908484462 ) ) ;
#6222 = CIRCLE ( 'NONE', #11375, 13.50000000000000000 ) ;
#6223 = AXIS2_PLACEMENT_3D ( 'NONE', #81237, #64553, #73684 ) ;
#6224 = LINE ( 'NONE', #14315, #106123 ) ;
#6225 = CARTESIAN_POINT ( 'NONE',  ( 64.30440556324268186, -18.62726074519799724, 73.56828063249902527 ) ) ;
#6226 = ADVANCED_FACE ( 'NONE', ( #16614 ), #92091, .F. ) ;
#6227 = EDGE_CURVE ( 'NONE', #9931, #104720, #83468, .T. ) ;
#6228 = CIRCLE ( 'NONE', #57880, 6.499999999999999112 ) ;
#6229 = EDGE_LOOP ( 'NONE', ( #77598, #60893, #50809, #55908 ) ) ;
#6230 = DIRECTION ( 'NONE',  ( -1.000000000000000000, -1.224606353822377258E-16, -0.000000000000000000 ) ) ;
#6231 = AXIS2_PLACEMENT_3D ( 'NONE', #82141, #96757, #97796 ) ;
#6232 = CARTESIAN_POINT ( 'NONE',  ( -2.977408999572654480, -28.62500000204838813, 7.188101187499999156 ) ) ;
#6233 = SURFACE_STYLE_FILL_AREA ( #104405 ) ;
#6234 = EDGE_LOOP ( 'NONE', ( #47230, #47936, #742, #19639, #46419, #100395 ) ) ;
#6235 = CARTESIAN_POINT ( 'NONE',  ( 47.03591514779354554, 18.70176887044719294, 14.84266952052376176 ) ) ;
#6236 = DIRECTION ( 'NONE',  ( -1.000000000000000000, -0.000000000000000000, -0.000000000000000000 ) ) ;
#6237 = CARTESIAN_POINT ( 'NONE',  ( 7.999999999999998224, -30.78125000409677625, 3.313708498984766493 ) ) ;
#6238 = CARTESIAN_POINT ( 'NONE',  ( 4.175893272574712434, -3.000000000000000000, 7.137815226410047842 ) ) ;
#6239 = CARTESIAN_POINT ( 'NONE',  ( 86.39719173753884718, -50.13946290863540156, 191.2655366294524981 ) ) ;
#6240 = SURFACE_SIDE_STYLE ('',( #32690 ) ) ;
#6241 = AXIS2_PLACEMENT_3D ( 'NONE', #45075, #2997, #19242 ) ;
#6242 = CARTESIAN_POINT ( 'NONE',  ( -5.171846360987437663, 6.036654300442626742, 5.000000000000000000 ) ) ;
#6243 =( NAMED_UNIT ( * ) PLANE_ANGLE_UNIT ( ) SI_UNIT ( $, .RADIAN. ) );
#6244 = CARTESIAN_POINT ( 'NONE',  ( 19.73463816634106038, 304.7971333121957969, 8.925379062039111133 ) ) ;
#6245 = ORIENTED_EDGE ( 'NONE', *, *, #69895, .F. ) ;
#6246 =( LENGTH_UNIT ( ) NAMED_UNIT ( * ) SI_UNIT ( .MILLI., .METRE. ) );
#6247 = FACE_OUTER_BOUND ( 'NONE', #18731, .T. ) ;
#6248 = AXIS2_PLACEMENT_3D ( 'NONE', #55121, #47565, #72379 ) ;
#6249 = CARTESIAN_POINT ( 'NONE',  ( 21.44740118747756341, -59.99999999999999289, 40.42893638695045411 ) ) ;
#6250 = CARTESIAN_POINT ( 'NONE',  ( -99.84481721452227987, -29.99999999999999645, 186.2371469292183406 ) ) ;
#6251 = EDGE_CURVE ( 'NONE', #98662, #78892, #18233, .T. ) ;
#6252 = DIRECTION ( 'NONE',  ( -1.000000000000000000, -0.000000000000000000, -0.000000000000000000 ) ) ;
#6253 = CARTESIAN_POINT ( 'NONE',  ( 35.36861649463124735, -57.69554417999864171, 49.52702078849532086 ) ) ;
#6254 = EDGE_CURVE ( 'NONE', #35136, #62746, #28852, .T. ) ;
#6256 = DIRECTION ( 'NONE',  ( 0.000000000000000000, 0.000000000000000000, -1.000000000000000000 ) ) ;
#6255 = CARTESIAN_POINT ( 'NONE',  ( -9.165151389911699198, 249.7368049370512324, 4.000000000000006217 ) ) ;
#6257 = SURFACE_STYLE_FILL_AREA ( #71531 ) ;
#6258 = CARTESIAN_POINT ( 'NONE',  ( 0.000000000000000000, 0.000000000000000000, -6.123524522925831270 ) ) ;
#6259 = CARTESIAN_POINT ( 'NONE',  ( -9.373884331924891455, 15.95332971149351842, 3.487646406148589229 ) ) ;
#6260 = CARTESIAN_POINT ( 'NONE',  ( -45.99999999998767919, 436.0044609851116206, 15.17967024737457749 ) ) ;
#6261 = CARTESIAN_POINT ( 'NONE',  ( -18.78363382869726195, -60.00000000000001421, 40.07425195021468767 ) ) ;
#6262 = CARTESIAN_POINT ( 'NONE',  ( 1.000000000000004441, -69.59657292934913642, 12.76848391599222410 ) ) ;
#6263 = AXIS2_PLACEMENT_3D ( 'NONE', #74279, #89938, #25240 ) ;
#6264 = CARTESIAN_POINT ( 'NONE',  ( -87.15827005838086450, -24.32436580448878516, 187.0120937654315014 ) ) ;
#6265 = ORIENTED_EDGE ( 'NONE', *, *, #99016, .F. ) ;
#6266 = CARTESIAN_POINT ( 'NONE',  ( 17.50000000000002842, 49.17341269448252206, 64.03715209375951645 ) ) ;
#6267 = PRESENTATION_STYLE_ASSIGNMENT (( #19347 ) ) ;
#6268 = CARTESIAN_POINT ( 'NONE',  ( -13.47192767882545539, -39.47621330262420258, 30.55147369851395212 ) ) ;
#6270 = CARTESIAN_POINT ( 'NONE',  ( 38.85446894546473828, 460.8903912184138676, 2.218456751109172398 ) ) ;
#6269 = CARTESIAN_POINT ( 'NONE',  ( -106.2097612562338753, -59.99999999999998579, 163.7908689420960400 ) ) ;
#6271 = CIRCLE ( 'NONE', #33636, 3.309500000000001663 ) ;
#6272 = ORIENTED_EDGE ( 'NONE', *, *, #51398, .F. ) ;
#6273 = CARTESIAN_POINT ( 'NONE',  ( -7.500000000000007105, 25.66666666666800012, -68.91429205785459544 ) ) ;
#6274 = CARTESIAN_POINT ( 'NONE',  ( -9.060614273896861803, -4.999999999999993783, -17.33913672108680259 ) ) ;
#6275 = CARTESIAN_POINT ( 'NONE',  ( 42.57704743493908950, 486.1612337113410831, 7.852296464539689325 ) ) ;
#6276 = CIRCLE ( 'NONE', #102778, 14.99698745252234566 ) ;
#6277 = SURFACE_STYLE_FILL_AREA ( #52317 ) ;
#6278 = CARTESIAN_POINT ( 'NONE',  ( 15.88092429543898199, 3.778118985502688432, -3.597070451748276554 ) ) ;
#6279 = CARTESIAN_POINT ( 'NONE',  ( 66.96457860869179513, -60.00000000000000000, 126.4729726693442302 ) ) ;
#6280 = EDGE_CURVE ( 'NONE', #38530, #34113, #36478, .T. ) ;
#6281 = CARTESIAN_POINT ( 'NONE',  ( -40.17205142263708240, 310.2804317922712016, -6.358608209531249500 ) ) ;
#6282 = ORIENTED_EDGE ( 'NONE', *, *, #59716, .F. ) ;
#6283 = CARTESIAN_POINT ( 'NONE',  ( 18.09999999999999787, 3.309500000000003439, 4.052968581778167743E-16 ) ) ;
#6284 = DIRECTION ( 'NONE',  ( -1.000000000000000000, 0.000000000000000000, 0.000000000000000000 ) ) ;
#6285 = CIRCLE ( 'NONE', #33903, 4.171999999999999709 ) ;
#6286 = CIRCLE ( 'NONE', #30435, 1.000000000000000666 ) ;
#6288 = FACE_OUTER_BOUND ( 'NONE', #62195, .T. ) ;
#6287 = CARTESIAN_POINT ( 'NONE',  ( 16.61664997849939240, -30.00000000000006395, 37.21280938527437598 ) ) ;
#6289 = CARTESIAN_POINT ( 'NONE',  ( 3.910186774093608264, -1.060342764005019589, 104.5757226097576336 ) ) ;
#6290 = VERTEX_POINT ( 'NONE', #11152 ) ;
#6291 = CARTESIAN_POINT ( 'NONE',  ( -25.07191001826344490, 307.6538819443658213, 10.57909120790611723 ) ) ;
#6292 = ORIENTED_EDGE ( 'NONE', *, *, #48303, .F. ) ;
#6293 = CARTESIAN_POINT ( 'NONE',  ( 19.83463548332445825, 303.8035096162420245, 9.926734387303334017 ) ) ;
#6294 = CARTESIAN_POINT ( 'NONE',  ( 0.000000000000000000, 0.000000000000000000, 0.000000000000000000 ) ) ;
#6295 =( LENGTH_UNIT ( ) NAMED_UNIT ( * ) SI_UNIT ( .MILLI., .METRE. ) );
#6297 = ADVANCED_FACE ( 'NONE', ( #53235 ), #43546, .F. ) ;
#6296 = VERTEX_POINT ( 'NONE', #68359 ) ;
#6298 = SURFACE_STYLE_FILL_AREA ( #40803 ) ;
#6299 = CARTESIAN_POINT ( 'NONE',  ( -113.3259981442381275, -59.99999999999020872, 187.7190709742288277 ) ) ;
#6300 = CARTESIAN_POINT ( 'NONE',  ( 5.821900211247815982, 1.420906337213440507, -6.500000000000000888 ) ) ;
#6301 = CARTESIAN_POINT ( 'NONE',  ( 79.18097233721817929, -60.00000000000002132, 194.8823859941057037 ) ) ;
#6302 = DIRECTION ( 'NONE',  ( 1.000000000000000000, -0.000000000000000000, -0.000000000000000000 ) ) ;
#6303 = CARTESIAN_POINT ( 'NONE',  ( 0.3383111667213267171, 25.18062061424821607, -40.71479504876042910 ) ) ;
#6305 = CARTESIAN_POINT ( 'NONE',  ( 9.152592288502010121, -32.51055960119349209, 29.30987820687813894 ) ) ;
#6304 = CARTESIAN_POINT ( 'NONE',  ( -106.6847104835838564, -14.21045842199429288, 180.1424598013736329 ) ) ;
#6306 = DIRECTION ( 'NONE',  ( 0.000000000000000000, -1.000000000000000000, 0.000000000000000000 ) ) ;
#6307 = FILL_AREA_STYLE ('',( #6850 ) ) ;
#6308 = CARTESIAN_POINT ( 'NONE',  ( -44.90547982323007403, -49.89649444956833690, 46.32591069718235843 ) ) ;
#6309 = DIRECTION ( 'NONE',  ( -0.8660254037844378194, 0.5000000000000013323, 0.000000000000000000 ) ) ;
#6310 = ORIENTED_EDGE ( 'NONE', *, *, #30046, .F. ) ;
#6311 =( NAMED_UNIT ( * ) PLANE_ANGLE_UNIT ( ) SI_UNIT ( $, .RADIAN. ) );
#6312 = DIRECTION ( 'NONE',  ( 0.000000000000000000, 0.5000000000000008882, -0.8660254037844381525 ) ) ;
#6313 = SURFACE_SIDE_STYLE ('',( #83798 ) ) ;
#6315 = ADVANCED_FACE ( 'NONE', ( #3081 ), #53754, .F. ) ;
#6314 = FACE_OUTER_BOUND ( 'NONE', #32475, .T. ) ;
#6316 = CARTESIAN_POINT ( 'NONE',  ( 39.83349330513380693, 4.000000000000002665, 0.000000000000000000 ) ) ;
#6318 = ORIENTED_EDGE ( 'NONE', *, *, #28723, .T. ) ;
#6317 = AXIS2_PLACEMENT_3D ( 'NONE', #90288, #48743, #58457 ) ;
#6319 = CARTESIAN_POINT ( 'NONE',  ( -13.71361667675544993, -8.878897062923181593, 12.10099128770297661 ) ) ;
#6320 = ORIENTED_EDGE ( 'NONE', *, *, #94779, .T. ) ;
#6321 = CARTESIAN_POINT ( 'NONE',  ( 104.1025144181177211, -30.00000000000091305, 196.4537446789288708 ) ) ;
#6322 = CARTESIAN_POINT ( 'NONE',  ( 6.611590817483814497, 41.87945146461261459, -59.42330382799539024 ) ) ;
#6323 = CARTESIAN_POINT ( 'NONE',  ( 97.95630416740392832, -30.00000000000000000, 137.2274071578905250 ) ) ;
#6324 = EDGE_CURVE ( 'NONE', #38799, #58472, #52683, .T. ) ;
#6325 = DIRECTION ( 'NONE',  ( -0.9133097175878012175, -0.1295276157553482965, 0.3861190962856225206 ) ) ;
#6326 = ORIENTED_EDGE ( 'NONE', *, *, #2754, .F. ) ;
#6327 = ORIENTED_EDGE ( 'NONE', *, *, #30920, .T. ) ;
#6328 = ORIENTED_EDGE ( 'NONE', *, *, #37600, .T. ) ;
#6329 = CARTESIAN_POINT ( 'NONE',  ( -27.86871601328855874, 36.37495722881055826, 9.810583054065073583 ) ) ;
#6330 = CARTESIAN_POINT ( 'NONE',  ( -46.00000000000000000, 438.2642212955981336, 10.59429296198687886 ) ) ;
#6331 = DIRECTION ( 'NONE',  ( -0.9915366780650367584, -0.1269898409407732853, -0.02699252395736589927 ) ) ;
#6332 = EDGE_CURVE ( 'NONE', #17481, #96379, #86698, .T. ) ;
#6333 = ORIENTED_EDGE ( 'NONE', *, *, #47887, .F. ) ;
#6334 = FACE_OUTER_BOUND ( 'NONE', #71553, .T. ) ;
#6335 = VERTEX_POINT ( 'NONE', #54798 ) ;
#6336 = CARTESIAN_POINT ( 'NONE',  ( 0.000000000000000000, 0.000000000000000000, -8.500000000000000000 ) ) ;
#6337 = CARTESIAN_POINT ( 'NONE',  ( 89.78679446632952477, -38.52166357420221487, 200.5186810406769666 ) ) ;
#6338 = CARTESIAN_POINT ( 'NONE',  ( 11.76188850610210324, 11.37617155923007850, 9.883422334778840579 ) ) ;
#6339 = CARTESIAN_POINT ( 'NONE',  ( 84.01433852174905326, -45.28719617900539163, 2.480345902927773238 ) ) ;
#6340 = CARTESIAN_POINT ( 'NONE',  ( 67.06464718582454054, -38.00000000000002132, 91.54358707406134954 ) ) ;
#6341 = CARTESIAN_POINT ( 'NONE',  ( 27.91797385465295989, 308.8116655838868496, 11.34157976637432341 ) ) ;
#6342 = CARTESIAN_POINT ( 'NONE',  ( 43.00000000000024158, 485.2629658518202973, -2.796394914059508352 ) ) ;
#6343 = AXIS2_PLACEMENT_3D ( 'NONE', #7986, #40897, #73782 ) ;
#6344 = DIRECTION ( 'NONE',  ( -0.000000000000000000, 1.000000000000000000, -0.000000000000000000 ) ) ;
#6345 = ADVANCED_FACE ( 'NONE', ( #104968 ), #87201, .T. ) ;
#6346 = CYLINDRICAL_SURFACE ( 'NONE', #83658, 1.250000000000001110 ) ;
#6347 = DIRECTION ( 'NONE',  ( -1.000000000000000000, -0.000000000000000000, -0.000000000000000000 ) ) ;
#6348 = ORIENTED_EDGE ( 'NONE', *, *, #14083, .F. ) ;
#6349 = FACE_OUTER_BOUND ( 'NONE', #13298, .T. ) ;
#6350 = CARTESIAN_POINT ( 'NONE',  ( -34.28628779893050194, 463.1569812994642348, 5.966395430562092095 ) ) ;
#6351 = CARTESIAN_POINT ( 'NONE',  ( -3.727843730184232207, 20.26410795673177745, 4.999999999999997335 ) ) ;
#6352 = ORIENTED_EDGE ( 'NONE', *, *, #94444, .T. ) ;
#6353 = CARTESIAN_POINT ( 'NONE',  ( 32.15963082908665172, 464.7082849654401002, 10.94047064225035903 ) ) ;
#6354 = CARTESIAN_POINT ( 'NONE',  ( -31.35447620051816031, 299.6032654252466614, 11.00407147780933670 ) ) ;
#6355 = CARTESIAN_POINT ( 'NONE',  ( -5.000000000000000888, -50.00000000000000000, 42.58845726811989607 ) ) ;
#6356 = UNCERTAINTY_MEASURE_WITH_UNIT (LENGTH_MEASURE( 1.000000000000000082E-05 ), #52707, 'distance_accuracy_value', 'NONE');
#6357 = CARTESIAN_POINT ( 'NONE',  ( 47.40949999999999420, 0.000000000000000000, 0.000000000000000000 ) ) ;
#6358 = CARTESIAN_POINT ( 'NONE',  ( 3.313708498984762052, -15.21874999999999289, -8.000000000000000000 ) ) ;
#6359 = CONICAL_SURFACE ( 'NONE', #11520, 3.309500000000007880, 0.9599310885968770357 ) ;
#6361 = CARTESIAN_POINT ( 'NONE',  ( -37.42621287545377129, -36.69657090219475037, 46.66406363766312637 ) ) ;
#6360 = CIRCLE ( 'NONE', #88995, 5.000000000000011546 ) ;
#6362 = PRODUCT_DEFINITION_SHAPE ( 'NONE', 'NONE',  #106801 ) ;
#6363 = AXIS2_PLACEMENT_3D ( 'NONE', #65929, #100948, #83693 ) ;
#6364 = AXIS2_PLACEMENT_3D ( 'NONE', #54817, #69442, #61352 ) ;
#6365 = PLANE ( 'NONE',  #101806 ) ;
#6366 = VECTOR ( 'NONE', #63515, 1000.000000000000000 ) ;
#6367 = VERTEX_POINT ( 'NONE', #54258 ) ;
#6368 = CARTESIAN_POINT ( 'NONE',  ( 86.40507261641900527, -17.60714839840921186, 177.3339586084961752 ) ) ;
#6369 = EDGE_CURVE ( 'NONE', #15045, #10855, #82618, .T. ) ;
#6370 = CARTESIAN_POINT ( 'NONE',  ( -37.88646966148060358, 27.49864696007435683, 13.42567359854803932 ) ) ;
#6371 = PRESENTATION_STYLE_ASSIGNMENT (( #88902 ) ) ;
#6372 = ORIENTED_EDGE ( 'NONE', *, *, #54863, .T. ) ;
#6373 = CARTESIAN_POINT ( 'NONE',  ( 94.51533167486907416, -57.67223201566687862, 27.17635600706317689 ) ) ;
#6374 =( GEOMETRIC_REPRESENTATION_CONTEXT ( 3 ) GLOBAL_UNCERTAINTY_ASSIGNED_CONTEXT ( ( #103059 ) ) GLOBAL_UNIT_ASSIGNED_CONTEXT ( ( #88173, #62317, #79011 ) ) REPRESENTATION_CONTEXT ( 'NONE', 'WORKASPACE' ) );
#6375 = DIRECTION ( 'NONE',  ( 0.000000000000000000, -1.000000000000000000, 0.000000000000000000 ) ) ;
#6376 = FACE_OUTER_BOUND ( 'NONE', #56628, .T. ) ;
#6377 = AXIS2_PLACEMENT_3D ( 'NONE', #73390, #90129, #39992 ) ;
#6378 = FILL_AREA_STYLE ('',( #73771 ) ) ;
#6379 =( BOUNDED_CURVE ( )  B_SPLINE_CURVE ( 2, ( #43883, #19133, #84883, #10970, #86508, #88078, #4495, #22832, #95113 ),
 .UNSPECIFIED., .F., .F. ) 
 B_SPLINE_CURVE_WITH_KNOTS ( ( 3, 2, 2, 2, 3 ),
 ( 0.3970588235294117418, 0.4044117647058823595, 0.4117647058823529216, 0.4191176470588235947, 0.4264705882352941568 ),
 .UNSPECIFIED. ) 
 CURVE ( )  GEOMETRIC_REPRESENTATION_ITEM ( )  RATIONAL_B_SPLINE_CURVE ( ( 1.000000000000000000, 0.9238795325112867385, 1.000000000000000000, 0.9238795325112867385, 1.000000000000000000, 0.9238795325112867385, 1.000000000000000000, 0.9238795325112861834, 1.000000000000000666 ) ) 
 REPRESENTATION_ITEM ( '' )  );
#6380 = EDGE_CURVE ( 'NONE', #1527, #105973, #25846, .T. ) ;
#6381 = CARTESIAN_POINT ( 'NONE',  ( 29.35512824071881255, 13.99081654327145507, 42.06953762909855499 ) ) ;
#6382 = CARTESIAN_POINT ( 'NONE',  ( 4.175893272574712434, -3.000000000000000000, 7.137815226410047842 ) ) ;
#6383 = DIRECTION ( 'NONE',  ( 0.000000000000000000, -1.000000000000000000, 0.000000000000000000 ) ) ;
#6384 = EDGE_CURVE ( 'NONE', #103542, #18315, #58531, .T. ) ;
#6386 = CARTESIAN_POINT ( 'NONE',  ( -44.12472801210821416, 485.7238370326489871, 3.975897585127424527 ) ) ;
#6385 = CARTESIAN_POINT ( 'NONE',  ( 37.45552916193109638, 490.9506484630742875, 12.34578863136703930 ) ) ;
#6387 = CARTESIAN_POINT ( 'NONE',  ( 43.41290683822503382, 487.0833545439620593, 7.569976829064901658 ) ) ;
#6388 = DIRECTION ( 'NONE',  ( -1.000000000000000000, -0.000000000000000000, -0.000000000000000000 ) ) ;
#6389 = CARTESIAN_POINT ( 'NONE',  ( 1.590636543681225312, -5.000000000000000000, -96.99986829838745450 ) ) ;
#6390 = CARTESIAN_POINT ( 'NONE',  ( -5.452796619269896006, -22.28572503460438625, -30.53339323392108895 ) ) ;
#6391 = PRESENTATION_STYLE_ASSIGNMENT (( #97518 ) ) ;
#6392 = CARTESIAN_POINT ( 'NONE',  ( -83.28104296813326357, -38.00000000000002842, 29.79366431696643147 ) ) ;
#6393 = AXIS2_PLACEMENT_3D ( 'NONE', #52758, #68428, #2067 ) ;
#6394 = EDGE_LOOP ( 'NONE', ( #5563, #15262, #68158, #89923 ) ) ;
#6395 = CARTESIAN_POINT ( 'NONE',  ( 5.975663821521748353, -7.000939006314043311, -0.8740179403733212560 ) ) ;
#6396 = FILL_AREA_STYLE ('',( #96496 ) ) ;
#6397 = AXIS2_PLACEMENT_3D ( 'NONE', #77350, #9942, #68189 ) ;
#6398 = CARTESIAN_POINT ( 'NONE',  ( -8.888168502148841910, -16.05798408390882770, -34.89684864719075819 ) ) ;
#6400 = CARTESIAN_POINT ( 'NONE',  ( -21.82264282896743879, -21.77046146735031584, -29.53569673438909149 ) ) ;
#6399 = CARTESIAN_POINT ( 'NONE',  ( 39.56197461363974099, -0.1944580884125578779, -19.78098730681987405 ) ) ;
#6401 = EDGE_CURVE ( 'NONE', #38536, #25105, #1629, .T. ) ;
#6402 = ORIENTED_EDGE ( 'NONE', *, *, #44781, .T. ) ;
#6403 = CARTESIAN_POINT ( 'NONE',  ( 5.147825380265281581, 5.688155668807426402, -7.450218641349906079 ) ) ;
#6404 = ORIENTED_EDGE ( 'NONE', *, *, #6595, .F. ) ;
#6405 = SURFACE_STYLE_USAGE ( .BOTH. , #106699 ) ;
#6406 = DIRECTION ( 'NONE',  ( -0.000000000000000000, -1.000000000000000000, -0.000000000000000000 ) ) ;
#6407 = CARTESIAN_POINT ( 'NONE',  ( -92.31848817267784568, -60.00000000000000711, 1.263419265082847520 ) ) ;
#6408 = ORIENTED_EDGE ( 'NONE', *, *, #83198, .T. ) ;
#6409 = DIRECTION ( 'NONE',  ( -1.000000000000000000, -1.224606353822377258E-16, -0.000000000000000000 ) ) ;
#6410 = CARTESIAN_POINT ( 'NONE',  ( -7.474625967136768523, 54.29719554478052146, -2.154566369991844699 ) ) ;
#6411 = CARTESIAN_POINT ( 'NONE',  ( 97.19053058376982790, -37.72816749976003337, 192.7922990471952005 ) ) ;
#6413 = CARTESIAN_POINT ( 'NONE',  ( 30.00000000000000000, 9.797174393178835518E-16, -8.000000000000007105 ) ) ;
#6412 = CYLINDRICAL_SURFACE ( 'NONE', #4454, 1.250000000000001110 ) ;
#6414 = CARTESIAN_POINT ( 'NONE',  ( -84.99204860051307264, -18.63719649618825969, 155.3315940931620105 ) ) ;
#6415 = EDGE_CURVE ( 'NONE', #43584, #46987, #40216, .T. ) ;
#6416 = EDGE_LOOP ( 'NONE', ( #89677, #90438, #785, #66998, #84441 ) ) ;
#6417 = ORIENTED_EDGE ( 'NONE', *, *, #28581, .T. ) ;
#6418 = VERTEX_POINT ( 'NONE', #24071 ) ;
#6419 = CARTESIAN_POINT ( 'NONE',  ( 32.11440402022499541, 433.9890634525672795, 24.22968092281466923 ) ) ;
#6420 = CARTESIAN_POINT ( 'NONE',  ( -6.158544544216538519, -12.16561743015693153, 11.88011416285757349 ) ) ;
#6421 = CARTESIAN_POINT ( 'NONE',  ( 0.000000000000000000, -8.000000000000000000, 0.000000000000000000 ) ) ;
#6422 = ORIENTED_EDGE ( 'NONE', *, *, #69819, .F. ) ;
#6423 =( NAMED_UNIT ( * ) SI_UNIT ( $, .STERADIAN. ) SOLID_ANGLE_UNIT ( ) );
#6424 = CARTESIAN_POINT ( 'NONE',  ( -76.05665976993959987, -57.54410268428485153, 193.2876952671887523 ) ) ;
#6425 = LINE ( 'NONE', #22662, #57718 ) ;
#6426 = CARTESIAN_POINT ( 'NONE',  ( -23.85217781305828311, 47.99999999999999289, 60.68504519422551624 ) ) ;
#6427 = CIRCLE ( 'NONE', #46113, 0.7733184030943203169 ) ;
#6428 = CARTESIAN_POINT ( 'NONE',  ( 8.542937654374686218, 0.000000000000000000, -6.800000000000000711 ) ) ;
#6429 = CIRCLE ( 'NONE', #82196, 1.000000000000000888 ) ;
#6430 = DIRECTION ( 'NONE',  ( 0.000000000000000000, -1.000000000000000000, 0.000000000000000000 ) ) ;
#6431 = CARTESIAN_POINT ( 'NONE',  ( -57.68513734192992359, -30.00000000000002487, -33.51766283710919225 ) ) ;
#6432 = CARTESIAN_POINT ( 'NONE',  ( -52.56680815376439853, -59.99999999999999289, 85.36473592189453541 ) ) ;
#6433 = CARTESIAN_POINT ( 'NONE',  ( -52.87296361776452613, -53.37811214081175848, 61.20528467236419345 ) ) ;
#6434 = VERTEX_POINT ( 'NONE', #24596 ) ;
#6435 = CARTESIAN_POINT ( 'NONE',  ( 26.36650669486618881, 1.474610560812782335E-15, 0.000000000000000000 ) ) ;
#6436 = AXIS2_PLACEMENT_3D ( 'NONE', #46952, #63701, #80913 ) ;
#6437 = EDGE_LOOP ( 'NONE', ( #77921, #93869, #44205, #16902, #36277 ) ) ;
#6438 = AXIS2_PLACEMENT_3D ( 'NONE', #94938, #30743, #63629 ) ;
#6439 = CARTESIAN_POINT ( 'NONE',  ( -102.4347604686928292, -60.19196468994024940, 193.6661079742802372 ) ) ;
#6440 = COLOUR_RGB ( '', 0.31764706, 0.68627451, 0.89019608) ;
#6441 = CARTESIAN_POINT ( 'NONE',  ( -30.82851008854539998, 15.24887380073562504, -40.33969805263218689 ) ) ;
#6442 = VERTEX_POINT ( 'NONE', #50418 ) ;
#6443 = CARTESIAN_POINT ( 'NONE',  ( 18.93966886101837233, 49.22383349382435824, 62.05948745186926629 ) ) ;
#6444 = B_SPLINE_CURVE_WITH_KNOTS ( 'NONE', 3,
 ( #17132, #16046, #50525, #32796, #33863, #9011, #66735, #6892, #65668, #98551, #74280, #99078, #99620, #39812, #356, #40325, #106105, #24182, #57025, #24702 ),
 .UNSPECIFIED., .F., .F.,
 ( 4, 2, 2, 2, 2, 2, 2, 2, 2, 4 ),
 ( 0.007062422899244994931, 0.007566298266050987611, 0.008070173632856980292, 0.008322111316259981836, 0.008574048999662985115, 0.009077924366468989939, 0.009581799733274994763, 0.01008567510008100132, 0.01058955046688700441, 0.01109342583369301097 ),
 .UNSPECIFIED. ) ;
#6445 = CARTESIAN_POINT ( 'NONE',  ( 105.3163565900507734, -38.35599845780108552, 119.8810476205262319 ) ) ;
#6446 = CARTESIAN_POINT ( 'NONE',  ( 48.69590189480657472, 13.58600142653058818, 16.66526863408493853 ) ) ;
#6447 = DIRECTION ( 'NONE',  ( 0.000000000000000000, -1.000000000000000000, 0.000000000000000000 ) ) ;
#6448 = CARTESIAN_POINT ( 'NONE',  ( -8.763358074753723415, 294.6787817714944140, 1.900260594084348220 ) ) ;
#6449 = CARTESIAN_POINT ( 'NONE',  ( 43.10000000000000142, 1.533819458162526451E-15, 0.000000000000000000 ) ) ;
#6450 = CARTESIAN_POINT ( 'NONE',  ( 62.34328654791936941, -30.00000000000000355, 72.93326640765459956 ) ) ;
#6451 = CIRCLE ( 'NONE', #66761, 13.27631144943088515 ) ;
#6452 = CARTESIAN_POINT ( 'NONE',  ( 0.2565376335216121295, -2.516992571280029178, 6.499999999999999112 ) ) ;
#6453 = CARTESIAN_POINT ( 'NONE',  ( 4.271055963817978807, 52.15840228002415557, -6.537475947608907489 ) ) ;
#6454 = CARTESIAN_POINT ( 'NONE',  ( 32.61650669486618881, 1.474610560812782335E-15, 0.000000000000000000 ) ) ;
#6455 = ADVANCED_FACE ( 'NONE', ( #56915 ), #18908, .T. ) ;
#6456 = DIRECTION ( 'NONE',  ( -0.000000000000000000, 1.000000000000000000, -0.000000000000000000 ) ) ;
#6457 = EDGE_CURVE ( 'NONE', #76468, #104209, #90363, .T. ) ;
#6458 = ORIENTED_EDGE ( 'NONE', *, *, #53109, .F. ) ;
#6459 = ORIENTED_EDGE ( 'NONE', *, *, #40008, .T. ) ;
#6460 = CARTESIAN_POINT ( 'NONE',  ( 49.86853440584077646, -25.66414929712663096, 46.00440597202735660 ) ) ;
#6461 = CARTESIAN_POINT ( 'NONE',  ( -1.023312400211863871, 296.8556866932425464, -10.00051715684043074 ) ) ;
#6462 = CARTESIAN_POINT ( 'NONE',  ( 80.00000000000000000, 500000.0000000000582, -21.09707704303352926 ) ) ;
#6463 = ADVANCED_FACE ( 'NONE', ( #33213 ), #634, .F. ) ;
#6464 = CARTESIAN_POINT ( 'NONE',  ( -104.2819284261560142, -38.40732750122956674, 198.1583120562690965 ) ) ;
#6465 = AXIS2_PLACEMENT_3D ( 'NONE', #92433, #58497, #27767 ) ;
#6466 = EDGE_LOOP ( 'NONE', ( #82489, #72996, #80241, #28099, #21796, #20538 ) ) ;
#6467 = CARTESIAN_POINT ( 'NONE',  ( 90.74859279193630357, -38.34261006322929433, 6.457795357414656046 ) ) ;
#6468 = CARTESIAN_POINT ( 'NONE',  ( 13.51938198577379779, 20.10480383923402314, -7.057786160369816209 ) ) ;
#6469 = CARTESIAN_POINT ( 'NONE',  ( -19.45212154763352430, 49.97862309486527721, 60.60657320435567641 ) ) ;
#6470 = CARTESIAN_POINT ( 'NONE',  ( -42.73562161879612376, 422.3951324741119606, 19.42488791944230542 ) ) ;
#6471 = CARTESIAN_POINT ( 'NONE',  ( 102.1416586219354627, -37.84845812144148169, 158.6799647160197253 ) ) ;
#6472 = CARTESIAN_POINT ( 'NONE',  ( -8.000000000000000000, 0.000000000000000000, -9.274828571428571422 ) ) ;
#6473 = CARTESIAN_POINT ( 'NONE',  ( 21.97741296367617991, 27.90380497738007293, 32.31715157276715189 ) ) ;
#6474 = CARTESIAN_POINT ( 'NONE',  ( 19.36103579130787367, 294.6347466944262692, -10.04613669444748680 ) ) ;
#6475 = SURFACE_STYLE_USAGE ( .BOTH. , #64216 ) ;
#6476 = CARTESIAN_POINT ( 'NONE',  ( 0.000000000000000000, 47.29617335651134624, 0.000000000000000000 ) ) ;
#6477 = TOROIDAL_SURFACE ( 'NONE', #75384, 8.000000000000007105, 1.000000000000000888 ) ;
#6478 = CARTESIAN_POINT ( 'NONE',  ( 97.69789586047579633, -60.00000000000000711, 202.4097175802237132 ) ) ;
#6479 = ADVANCED_FACE ( 'NONE', ( #57986 ), #90907, .T. ) ;
#6480 = AXIS2_PLACEMENT_3D ( 'NONE', #92796, #57752, #83631 ) ;
#6481 = CARTESIAN_POINT ( 'NONE',  ( 23.21751746555303342, -1.200000000000000030E-05, 31.95617127781017075 ) ) ;
#6482 = VERTEX_POINT ( 'NONE', #32147 ) ;
#6483 = CARTESIAN_POINT ( 'NONE',  ( 57.28223379198149701, -56.85411367214971534, 73.21148081599464774 ) ) ;
#6484 = CARTESIAN_POINT ( 'NONE',  ( -36.05525903195442083, 302.6656030494100378, -8.225097448474809170 ) ) ;
#6485 = CARTESIAN_POINT ( 'NONE',  ( 9.574562898131892652, -51.35212381342775956, 24.10796671758935261 ) ) ;
#6486 = CARTESIAN_POINT ( 'NONE',  ( -7.213352437320217803, 27.98163526992318495, -3.463014597543478068 ) ) ;
#6487 = VERTEX_POINT ( 'NONE', #33748 ) ;
#6489 = CARTESIAN_POINT ( 'NONE',  ( -9.574118164638793615, -51.35373487335582610, 24.10642939627973291 ) ) ;
#6488 = CARTESIAN_POINT ( 'NONE',  ( -109.6873753914951095, -38.35590170415876798, 187.5827713266319847 ) ) ;
#6490 = CARTESIAN_POINT ( 'NONE',  ( -9.797174393178825657E-16, -3.000000000000000000, 8.000000000000000000 ) ) ;
#6491 = CARTESIAN_POINT ( 'NONE',  ( 23.96530074296727975, 306.2618658405915539, 9.248980163680499800 ) ) ;
#6492 = CARTESIAN_POINT ( 'NONE',  ( 8.929771841637641927, 6.123233995736772199E-16, -5.000000000000001776 ) ) ;
#6493 = CARTESIAN_POINT ( 'NONE',  ( -3.313708498984760720, -34.53125000000000000, -8.000000000000000000 ) ) ;
#6494 = CARTESIAN_POINT ( 'NONE',  ( -7.996668422911731078, -5.000000000000002665, -78.85453279917058467 ) ) ;
#6495 = VERTEX_POINT ( 'NONE', #99504 ) ;
#6496 = CARTESIAN_POINT ( 'NONE',  ( 81.09017685471619075, -60.52596391356583894, 183.7721125982857302 ) ) ;
#6497 = CARTESIAN_POINT ( 'NONE',  ( 7.869023716279121672, 87.19016966530782042, -2.311115933264685126E-30 ) ) ;
#6498 = CARTESIAN_POINT ( 'NONE',  ( -35.83770293177492050, 439.9021865884288331, 24.29457972161610968 ) ) ;
#6499 = ORIENTED_EDGE ( 'NONE', *, *, #97094, .T. ) ;
#6500 = CARTESIAN_POINT ( 'NONE',  ( -27.15064582331548237, 305.1140881896778296, -9.501787623090212520 ) ) ;
#6501 = CARTESIAN_POINT ( 'NONE',  ( 7.253185102479642765, -3.609892095615550467, -18.04361009492445689 ) ) ;
#6502 = CARTESIAN_POINT ( 'NONE',  ( 26.94485550679278063, 34.53204227594014952, -10.05698433968635719 ) ) ;
#6503 = CARTESIAN_POINT ( 'NONE',  ( -10.47772246152093700, 50.00000000000000711, -78.93829266524170407 ) ) ;
#6504 = CARTESIAN_POINT ( 'NONE',  ( 0.000000000000000000, 0.000000000000000000, 0.000000000000000000 ) ) ;
#6505 = VERTEX_POINT ( 'NONE', #48819 ) ;
#6506 = EDGE_CURVE ( 'NONE', #91829, #44978, #36159, .T. ) ;
#6507 = B_SPLINE_CURVE_WITH_KNOTS ( 'NONE', 3,
 ( #10662, #77545, #61373, #69459, #70518, #11187, #52724, #19885, #20428, #36065, #3663, #85101, #86191, #78588, #94265, #12265, #93730, #44119 ),
 .UNSPECIFIED., .F., .F.,
 ( 4, 2, 2, 2, 2, 2, 2, 2, 4 ),
 ( 0.5000000000000000000, 0.5625000000000000000, 0.6250000000000000000, 0.6875000000000000000, 0.7500000000000000000, 0.8125000000000000000, 0.8750000000000000000, 0.9375000000000000000, 1.000000000000000000 ),
 .UNSPECIFIED. ) ;
#6508 = AXIS2_PLACEMENT_3D ( 'NONE', #45208, #36080, #27988 ) ;
#6509 = CIRCLE ( 'NONE', #61690, 1.000000000000000666 ) ;
#6510 = CARTESIAN_POINT ( 'NONE',  ( -13.00000000000003730, -65.00000000000000000, 4.000000000000002665 ) ) ;
#6511 = LINE ( 'NONE', #32424, #44125 ) ;
#6512 = EDGE_CURVE ( 'NONE', #88846, #93114, #1324, .T. ) ;
#6513 = EDGE_CURVE ( 'NONE', #31665, #91936, #51890, .T. ) ;
#6515 = CARTESIAN_POINT ( 'NONE',  ( -10.68634199976106913, 15.16085412443461600, -9.768909368315327413 ) ) ;
#6514 = DIRECTION ( 'NONE',  ( 0.000000000000000000, 1.000000000000000000, -1.224646799147353207E-16 ) ) ;
#6516 = CARTESIAN_POINT ( 'NONE',  ( 7.188101187499999156, -22.25000000204839168, 2.977408999572654924 ) ) ;
#6517 = CARTESIAN_POINT ( 'NONE',  ( -29.27130674176756031, 18.74791880384168863, -39.67321021315769514 ) ) ;
#6518 = STYLED_ITEM ( 'NONE', ( #70521 ), #4449 ) ;
#6519 = DIRECTION ( 'NONE',  ( 1.150791560227848297E-16, -0.3420201433256725987, 0.9396926207859068736 ) ) ;
#6520 = ORIENTED_EDGE ( 'NONE', *, *, #104754, .F. ) ;
#6521 = CARTESIAN_POINT ( 'NONE',  ( 0.000000000000000000, 3.999999999999996447, -10.00000000000003730 ) ) ;
#6522 = CARTESIAN_POINT ( 'NONE',  ( 14.29190075645216851, 6.456385560668102208, -7.561819230143448145 ) ) ;
#6523 = CARTESIAN_POINT ( 'NONE',  ( -8.420691126292242146, 123.3228360287979797, -5.000000000001269207 ) ) ;
#6524 = CYLINDRICAL_SURFACE ( 'NONE', #11893, 8.500000000000000000 ) ;
#6525 = LINE ( 'NONE', #88533, #81085 ) ;
#6526 = EDGE_CURVE ( 'NONE', #24323, #37342, #49888, .T. ) ;
#6527 = ORIENTED_EDGE ( 'NONE', *, *, #19211, .F. ) ;
#6528 = AXIS2_PLACEMENT_3D ( 'NONE', #61092, #68662, #84826 ) ;
#6529 = SURFACE_SIDE_STYLE ('',( #54538 ) ) ;
#6530 = DIRECTION ( 'NONE',  ( 0.000000000000000000, -1.000000000000000000, 0.000000000000000000 ) ) ;
#6531 = ORIENTED_EDGE ( 'NONE', *, *, #64000, .F. ) ;
#6532 = LINE ( 'NONE', #31395, #12767 ) ;
#6533 = CARTESIAN_POINT ( 'NONE',  ( -2.520370815125278163, -0.4217707021250795552, 103.1554032654397588 ) ) ;
#6534 = COLOUR_RGB ( '', 0.40784314, 0.44705882, 0.49803922) ;
#6535 = CARTESIAN_POINT ( 'NONE',  ( 7.109733078360420677, 41.69026692163959069, -59.69141567447950081 ) ) ;
#6536 = FILL_AREA_STYLE ('',( #91077 ) ) ;
#6537 = CARTESIAN_POINT ( 'NONE',  ( -106.4915674334330191, -59.99999999999998579, 119.4613221490214272 ) ) ;
#6538 = DIRECTION ( 'NONE',  ( -0.5735764363510497121, 0.8191520442889892450, 1.003171929053521665E-16 ) ) ;
#6539 = CARTESIAN_POINT ( 'NONE',  ( 15.11650669486618881, 1.474610560812782335E-15, 0.000000000000000000 ) ) ;
#6540 = CARTESIAN_POINT ( 'NONE',  ( -32.83699446692833135, 465.7129794908040594, 11.08673065710671857 ) ) ;
#6541 = EDGE_CURVE ( 'NONE', #39221, #82852, #36946, .T. ) ;
#6542 = CARTESIAN_POINT ( 'NONE',  ( -1.570796324976843295, -5.000000000000002665, -97.00000000000000000 ) ) ;
#6543 = CARTESIAN_POINT ( 'NONE',  ( -82.41309296567457920, -50.00852957772184482, 179.9562645980678042 ) ) ;
#6544 = ORIENTED_EDGE ( 'NONE', *, *, #78306, .F. ) ;
#6545 =( NAMED_UNIT ( * ) PLANE_ANGLE_UNIT ( ) SI_UNIT ( $, .RADIAN. ) );
#6546 = EDGE_LOOP ( 'NONE', ( #28352, #87371, #49044, #6727, #77961 ) ) ;
#6547 = DIRECTION ( 'NONE',  ( -1.000000000000000000, 0.000000000000000000, 0.000000000000000000 ) ) ;
#6548 = DIRECTION ( 'NONE',  ( -1.000000000000000000, 0.000000000000000000, 0.000000000000000000 ) ) ;
#6549 = CARTESIAN_POINT ( 'NONE',  ( -83.04985898644524411, -37.82368260205146981, 27.05149038700534447 ) ) ;
#6550 = CARTESIAN_POINT ( 'NONE',  ( -15.72109914222335902, 304.5560401976859453, 9.874133138051915282 ) ) ;
#6551 = AXIS2_PLACEMENT_3D ( 'NONE', #99514, #33222, #98972 ) ;
#6552 = CARTESIAN_POINT ( 'NONE',  ( -16.07816244837236752, 5.101897851396789640, -4.232350007281748816 ) ) ;
#6553 = CARTESIAN_POINT ( 'NONE',  ( 4.086538315195368476, 13.70928807340287747, -5.000000000000000000 ) ) ;
#6554 = FACE_OUTER_BOUND ( 'NONE', #96155, .T. ) ;
#6555 = FACE_OUTER_BOUND ( 'NONE', #24199, .T. ) ;
#6556 = VECTOR ( 'NONE', #71348, 1000.000000000000114 ) ;
#6557 = CARTESIAN_POINT ( 'NONE',  ( 105.3887446370168135, -14.21045842199438347, 188.2131443117102663 ) ) ;
#6558 = ADVANCED_FACE ( 'NONE', ( #76832, #53100 ), #20253, .T. ) ;
#6559 = CARTESIAN_POINT ( 'NONE',  ( -99.88998825557715122, -14.21045842199445808, 111.7645417027540304 ) ) ;
#6560 = CARTESIAN_POINT ( 'NONE',  ( -64.08967996622652663, -22.10365852731207781, 74.71439323467923543 ) ) ;
#6561 = ORIENTED_EDGE ( 'NONE', *, *, #81919, .T. ) ;
#6562 = CARTESIAN_POINT ( 'NONE',  ( -11.84577904457109376, 39.42593554084623975, 63.98138733196459782 ) ) ;
#6563 = CARTESIAN_POINT ( 'NONE',  ( 74.39743302387351775, -60.00000000001976019, 190.5079982696796890 ) ) ;
#6564 = ORIENTED_EDGE ( 'NONE', *, *, #25322, .T. ) ;
#6565 = CARTESIAN_POINT ( 'NONE',  ( 2.007425432336742421, -35.99147847551537183, 29.88588737300932507 ) ) ;
#6566 = CARTESIAN_POINT ( 'NONE',  ( 5.082755093536325930, -19.34375000204838457, -5.082755093536325042 ) ) ;
#6567 =( GEOMETRIC_REPRESENTATION_CONTEXT ( 3 ) GLOBAL_UNCERTAINTY_ASSIGNED_CONTEXT ( ( #77244 ) ) GLOBAL_UNIT_ASSIGNED_CONTEXT ( ( #64804, #88557, #104192 ) ) REPRESENTATION_CONTEXT ( 'NONE', 'WORKASPACE' ) );
#6568 = CARTESIAN_POINT ( 'NONE',  ( 32.92521947946379868, 485.8269030686106476, 5.191998502003437821 ) ) ;
#6569 = VERTEX_POINT ( 'NONE', #61199 ) ;
#6571 = CARTESIAN_POINT ( 'NONE',  ( 4.898587196589412829E-16, -27.31250000409677270, -8.000000000000000000 ) ) ;
#6570 = AXIS2_PLACEMENT_3D ( 'NONE', #93961, #20111, #44888 ) ;
#6572 = ORIENTED_EDGE ( 'NONE', *, *, #42271, .T. ) ;
#6573 = CARTESIAN_POINT ( 'NONE',  ( 10.45066360978653641, 46.08369782028255202, -12.90779740156203914 ) ) ;
#6574 = DIRECTION ( 'NONE',  ( -1.000000000000000000, -0.000000000000000000, -0.000000000000000000 ) ) ;
#6575 = CARTESIAN_POINT ( 'NONE',  ( -105.2092481652586144, -60.00000000000000000, 199.0630387942247808 ) ) ;
#6576 = CARTESIAN_POINT ( 'NONE',  ( -18.99999999999999289, 5.000000000000000888, 25.00000000000000000 ) ) ;
#6577 = CARTESIAN_POINT ( 'NONE',  ( -7.188101187500001821, -26.37500000204838457, -2.977408999572651371 ) ) ;
#6578 = CARTESIAN_POINT ( 'NONE',  ( 44.07878952698373354, 464.4042052658809894, 9.617740716628523145 ) ) ;
#6579 = CARTESIAN_POINT ( 'NONE',  ( -12.01355111023868361, 17.09226180711344156, 9.133437940809011835 ) ) ;
#6580 = CARTESIAN_POINT ( 'NONE',  ( 1.000000000000000000, -59.33342285666933691, 7.478329308248535590 ) ) ;
#6581 = CARTESIAN_POINT ( 'NONE',  ( 6.145467200814584530, 50.00000000000543565, -92.99666842292452884 ) ) ;
#6582 = DIRECTION ( 'NONE',  ( 0.000000000000000000, 1.000000000000000000, 0.000000000000000000 ) ) ;
#6583 = CARTESIAN_POINT ( 'NONE',  ( 0.000000000000000000, 48.00000000000000000, 0.000000000000000000 ) ) ;
#6584 = EDGE_CURVE ( 'NONE', #29730, #34186, #17185, .T. ) ;
#6585 = CARTESIAN_POINT ( 'NONE',  ( 34.73799231214650263, 320.8457050503890287, -5.619366639134932839 ) ) ;
#6586 = CARTESIAN_POINT ( 'NONE',  ( -32.92861475816587813, -46.43446236043871522, 35.59579179906526036 ) ) ;
#6587 = ORIENTED_EDGE ( 'NONE', *, *, #84567, .T. ) ;
#6588 = CARTESIAN_POINT ( 'NONE',  ( -15.92248761028720949, 43.99412595793401692, -88.61019858215870215 ) ) ;
#6589 = AXIS2_PLACEMENT_3D ( 'NONE', #16954, #49831, #73564 ) ;
#6590 = AXIS2_PLACEMENT_3D ( 'NONE', #80066, #46130, #11203 ) ;
#6591 = CARTESIAN_POINT ( 'NONE',  ( 38.12793368476380351, -18.75744117181308113, 32.82679780025620175 ) ) ;
#6593 =( GEOMETRIC_REPRESENTATION_CONTEXT ( 3 ) GLOBAL_UNCERTAINTY_ASSIGNED_CONTEXT ( ( #74288 ) ) GLOBAL_UNIT_ASSIGNED_CONTEXT ( ( #25168, #51533, #83368 ) ) REPRESENTATION_CONTEXT ( 'NONE', 'WORKASPACE' ) );
#6592 = CARTESIAN_POINT ( 'NONE',  ( 5.820808985963070725, 3.863013742957921305E-12, 21.65942590380143074 ) ) ;
#6594 = ORIENTED_EDGE ( 'NONE', *, *, #59211, .T. ) ;
#6595 = EDGE_CURVE ( 'NONE', #19817, #37427, #56730, .T. ) ;
#6596 = CARTESIAN_POINT ( 'NONE',  ( -43.02661387979790675, 465.7449615347597387, 11.43319743843399827 ) ) ;
#6597 = EDGE_CURVE ( 'NONE', #23687, #34601, #84307, .T. ) ;
#6598 = CARTESIAN_POINT ( 'NONE',  ( -70.94375269799076023, -38.32938429878745268, 139.5278196086539992 ) ) ;
#6599 = ORIENTED_EDGE ( 'NONE', *, *, #102807, .T. ) ;
#6601 = CARTESIAN_POINT ( 'NONE',  ( -30.35537264529554946, 338.7115663565144246, 18.05293407820170515 ) ) ;
#6600 = CYLINDRICAL_SURFACE ( 'NONE', #79649, 5.000000000000002665 ) ;
#6602 = CARTESIAN_POINT ( 'NONE',  ( -4.250000000000000000, 5.204748896376250699E-16, -3.393184225085859929 ) ) ;
#6603 = DIRECTION ( 'NONE',  ( -0.000000000000000000, -1.000000000000000000, -0.000000000000000000 ) ) ;
#6604 = AXIS2_PLACEMENT_3D ( 'NONE', #51342, #76684, #35199 ) ;
#6605 = DIRECTION ( 'NONE',  ( 1.000000000000000000, 1.224606353822377258E-16, 0.000000000000000000 ) ) ;
#6606 = EDGE_CURVE ( 'NONE', #89859, #6703, #80159, .T. ) ;
#6607 = CARTESIAN_POINT ( 'NONE',  ( 0.000000000000000000, 115.0000000000000000, 0.000000000000000000 ) ) ;
#6608 = DIRECTION ( 'NONE',  ( -0.000000000000000000, -1.000000000000000000, -0.000000000000000000 ) ) ;
#6609 = DIRECTION ( 'NONE',  ( 0.000000000000000000, -1.000000000000000000, 0.000000000000000000 ) ) ;
#6610 = ADVANCED_FACE ( 'NONE', ( #83862 ), #93013, .T. ) ;
#6611 = CARTESIAN_POINT ( 'NONE',  ( 94.29218632224478824, -59.99999999999999289, 43.67174873413125624 ) ) ;
#6612 = CYLINDRICAL_SURFACE ( 'NONE', #29043, 1.000000000000000888 ) ;
#6613 = EDGE_CURVE ( 'NONE', #26386, #88824, #60901, .T. ) ;
#6614 = CARTESIAN_POINT ( 'NONE',  ( 0.000000000000000000, 0.000000000000000000, 0.000000000000000000 ) ) ;
#6615 = CARTESIAN_POINT ( 'NONE',  ( -2.499999999999999556, -8.980731864869721193, 18.56355538366596747 ) ) ;
#6616 = ORIENTED_EDGE ( 'NONE', *, *, #81398, .F. ) ;
#6617 = AXIS2_PLACEMENT_3D ( 'NONE', #74458, #56129, #41572 ) ;
#6618 = CARTESIAN_POINT ( 'NONE',  ( -87.15276554055643032, -29.99999999999880984, -18.40125190494982377 ) ) ;
#6619 = ORIENTED_EDGE ( 'NONE', *, *, #12314, .T. ) ;
#6620 = CARTESIAN_POINT ( 'NONE',  ( -3.433100064643267224, -49.17501837727334646, 103.8029703184011368 ) ) ;
#6621 = CARTESIAN_POINT ( 'NONE',  ( -16.01293590580086601, 3.745177866445512205, 0.6593600975892003335 ) ) ;
#6622 = CARTESIAN_POINT ( 'NONE',  ( 4.322723262675009614, 10.88947096379691715, 5.000000000000002665 ) ) ;
#6623 = DIRECTION ( 'NONE',  ( -0.000000000000000000, -0.000000000000000000, -1.000000000000000000 ) ) ;
#6624 = CARTESIAN_POINT ( 'NONE',  ( 0.000000000000000000, 49.00000000000000000, 0.000000000000000000 ) ) ;
#6625 = CARTESIAN_POINT ( 'NONE',  ( 7.188101187499999156, -22.62500000204838813, 2.977408999572654924 ) ) ;
#6626 = DIRECTION ( 'NONE',  ( 0.000000000000000000, 1.000000000000000000, 0.000000000000000000 ) ) ;
#6627 = CYLINDRICAL_SURFACE ( 'NONE', #95634, 1.250000000000001110 ) ;
#6628 = CARTESIAN_POINT ( 'NONE',  ( 7.312789351686414641, 41.37363122699996865, -69.62136458039658748 ) ) ;
#6629 = ORIENTED_EDGE ( 'NONE', *, *, #85837, .T. ) ;
#6630 = AXIS2_PLACEMENT_3D ( 'NONE', #100257, #94725, #94176 ) ;
#6631 = APPLICATION_CONTEXT ( 'automotive_design' ) ;
#6632 = AXIS2_PLACEMENT_3D ( 'NONE', #51803, #82583, #16790 ) ;
#6634 = EDGE_LOOP ( 'NONE', ( #83871, #95022, #1871, #55637 ) ) ;
#6633 = CARTESIAN_POINT ( 'NONE',  ( 4.175533140205451410, -1.555218955346045595, 102.9090322054120747 ) ) ;
#6635 = CARTESIAN_POINT ( 'NONE',  ( 82.53639495069484155, -22.15581645431107560, 142.5669552073890713 ) ) ;
#6636 = CARTESIAN_POINT ( 'NONE',  ( 15.29749241881251720, 3.521433830170186408, -3.946287723025023730 ) ) ;
#6637 = ORIENTED_EDGE ( 'NONE', *, *, #48835, .F. ) ;
#6638 = CARTESIAN_POINT ( 'NONE',  ( -12.50000000000000711, 39.72724458256214319, -64.92461122767875281 ) ) ;
#6639 = CARTESIAN_POINT ( 'NONE',  ( -1.248782720325924522, 16.17015974394703903, -50.36890103335689162 ) ) ;
#6640 = CARTESIAN_POINT ( 'NONE',  ( 7.188101187500000044, -10.15625000204838457, 0.000000000000000000 ) ) ;
#6641 = CARTESIAN_POINT ( 'NONE',  ( 7.151217271224853178, 28.21250599554285543, -3.587901469523288700 ) ) ;
#6642 = CARTESIAN_POINT ( 'NONE',  ( -2.832004189415751050, -57.67120204282113605, 41.61186672541032294 ) ) ;
#6643 = B_SPLINE_SURFACE_WITH_KNOTS ( 'NONE', 1, 3, ( 
 ( #56575, #433, #31288, #64174, #106724, #98108, #97045, #88963, #72758, #75426, #35543, #10159, #84598, #67874, #77023, #59799, #10680, #34487, #52209, #99704, #84057, #19378, #51677, #965, #100757, #43073, #25875, #11206 ),
 ( #42526, #25318, #66814, #26926, #59264, #17213, #92676, #58731, #51140, #9615, #82993, #27460, #75961, #68418, #2059, #85122, #18833, #44139, #91630, #50600, #92137, #3141, #66273, #18286, #9088, #99160, #1520, #43596 ) ),
 .UNSPECIFIED., .F., .F., .F.,
 ( 2, 2 ),
 ( 4, 2, 2, 2, 2, 2, 2, 2, 2, 2, 2, 2, 2, 4 ),
 ( 0.000000000000000000, 1.000000000000000000 ),
 ( 0.08901491201581737678, 0.1032490540155679704, 0.1174831960153185778, 0.1317173380150691853, 0.1459514800148197788, 0.1744197640143299588, 0.2028880480138401388, 0.2598246160128514504, 0.3167611840118632616, 0.4306343200098861623, 0.5445074560079088410, 0.6583805920059359051, 0.7722537280039543095, 1.000000000000000000 ),
 .UNSPECIFIED. ) ;
#6644 = CARTESIAN_POINT ( 'NONE',  ( 17.32310258173999884, 302.5970833027072899, 9.883176158642797304 ) ) ;
#6645 = ORIENTED_EDGE ( 'NONE', *, *, #54274, .T. ) ;
#6646 = SURFACE_STYLE_FILL_AREA ( #47626 ) ;
#6647 = DIRECTION ( 'NONE',  ( -0.000000000000000000, -1.000000000000000000, -0.000000000000000000 ) ) ;
#6648 = CARTESIAN_POINT ( 'NONE',  ( 31.82717529009398305, 18.64284798592574433, -21.53956455643801604 ) ) ;
#6649 = EDGE_CURVE ( 'NONE', #72783, #12603, #48060, .T. ) ;
#6650 = DIRECTION ( 'NONE',  ( -1.000000000000000000, -1.224606353822377258E-16, -0.000000000000000000 ) ) ;
#6651 = ORIENTED_EDGE ( 'NONE', *, *, #63592, .F. ) ;
#6652 = CARTESIAN_POINT ( 'NONE',  ( 5.656854249492378806, -12.87500000409676915, 5.656854249492381470 ) ) ;
#6653 = CARTESIAN_POINT ( 'NONE',  ( -33.91219190039863207, -23.55191230016975013, 33.12023192167306007 ) ) ;
#6654 = CARTESIAN_POINT ( 'NONE',  ( 9.999999999999953815, 15.00000000000004974, 1.544939622598893836 ) ) ;
#6655 = VECTOR ( 'NONE', #308, 1000.000000000000227 ) ;
#6656 = FACE_OUTER_BOUND ( 'NONE', #52972, .T. ) ;
#6657 = CIRCLE ( 'NONE', #61829, 5.000000000000011546 ) ;
#6658 = CARTESIAN_POINT ( 'NONE',  ( -8.000000000000001776, -16.15624999999999289, 3.313708498984759387 ) ) ;
#6659 = CARTESIAN_POINT ( 'NONE',  ( 6.750000000000017764, 11.69134295108991317, -13.00000000000000000 ) ) ;
#6660 = PRODUCT_CONTEXT ( 'NONE', #61797, 'mechanical' ) ;
#6661 = CARTESIAN_POINT ( 'NONE',  ( 38.81498927201410254, 27.33046494171043861, 12.09893127910710220 ) ) ;
#6662 = ORIENTED_EDGE ( 'NONE', *, *, #100036, .T. ) ;
#6663 = CARTESIAN_POINT ( 'NONE',  ( 10.85169291771124911, 43.18003339092611270, 15.27576842164405946 ) ) ;
#6664 = SURFACE_STYLE_USAGE ( .BOTH. , #102717 ) ;
#6665 = DIRECTION ( 'NONE',  ( 0.000000000000000000, 0.000000000000000000, 1.000000000000000000 ) ) ;
#6666 = DIRECTION ( 'NONE',  ( 0.000000000000000000, -1.000000000000000000, -1.155626614413199331E-16 ) ) ;
#6667 = DIRECTION ( 'NONE',  ( 0.000000000000000000, -1.000000000000000000, 0.000000000000000000 ) ) ;
#6668 = CARTESIAN_POINT ( 'NONE',  ( 5.500000000000007105, 42.00000000000000000, -70.16688272716299934 ) ) ;
#6669 = VERTEX_POINT ( 'NONE', #1868 ) ;
#6670 = LINE ( 'NONE', #30992, #28969 ) ;
#6671 = CARTESIAN_POINT ( 'NONE',  ( 91.14659984513072288, -57.61327065490866772, 204.1982474754030932 ) ) ;
#6672 = VECTOR ( 'NONE', #93209, 1000.000000000000000 ) ;
#6673 = CONICAL_SURFACE ( 'NONE', #13525, 5.000000000000000000, 0.9599310885968913576 ) ;
#6674 = CARTESIAN_POINT ( 'NONE',  ( 34.63438812787640586, 463.6460534741173660, 19.43326544948845935 ) ) ;
#6675 = DIRECTION ( 'NONE',  ( 1.000000000000000000, 0.000000000000000000, 0.000000000000000000 ) ) ;
#6676 = CYLINDRICAL_SURFACE ( 'NONE', #4777, 4.000000000000000000 ) ;
#6677 = CARTESIAN_POINT ( 'NONE',  ( -72.99129151139911187, -60.00000000000001421, 162.3848276614833708 ) ) ;
#6678 = CARTESIAN_POINT ( 'NONE',  ( -40.07586470527510158, 337.7832441655235129, 20.21182470898328631 ) ) ;
#6679 = CARTESIAN_POINT ( 'NONE',  ( -3.397250002282850685E-16, 7.693909156114118630, -6.460786012260019362 ) ) ;
#6680 = EDGE_CURVE ( 'NONE', #30745, #43471, #70609, .T. ) ;
#6681 = CARTESIAN_POINT ( 'NONE',  ( 37.84772257691316355, 50.00000000000000000, 50.69408796163846631 ) ) ;
#6682 = CARTESIAN_POINT ( 'NONE',  ( -86.14149206422753480, -24.77051094580461665, 180.5811988458752921 ) ) ;
#6683 = ORIENTED_EDGE ( 'NONE', *, *, #46491, .T. ) ;
#6684 = CARTESIAN_POINT ( 'NONE',  ( 23.34833856664048923, 304.4235486217770017, -9.877270693249020184 ) ) ;
#6685 = ORIENTED_EDGE ( 'NONE', *, *, #41821, .F. ) ;
#6686 = CARTESIAN_POINT ( 'NONE',  ( 12.48746907676921047, -3.545640499968000459, -76.71370838498249611 ) ) ;
#6687 = CARTESIAN_POINT ( 'NONE',  ( -27.38137115745341887, 306.5387002105908323, -9.403261508857470474 ) ) ;
#6688 = CARTESIAN_POINT ( 'NONE',  ( -83.26091089620432228, -52.71980576326409107, -16.35630072882100094 ) ) ;
#6689 = AXIS2_PLACEMENT_3D ( 'NONE', #23700, #23166, #72226 ) ;
#6690 = CARTESIAN_POINT ( 'NONE',  ( 7.347880794884118356E-15, 0.000000000000000000, -60.00000000000000000 ) ) ;
#6691 = DIRECTION ( 'NONE',  ( 0.000000000000000000, -0.9911985061125714314, 0.1323839925376427140 ) ) ;
#6692 = AXIS2_PLACEMENT_3D ( 'NONE', #34960, #49504, #50552 ) ;
#6693 = ORIENTED_EDGE ( 'NONE', *, *, #34723, .F. ) ;
#6694 = CARTESIAN_POINT ( 'NONE',  ( 0.000000000000000000, 4.898587196589412829E-16, -4.000000000000000000 ) ) ;
#6695 = DIRECTION ( 'NONE',  ( -0.000000000000000000, 1.000000000000000000, 1.877893248421449282E-16 ) ) ;
#6697 = CARTESIAN_POINT ( 'NONE',  ( 16.57301948837259786, 0.000000000000000000, 4.453875240779975542 ) ) ;
#6696 = B_SPLINE_CURVE_WITH_KNOTS ( 'NONE', 3,
 ( #99172, #65761, #15604, #97571 ),
 .UNSPECIFIED., .F., .F.,
 ( 4, 4 ),
 ( 0.000000000000000000, 0.001668351617186237222 ),
 .UNSPECIFIED. ) ;
#6698 = AXIS2_PLACEMENT_3D ( 'NONE', #100132, #860, #82356 ) ;
#6699 = CARTESIAN_POINT ( 'NONE',  ( 41.82792046605465686, 1.340359594676612611E-15, 0.000000000000000000 ) ) ;
#6700 = CARTESIAN_POINT ( 'NONE',  ( 87.19843643122861465, -14.21045842199432307, -12.73007766572366606 ) ) ;
#6701 = CARTESIAN_POINT ( 'NONE',  ( -77.56842044869100050, -22.13782245202111199, 118.4993958490866248 ) ) ;
#6702 = PRODUCT_DEFINITION ( 'UNKNOWN', '', #12803, #72647 ) ;
#6703 = VERTEX_POINT ( 'NONE', #27277 ) ;
#6704 = CARTESIAN_POINT ( 'NONE',  ( 37.54937173058232247, -29.99999999999994671, 45.10736187702755018 ) ) ;
#6705 = CARTESIAN_POINT ( 'NONE',  ( 63.81650669486618455, 6.856755485862130937E-15, 0.000000000000000000 ) ) ;
#6706 = CARTESIAN_POINT ( 'NONE',  ( 71.41732950648065525, -57.68013501089347272, 166.1457025563863681 ) ) ;
#6707 = CARTESIAN_POINT ( 'NONE',  ( 27.85283950832558375, 34.47317612687007937, 7.792265204343589602 ) ) ;
#6709 = CIRCLE ( 'NONE', #56661, 0.6186547224754559426 ) ;
#6708 = CARTESIAN_POINT ( 'NONE',  ( 33.43853150106103556, 315.3224335203053670, -7.014529384187835781 ) ) ;
#6710 = CARTESIAN_POINT ( 'NONE',  ( 31.36650669486618881, -3.999999999999998224, 0.000000000000000000 ) ) ;
#6711 = VERTEX_POINT ( 'NONE', #44486 ) ;
#6712 = CONICAL_SURFACE ( 'NONE', #75621, 5.000000000000001776, 0.9599310885968803664 ) ;
#6713 = DIRECTION ( 'NONE',  ( -1.000000000000000000, -1.224606353822377258E-16, -0.000000000000000000 ) ) ;
#6714 = CARTESIAN_POINT ( 'NONE',  ( 38.54515645702225868, -5.000000000000000000, 6.123233995736768255E-16 ) ) ;
#6716 = CARTESIAN_POINT ( 'NONE',  ( -106.2188175271023454, -60.15512191887798821, 163.5221892134918278 ) ) ;
#6715 = CARTESIAN_POINT ( 'NONE',  ( -16.52732684424165654, 43.98685724163156863, -87.77868211029610279 ) ) ;
#6717 = CARTESIAN_POINT ( 'NONE',  ( 2.977408999572650927, -20.37500000204838457, -7.188101187500001821 ) ) ;
#6718 = CARTESIAN_POINT ( 'NONE',  ( 44.15895461028591740, 485.1651389999606181, 0.5848183293818906003 ) ) ;
#6719 =( BOUNDED_SURFACE ( )  B_SPLINE_SURFACE ( 2, 3, ( 
 ( #83543, #27493, #20481, #9644, #3715, #18863, #42554, #67902 ),
 ( #34515, #10187, #100789, #53321, #93243, #75455, #11240, #85148 ),
 ( #10709, #92166, #11776, #44166, #43624, #51166, #68446, #26951 ) ),
 .UNSPECIFIED., .F., .F., .F. ) 
 B_SPLINE_SURFACE_WITH_KNOTS ( ( 3, 3 ),
 ( 4, 2, 2, 4 ),
 ( 0.000000000000000000, 1.000000000000000000 ),
 ( 0.001098271369759734172, 0.002880329893317254419, 0.01191429205785460299, 0.01567206406577980465 ),
 .UNSPECIFIED. ) 
 GEOMETRIC_REPRESENTATION_ITEM ( )  RATIONAL_B_SPLINE_SURFACE ( (
 ( 1.000000000000000000, 1.000000000000000000, 1.000000000000000000, 1.000000000000000000, 1.000000000000000000, 1.000000000000000000, 1.000000000000000000, 1.000000000000000000),
 ( 1.857142857142858317, 1.857142857142858317, 1.857142857142858317, 1.857142857142858317, 1.857142857142858317, 1.857142857142858317, 1.857142857142858317, 1.857142857142858317),
 ( 1.000000000000000000, 1.000000000000000000, 1.000000000000000000, 1.000000000000000000, 1.000000000000000000, 1.000000000000000000, 1.000000000000000000, 1.000000000000000000) ) ) 
 REPRESENTATION_ITEM ( '' )  SURFACE ( )  );
#6720 = CARTESIAN_POINT ( 'NONE',  ( 9.176645556628256983, 84.47260967593273051, 3.973966573947710135 ) ) ;
#6721 = CARTESIAN_POINT ( 'NONE',  ( 6.917892303299533197, 41.82074860089118573, -68.91429206365098992 ) ) ;
#6722 = VERTEX_POINT ( 'NONE', #12093 ) ;
#6723 = CARTESIAN_POINT ( 'NONE',  ( -7.915341292092665348, -3.857523022641996757, -7.913710289178197854 ) ) ;
#6724 = DIRECTION ( 'NONE',  ( -0.000000000000000000, 1.000000000000000000, -0.000000000000000000 ) ) ;
#6725 = B_SPLINE_CURVE_WITH_KNOTS ( 'NONE', 3,
 ( #90781, #73507, #8780, #32566, #16345, #8250, #106406, #16895, #50300, #72976, #49775, #98331, #9302, #65437, #49231, #652, #42212, #64906, #97790, #82677, #23954, #24487, #41164, #57323, #89719, #40621, #74045, #127, #65962, #41687, #33617, #66489 ),
 .UNSPECIFIED., .F., .F.,
 ( 4, 2, 2, 2, 2, 2, 2, 2, 2, 2, 2, 2, 2, 2, 2, 4 ),
 ( 0.01223842624040720820, 0.01316182229273521118, 0.01362352031889921961, 0.01408521834506322977, 0.01431606735814522705, 0.01454691637122722432, 0.01477776538430922160, 0.01500861439739121887, 0.01523946341047322656, 0.01547031242355523251, 0.01593201044971924440, 0.01639370847588325283, 0.01685540650204726473, 0.01777880255437528506, 0.01870219860670330886, 0.01962559465903132919 ),
 .UNSPECIFIED. ) ;
#6726 = CIRCLE ( 'NONE', #60120, 4.000000000000000888 ) ;
#6727 = ORIENTED_EDGE ( 'NONE', *, *, #104724, .T. ) ;
#6728 = CARTESIAN_POINT ( 'NONE',  ( 59.89460441624491693, 6.975173280561618775E-15, 0.000000000000000000 ) ) ;
#6730 = CARTESIAN_POINT ( 'NONE',  ( 29.95010272283230535, -18.65120705511333909, 29.35495255050972219 ) ) ;
#6729 = DIRECTION ( 'NONE',  ( 0.000000000000000000, 0.000000000000000000, -1.000000000000000000 ) ) ;
#6731 = CARTESIAN_POINT ( 'NONE',  ( -24.35655756968438013, 25.22426415880443784, 32.47765811203136366 ) ) ;
#6732 = VERTEX_POINT ( 'NONE', #67693 ) ;
#6733 = EDGE_CURVE ( 'NONE', #54018, #67401, #98163, .T. ) ;
#6734 = ORIENTED_EDGE ( 'NONE', *, *, #70596, .F. ) ;
#6735 = CARTESIAN_POINT ( 'NONE',  ( -1.102351293730349013, 43.39607531963768849, -18.11074648114046681 ) ) ;
#6736 = CARTESIAN_POINT ( 'NONE',  ( 42.76230833568492073, 461.1825766694568642, 3.198895819599614221 ) ) ;
#6737 = CARTESIAN_POINT ( 'NONE',  ( 14.15420665121519939, 0.7683508055187184826, 14.98090773217467664 ) ) ;
#6738 = DIRECTION ( 'NONE',  ( 0.000000000000000000, 0.000000000000000000, 1.000000000000000000 ) ) ;
#6739 = ORIENTED_EDGE ( 'NONE', *, *, #103409, .T. ) ;
#6740 = AXIS2_PLACEMENT_3D ( 'NONE', #13022, #85899, #3899 ) ;
#6741 = CARTESIAN_POINT ( 'NONE',  ( 33.13150386023963989, -60.00000000000000000, -40.54080046662263470 ) ) ;
#6742 = FACE_OUTER_BOUND ( 'NONE', #12802, .T. ) ;
#6743 = CARTESIAN_POINT ( 'NONE',  ( -0.000000000000000000, 34.25047185182970111, -44.13186320217320713 ) ) ;
#6744 = EDGE_CURVE ( 'NONE', #23775, #9645, #17151, .T. ) ;
#6745 = CARTESIAN_POINT ( 'NONE',  ( -11.99986829839165203, -5.000000000000000000, -86.59063654369539620 ) ) ;
#6746 = EDGE_CURVE ( 'NONE', #71455, #6434, #43942, .T. ) ;
#6747 = DIRECTION ( 'NONE',  ( -1.000000000000000000, -0.000000000000000000, -0.000000000000000000 ) ) ;
#6748 = ORIENTED_EDGE ( 'NONE', *, *, #1705, .T. ) ;
#6749 = ORIENTED_EDGE ( 'NONE', *, *, #37385, .T. ) ;
#6750 = EDGE_CURVE ( 'NONE', #63565, #43261, #37353, .T. ) ;
#6751 = ORIENTED_EDGE ( 'NONE', *, *, #18659, .T. ) ;
#6752 = CARTESIAN_POINT ( 'NONE',  ( -2.324561895696642773E-13, 53.39766064372246746, 10.25000000000230038 ) ) ;
#6753 = DIRECTION ( 'NONE',  ( -0.000000000000000000, -0.000000000000000000, 1.000000000000000000 ) ) ;
#6754 = DIRECTION ( 'NONE',  ( -1.000000000000000000, -1.224606353822377258E-16, -0.000000000000000000 ) ) ;
#6755 = CARTESIAN_POINT ( 'NONE',  ( 20.33092854325555621, 302.8589055981394154, 9.938509071751244761 ) ) ;
#6756 = CARTESIAN_POINT ( 'NONE',  ( -43.60671974750798796, 374.5964741257981245, 14.40348595307846757 ) ) ;
#6757 = CARTESIAN_POINT ( 'NONE',  ( -6.054168735073517382, -62.91602293657745548, 14.37668516551084075 ) ) ;
#6759 = DIRECTION ( 'NONE',  ( 1.000000000000000000, 1.224606353822377258E-16, 0.000000000000000000 ) ) ;
#6758 = AXIS2_PLACEMENT_3D ( 'NONE', #98048, #6909, #16602 ) ;
#6760 = DIRECTION ( 'NONE',  ( -1.000000000000000000, -0.000000000000000000, -0.000000000000000000 ) ) ;
#6761 = VERTEX_POINT ( 'NONE', #43418 ) ;
#6762 = CARTESIAN_POINT ( 'NONE',  ( 46.02200000000003399, 0.000000000000000000, 0.000000000000000000 ) ) ;
#6763 = EDGE_LOOP ( 'NONE', ( #104933, #74489, #83872, #85133 ) ) ;
#6764 = CARTESIAN_POINT ( 'NONE',  ( 0.000000000000000000, -78.00000000000000000, 39.00000000000000000 ) ) ;
#6765 = CARTESIAN_POINT ( 'NONE',  ( 20.97754405179127346, 294.8763868968453608, 9.942224931492237516 ) ) ;
#6766 = FILL_AREA_STYLE ('',( #47744 ) ) ;
#6767 = CIRCLE ( 'NONE', #91168, 4.000000000000000000 ) ;
#6768 = MECHANICAL_DESIGN_GEOMETRIC_PRESENTATION_REPRESENTATION (  '', ( #72207 ), #39719 ) ;
#6769 = CARTESIAN_POINT ( 'NONE',  ( -57.52277648265613408, -60.00000000000000711, 75.19842801418919009 ) ) ;
#6770 = CARTESIAN_POINT ( 'NONE',  ( 65.68943055205097892, -18.62638644426881385, 77.38610594788109154 ) ) ;
#6771 = EDGE_LOOP ( 'NONE', ( #10359, #69863 ) ) ;
#6772 = CARTESIAN_POINT ( 'NONE',  ( 41.35030302661661494, 464.3615232856287776, 17.53848297742646523 ) ) ;
#6773 = CARTESIAN_POINT ( 'NONE',  ( 0.2578475836320761050, -6.890627091270383531, -1.065083781909173632 ) ) ;
#6774 = CARTESIAN_POINT ( 'NONE',  ( 3.750000000000007105, 6.495190528383288253, 1.734723475976807094E-15 ) ) ;
#6775 = EDGE_LOOP ( 'NONE', ( #89563, #104379, #6662 ) ) ;
#6776 = AXIS2_PLACEMENT_3D ( 'NONE', #18682, #25172, #76339 ) ;
#6777 =( NAMED_UNIT ( * ) SI_UNIT ( $, .STERADIAN. ) SOLID_ANGLE_UNIT ( ) );
#6778 = CARTESIAN_POINT ( 'NONE',  ( 46.96293930799767224, 18.79139706470995108, 14.94845605815066136 ) ) ;
#6779 = CIRCLE ( 'NONE', #48111, 5.000000000000011546 ) ;
#6780 = CARTESIAN_POINT ( 'NONE',  ( -37.26845974722169785, 490.8898249940490359, 12.42613736167099425 ) ) ;
#6781 = EDGE_CURVE ( 'NONE', #1839, #56748, #93987, .T. ) ;
#6782 = CARTESIAN_POINT ( 'NONE',  ( 5.656854249492378806, -30.87500000409677625, 5.656854249492381470 ) ) ;
#6783 = CARTESIAN_POINT ( 'NONE',  ( 86.48456354109262634, -17.02907541486232645, 183.8954425549199243 ) ) ;
#6784 = CONICAL_SURFACE ( 'NONE', #65391, 4.999999999999999112, 0.7853981633974543852 ) ;
#6785 = LINE ( 'NONE', #32144, #86091 ) ;
#6786 = UNCERTAINTY_MEASURE_WITH_UNIT (LENGTH_MEASURE( 1.000000000000000082E-05 ), #63979, 'distance_accuracy_value', 'NONE');
#6787 = CARTESIAN_POINT ( 'NONE',  ( -10.04820350651657357, 7.431158258250301074, 4.999999999999990230 ) ) ;
#6788 = CARTESIAN_POINT ( 'NONE',  ( -43.00000000000000000, 459.9277931459707247, 6.461582622321705216 ) ) ;
#6789 = CARTESIAN_POINT ( 'NONE',  ( 6.657112139591454536, 304.7445950413702462, 8.914202688817031373 ) ) ;
#6790 = ORIENTED_EDGE ( 'NONE', *, *, #30179, .T. ) ;
#6791 = CARTESIAN_POINT ( 'NONE',  ( 0.5805565836007582359, 3.752776749732553263, -6.499999999999999112 ) ) ;
#6792 = CARTESIAN_POINT ( 'NONE',  ( 33.26116186592400936, -60.00000000000000711, 45.03127399487921423 ) ) ;
#6793 = CARTESIAN_POINT ( 'NONE',  ( -98.86309202372207494, -30.00000000000000000, 189.1393124449016625 ) ) ;
#6794 = ADVANCED_FACE ( 'NONE', ( #30978 ), #39100, .T. ) ;
#6795 = DIRECTION ( 'NONE',  ( 0.000000000000000000, -1.000000000000000000, 0.000000000000000000 ) ) ;
#6796 = CARTESIAN_POINT ( 'NONE',  ( 35.34307722619001879, -57.69551862194811065, 49.50014266750830672 ) ) ;
#6798 = CARTESIAN_POINT ( 'NONE',  ( 43.19180182229770537, 464.9217280166857336, 10.90460934079956523 ) ) ;
#6797 = CARTESIAN_POINT ( 'NONE',  ( 5.420470438621123321, 41.88321586334136981, -59.04137885805280916 ) ) ;
#6800 = CARTESIAN_POINT ( 'NONE',  ( -22.51022956527200947, 41.90417131191598799, -79.55355073162097312 ) ) ;
#6799 = CIRCLE ( 'NONE', #73925, 2.999999999999992450 ) ;
#6801 = CARTESIAN_POINT ( 'NONE',  ( -32.06000226508932371, 464.8616989741469183, 13.97143297948053764 ) ) ;
#6802 =( LENGTH_UNIT ( ) NAMED_UNIT ( * ) SI_UNIT ( .MILLI., .METRE. ) );
#6803 = DIRECTION ( 'NONE',  ( 1.000000000000000000, -0.000000000000000000, -0.000000000000000000 ) ) ;
#6804 = CARTESIAN_POINT ( 'NONE',  ( -25.16295877377567436, -60.00000000000000711, 41.21436381525774095 ) ) ;
#6805 = CARTESIAN_POINT ( 'NONE',  ( 13.94300157694754461, 6.957367296339416640, 7.995343388762901959 ) ) ;
#6806 = ADVANCED_FACE ( 'NONE', ( #62791 ), #44245, .T. ) ;
#6807 = CARTESIAN_POINT ( 'NONE',  ( -86.79095994919661905, -24.35916602586322810, 185.5609027488455354 ) ) ;
#6808 = VERTEX_POINT ( 'NONE', #71387 ) ;
#6809 = CARTESIAN_POINT ( 'NONE',  ( 17.49999999999998934, 50.03360497985808308, 63.82236279034708559 ) ) ;
#6810 = CARTESIAN_POINT ( 'NONE',  ( 35.52862250380135123, 439.1409266922558459, 24.07163373315673738 ) ) ;
#6811 = CARTESIAN_POINT ( 'NONE',  ( -13.61893567220048773, -49.92092318789549665, 32.29805822840884844 ) ) ;
#6812 = FACE_OUTER_BOUND ( 'NONE', #85185, .T. ) ;
#6813 = EDGE_CURVE ( 'NONE', #36986, #103730, #1079, .T. ) ;
#6814 = CARTESIAN_POINT ( 'NONE',  ( 0.9108756637621119312, -6.979659189788956830, -6.219623095962687920 ) ) ;
#6815 = VERTEX_POINT ( 'NONE', #6659 ) ;
#6816 = FACE_OUTER_BOUND ( 'NONE', #98880, .T. ) ;
#6817 = CARTESIAN_POINT ( 'NONE',  ( -7.261743840243895853, -3.634783834963452698, -18.04052776593958285 ) ) ;
#6818 = CARTESIAN_POINT ( 'NONE',  ( 68.45015997180047407, -1.232595164407830946E-29, 4.000000000000007105 ) ) ;
#6819 = VECTOR ( 'NONE', #76831, 1000.000000000000000 ) ;
#6820 = CARTESIAN_POINT ( 'NONE',  ( 73.07582179318477245, -60.00000000000000711, 163.1513601165613068 ) ) ;
#6821 = CARTESIAN_POINT ( 'NONE',  ( -0.3380055730847335571, 53.40879994520549445, -10.21500750740870700 ) ) ;
#6822 = ORIENTED_EDGE ( 'NONE', *, *, #80311, .F. ) ;
#6823 = DIRECTION ( 'NONE',  ( -0.000000000000000000, -0.000000000000000000, -1.000000000000000000 ) ) ;
#6824 =( NAMED_UNIT ( * ) PLANE_ANGLE_UNIT ( ) SI_UNIT ( $, .RADIAN. ) );
#6825 = CIRCLE ( 'NONE', #34198, 5.000000000000001776 ) ;
#6827 = CARTESIAN_POINT ( 'NONE',  ( 0.000000000000000000, 0.000000000000000000, -4.567799999999999194 ) ) ;
#6826 = CARTESIAN_POINT ( 'NONE',  ( 39.73542184579525838, -14.21045842199450782, 43.02758494329003014 ) ) ;
#6828 = CARTESIAN_POINT ( 'NONE',  ( 4.322615621094081817, 141.1094294873553849, -4.999999999999998224 ) ) ;
#6829 = CARTESIAN_POINT ( 'NONE',  ( -4.999999999999993783, -4.000000000000002665, 102.2532056551910387 ) ) ;
#6830 = ORIENTED_EDGE ( 'NONE', *, *, #100436, .T. ) ;
#6831 = ADVANCED_FACE ( 'NONE', ( #96227 ), #95918, .F. ) ;
#6832 = CARTESIAN_POINT ( 'NONE',  ( -30.46048364471454661, 326.5320051201829870, 15.51034741246410498 ) ) ;
#6833 = ORIENTED_EDGE ( 'NONE', *, *, #20025, .F. ) ;
#6834 = CARTESIAN_POINT ( 'NONE',  ( 0.000000000000000000, 0.000000000000000000, 0.000000000000000000 ) ) ;
#6835 = CARTESIAN_POINT ( 'NONE',  ( -3.400000000000000355, 4.163799117101001052E-16, -2.716724522925831220 ) ) ;
#6836 = DIRECTION ( 'NONE',  ( -0.8191520442889913545, 0.000000000000000000, -0.5735764363510468256 ) ) ;
#6837 = ORIENTED_EDGE ( 'NONE', *, *, #1747, .T. ) ;
#6838 = CARTESIAN_POINT ( 'NONE',  ( 56.06936961874005476, 50.00000000006009770, -33.41736086627872027 ) ) ;
#6839 = CARTESIAN_POINT ( 'NONE',  ( 5.000000000000000000, -13.90268927672022947, 9.980021953238734866 ) ) ;
#6840 = CIRCLE ( 'NONE', #44836, 4.000000000000000888 ) ;
#6841 = CARTESIAN_POINT ( 'NONE',  ( -79.72833642093169715, -59.99999999999754863, 199.4660593480937791 ) ) ;
#6842 = CARTESIAN_POINT ( 'NONE',  ( 46.00000000000000711, 486.3401354059829487, 3.362847677636602306 ) ) ;
#6843 = CARTESIAN_POINT ( 'NONE',  ( 78.42325447905815849, -60.00000000000002842, 193.6655075910977359 ) ) ;
#6844 = FACE_OUTER_BOUND ( 'NONE', #54156, .T. ) ;
#6845 = CARTESIAN_POINT ( 'NONE',  ( 0.8403905909943980568, 25.95797979004243317, -38.57101967074649451 ) ) ;
#6847 = CARTESIAN_POINT ( 'NONE',  ( 9.055366547345554906, -22.06741143183647225, 27.56839278369679747 ) ) ;
#6846 = CARTESIAN_POINT ( 'NONE',  ( -113.3391396720030428, -60.00000000000005684, 187.7090405971777898 ) ) ;
#6849 = CARTESIAN_POINT ( 'NONE',  ( 93.54169269461303315, -38.00000000000000000, 99.15423023452258633 ) ) ;
#6848 = PRODUCT_DEFINITION_CONTEXT ( 'detailed design', #28730, 'design' ) ;
#6850 = FILL_AREA_STYLE_COLOUR ( '', #51650 ) ;
#6851 = VECTOR ( 'NONE', #101786, 1000.000000000000000 ) ;
#6852 = CARTESIAN_POINT ( 'NONE',  ( -44.95452292836267816, -53.35130017089566223, 47.31599179322356719 ) ) ;
#6853 = CARTESIAN_POINT ( 'NONE',  ( -8.786988139152953468E-15, 18.64300841652315910, 38.36521369532682257 ) ) ;
#6854 = EDGE_LOOP ( 'NONE', ( #42023, #50113, #47329, #52349 ) ) ;
#6855 = DIRECTION ( 'NONE',  ( 0.000000000000000000, 0.000000000000000000, -1.000000000000000000 ) ) ;
#6856 = CARTESIAN_POINT ( 'NONE',  ( 0.05533025579362120527, 6.264553569211842365, -2.149474931388136945 ) ) ;
#6857 = CARTESIAN_POINT ( 'NONE',  ( 2.500000000000002220, -10.61161631886071000, -19.67321533785385412 ) ) ;
#6858 = CARTESIAN_POINT ( 'NONE',  ( 13.58757579978431629, 304.5480424167135993, -9.064568323117281778 ) ) ;
#6859 = DIRECTION ( 'NONE',  ( 0.000000000000000000, -1.000000000000000000, 0.000000000000000000 ) ) ;
#6860 = ORIENTED_EDGE ( 'NONE', *, *, #84496, .T. ) ;
#6861 = CARTESIAN_POINT ( 'NONE',  ( 4.750186375024036955, -48.62189236691690297, 104.3180500829682131 ) ) ;
#6862 = ORIENTED_EDGE ( 'NONE', *, *, #101224, .F. ) ;
#6863 = CARTESIAN_POINT ( 'NONE',  ( 107.4906260354581349, -29.99999999999830536, 190.3131457271783518 ) ) ;
#6864 = CARTESIAN_POINT ( 'NONE',  ( -27.10511071441182906, 36.60571256639526894, 10.05698433968618488 ) ) ;
#6865 = CARTESIAN_POINT ( 'NONE',  ( 6.511374583785752179, 41.81949009030999775, -59.12906284281419289 ) ) ;
#6867 = EDGE_CURVE ( 'NONE', #3716, #7616, #83995, .T. ) ;
#6866 = CYLINDRICAL_SURFACE ( 'NONE', #23920, 5.000000000000001776 ) ;
#6868 = CARTESIAN_POINT ( 'NONE',  ( 94.33119406073718949, -29.99999999999999645, 113.9538965140871198 ) ) ;
#6869 = EDGE_CURVE ( 'NONE', #100861, #98784, #4602, .T. ) ;
#6870 = CARTESIAN_POINT ( 'NONE',  ( 46.00000000000000000, 450.0000000000002274, 13.20242257375370976 ) ) ;
#6871 = ORIENTED_EDGE ( 'NONE', *, *, #16330, .T. ) ;
#6872 = AXIS2_PLACEMENT_3D ( 'NONE', #102579, #19586, #86421 ) ;
#6873 = ORIENTED_EDGE ( 'NONE', *, *, #82191, .F. ) ;
#6874 = ORIENTED_EDGE ( 'NONE', *, *, #85049, .F. ) ;
#6875 = DIRECTION ( 'NONE',  ( 1.000000000000000000, 1.224606353822377258E-16, 0.000000000000000000 ) ) ;
#6876 = CARTESIAN_POINT ( 'NONE',  ( 21.97273450119370963, 25.82538667424861245, 32.15393027124035541 ) ) ;
#6877 = ADVANCED_FACE ( 'NONE', ( #97262 ), #2884, .T. ) ;
#6878 = CARTESIAN_POINT ( 'NONE',  ( -40.00898563721548840, 463.9413272056387996, 18.74131282407823207 ) ) ;
#6879 = EDGE_LOOP ( 'NONE', ( #11834, #99440, #14654, #42399, #81650 ) ) ;
#6880 = FACE_OUTER_BOUND ( 'NONE', #23165, .T. ) ;
#6881 = CONICAL_SURFACE ( 'NONE', #70634, 5.000000000000001776, 0.9599310885968803664 ) ;
#6882 = ORIENTED_EDGE ( 'NONE', *, *, #82406, .T. ) ;
#6883 = CARTESIAN_POINT ( 'NONE',  ( 6.499999999999999112, 3.752776749732559036, -8.000000000000000000 ) ) ;
#6884 = CARTESIAN_POINT ( 'NONE',  ( 79.09286514343337160, -38.69997524062500815, 191.1501546668640117 ) ) ;
#6885 = CARTESIAN_POINT ( 'NONE',  ( 14.21511914782685082, 4.168509763117726585, 4.751336337983421032 ) ) ;
#6886 = CARTESIAN_POINT ( 'NONE',  ( 85.54804277169388627, -52.72484354478569202, -1.684791068517219381 ) ) ;
#6887 = CARTESIAN_POINT ( 'NONE',  ( 6.683837171061805194, -3.955946848495972556, -6.851900933636989599 ) ) ;
#6888 = CARTESIAN_POINT ( 'NONE',  ( 39.42236559726133294, 328.0579091555865148, 18.01452268087317776 ) ) ;
#6889 = CARTESIAN_POINT ( 'NONE',  ( 10.28624191511809371, 45.38549880562041494, -15.40779740156171762 ) ) ;
#6890 = CONICAL_SURFACE ( 'NONE', #5212, 4.172000000000009479, 0.9599310885968813656 ) ;
#6891 = CARTESIAN_POINT ( 'NONE',  ( 0.2573354458087852015, -4.368923434677197903, -5.432802636760778903 ) ) ;
#6892 = CARTESIAN_POINT ( 'NONE',  ( -28.19190453213781566, 34.18019048552498163, -9.430186636756511476 ) ) ;
#6893 = CARTESIAN_POINT ( 'NONE',  ( 0.000000000000000000, 69.00000000000000000, -4.999999999999993783 ) ) ;
#6894 = SURFACE_STYLE_FILL_AREA ( #39816 ) ;
#6895 = CARTESIAN_POINT ( 'NONE',  ( 11.84999999999999787, 1.533819458162526451E-15, 0.000000000000000000 ) ) ;
#6896 = EDGE_LOOP ( 'NONE', ( #2850, #96097, #36749, #14788 ) ) ;
#6897 = CARTESIAN_POINT ( 'NONE',  ( -42.21835935851050436, 436.4384481632509392, 19.62208033733266177 ) ) ;
#6899 = CARTESIAN_POINT ( 'NONE',  ( -25.28458893461199253, 304.8349036104926881, 10.37793651244948379 ) ) ;
#6898 =( NAMED_UNIT ( * ) PLANE_ANGLE_UNIT ( ) SI_UNIT ( $, .RADIAN. ) );
#6900 = CARTESIAN_POINT ( 'NONE',  ( 32.76922047444633534, 484.1128301720478930, 1.839745883407026161 ) ) ;
#6901 = FACE_OUTER_BOUND ( 'NONE', #47116, .T. ) ;
#6902 = CARTESIAN_POINT ( 'NONE',  ( 8.000000000000000000, -15.40624999999999467, -3.313708498984761608 ) ) ;
#6903 = CARTESIAN_POINT ( 'NONE',  ( 25.37876591545637339, -29.29967622782716319, 38.35509702236433327 ) ) ;
#6904 = AXIS2_PLACEMENT_3D ( 'NONE', #89182, #19050, #84806 ) ;
#6905 = ADVANCED_FACE ( 'NONE', ( #15286 ), #95982, .F. ) ;
#6906 = ORIENTED_EDGE ( 'NONE', *, *, #12047, .T. ) ;
#6907 = CARTESIAN_POINT ( 'NONE',  ( 86.05773094049673944, -24.85131605070118255, 179.6131699954536316 ) ) ;
#6908 = ADVANCED_FACE ( 'NONE', ( #32023 ), #66486, .T. ) ;
#6909 = DIRECTION ( 'NONE',  ( -1.000000000000000000, -0.000000000000000000, -0.000000000000000000 ) ) ;
#6910 =( LENGTH_UNIT ( ) NAMED_UNIT ( * ) SI_UNIT ( .MILLI., .METRE. ) );
#6911 = ORIENTED_EDGE ( 'NONE', *, *, #42907, .T. ) ;
#6912 = CARTESIAN_POINT ( 'NONE',  ( 93.83752300881383235, -57.67474270103812728, 11.11646394693934248 ) ) ;
#6913 = CARTESIAN_POINT ( 'NONE',  ( 36.64367452218242249, 437.9806829953244574, 4.218857897681470348 ) ) ;
#6914 =( LENGTH_UNIT ( ) NAMED_UNIT ( * ) SI_UNIT ( .MILLI., .METRE. ) );
#6915 = DIRECTION ( 'NONE',  ( 0.000000000000000000, -1.000000000000000000, 0.000000000000000000 ) ) ;
#6916 = EDGE_CURVE ( 'NONE', #58722, #77575, #94222, .T. ) ;
#6917 =( GEOMETRIC_REPRESENTATION_CONTEXT ( 3 ) GLOBAL_UNCERTAINTY_ASSIGNED_CONTEXT ( ( #105595 ) ) GLOBAL_UNIT_ASSIGNED_CONTEXT ( ( #11210, #10683, #60343 ) ) REPRESENTATION_CONTEXT ( 'NONE', 'WORKASPACE' ) );
#6918 = EDGE_CURVE ( 'NONE', #50266, #77582, #74043, .T. ) ;
#6919 = CARTESIAN_POINT ( 'NONE',  ( -84.15743021832903992, -38.00000000000000000, 177.7979622954009358 ) ) ;
#6920 = CARTESIAN_POINT ( 'NONE',  ( 0.000000000000000000, -5.000000000000000000, 10.00000000000000000 ) ) ;
#6921 = LINE ( 'NONE', #71649, #80761 ) ;
#6923 = CARTESIAN_POINT ( 'NONE',  ( -11.95123837978005987, 10.78773100921685568, 9.767553402682516150 ) ) ;
#6922 = AXIS2_PLACEMENT_3D ( 'NONE', #17181, #33370, #16633 ) ;
#6924 = VERTEX_POINT ( 'NONE', #89184 ) ;
#6925 = SURFACE_STYLE_USAGE ( .BOTH. , #79228 ) ;
#6926 = CARTESIAN_POINT ( 'NONE',  ( -10.50000000000000711, -5.000000000000000000, -80.60844091781802945 ) ) ;
#6927 = CARTESIAN_POINT ( 'NONE',  ( -28.23212443805781646, 36.30340067818252692, -9.354155958373395308 ) ) ;
#6928 = CARTESIAN_POINT ( 'NONE',  ( 9.090909090909086387, 16.00000000000000000, -4.165977904505313134 ) ) ;
#6929 = SURFACE_SIDE_STYLE ('',( #7446 ) ) ;
#6930 = CARTESIAN_POINT ( 'NONE',  ( 0.000000000000000000, 0.000000000000000000, 4.000000000000000000 ) ) ;
#6931 = ORIENTED_EDGE ( 'NONE', *, *, #28199, .T. ) ;
#6932 = CARTESIAN_POINT ( 'NONE',  ( 6.169949891408690767, -4.949864754179316151, -4.426582755168344541 ) ) ;
#6933 = CARTESIAN_POINT ( 'NONE',  ( 0.01688885742776573967, 6.535341423375589542, -4.680456609903974829 ) ) ;
#6934 = CARTESIAN_POINT ( 'NONE',  ( -9.355518002030276392, -16.12908517271025133, -34.86275573499951008 ) ) ;
#6935 = ADVANCED_FACE ( 'NONE', ( #33095 ), #42321, .F. ) ;
#6937 = CARTESIAN_POINT ( 'NONE',  ( -54.57924045077913178, -60.22828080784039173, -31.12148306891128868 ) ) ;
#6936 = SURFACE_SIDE_STYLE ('',( #70626 ) ) ;
#6938 = VERTEX_POINT ( 'NONE', #76168 ) ;
#6939 = CIRCLE ( 'NONE', #62885, 4.000000000000001776 ) ;
#6940 = ORIENTED_EDGE ( 'NONE', *, *, #62106, .F. ) ;
#6941 = EDGE_CURVE ( 'NONE', #32369, #18346, #40235, .T. ) ;
#6942 = CARTESIAN_POINT ( 'NONE',  ( 10.91084845930706670, 43.80514505252456559, -13.06319618974774954 ) ) ;
#6943 = VECTOR ( 'NONE', #45505, 1000.000000000000227 ) ;
#6944 = CARTESIAN_POINT ( 'NONE',  ( 12.13034742782427955, 48.00000000000000000, -93.82352941176471006 ) ) ;
#6945 = CARTESIAN_POINT ( 'NONE',  ( -92.38040701271825128, -60.00000000000000000, 0.4176965262226800535 ) ) ;
#6946 = B_SPLINE_CURVE_WITH_KNOTS ( 'NONE', 3,
 ( #42118, #66946, #69080, #59393, #60470, #75004, #93348, #51804, #52336, #101953, #9210, #58859, #50723, #34073, #103034, #52877, #20581, #13462, #102499, #30758, #78728, #45854, #95461, #85805, #53927, #86858, #44806, #13992, #46384, #63100, #29190, #11879, #53419, #54438 ),
 .UNSPECIFIED., .F., .F.,
 ( 4, 2, 2, 2, 2, 2, 2, 2, 2, 2, 2, 2, 2, 2, 2, 2, 4 ),
 ( 0.01257177810263095975, 0.01335728547384937119, 0.01414279284506778263, 0.01492830021628619580, 0.01571380758750460724, 0.01649931495872301868, 0.01728482232994143011, 0.01807032970115984155, 0.01885583707237825299, 0.01964134444359666443, 0.02042685181481507933, 0.02121235918603348730, 0.02199786655725190221, 0.02278337392847031018, 0.02356888129968872508, 0.02435438867090713652, 0.02513989604212554796 ),
 .UNSPECIFIED. ) ;
#6947 = EDGE_LOOP ( 'NONE', ( #62730, #30411, #85038, #28426 ) ) ;
#6948 = CARTESIAN_POINT ( 'NONE',  ( 3.983571028020258975, -22.12038543825604364, -30.53674616711531087 ) ) ;
#6949 = CARTESIAN_POINT ( 'NONE',  ( -10.00000000000000178, 15.00000000000000000, 1.734723475976807489E-15 ) ) ;
#6950 = CARTESIAN_POINT ( 'NONE',  ( 96.63576135145862622, -37.72004133599708098, 192.9127721459992699 ) ) ;
#6952 = CARTESIAN_POINT ( 'NONE',  ( -47.14566430936581298, 12.03638540833422965, 16.50097935118110115 ) ) ;
#6951 = CARTESIAN_POINT ( 'NONE',  ( 0.000000000000000000, 0.000000000000000000, -9.974599999999998801 ) ) ;
#6953 = CIRCLE ( 'NONE', #32859, 4.000000000000007105 ) ;
#6954 = CARTESIAN_POINT ( 'NONE',  ( -83.05174168264076684, -36.01502199835699258, 164.7559579327255221 ) ) ;
#6955 = ORIENTED_EDGE ( 'NONE', *, *, #36004, .F. ) ;
#6956 = ORIENTED_EDGE ( 'NONE', *, *, #82391, .F. ) ;
#6957 = VERTEX_POINT ( 'NONE', #18500 ) ;
#6958 = CARTESIAN_POINT ( 'NONE',  ( 14.92208856357891911, -5.000000000000000000, -7.448748508018040226 ) ) ;
#6959 = CARTESIAN_POINT ( 'NONE',  ( -5.000000000000000000, -14.50704001784967012, 12.23934196172818289 ) ) ;
#6960 = ORIENTED_EDGE ( 'NONE', *, *, #72848, .T. ) ;
#6961 = FACE_OUTER_BOUND ( 'NONE', #13996, .T. ) ;
#6962 = CARTESIAN_POINT ( 'NONE',  ( -0.000000000000000000, 53.37899725327129374, -25.05398456423234066 ) ) ;
#6963 = DIRECTION ( 'NONE',  ( -1.000000000000000000, -0.000000000000000000, -0.000000000000000000 ) ) ;
#6964 = CARTESIAN_POINT ( 'NONE',  ( -113.3548229410037465, -57.67117998536030399, 185.4730977758015911 ) ) ;
#6965 = CARTESIAN_POINT ( 'NONE',  ( 25.59999999999999787, 3.309500000000003439, 0.000000000000000000 ) ) ;
#6966 = CARTESIAN_POINT ( 'NONE',  ( -41.61668529618729195, 48.00000000000000711, 50.19614130198706192 ) ) ;
#6967 = CARTESIAN_POINT ( 'NONE',  ( -1.012227586502681520, 25.34501299846268196, 40.25169118181511152 ) ) ;
#6968 = CARTESIAN_POINT ( 'NONE',  ( 27.33349330513380337, -4.000000000000000000, 4.898587196589415787E-16 ) ) ;
#6969 = AXIS2_PLACEMENT_3D ( 'NONE', #105752, #15678, #48567 ) ;
#6970 = CARTESIAN_POINT ( 'NONE',  ( -41.39220545275658480, -29.99999999999999289, -36.78659115423995729 ) ) ;
#6971 = CARTESIAN_POINT ( 'NONE',  ( -8.555246586836847911, -60.00000000000005684, 41.98716887921269603 ) ) ;
#6972 = CARTESIAN_POINT ( 'NONE',  ( -54.17978373078881305, -18.69462178154748244, 50.60429759934945793 ) ) ;
#6973 = MECHANICAL_DESIGN_GEOMETRIC_PRESENTATION_REPRESENTATION (  '', ( #67291 ), #20834 ) ;
#6974 = DIRECTION ( 'NONE',  ( 0.000000000000000000, 0.000000000000000000, 1.000000000000000000 ) ) ;
#6975 = EDGE_LOOP ( 'NONE', ( #24585, #60326 ) ) ;
#6976 = CARTESIAN_POINT ( 'NONE',  ( -99.94433702487522453, -52.76369124458621229, 194.2390971257265733 ) ) ;
#6977 = CARTESIAN_POINT ( 'NONE',  ( -8.557829126458644353, 294.6841484303073457, -5.194105103834561810 ) ) ;
#6978 = VERTEX_POINT ( 'NONE', #52970 ) ;
#6979 = CARTESIAN_POINT ( 'NONE',  ( -17.71939945264027116, 43.32309323114717614, 4.750313492600014342 ) ) ;
#6980 = CARTESIAN_POINT ( 'NONE',  ( 83.63364292175512560, -38.35741735095676574, -24.00537533077424968 ) ) ;
#6981 = CARTESIAN_POINT ( 'NONE',  ( 48.76802610285364636, 13.46002349908646600, 16.61772763643222106 ) ) ;
#6982 = DIRECTION ( 'NONE',  ( 0.000000000000000000, 0.000000000000000000, 1.000000000000000000 ) ) ;
#6983 = CARTESIAN_POINT ( 'NONE',  ( -0.9627149523877855941, 294.8487549629966225, 9.936351565768161365 ) ) ;
#6984 = CARTESIAN_POINT ( 'NONE',  ( 4.250000000000000000, 0.000000000000000000, -2.342872917771300578 ) ) ;
#6985 = CARTESIAN_POINT ( 'NONE',  ( 85.15477469677583144, -29.99999999999999645, 171.7644904280243452 ) ) ;
#6986 = CARTESIAN_POINT ( 'NONE',  ( -9.914196165181285991, 7.656226977557262892, -0.000000000000000000 ) ) ;
#6987 = CARTESIAN_POINT ( 'NONE',  ( 35.96015918321334226, 491.7728760210418386, 12.54260821243886248 ) ) ;
#6988 = DIRECTION ( 'NONE',  ( -0.000000000000000000, -0.000000000000000000, -1.000000000000000000 ) ) ;
#6989 = EDGE_CURVE ( 'NONE', #2280, #84655, #23636, .T. ) ;
#6990 = SURFACE_STYLE_USAGE ( .BOTH. , #91650 ) ;
#6991 =( GEOMETRIC_REPRESENTATION_CONTEXT ( 3 ) GLOBAL_UNCERTAINTY_ASSIGNED_CONTEXT ( ( #16056 ) ) GLOBAL_UNIT_ASSIGNED_CONTEXT ( ( #76106, #93902, #85273 ) ) REPRESENTATION_CONTEXT ( 'NONE', 'WORKASPACE' ) );
#6992 = EDGE_LOOP ( 'NONE', ( #96704, #15774, #68654 ) ) ;
#6993 = VERTEX_POINT ( 'NONE', #75094 ) ;
#6994 = CARTESIAN_POINT ( 'NONE',  ( 49.74300220995602473, -60.29126617275993283, 57.32551668852249094 ) ) ;
#6995 = CARTESIAN_POINT ( 'NONE',  ( 5.411617511166468830, 41.81753644224158251, -58.91471485095114247 ) ) ;
#6996 = EDGE_CURVE ( 'NONE', #68693, #40430, #97648, .T. ) ;
#6997 = CARTESIAN_POINT ( 'NONE',  ( -4.678819457397405124, 143.9212778189090045, 0.000000000000000000 ) ) ;
#6998 = ORIENTED_EDGE ( 'NONE', *, *, #10917, .T. ) ;
#6999 = CARTESIAN_POINT ( 'NONE',  ( -108.9262910262880268, -38.35648934207953431, 190.3667217115266226 ) ) ;
#7000 = ORIENTED_EDGE ( 'NONE', *, *, #62847, .T. ) ;
#7001 = CARTESIAN_POINT ( 'NONE',  ( 101.4849516909198428, -38.35588639963484781, 97.13440198566154038 ) ) ;
#7002 = CARTESIAN_POINT ( 'NONE',  ( 10.88589977545114351, 9.036462124315177036, -10.02161580976883215 ) ) ;
#7003 = CARTESIAN_POINT ( 'NONE',  ( -19.38698831337739747, 49.93019163697051965, 61.03974490994094282 ) ) ;
#7004 =( NAMED_UNIT ( * ) PLANE_ANGLE_UNIT ( ) SI_UNIT ( $, .RADIAN. ) );
#7005 = CARTESIAN_POINT ( 'NONE',  ( 102.3119119459010449, -37.84840099971084726, 161.0091571851309027 ) ) ;
#7006 = CARTESIAN_POINT ( 'NONE',  ( -32.09911992168215988, 438.9232547152093957, 23.66653216045978070 ) ) ;
#7007 = CARTESIAN_POINT ( 'NONE',  ( -28.36969756101606066, 307.4744456504976142, -9.185496674863943056 ) ) ;
#7008 = DIRECTION ( 'NONE',  ( 0.000000000000000000, 0.000000000000000000, 1.000000000000000000 ) ) ;
#7009 = CARTESIAN_POINT ( 'NONE',  ( 12.49999999999999822, -4.999999999999999112, -9.904958390907012244 ) ) ;
#7010 = CARTESIAN_POINT ( 'NONE',  ( 80.22574947771531129, -60.00000000000001421, 196.2602844723502358 ) ) ;
#7011 =( BOUNDED_CURVE ( )  B_SPLINE_CURVE ( 2, ( #14731, #49223, #41677, #65427, #97253, #32015, #106394, #64891, #81574 ),
 .UNSPECIFIED., .F., .F. ) 
 B_SPLINE_CURVE_WITH_KNOTS ( ( 3, 2, 2, 2, 3 ),
 ( 0.6029411764705883137, 0.6102941176470589868, 0.6176470588235295489, 0.6250000000000001110, 0.6323529411764706731 ),
 .UNSPECIFIED. ) 
 CURVE ( )  GEOMETRIC_REPRESENTATION_ITEM ( )  RATIONAL_B_SPLINE_CURVE ( ( 0.9999999999999988898, 0.9238795325112878487, 1.000000000000000000, 0.9238795325112867385, 1.000000000000000000, 0.9238795325112867385, 1.000000000000000000, 0.9238795325112856283, 1.000000000000001110 ) ) 
 REPRESENTATION_ITEM ( '' )  );
#7012 = CARTESIAN_POINT ( 'NONE',  ( -16.42305555460499278, 34.33297338635910023, 24.27376821836415388 ) ) ;
#7013 = COLOUR_RGB ( '', 0.66274510, 0.83137255, 0.94901961) ;
#7014 = ORIENTED_EDGE ( 'NONE', *, *, #50545, .F. ) ;
#7015 = CARTESIAN_POINT ( 'NONE',  ( 56.41533150989165080, -42.96560079021762846, 64.88708484893876971 ) ) ;
#7016 = CARTESIAN_POINT ( 'NONE',  ( -26.90859973661891402, 304.9597527792883511, -9.536681949199044439 ) ) ;
#7017 = ADVANCED_FACE ( 'NONE', ( #51363 ), #32250, .T. ) ;
#7018 = CARTESIAN_POINT ( 'NONE',  ( 15.75384615384615294, -4.171999999999999709, 0.000000000000000000 ) ) ;
#7019 = CARTESIAN_POINT ( 'NONE',  ( -7.619135598915494967, 26.82694632215321207, 2.449260492474797157 ) ) ;
#7020 = ORIENTED_EDGE ( 'NONE', *, *, #4729, .F. ) ;
#7021 = VECTOR ( 'NONE', #65313, 1000.000000000000000 ) ;
#7023 = CARTESIAN_POINT ( 'NONE',  ( -14.82123240307241296, 22.90480191141017485, -2.008241678658511997 ) ) ;
#7022 = CARTESIAN_POINT ( 'NONE',  ( -108.2151194096256006, -38.35755553628541747, 192.4188466880123656 ) ) ;
#7024 = LINE ( 'NONE', #39941, #25427 ) ;
#7025 = CARTESIAN_POINT ( 'NONE',  ( 30.63851678811156631, 340.2470915159922811, 17.36724565301306811 ) ) ;
#7026 = DIRECTION ( 'NONE',  ( 0.000000000000000000, 1.000000000000000000, -1.224646799147353207E-16 ) ) ;
#7027 = CARTESIAN_POINT ( 'NONE',  ( -8.000000000000001776, -34.15624999999999289, 3.313708498984758943 ) ) ;
#7028 = CARTESIAN_POINT ( 'NONE',  ( -17.49999999999996803, 45.90000000000000568, 64.09953197957064219 ) ) ;
#7029 = AXIS2_PLACEMENT_3D ( 'NONE', #87377, #38310, #36736 ) ;
#7030 = AXIS2_PLACEMENT_3D ( 'NONE', #41526, #57169, #105210 ) ;
#7031 = ADVANCED_FACE ( 'NONE', ( #35768 ), #54609, .T. ) ;
#7032 = CARTESIAN_POINT ( 'NONE',  ( 55.59873597034290071, 48.00000000000000711, -34.06437516161191326 ) ) ;
#7033 = ORIENTED_EDGE ( 'NONE', *, *, #73524, .F. ) ;
#7034 = CARTESIAN_POINT ( 'NONE',  ( 86.10674275497149210, -18.36954599775684827, 167.2017617639139360 ) ) ;
#7035 = CARTESIAN_POINT ( 'NONE',  ( 0.000000000000000000, 0.000000000000000000, 0.000000000000000000 ) ) ;
#7036 = CARTESIAN_POINT ( 'NONE',  ( -37.72381677393462240, 438.6275846837065728, 23.63981362230112282 ) ) ;
#7037 = EDGE_LOOP ( 'NONE', ( #38228, #93247, #73189, #106362, #44468 ) ) ;
#7038 = CARTESIAN_POINT ( 'NONE',  ( 105.5353273971932140, 1.030564683017419500E-14, 0.000000000000000000 ) ) ;
#7039 = CARTESIAN_POINT ( 'NONE',  ( 7.499997280422757484, -2.963001255694796665, -20.99866594763298266 ) ) ;
#7040 = FACE_OUTER_BOUND ( 'NONE', #93887, .T. ) ;
#7041 = CARTESIAN_POINT ( 'NONE',  ( 14.91461412207629422, 1.322532983912315885, -1.774597446655453048 ) ) ;
#7042 = CARTESIAN_POINT ( 'NONE',  ( 0.000000000000000000, 6.123233995736770227E-16, -5.000000000000002665 ) ) ;
#7043 = CARTESIAN_POINT ( 'NONE',  ( -29.35352825446822678, 8.824359840618493322, -42.06917583815513240 ) ) ;
#7044 = EDGE_CURVE ( 'NONE', #52941, #21651, #84274, .T. ) ;
#7045 = ORIENTED_EDGE ( 'NONE', *, *, #45975, .F. ) ;
#7046 = CIRCLE ( 'NONE', #105225, 1.000000000000000444 ) ;
#7047 = CARTESIAN_POINT ( 'NONE',  ( 6.500000000000600409, 0.6542365398605715088, -6.055391205187021342 ) ) ;
#7048 = CARTESIAN_POINT ( 'NONE',  ( -4.175533140205450522, -48.44478104465395774, 102.9090322054120890 ) ) ;
#7050 = CARTESIAN_POINT ( 'NONE',  ( -13.94870603575048129, 6.950772033844307529, -7.980207832019492464 ) ) ;
#7049 = CARTESIAN_POINT ( 'NONE',  ( 7.500000000000005329, 40.28748004600710431, -68.91429205818927528 ) ) ;
#7051 = CARTESIAN_POINT ( 'NONE',  ( -7.188101187500001821, -14.00000000204838457, -2.977408999572651371 ) ) ;
#7052 = CARTESIAN_POINT ( 'NONE',  ( 20.49977525862255590, 302.8459220885798686, -10.00124997875689203 ) ) ;
#7053 = DIRECTION ( 'NONE',  ( -0.000000000000000000, 1.000000000000000000, -0.000000000000000000 ) ) ;
#7054 = VERTEX_POINT ( 'NONE', #61075 ) ;
#7055 = CARTESIAN_POINT ( 'NONE',  ( -18.91772294278450772, 48.00000000000000000, 62.18609455171461065 ) ) ;
#7056 = CARTESIAN_POINT ( 'NONE',  ( -4.000000000000000000, 0.000000000000000000, -2.296599999999999753 ) ) ;
#7057 = CARTESIAN_POINT ( 'NONE',  ( -7.939742226420592353, 97.07168777242631563, -5.080791182465135870E-12 ) ) ;
#7058 = CARTESIAN_POINT ( 'NONE',  ( -5.096247963242958257, -4.999999999999998224, -73.00359695307524532 ) ) ;
#7059 = EDGE_CURVE ( 'NONE', #26216, #48231, #14972, .T. ) ;
#7060 = CARTESIAN_POINT ( 'NONE',  ( -14.46400437353393009, 2.949852469129314869, 3.921916857617072871 ) ) ;
#7061 = VECTOR ( 'NONE', #10181, 1000.000000000000341 ) ;
#7062 = ORIENTED_EDGE ( 'NONE', *, *, #21567, .F. ) ;
#7063 = CARTESIAN_POINT ( 'NONE',  ( 44.26141237093871439, 435.3133447328257830, 11.28309783997975480 ) ) ;
#7064 = CARTESIAN_POINT ( 'NONE',  ( 26.08349330513380337, -4.000000000000000888, 4.898587196589416773E-16 ) ) ;
#7065 = ORIENTED_EDGE ( 'NONE', *, *, #89884, .F. ) ;
#7066 = EDGE_CURVE ( 'NONE', #27686, #93080, #32641, .T. ) ;
#7067 = ADVANCED_FACE ( 'NONE', ( #34696 ), #2269, .F. ) ;
#7068 = CARTESIAN_POINT ( 'NONE',  ( 23.09999999999999432, 1.533819458162526451E-15, 0.000000000000000000 ) ) ;
#7069 = DIRECTION ( 'NONE',  ( 1.000000000000000000, 0.000000000000000000, 0.000000000000000000 ) ) ;
#7070 = CARTESIAN_POINT ( 'NONE',  ( -3.352941176470589646, -48.79941684889505638, 104.5794940929807524 ) ) ;
#7071 = UNCERTAINTY_MEASURE_WITH_UNIT (LENGTH_MEASURE( 1.000000000000000082E-05 ), #3639, 'distance_accuracy_value', 'NONE');
#7072 = CARTESIAN_POINT ( 'NONE',  ( -110.1353205782709495, -60.00000000000000711, 144.5369955810122065 ) ) ;
#7073 = CARTESIAN_POINT ( 'NONE',  ( 29.68315524076925982, 18.29184282782464166, -39.60535821593530414 ) ) ;
#7074 = CARTESIAN_POINT ( 'NONE',  ( -14.88296169672398328, 41.91403674972022486, -82.91973998541202207 ) ) ;
#7075 = DIRECTION ( 'NONE',  ( -0.000000000000000000, -1.000000000000000000, -0.000000000000000000 ) ) ;
#7076 = DIRECTION ( 'NONE',  ( 0.9167413600884036784, 0.000000000000000000, -0.3994812620177121132 ) ) ;
#7078 = CARTESIAN_POINT ( 'NONE',  ( 37.67992928262796681, 491.6871197847727899, 12.48602433195153161 ) ) ;
#7077 = CARTESIAN_POINT ( 'NONE',  ( 10.48543666094731996, -5.000000000000002665, -78.95657223723277696 ) ) ;
#7079 = CARTESIAN_POINT ( 'NONE',  ( -81.01496773232567250, -60.51907568041632146, 183.3200419029122941 ) ) ;
#7080 = EDGE_LOOP ( 'NONE', ( #105309, #27562, #18052 ) ) ;
#7081 = STYLED_ITEM ( 'NONE', ( #92364 ), #7853 ) ;
#7083 = EDGE_CURVE ( 'NONE', #16331, #62158, #81478, .T. ) ;
#7082 = CIRCLE ( 'NONE', #79385, 4.000000000000000000 ) ;
#7084 = VERTEX_POINT ( 'NONE', #98064 ) ;
#7085 = AXIS2_PLACEMENT_3D ( 'NONE', #82101, #56759, #31993 ) ;
#7086 = EDGE_LOOP ( 'NONE', ( #2788, #40416, #106431 ) ) ;
#7087 = CARTESIAN_POINT ( 'NONE',  ( 38.86638200451619696, 1.340359594676612611E-15, 0.000000000000000000 ) ) ;
#7088 = CARTESIAN_POINT ( 'NONE',  ( 32.85155332502864667, 463.8111683108725174, 7.359358840565818127 ) ) ;
#7089 = CIRCLE ( 'NONE', #43292, 4.000000000000001776 ) ;
#7090 = CARTESIAN_POINT ( 'NONE',  ( 30.00000000000000000, 461.8887775513396150, 11.55279652844105698 ) ) ;
#7091 = DIRECTION ( 'NONE',  ( 0.000000000000000000, 0.000000000000000000, 1.000000000000000000 ) ) ;
#7092 = CARTESIAN_POINT ( 'NONE',  ( -32.87547266101557852, 465.6993878536674742, 10.91512469976539279 ) ) ;
#7093 = CARTESIAN_POINT ( 'NONE',  ( 106.8235258757864869, -14.21045842199432307, 178.1026719309843429 ) ) ;
#7094 = PRESENTATION_LAYER_ASSIGNMENT (  '', '', ( #58792 ) ) ;
#7095 = CARTESIAN_POINT ( 'NONE',  ( -106.2142031390243488, -14.21045842199427867, 184.2056779555663582 ) ) ;
#7096 = CARTESIAN_POINT ( 'NONE',  ( -62.91815421806131070, -46.43920947130374799, 83.70092769440094571 ) ) ;
#7097 = VERTEX_POINT ( 'NONE', #15552 ) ;
#7098 = CARTESIAN_POINT ( 'NONE',  ( 0.3167204509598381956, 8.479269695850865318, -1.313474075707212974 ) ) ;
#7099 = CARTESIAN_POINT ( 'NONE',  ( 102.1655696349906037, -59.99999999999998579, 79.68160258763181503 ) ) ;
#7100 = ORIENTED_EDGE ( 'NONE', *, *, #18382, .F. ) ;
#7101 = CARTESIAN_POINT ( 'NONE',  ( 2.047183246720497340, -56.87785484247199719, 33.36663002190862670 ) ) ;
#7102 = CARTESIAN_POINT ( 'NONE',  ( 7.188101187500000933, -11.93750000204838635, -2.977408999572650483 ) ) ;
#7103 = DIRECTION ( 'NONE',  ( 0.000000000000000000, -1.000000000000000000, 0.000000000000000000 ) ) ;
#7104 = ORIENTED_EDGE ( 'NONE', *, *, #81782, .F. ) ;
#7105 = B_SPLINE_CURVE_WITH_KNOTS ( 'NONE', 3,
 ( #47436, #45864, #63654, #39376 ),
 .UNSPECIFIED., .F., .F.,
 ( 4, 4 ),
 ( 0.0008676662333014916340, 0.02106922348384824423 ),
 .UNSPECIFIED. ) ;
#7106 = CARTESIAN_POINT ( 'NONE',  ( 83.28888888888889142, -4.171999999999998820, 5.616230220889773285E-16 ) ) ;
#7107 = ORIENTED_EDGE ( 'NONE', *, *, #71450, .T. ) ;
#7108 = CARTESIAN_POINT ( 'NONE',  ( 11.36508313652854163, 45.70357710343880342, -13.50657646266327383 ) ) ;
#7109 = CARTESIAN_POINT ( 'NONE',  ( -111.3575414531999002, -60.00000000000002132, 155.6755428621777639 ) ) ;
#7110 = CARTESIAN_POINT ( 'NONE',  ( 9.728280252476675827, -57.17794266280819926, 24.67413300948206967 ) ) ;
#7111 = CARTESIAN_POINT ( 'NONE',  ( 7.188101187500001821, -26.93750000204838457, -2.977408999572650483 ) ) ;
#7112 = CARTESIAN_POINT ( 'NONE',  ( 45.99999999997967848, 463.5320417905273302, 9.382446278464357192 ) ) ;
#7113 = CARTESIAN_POINT ( 'NONE',  ( -12.45419940525628988, 18.15241938591149662, 8.579672614547556364 ) ) ;
#7114 = CARTESIAN_POINT ( 'NONE',  ( 13.50000000000000533, 0.6589394956329788222, -13.00000000000000000 ) ) ;
#7115 = CARTESIAN_POINT ( 'NONE',  ( 15.26274976730916499, -5.960238452850545876, 13.77689897405315200 ) ) ;
#7116 = DIRECTION ( 'NONE',  ( -1.000000000000000000, -1.224606353822377258E-16, -0.000000000000000000 ) ) ;
#7117 = EDGE_CURVE ( 'NONE', #33657, #42175, #71877, .T. ) ;
#7118 = CARTESIAN_POINT ( 'NONE',  ( 35.80004365250785980, 328.0257370263789767, -3.832668609434584095 ) ) ;
#7119 = CARTESIAN_POINT ( 'NONE',  ( -33.16678848657432610, -39.49658583418889890, 34.42063352927269193 ) ) ;
#7120 = STYLED_ITEM ( 'NONE', ( #14905 ), #105482 ) ;
#7121 =( NAMED_UNIT ( * ) PLANE_ANGLE_UNIT ( ) SI_UNIT ( $, .RADIAN. ) );
#7122 = CARTESIAN_POINT ( 'NONE',  ( 38.10111135957357220, -39.51109722829941973, 37.25237634264367159 ) ) ;
#7123 = MECHANICAL_DESIGN_GEOMETRIC_PRESENTATION_REPRESENTATION (  '', ( #72574 ), #65725 ) ;
#7124 = CARTESIAN_POINT ( 'NONE',  ( -13.60704923275180711, -1.734723475976807094E-15, 10.45706415777857679 ) ) ;
#7125 = VERTEX_POINT ( 'NONE', #106140 ) ;
#7126 = EDGE_CURVE ( 'NONE', #51961, #69383, #99452, .T. ) ;
#7127 = EDGE_CURVE ( 'NONE', #8257, #60803, #80276, .T. ) ;
#7128 = CARTESIAN_POINT ( 'NONE',  ( 33.33807306180359831, 464.2324349908041654, 17.97546588399033141 ) ) ;
#7129 = MECHANICAL_DESIGN_GEOMETRIC_PRESENTATION_REPRESENTATION (  '', ( #14053 ), #41633 ) ;
#7130 = CARTESIAN_POINT ( 'NONE',  ( -73.92879853447317373, -38.32663868724161915, 159.7524117896638529 ) ) ;
#7131 = ORIENTED_EDGE ( 'NONE', *, *, #24281, .T. ) ;
#7133 = CARTESIAN_POINT ( 'NONE',  ( 33.56345473223404241, 299.9083031499212666, -8.874823776838020706 ) ) ;
#7132 = CARTESIAN_POINT ( 'NONE',  ( 20.77592568779148863, 6.123233995736772199E-16, -5.000000000000001776 ) ) ;
#7134 = DIRECTION ( 'NONE',  ( 0.9135154255858337624, 0.3026456445970197029, 0.2718366807904842863 ) ) ;
#7135 = CARTESIAN_POINT ( 'NONE',  ( -43.51084452654406221, 465.2903130129679994, 9.421687747986709383 ) ) ;
#7136 = CARTESIAN_POINT ( 'NONE',  ( 0.3381961372621271056, 43.18747244270107188, -18.71485033559731548 ) ) ;
#7137 = CARTESIAN_POINT ( 'NONE',  ( -37.88481199253353537, 25.64605156355563054, 10.95617127781058997 ) ) ;
#7138 = CARTESIAN_POINT ( 'NONE',  ( -30.86777479908530708, 345.9147241694792001, 18.50750428929681490 ) ) ;
#7139 = CARTESIAN_POINT ( 'NONE',  ( 37.56673239365841255, 25.47613764497371136, -13.45617127781092215 ) ) ;
#7140 = CARTESIAN_POINT ( 'NONE',  ( 96.40273327088657140, -60.00000000000000711, 58.78147464121637711 ) ) ;
#7141 = DIRECTION ( 'NONE',  ( 0.000000000000000000, -1.000000000000000000, 0.000000000000000000 ) ) ;
#7142 = FACE_BOUND ( 'NONE', #92578, .T. ) ;
#7143 = ORIENTED_EDGE ( 'NONE', *, *, #91024, .T. ) ;
#7144 = EDGE_CURVE ( 'NONE', #64475, #3854, #25408, .T. ) ;
#7145 = CARTESIAN_POINT ( 'NONE',  ( -93.63610435622004502, -29.99999999996020605, 58.27751359658407182 ) ) ;
#7146 = ORIENTED_EDGE ( 'NONE', *, *, #64988, .T. ) ;
#7147 = CARTESIAN_POINT ( 'NONE',  ( 0.000000000000000000, 1.500000000000000888, 0.000000000000000000 ) ) ;
#7148 = CARTESIAN_POINT ( 'NONE',  ( -16.03930365250128176, 4.449877915869574707, -3.144092084174250346 ) ) ;
#7149 = CARTESIAN_POINT ( 'NONE',  ( 3.768804542112334399, 19.36671096900046152, 5.000000000000000000 ) ) ;
#7150 = DIRECTION ( 'NONE',  ( 0.000000000000000000, 0.000000000000000000, 1.000000000000000000 ) ) ;
#7151 = CARTESIAN_POINT ( 'NONE',  ( 9.536842176398144133, 27.35764630116009855, 3.014135744008177298 ) ) ;
#7152 = CARTESIAN_POINT ( 'NONE',  ( 2.977408999572650927, -28.25000000204838813, -7.188101187500001821 ) ) ;
#7153 = PLANE ( 'NONE',  #93258 ) ;
#7154 =( NAMED_UNIT ( * ) PLANE_ANGLE_UNIT ( ) SI_UNIT ( $, .RADIAN. ) );
#7155 = CARTESIAN_POINT ( 'NONE',  ( 7.096116585776479191, 40.56175638390114813, -70.95279415343941309 ) ) ;
#7156 = ORIENTED_EDGE ( 'NONE', *, *, #51668, .T. ) ;
#7158 = ORIENTED_EDGE ( 'NONE', *, *, #85792, .T. ) ;
#7157 = LINE ( 'NONE', #105856, #20275 ) ;
#7159 = CARTESIAN_POINT ( 'NONE',  ( 79.83490250164462054, -46.43441910742400580, 152.6729557515090221 ) ) ;
#7160 = CARTESIAN_POINT ( 'NONE',  ( -38.69367500482761812, 27.29977269400058049, -12.75349522650845202 ) ) ;
#7161 = VERTEX_POINT ( 'NONE', #4414 ) ;
#7162 = CIRCLE ( 'NONE', #48429, 62.00000000000000000 ) ;
#7163 = CARTESIAN_POINT ( 'NONE',  ( -59.16624074119484078, 50.00000000000000000, 21.79082393248474503 ) ) ;
#7164 = CARTESIAN_POINT ( 'NONE',  ( -14.91461412207421411, 1.322532983914281868, 1.774597446674108792 ) ) ;
#7165 = CARTESIAN_POINT ( 'NONE',  ( -5.082755093536325042, -14.09375000204838457, -5.082755093536325930 ) ) ;
#7166 = CARTESIAN_POINT ( 'NONE',  ( 7.800703710507055355, 26.41404307342058644, 1.791736796405272170 ) ) ;
#7167 = CIRCLE ( 'NONE', #81217, 4.000000000000000888 ) ;
#7168 = CARTESIAN_POINT ( 'NONE',  ( -18.14395573440383203, -57.67158919250769600, 41.98617601139094546 ) ) ;
#7169 = CARTESIAN_POINT ( 'NONE',  ( 10.24586172992462707, 302.6397306569780312, 9.891919218941357173 ) ) ;
#7170 = ORIENTED_EDGE ( 'NONE', *, *, #36957, .T. ) ;
#7171 = FACE_OUTER_BOUND ( 'NONE', #21911, .T. ) ;
#7173 = CARTESIAN_POINT ( 'NONE',  ( 3.363233428609793130, 121.3096164343346999, 4.999999999999998224 ) ) ;
#7172 = TOROIDAL_SURFACE ( 'NONE', #55443, 59.50000000000000000, 0.5000000000000000000 ) ;
#7174 = CARTESIAN_POINT ( 'NONE',  ( 7.425374080001780008, 41.07993796427307842, -59.67056350572800483 ) ) ;
#7175 = CIRCLE ( 'NONE', #82946, 5.000000000000002665 ) ;
#7176 = FACE_OUTER_BOUND ( 'NONE', #86838, .T. ) ;
#7177 = ORIENTED_EDGE ( 'NONE', *, *, #54153, .F. ) ;
#7178 = CARTESIAN_POINT ( 'NONE',  ( 8.000000000000000000, -14.18750000409677092, 0.000000000000000000 ) ) ;
#7179 = CARTESIAN_POINT ( 'NONE',  ( -19.56313861856585135, -16.92226382200795953, 31.48483935735937322 ) ) ;
#7180 = CARTESIAN_POINT ( 'NONE',  ( -38.67559328634845173, 490.7810811343264845, 11.84720182290557844 ) ) ;
#7181 = CARTESIAN_POINT ( 'NONE',  ( 0.4143732981959021844, 52.15072962189677952, -7.817691439387481012 ) ) ;
#7182 = PLANE ( 'NONE',  #79725 ) ;
#7183 = CARTESIAN_POINT ( 'NONE',  ( 33.50629336895840282, 439.8577465421020065, 24.25469227980369524 ) ) ;
#7184 = APPLICATION_PROTOCOL_DEFINITION ( 'draft international standard', 'automotive_design', 1998, #61797 ) ;
#7185 = CARTESIAN_POINT ( 'NONE',  ( -10.51914831753094148, -11.53309007499742478, 17.75417121042075053 ) ) ;
#7186 = ORIENTED_EDGE ( 'NONE', *, *, #46079, .F. ) ;
#7187 = CARTESIAN_POINT ( 'NONE',  ( -4.572719631913240157, -47.86564882870907667, 40.42917486031264929 ) ) ;
#7188 = CARTESIAN_POINT ( 'NONE',  ( -3.836411046841926797, 15.00000000000001066, 9.999999999999959144 ) ) ;
#7189 = DIRECTION ( 'NONE',  ( -1.000000000000000000, -1.224606353822377258E-16, -0.000000000000000000 ) ) ;
#7190 = CARTESIAN_POINT ( 'NONE',  ( 40.56629821760718357, -33.14137426171819811, -37.41307075545274330 ) ) ;
#7191 = CARTESIAN_POINT ( 'NONE',  ( 60.63333333333333286, 6.915964383211875250E-15, 0.000000000000000000 ) ) ;
#7192 = DIRECTION ( 'NONE',  ( 0.000000000000000000, 0.000000000000000000, 1.000000000000000000 ) ) ;
#7193 = EDGE_CURVE ( 'NONE', #84992, #101817, #102152, .T. ) ;
#7194 = VECTOR ( 'NONE', #72759, 1000.000000000000000 ) ;
#7195 = ORIENTED_EDGE ( 'NONE', *, *, #55288, .T. ) ;
#7196 = CARTESIAN_POINT ( 'NONE',  ( -43.00000000000000000, 436.0987441542287115, 7.567257455462727656 ) ) ;
#7197 = CARTESIAN_POINT ( 'NONE',  ( 101.5234275403970230, -57.63077336659093675, 203.4510901792717448 ) ) ;
#7198 = VECTOR ( 'NONE', #74642, 1000.000000000000000 ) ;
#7199 = EDGE_CURVE ( 'NONE', #4657, #54111, #64949, .T. ) ;
#7200 = EDGE_CURVE ( 'NONE', #77985, #38642, #44323, .T. ) ;
#7201 = EDGE_CURVE ( 'NONE', #47934, #88346, #51149, .T. ) ;
#7202 = CARTESIAN_POINT ( 'NONE',  ( 35.63058582596927693, 464.1921406587381966, 19.33089630041451201 ) ) ;
#7203 = COLOUR_RGB ( '', 0.40784314, 0.44705882, 0.49803922) ;
#7204 = CARTESIAN_POINT ( 'NONE',  ( -9.324472166507712600, 51.33783191909205357, -3.783589396988578102 ) ) ;
#7205 = CARTESIAN_POINT ( 'NONE',  ( -6.465258847094798256, 53.70062699890282687, 6.847807190413986334 ) ) ;
#7206 = CARTESIAN_POINT ( 'NONE',  ( -74.29762348972462860, -60.00000000000000711, 175.1860712289616799 ) ) ;
#7207 = ADVANCED_FACE ( 'NONE', ( #2020 ), #34968, .T. ) ;
#7208 = CARTESIAN_POINT ( 'NONE',  ( -7.000000000000000000, 8.572527594031471218E-16, -8.574621033218877031 ) ) ;
#7209 = CARTESIAN_POINT ( 'NONE',  ( -39.84233570596349949, 333.3323931548420660, 19.23895789620553032 ) ) ;
#7210 = CARTESIAN_POINT ( 'NONE',  ( -84.86190328036930453, -42.95973281295992763, 185.2921246785317635 ) ) ;
#7211 = ORIENTED_EDGE ( 'NONE', *, *, #13896, .T. ) ;
#7212 = CARTESIAN_POINT ( 'NONE',  ( 29.86158665938207335, 311.4578868317084925, -8.460588905613484201 ) ) ;
#7213 = EDGE_CURVE ( 'NONE', #64079, #21657, #9046, .T. ) ;
#7214 = ORIENTED_EDGE ( 'NONE', *, *, #82612, .T. ) ;
#7215 = CARTESIAN_POINT ( 'NONE',  ( -6.943926999490789065, -10.53300992626148869, -3.973092371898544251 ) ) ;
#7216 = SURFACE_STYLE_FILL_AREA ( #73000 ) ;
#7217 = CARTESIAN_POINT ( 'NONE',  ( -83.26222442445862271, -45.25913346788161817, -13.97201566420315366 ) ) ;
#7218 = DIRECTION ( 'NONE',  ( 0.000000000000000000, 0.000000000000000000, 1.000000000000000000 ) ) ;
#7219 = DIRECTION ( 'NONE',  ( -1.000000000000000000, -0.000000000000000000, -0.000000000000000000 ) ) ;
#7220 = ORIENTED_EDGE ( 'NONE', *, *, #64286, .F. ) ;
#7221 = CARTESIAN_POINT ( 'NONE',  ( 55.26095113931063452, 4.000000000000015099, 4.898587196589422689E-16 ) ) ;
#7222 = CARTESIAN_POINT ( 'NONE',  ( 19.43146043914768129, -2.896176105056903703E-12, 11.19959342721819695 ) ) ;
#7223 = DIRECTION ( 'NONE',  ( -1.000000000000000000, -1.224606353822377258E-16, -0.000000000000000000 ) ) ;
#7224 = CARTESIAN_POINT ( 'NONE',  ( 90.14752496014264693, -29.99999999999995026, -6.310861463900848456 ) ) ;
#7225 = CARTESIAN_POINT ( 'NONE',  ( -77.90030443299963281, -29.08352689348323850, 125.1943772946299589 ) ) ;
#7226 = ORIENTED_EDGE ( 'NONE', *, *, #10243, .F. ) ;
#7227 = CARTESIAN_POINT ( 'NONE',  ( 20.43634719630433594, -14.21045842199429998, 34.90381869870211062 ) ) ;
#7228 = DIRECTION ( 'NONE',  ( 0.000000000000000000, 0.000000000000000000, 1.000000000000000000 ) ) ;
#7229 = CARTESIAN_POINT ( 'NONE',  ( 70.47149586861833370, -57.68248580236559064, 157.7590444366918803 ) ) ;
#7230 = DIRECTION ( 'NONE',  ( 0.000000000000000000, -1.000000000000000000, 0.000000000000000000 ) ) ;
#7231 = CARTESIAN_POINT ( 'NONE',  ( 40.52582510012484107, 311.5116601731387505, -6.047907428142603514 ) ) ;
#7232 = LINE ( 'NONE', #80590, #75225 ) ;
#7233 = ORIENTED_EDGE ( 'NONE', *, *, #6384, .T. ) ;
#7234 = LINE ( 'NONE', #29961, #16499 ) ;
#7235 = AXIS2_PLACEMENT_3D ( 'NONE', #17943, #68629, #67021 ) ;
#7236 = DIRECTION ( 'NONE',  ( -0.000000000000000000, 1.000000000000000000, -0.000000000000000000 ) ) ;
#7237 = FACE_BOUND ( 'NONE', #63202, .T. ) ;
#7238 = CARTESIAN_POINT ( 'NONE',  ( -5.082755093536326818, -21.21875000204838457, 5.082755093536325042 ) ) ;
#7239 = AXIS2_PLACEMENT_3D ( 'NONE', #25810, #68892, #59199 ) ;
#7240 = CARTESIAN_POINT ( 'NONE',  ( 9.536842176398147686, 82.35764630116013052, 3.014135744008184847 ) ) ;
#7241 = CARTESIAN_POINT ( 'NONE',  ( 0.000000000000000000, 0.000000000000000000, 0.000000000000000000 ) ) ;
#7242 = CARTESIAN_POINT ( 'NONE',  ( -7.500000000000000000, 1.644753667992016055, -7.029983668656049289 ) ) ;
#7243 = ADVANCED_FACE ( 'NONE', ( #74316 ), #78710, .T. ) ;
#7244 = VERTEX_POINT ( 'NONE', #26883 ) ;
#7245 = CARTESIAN_POINT ( 'NONE',  ( 43.97702309827923983, 485.9235625652956969, 4.765750180331959740 ) ) ;
#7246 = CIRCLE ( 'NONE', #102031, 10.00000000000000178 ) ;
#7248 = CARTESIAN_POINT ( 'NONE',  ( 30.40514414639649132, -39.48589796098298876, 33.27119446255795054 ) ) ;
#7247 = CARTESIAN_POINT ( 'NONE',  ( -1.425880015568740777, -60.00000000000000711, 42.00000000000002132 ) ) ;
#7249 = CARTESIAN_POINT ( 'NONE',  ( -4.331568300327791832, 52.16491803293271801, -6.474400360773702623 ) ) ;
#7250 = ORIENTED_EDGE ( 'NONE', *, *, #6181, .T. ) ;
#7251 = EDGE_CURVE ( 'NONE', #27394, #41040, #33766, .T. ) ;
#7252 = AXIS2_PLACEMENT_3D ( 'NONE', #32155, #39188, #72066 ) ;
#7253 = VERTEX_POINT ( 'NONE', #82419 ) ;
#7255 = CARTESIAN_POINT ( 'NONE',  ( 0.3383419327415344013, 51.28045727062713866, 10.21496599268967387 ) ) ;
#7254 = DIRECTION ( 'NONE',  ( 0.000000000000000000, -1.000000000000000000, 0.000000000000000000 ) ) ;
#7256 = CARTESIAN_POINT ( 'NONE',  ( -15.43387005369899256, 294.5569523601460560, -10.06267239232150068 ) ) ;
#7257 = CARTESIAN_POINT ( 'NONE',  ( -16.75187969033531132, 34.25544727262101219, -24.30698433968676753 ) ) ;
#7258 = CARTESIAN_POINT ( 'NONE',  ( 32.03420920423157270, 464.8550977446587922, 13.91744750517720952 ) ) ;
#7259 = CARTESIAN_POINT ( 'NONE',  ( 0.000000000000000000, 0.000000000000000000, 1.734723475976807094E-15 ) ) ;
#7260 = ORIENTED_EDGE ( 'NONE', *, *, #92514, .F. ) ;
#7261 = CARTESIAN_POINT ( 'NONE',  ( 63.78324300990938411, -60.00000000000002842, -34.57572711317787650 ) ) ;
#7262 = CARTESIAN_POINT ( 'NONE',  ( 84.85176311637069091, -30.00000000000000711, 168.9139284579673301 ) ) ;
#7263 = CARTESIAN_POINT ( 'NONE',  ( -33.07276483573667747, 438.9325140356154975, 23.89537236861306013 ) ) ;
#7264 = CARTESIAN_POINT ( 'NONE',  ( 75.38474497803707663, -29.99999999999999645, -17.81191432453914913 ) ) ;
#7265 = CARTESIAN_POINT ( 'NONE',  ( 47.44718022415288772, 11.18620753528884748, -16.71882890723522053 ) ) ;
#7266 = ORIENTED_EDGE ( 'NONE', *, *, #92792, .T. ) ;
#7267 = CIRCLE ( 'NONE', #29728, 5.000000000000011546 ) ;
#7268 = ORIENTED_EDGE ( 'NONE', *, *, #105739, .T. ) ;
#7269 = EDGE_LOOP ( 'NONE', ( #58893, #51042 ) ) ;
#7270 = CYLINDRICAL_SURFACE ( 'NONE', #58967, 4.000000000000000000 ) ;
#7271 = FILL_AREA_STYLE ('',( #65529 ) ) ;
#7272 = LINE ( 'NONE', #32658, #40148 ) ;
#7273 = DIRECTION ( 'NONE',  ( 1.000000000000000000, -0.000000000000000000, -0.000000000000000000 ) ) ;
#7274 = PRESENTATION_LAYER_ASSIGNMENT (  '', '', ( #2111 ) ) ;
#7275 = CARTESIAN_POINT ( 'NONE',  ( -45.29202373334744181, 362.1633252469901549, 4.985022154565413643 ) ) ;
#7276 = CARTESIAN_POINT ( 'NONE',  ( -4.458592195379179834, -66.17896604625831003, 13.13601379408565961 ) ) ;
#7277 = DIRECTION ( 'NONE',  ( 0.000000000000000000, -1.000000000000000000, 0.000000000000000000 ) ) ;
#7278 = CARTESIAN_POINT ( 'NONE',  ( 0.000000000000000000, 7.511572993685796142E-16, -6.500000000000000888 ) ) ;
#7279 = ORIENTED_EDGE ( 'NONE', *, *, #44473, .F. ) ;
#7280 = EDGE_CURVE ( 'NONE', #71976, #78701, #27296, .T. ) ;
#7281 = CARTESIAN_POINT ( 'NONE',  ( 29.85247340496056268, 12.86254483752417954, 39.61457847635354312 ) ) ;
#7282 = AXIS2_PLACEMENT_3D ( 'NONE', #31912, #12, #6012 ) ;
#7283 = ORIENTED_EDGE ( 'NONE', *, *, #96603, .F. ) ;
#7284 = CARTESIAN_POINT ( 'NONE',  ( 50.94745919686198476, 50.00000000000000000, -37.05882352941176094 ) ) ;
#7285 = CARTESIAN_POINT ( 'NONE',  ( 18.41162169223098033, 304.6294254666754568, 9.889731659030220001 ) ) ;
#7286 = SURFACE_STYLE_USAGE ( .BOTH. , #72562 ) ;
#7287 = EDGE_CURVE ( 'NONE', #56205, #86892, #59558, .T. ) ;
#7288 = CARTESIAN_POINT ( 'NONE',  ( -20.84632109279829493, -59.99999999999998579, 34.49850619988961142 ) ) ;
#7289 = CARTESIAN_POINT ( 'NONE',  ( 67.76856916487194837, -32.53299590129649488, 90.77966141860517268 ) ) ;
#7290 = ORIENTED_EDGE ( 'NONE', *, *, #1980, .F. ) ;
#7291 = CARTESIAN_POINT ( 'NONE',  ( 39.01446284274602760, 463.6644110202811362, 19.39997085980421687 ) ) ;
#7292 = CARTESIAN_POINT ( 'NONE',  ( -32.85155332502864667, 463.8111683108725174, 7.359358840565846549 ) ) ;
#7293 = CARTESIAN_POINT ( 'NONE',  ( 4.000000000000000000, 4.898587196589412829E-16, -0.02540000000000007530 ) ) ;
#7294 = EDGE_LOOP ( 'NONE', ( #85658, #92876, #22062, #11630, #39143, #60502 ) ) ;
#7295 =( LENGTH_UNIT ( ) NAMED_UNIT ( * ) SI_UNIT ( .MILLI., .METRE. ) );
#7296 = CARTESIAN_POINT ( 'NONE',  ( 47.90443661882645898, 17.06459462766588331, 14.35535821593427386 ) ) ;
#7297 = CARTESIAN_POINT ( 'NONE',  ( -35.15824258293415028, 491.5080798214892752, 12.36499586378574733 ) ) ;
#7298 = CARTESIAN_POINT ( 'NONE',  ( -3.313708498984765161, -29.65625000409676915, 7.999999999999998224 ) ) ;
#7299 = CARTESIAN_POINT ( 'NONE',  ( -10.00000000000000000, -5.000000000000000000, -2.617993873628155832 ) ) ;
#7300 = CARTESIAN_POINT ( 'NONE',  ( 33.84761347220318584, 488.7471039746334895, 11.01988148152525504 ) ) ;
#7301 = CIRCLE ( 'NONE', #19458, 5.000000000000001776 ) ;
#7302 = CARTESIAN_POINT ( 'NONE',  ( 9.918512371096300129, 33.79282992270550068, -1.297150762882706143 ) ) ;
#7303 = CARTESIAN_POINT ( 'NONE',  ( 0.000000000000000000, 0.000000000000000000, 5.000000000000000000 ) ) ;
#7304 = SURFACE_SIDE_STYLE ('',( #29650 ) ) ;
#7305 =( LENGTH_UNIT ( ) NAMED_UNIT ( * ) SI_UNIT ( .MILLI., .METRE. ) );
#7306 = VERTEX_POINT ( 'NONE', #27957 ) ;
#7307 = DIRECTION ( 'NONE',  ( 0.000000000000000000, 0.000000000000000000, 1.000000000000000000 ) ) ;
#7308 = CARTESIAN_POINT ( 'NONE',  ( -14.54015256618497176, 142.2617268803927573, 0.000000000000000000 ) ) ;
#7309 = MECHANICAL_DESIGN_GEOMETRIC_PRESENTATION_REPRESENTATION (  '', ( #81364 ), #93502 ) ;
#7310 = CARTESIAN_POINT ( 'NONE',  ( 16.33361799548379523, 5.000000000000003553, 0.000000000000000000 ) ) ;
#7311 = CARTESIAN_POINT ( 'NONE',  ( -95.50364921585600086, -30.00000000000000711, 191.3268544109589300 ) ) ;
#7312 = EDGE_CURVE ( 'NONE', #97430, #3119, #18790, .T. ) ;
#7313 = CARTESIAN_POINT ( 'NONE',  ( 4.250000000000000000, 0.000000000000000000, -6.235812796514431433 ) ) ;
#7314 = STYLED_ITEM ( 'NONE', ( #97087 ), #21210 ) ;
#7315 = CARTESIAN_POINT ( 'NONE',  ( 37.94872683402551417, -57.69547342295989978, 52.59817782003744924 ) ) ;
#7317 = CARTESIAN_POINT ( 'NONE',  ( 43.03894652950267385, 464.9992092536288624, 11.55502599541370046 ) ) ;
#7316 = CARTESIAN_POINT ( 'NONE',  ( 15.94658505612039612, -2.878035407438557236, 14.72409133791870595 ) ) ;
#7318 = ADVANCED_FACE ( 'NONE', ( #103388 ), #102322, .F. ) ;
#7319 = ADVANCED_FACE ( 'NONE', ( #36043 ), #12709, .F. ) ;
#7320 = CARTESIAN_POINT ( 'NONE',  ( 1.641472239120435717, -21.31623762121044052, -38.55282611630758538 ) ) ;
#7321 = CARTESIAN_POINT ( 'NONE',  ( -9.341953373613074874, 15.21714514899110071, 3.572352985695586902 ) ) ;
#7322 = UNCERTAINTY_MEASURE_WITH_UNIT (LENGTH_MEASURE( 1.000000000000000082E-05 ), #97941, 'distance_accuracy_value', 'NONE');
#7323 = CARTESIAN_POINT ( 'NONE',  ( -7.370567298740709816, -60.00000000000000711, 39.63063440146133587 ) ) ;
#7324 = CARTESIAN_POINT ( 'NONE',  ( 14.01122214394832177, 20.85898477414747632, 6.193124377965379068 ) ) ;
#7325 = CARTESIAN_POINT ( 'NONE',  ( 1.249688359482191702, 45.80160873406245514, -17.33761737426925720 ) ) ;
#7326 = CARTESIAN_POINT ( 'NONE',  ( -86.90850660987527476, -31.72843720894637087, 187.1496124096579763 ) ) ;
#7327 = VERTEX_POINT ( 'NONE', #36574 ) ;
#7328 = CARTESIAN_POINT ( 'NONE',  ( 17.49999999999542410, 50.03176226080812228, 60.82931034966990325 ) ) ;
#7329 = CARTESIAN_POINT ( 'NONE',  ( 4.898587196589412829E-16, -12.12499999999999289, -8.000000000000000000 ) ) ;
#7330 = CARTESIAN_POINT ( 'NONE',  ( -6.036298205140932183, -29.03102288755636806, 28.71854023455634319 ) ) ;
#7331 = ADVANCED_FACE ( 'NONE', ( #28473 ), #56802, .F. ) ;
#7332 =( NAMED_UNIT ( * ) SI_UNIT ( $, .STERADIAN. ) SOLID_ANGLE_UNIT ( ) );
#7333 =( BOUNDED_CURVE ( )  B_SPLINE_CURVE ( 2, ( #69248, #53054, #73721 ),
 .UNSPECIFIED., .F., .F. ) 
 B_SPLINE_CURVE_WITH_KNOTS ( ( 3, 3 ),
 ( 0.000000000000000000, 1.000000000000000000 ),
 .UNSPECIFIED. ) 
 CURVE ( )  GEOMETRIC_REPRESENTATION_ITEM ( )  RATIONAL_B_SPLINE_CURVE ( ( 1.428571428571429269, 1.428571428571436375, 1.000000000000000000 ) ) 
 REPRESENTATION_ITEM ( '' )  );
#7334 = COLOUR_RGB ( '', 0.08235294, 0.09019608, 0.10196078) ;
#7336 = CARTESIAN_POINT ( 'NONE',  ( 41.18667489362654521, 461.2717826764273923, 2.470602812283018590 ) ) ;
#7335 = CARTESIAN_POINT ( 'NONE',  ( 6.725979247667766003, -3.622307570260328902, -6.470294263593361350 ) ) ;
#7337 = ADVANCED_BREP_SHAPE_REPRESENTATION ( '', ( #90947, #10728 ), #79871 ) ;
#7338 = ORIENTED_EDGE ( 'NONE', *, *, #102153, .T. ) ;
#7339 = CARTESIAN_POINT ( 'NONE',  ( 5.000000000000000000, -32.50000000000000000, 13.00000000000000178 ) ) ;
#7340 =( GEOMETRIC_REPRESENTATION_CONTEXT ( 3 ) GLOBAL_UNCERTAINTY_ASSIGNED_CONTEXT ( ( #55326 ) ) GLOBAL_UNIT_ASSIGNED_CONTEXT ( ( #12742, #82252, #72572 ) ) REPRESENTATION_CONTEXT ( 'NONE', 'WORKASPACE' ) );
#7341 = CARTESIAN_POINT ( 'NONE',  ( -7.701342750610986165, -4.999999999998212985, -18.36411236461060881 ) ) ;
#7342 = CARTESIAN_POINT ( 'NONE',  ( -30.04499556692276840, 7.904673525308127502, -42.05327650403284423 ) ) ;
#7343 = AXIS2_PLACEMENT_3D ( 'NONE', #91158, #1017, #65266 ) ;
#7344 = CARTESIAN_POINT ( 'NONE',  ( 34.32150620555758280, 300.7240803741787545, -8.683067128579168070 ) ) ;
#7345 = CYLINDRICAL_SURFACE ( 'NONE', #46709, 4.000000000000000888 ) ;
#7346 = CARTESIAN_POINT ( 'NONE',  ( 61.11682663846713837, 6.975173280561618775E-15, 0.000000000000000000 ) ) ;
#7347 = CARTESIAN_POINT ( 'NONE',  ( 71.07052165988230286, -60.00000000000000711, 147.7243966094672487 ) ) ;
#7348 = CARTESIAN_POINT ( 'NONE',  ( -35.74483125092430669, 413.6409941285803598, 6.029078300230034770 ) ) ;
#7349 = ORIENTED_EDGE ( 'NONE', *, *, #72208, .F. ) ;
#7350 = CARTESIAN_POINT ( 'NONE',  ( -3.888805312026751615, -29.99999999999997868, 6.385547335617978604 ) ) ;
#7351 = DIRECTION ( 'NONE',  ( -0.000000000000000000, -0.000000000000000000, -1.000000000000000000 ) ) ;
#7353 = DIRECTION ( 'NONE',  ( -1.000000000000000000, -0.000000000000000000, -0.000000000000000000 ) ) ;
#7352 =( LENGTH_UNIT ( ) NAMED_UNIT ( * ) SI_UNIT ( .MILLI., .METRE. ) );
#7354 = FILL_AREA_STYLE_COLOUR ( '', #80280 ) ;
#7355 = CARTESIAN_POINT ( 'NONE',  ( -5.437321008177367077, -2.342832151771177429, 104.0362115404844587 ) ) ;
#7356 = ORIENTED_EDGE ( 'NONE', *, *, #11079, .T. ) ;
#7357 = CARTESIAN_POINT ( 'NONE',  ( -29.01873216445066461, 322.4064345883938358, 14.26934359691588483 ) ) ;
#7358 = ORIENTED_EDGE ( 'NONE', *, *, #59904, .F. ) ;
#7359 = FACE_OUTER_BOUND ( 'NONE', #55272, .T. ) ;
#7360 = DIRECTION ( 'NONE',  ( 0.000000000000000000, 0.000000000000000000, -1.000000000000000000 ) ) ;
#7361 = DIRECTION ( 'NONE',  ( -1.000000000000000000, -0.000000000000000000, -0.000000000000000000 ) ) ;
#7362 = EDGE_LOOP ( 'NONE', ( #53550, #7290, #44171, #21213 ) ) ;
#7363 = CARTESIAN_POINT ( 'NONE',  ( -56.06936961864204250, 48.00000000000000000, -33.41736086623469504 ) ) ;
#7364 = FILL_AREA_STYLE_COLOUR ( '', #71436 ) ;
#7365 = CARTESIAN_POINT ( 'NONE',  ( -111.3949278518088306, -60.00000000000000000, 194.2500860083519285 ) ) ;
#7366 = CARTESIAN_POINT ( 'NONE',  ( 23.58349330513380337, 1.593028355512270962E-15, 0.000000000000000000 ) ) ;
#7367 = CARTESIAN_POINT ( 'NONE',  ( 88.17925955597732468, -60.00000000000002132, 201.4489170471512693 ) ) ;
#7368 = CARTESIAN_POINT ( 'NONE',  ( 85.59800593614014019, -2.002967142162725287E-29, 5.000000000000011546 ) ) ;
#7369 = CARTESIAN_POINT ( 'NONE',  ( -19.99999999999999289, 5.000000000000000888, 25.00000000000000000 ) ) ;
#7371 = CARTESIAN_POINT ( 'NONE',  ( 15.89902062379011660, -53.39644330016152907, 32.98550796398789942 ) ) ;
#7370 = CARTESIAN_POINT ( 'NONE',  ( -101.7136998165503883, -14.21045842199435150, 195.4607583018654395 ) ) ;
#7372 = CARTESIAN_POINT ( 'NONE',  ( 102.5622483503262288, -37.99999999999999289, 164.2734793211291731 ) ) ;
#7373 = EDGE_CURVE ( 'NONE', #94269, #2324, #81295, .T. ) ;
#7374 = CARTESIAN_POINT ( 'NONE',  ( -43.99789167439523396, -42.98520829747947403, 43.39751293111646646 ) ) ;
#7375 = CARTESIAN_POINT ( 'NONE',  ( -2.245730763533316132, 18.64284798592927217, 38.36507033181739246 ) ) ;
#7376 = ORIENTED_EDGE ( 'NONE', *, *, #40651, .T. ) ;
#7377 = CARTESIAN_POINT ( 'NONE',  ( -3.222962768498216414E-17, 13.85270131633358304, -7.000000000000011546 ) ) ;
#7378 = CARTESIAN_POINT ( 'NONE',  ( -4.804117642141982891, -64.31448375944374618, 13.02803471175172945 ) ) ;
#7379 = AXIS2_PLACEMENT_3D ( 'NONE', #26405, #93223, #10165 ) ;
#7380 = CARTESIAN_POINT ( 'NONE',  ( 98.59800593614012598, 1.016364837396684119E-14, 0.000000000000000000 ) ) ;
#7381 = CARTESIAN_POINT ( 'NONE',  ( 4.905194654929169396, -7.976056049801584891, 3.459476078998858117 ) ) ;
#7382 = FACE_BOUND ( 'NONE', #58866, .T. ) ;
#7383 = ORIENTED_EDGE ( 'NONE', *, *, #12903, .T. ) ;
#7384 = CARTESIAN_POINT ( 'NONE',  ( 4.902312018371809188, -46.91782384206802448, 103.3400275729950692 ) ) ;
#7385 = ORIENTED_EDGE ( 'NONE', *, *, #25370, .T. ) ;
#7386 = CARTESIAN_POINT ( 'NONE',  ( 98.13275984205787950, -29.99999999995851852, 199.6471406849189520 ) ) ;
#7387 = CARTESIAN_POINT ( 'NONE',  ( 45.99999999999999289, 461.1540656895900270, 8.531485566175636137 ) ) ;
#7388 = CIRCLE ( 'NONE', #84859, 4.000000000000000888 ) ;
#7389 = CARTESIAN_POINT ( 'NONE',  ( 6.645514545840788934, 41.91298724924220664, -59.84148600294046361 ) ) ;
#7390 = FILL_AREA_STYLE_COLOUR ( '', #86131 ) ;
#7391 = CARTESIAN_POINT ( 'NONE',  ( 97.92220087128177397, -29.99999999999999645, 136.9860503619559040 ) ) ;
#7392 = STYLED_ITEM ( 'NONE', ( #16237 ), #52538 ) ;
#7393 = ADVANCED_FACE ( 'NONE', ( #71015 ), #80156, .F. ) ;
#7394 = CARTESIAN_POINT ( 'NONE',  ( 7.934914944860278041, 101.1315435279989003, -1.051261972695691771 ) ) ;
#7395 = EDGE_LOOP ( 'NONE', ( #81045, #96428 ) ) ;
#7396 = ORIENTED_EDGE ( 'NONE', *, *, #37314, .F. ) ;
#7397 = ORIENTED_EDGE ( 'NONE', *, *, #82612, .F. ) ;
#7398 = CARTESIAN_POINT ( 'NONE',  ( 4.993259224064100499E-16, 0.3912769055735416113, -8.000000000000000000 ) ) ;
#7399 = CARTESIAN_POINT ( 'NONE',  ( -6.581905802744468126, 41.48827110272019780, -70.61906944529594909 ) ) ;
#7400 = CIRCLE ( 'NONE', #67706, 0.5000000000000004441 ) ;
#7401 = CYLINDRICAL_SURFACE ( 'NONE', #66858, 5.000000000000002665 ) ;
#7402 = ORIENTED_EDGE ( 'NONE', *, *, #105076, .F. ) ;
#7403 = CARTESIAN_POINT ( 'NONE',  ( 9.999952458099484076, 108.9998811452386462, 0.2653554233229081238 ) ) ;
#7404 = VERTEX_POINT ( 'NONE', #72598 ) ;
#7405 = DIRECTION ( 'NONE',  ( 0.000000000000000000, 1.000000000000000000, 0.000000000000000000 ) ) ;
#7406 = CARTESIAN_POINT ( 'NONE',  ( 85.62566950274205624, -38.66289190168809853, 198.8555151629249735 ) ) ;
#7407 = CARTESIAN_POINT ( 'NONE',  ( 12.99054989286523032, 8.523705905438497155, 8.946233657869846922 ) ) ;
#7408 = CARTESIAN_POINT ( 'NONE',  ( 64.24779899988634213, -38.00000000000000711, 83.19840595776713599 ) ) ;
#7409 = CARTESIAN_POINT ( 'NONE',  ( 29.29894309263326591, 313.0438134959539411, 12.40351596629518482 ) ) ;
#7410 = DIRECTION ( 'NONE',  ( 1.000000000000000000, -0.000000000000000000, 1.224646799147353207E-16 ) ) ;
#7411 = ADVANCED_FACE ( 'NONE', ( #105502 ), #101135, .T. ) ;
#7412 = CARTESIAN_POINT ( 'NONE',  ( 29.00000000000001066, 0.000000000000000000, 0.000000000000000000 ) ) ;
#7413 = CARTESIAN_POINT ( 'NONE',  ( -42.00989057912099156, 460.5566595377404155, 2.543045191514750059 ) ) ;
#7414 = CARTESIAN_POINT ( 'NONE',  ( -4.031080902170634417, -48.62189207507201161, 103.0284855429847681 ) ) ;
#7415 =( GEOMETRIC_REPRESENTATION_CONTEXT ( 3 ) GLOBAL_UNCERTAINTY_ASSIGNED_CONTEXT ( ( #19026 ) ) GLOBAL_UNIT_ASSIGNED_CONTEXT ( ( #30713, #31761, #87865 ) ) REPRESENTATION_CONTEXT ( 'NONE', 'WORKASPACE' ) );
#7416 = ORIENTED_EDGE ( 'NONE', *, *, #19218, .F. ) ;
#7417 = FACE_OUTER_BOUND ( 'NONE', #29082, .T. ) ;
#7418 = CARTESIAN_POINT ( 'NONE',  ( -31.99941821087105609, 300.2995772073126659, 11.16780820574502009 ) ) ;
#7419 = CARTESIAN_POINT ( 'NONE',  ( -4.225138137263944493, -48.93880982128749224, 104.4756818702664134 ) ) ;
#7420 = UNCERTAINTY_MEASURE_WITH_UNIT (LENGTH_MEASURE( 1.000000000000000082E-05 ), #62957, 'distance_accuracy_value', 'NONE');
#7421 = CARTESIAN_POINT ( 'NONE',  ( 0.000000000000000000, 0.000000000000000000, -7.000000000000011546 ) ) ;
#7422 = CARTESIAN_POINT ( 'NONE',  ( -3.313708498984760720, -13.53124999999999289, -8.000000000000000000 ) ) ;
#7423 = CARTESIAN_POINT ( 'NONE',  ( -3.380110533491807345, -18.24605901591677792, 35.03526125595637097 ) ) ;
#7424 = CARTESIAN_POINT ( 'NONE',  ( 1.128077836147720614, 302.8478239976497548, 9.936168295454386623 ) ) ;
#7425 = CARTESIAN_POINT ( 'NONE',  ( 3.308538776003295379, 303.8518027751323984, 9.936999415074360797 ) ) ;
#7426 = ORIENTED_EDGE ( 'NONE', *, *, #60694, .T. ) ;
#7427 = CARTESIAN_POINT ( 'NONE',  ( 86.28470205846313945, -21.13264878163486316, 179.4900229914080683 ) ) ;
#7428 = DIRECTION ( 'NONE',  ( 0.000000000000000000, 0.000000000000000000, 1.000000000000000000 ) ) ;
#7429 =( NAMED_UNIT ( * ) PLANE_ANGLE_UNIT ( ) SI_UNIT ( $, .RADIAN. ) );
#7430 = ORIENTED_EDGE ( 'NONE', *, *, #100420, .F. ) ;
#7431 = CARTESIAN_POINT ( 'NONE',  ( 93.97991700648807978, -57.67305785691176823, 18.55496576499952610 ) ) ;
#7432 = FACE_OUTER_BOUND ( 'NONE', #89099, .T. ) ;
#7433 = CARTESIAN_POINT ( 'NONE',  ( -2.499999999999996447, -30.00000000000000000, -13.00000000000000000 ) ) ;
#7434 = CARTESIAN_POINT ( 'NONE',  ( 8.559508646656350805, -1.200000000000000030E-05, -2.781152949374623873 ) ) ;
#7435 = B_SPLINE_CURVE_WITH_KNOTS ( 'NONE', 3,
 ( #54027, #38938, #70766, #45443 ),
 .UNSPECIFIED., .F., .F.,
 ( 4, 4 ),
 ( 1.734723475976807094E-18, 0.001714393297546049902 ),
 .UNSPECIFIED. ) ;
#7436 = CARTESIAN_POINT ( 'NONE',  ( 28.72970484482231157, 18.79180695567419335, 40.04448862869247705 ) ) ;
#7437 = CARTESIAN_POINT ( 'NONE',  ( 0.000000000000000000, -3.000000000000000000, 8.000000000000000000 ) ) ;
#7438 = DIRECTION ( 'NONE',  ( -1.000000000000000000, 0.000000000000000000, 0.000000000000000000 ) ) ;
#7440 = LINE ( 'NONE', #106134, #43050 ) ;
#7439 = PRESENTATION_STYLE_ASSIGNMENT (( #63052 ) ) ;
#7441 = CARTESIAN_POINT ( 'NONE',  ( -17.49999999999997513, 49.05239384892048093, 64.04602356109414529 ) ) ;
#7442 = CARTESIAN_POINT ( 'NONE',  ( -31.32517564075410021, 438.3829390354193265, 22.69287758365890539 ) ) ;
#7443 = CARTESIAN_POINT ( 'NONE',  ( -16.03025389958261471, 43.70290146489438854, -6.508476644219860496 ) ) ;
#7444 = CARTESIAN_POINT ( 'NONE',  ( -28.04619325667753671, 36.33495877514008754, -9.633940839559739899 ) ) ;
#7445 = CARTESIAN_POINT ( 'NONE',  ( 9.999999999999998224, 15.00000000000000000, -2.283746462400398747E-15 ) ) ;
#7446 = SURFACE_STYLE_FILL_AREA ( #73784 ) ;
#7447 = AXIS2_PLACEMENT_3D ( 'NONE', #86497, #99576, #49968 ) ;
#7448 = CARTESIAN_POINT ( 'NONE',  ( 32.87537929229700495, 485.0716560791287861, 1.465306988351172235 ) ) ;
#7449 = VERTEX_POINT ( 'NONE', #40233 ) ;
#7450 = PLANE ( 'NONE',  #51352 ) ;
#7451 =( NAMED_UNIT ( * ) SI_UNIT ( $, .STERADIAN. ) SOLID_ANGLE_UNIT ( ) );
#7452 = EDGE_CURVE ( 'NONE', #14964, #45269, #89135, .T. ) ;
#7453 = CIRCLE ( 'NONE', #35078, 4.000000000000000888 ) ;
#7454 = CARTESIAN_POINT ( 'NONE',  ( -11.08507223468469682, -16.42258121883788391, -34.72272924400278526 ) ) ;
#7455 = EDGE_CURVE ( 'NONE', #1846, #17567, #24788, .T. ) ;
#7457 = CARTESIAN_POINT ( 'NONE',  ( -65.15265132078000931, -60.22826349054815154, -28.17547081302746648 ) ) ;
#7456 = DIRECTION ( 'NONE',  ( 0.000000000000000000, -1.000000000000000000, 0.000000000000000000 ) ) ;
#7458 = ORIENTED_EDGE ( 'NONE', *, *, #66023, .T. ) ;
#7460 = EDGE_LOOP ( 'NONE', ( #94887, #63977 ) ) ;
#7459 = STYLED_ITEM ( 'NONE', ( #87569 ), #21810 ) ;
#7461 = DIRECTION ( 'NONE',  ( 0.000000000000000000, -1.000000000000000000, 0.000000000000000000 ) ) ;
#7462 = DIRECTION ( 'NONE',  ( -1.000000000000000000, -1.224606353822377258E-16, -0.000000000000000000 ) ) ;
#7463 = CARTESIAN_POINT ( 'NONE',  ( -66.30537473500707790, -60.00000000000000711, -33.79319030883430486 ) ) ;
#7464 = VERTEX_POINT ( 'NONE', #106554 ) ;
#7465 = CARTESIAN_POINT ( 'NONE',  ( 0.000000000000000000, -5.629165124598843661, 3.250000000000012879 ) ) ;
#7466 = DIRECTION ( 'NONE',  ( 0.000000000000000000, -1.000000000000000000, 0.000000000000000000 ) ) ;
#7467 = CARTESIAN_POINT ( 'NONE',  ( 96.11581706050769469, -52.82288690486888783, 195.4413948441345212 ) ) ;
#7469 = CARTESIAN_POINT ( 'NONE',  ( -17.89653557359973135, 45.30873500717390101, 5.550246105160095311 ) ) ;
#7468 = CARTESIAN_POINT ( 'NONE',  ( 7.500000000000007105, 152.0000000000000000, 5.000000000000000000 ) ) ;
#7470 = CARTESIAN_POINT ( 'NONE',  ( -80.03050186129850374, -56.86872676409061000, 169.5269957069628219 ) ) ;
#7471 = ORIENTED_EDGE ( 'NONE', *, *, #15064, .T. ) ;
#7472 = VECTOR ( 'NONE', #55440, 1000.000000000000000 ) ;
#7473 = ORIENTED_EDGE ( 'NONE', *, *, #30324, .F. ) ;
#7474 = ORIENTED_EDGE ( 'NONE', *, *, #92468, .F. ) ;
#7475 = FACE_OUTER_BOUND ( 'NONE', #80688, .T. ) ;
#7476 = STYLED_ITEM ( 'NONE', ( #63430 ), #97074 ) ;
#7477 = CARTESIAN_POINT ( 'NONE',  ( -5.000000000000000000, -14.06131484383571717, 13.29904837184955824 ) ) ;
#7478 = FILL_AREA_STYLE_COLOUR ( '', #69112 ) ;
#7479 = EDGE_LOOP ( 'NONE', ( #101320, #88875, #64650, #37692, #101755 ) ) ;
#7480 = CARTESIAN_POINT ( 'NONE',  ( 33.58349330513380693, 1.593028355512270962E-15, 0.000000000000000000 ) ) ;
#7481 = CARTESIAN_POINT ( 'NONE',  ( 0.000000000000000000, 14.17434517210798184, -56.74723269274520021 ) ) ;
#7482 =( GEOMETRIC_REPRESENTATION_CONTEXT ( 3 ) GLOBAL_UNCERTAINTY_ASSIGNED_CONTEXT ( ( #101204 ) ) GLOBAL_UNIT_ASSIGNED_CONTEXT ( ( #14337, #57448, #90367 ) ) REPRESENTATION_CONTEXT ( 'NONE', 'WORKASPACE' ) );
#7483 = CARTESIAN_POINT ( 'NONE',  ( -9.373884331924879021, 15.95332971149351842, -3.487646406148622980 ) ) ;
#7484 = CARTESIAN_POINT ( 'NONE',  ( -109.5878728966581832, -57.66746364524283308, 196.8330158634452118 ) ) ;
#7485 = CARTESIAN_POINT ( 'NONE',  ( 5.082755093536325930, -32.46875000204838813, -5.082755093536325042 ) ) ;
#7486 = CARTESIAN_POINT ( 'NONE',  ( -11.70968583459649182, 294.5933543508184016, -2.054959069366733448 ) ) ;
#7487 = CARTESIAN_POINT ( 'NONE',  ( -1.250037319930029422, 25.67361690534498209, 39.34156006938558647 ) ) ;
#7488 = CARTESIAN_POINT ( 'NONE',  ( 0.3381493856820239063, 28.19327355359043707, -38.28513279055599838 ) ) ;
#7489 = CARTESIAN_POINT ( 'NONE',  ( 53.63839714946880832, -30.00000000000003553, -34.46733499188162853 ) ) ;
#7490 = SHAPE_REPRESENTATION ( 'hex flange nut_din_Hexagon Flange Nut DIN 6923 - M10 - S', ( #10728 ), #71253 ) ;
#7491 = CARTESIAN_POINT ( 'NONE',  ( -31.98280533637225176, -29.99999999999996447, 41.00520926490388263 ) ) ;
#7492 = ADVANCED_FACE ( 'NONE', ( #49912 ), #58560, .T. ) ;
#7493 = CARTESIAN_POINT ( 'NONE',  ( -51.22124617248039158, -60.30834877352122447, 60.32251114123462798 ) ) ;
#7494 = CARTESIAN_POINT ( 'NONE',  ( 1.301042606982605321E-15, -5.000000000000000000, -10.00000000000000000 ) ) ;
#7495 = EDGE_LOOP ( 'NONE', ( #90806, #83704, #75712, #49989, #34012 ) ) ;
#7496 = CARTESIAN_POINT ( 'NONE',  ( -96.46940560253773356, -52.81427625367515333, 195.4040124156118168 ) ) ;
#7497 = CARTESIAN_POINT ( 'NONE',  ( -1.262177448353618889E-26, 294.8518027762758038, -10.00000000000000178 ) ) ;
#7498 = ORIENTED_EDGE ( 'NONE', *, *, #24544, .T. ) ;
#7499 = DIRECTION ( 'NONE',  ( -1.000000000000000000, -0.000000000000000000, -0.000000000000000000 ) ) ;
#7500 = CARTESIAN_POINT ( 'NONE',  ( 94.02105730861428867, -38.35588314265653764, 51.42162103336989531 ) ) ;
#7501 = CARTESIAN_POINT ( 'NONE',  ( 80.00000000000000000, -52.00000000000000000, -19.09707704303353282 ) ) ;
#7502 = CARTESIAN_POINT ( 'NONE',  ( 6.818272094961328023, 1.321852500971151922, -6.208027553811806598 ) ) ;
#7503 = CARTESIAN_POINT ( 'NONE',  ( -1.012484434415161560, 302.8485832914468006, 9.936327107976619999 ) ) ;
#7504 = CARTESIAN_POINT ( 'NONE',  ( 67.22793774957824553, 6.975173280561618775E-15, 0.000000000000000000 ) ) ;
#7505 = CARTESIAN_POINT ( 'NONE',  ( 75.34613995108148288, -30.00000000000000000, 113.5060042757550463 ) ) ;
#7506 = B_SPLINE_SURFACE_WITH_KNOTS ( 'NONE', 1, 3, ( 
 ( #36231, #35151, #91774, #59416, #27610, #84739, #75577, #101457, #92278, #68572, #68021, #1673, #61012, #19522, #69103, #52357, #85823, #44284, #44828, #100906, #27075, #3290, #11901, #36761, #93897, #34631, #59957, #20052 ),
 ( #77714, #3826, #99849, #104093, #70680, #4350, #21626, #21112, #96021, #86879, #37284, #38851, #55520, #54456, #46918, #71712, #53944, #87928, #103572, #104627, #63663, #30776, #54997, #5414, #95480, #69628, #38336, #94442 ) ),
 .UNSPECIFIED., .F., .F., .F.,
 ( 2, 2 ),
 ( 4, 2, 2, 2, 2, 2, 2, 2, 2, 2, 2, 2, 2, 4 ),
 ( 0.000000000000000000, 1.000000000000000000 ),
 ( 0.08901491201581737678, 0.1032490540155679704, 0.1174831960153185778, 0.1317173380150691853, 0.1459514800148197788, 0.1744197640143299588, 0.2028880480138401388, 0.2598246160128514504, 0.3167611840118632616, 0.4306343200098861623, 0.5445074560079088410, 0.6583805920059359051, 0.7722537280039543095, 1.000000000000000000 ),
 .UNSPECIFIED. ) ;
#7507 = CARTESIAN_POINT ( 'NONE',  ( 36.47828316237635704, 491.8387149836095205, 12.58546224877309427 ) ) ;
#7508 = EDGE_CURVE ( 'NONE', #104209, #8019, #8204, .T. ) ;
#7509 = CARTESIAN_POINT ( 'NONE',  ( -28.45522292534199238, 11.90502831567347108, 41.11935372236940367 ) ) ;
#7510 = CARTESIAN_POINT ( 'NONE',  ( -33.94783393359910662, 484.1261039197349305, 1.321740980884785532 ) ) ;
#7511 = CIRCLE ( 'NONE', #52330, 6.499999999999999112 ) ;
#7512 = VERTEX_POINT ( 'NONE', #99520 ) ;
#7513 = ORIENTED_EDGE ( 'NONE', *, *, #11088, .F. ) ;
#7514 = CARTESIAN_POINT ( 'NONE',  ( 48.95925862278320295, -42.97824454139764327, 50.18280914362345868 ) ) ;
#7515 = CARTESIAN_POINT ( 'NONE',  ( 6.249703441989621133, 41.65323758485251915, -58.70056750649388277 ) ) ;
#7516 = CARTESIAN_POINT ( 'NONE',  ( 36.80507370451574189, 28.12589318819196649, -11.20093102687100917 ) ) ;
#7517 = ORIENTED_EDGE ( 'NONE', *, *, #60368, .F. ) ;
#7518 = CARTESIAN_POINT ( 'NONE',  ( -90.65873703400211525, -38.34395918042547891, 9.055193890183026895 ) ) ;
#7519 = ORIENTED_EDGE ( 'NONE', *, *, #69952, .T. ) ;
#7520 = CARTESIAN_POINT ( 'NONE',  ( 28.34305552550043572, 34.21798169499945175, -8.615066575622451595 ) ) ;
#7521 = CARTESIAN_POINT ( 'NONE',  ( 93.42341124740551095, -38.35510331151919416, 46.74005875555363332 ) ) ;
#7522 = CARTESIAN_POINT ( 'NONE',  ( 11.66163491649460582, 15.90954947651264817, -9.571573500822044167 ) ) ;
#7523 = DIRECTION ( 'NONE',  ( 0.000000000000000000, 0.000000000000000000, 1.000000000000000000 ) ) ;
#7524 = CARTESIAN_POINT ( 'NONE',  ( 104.3685752548006462, -60.15138688519091659, 144.3650627233956527 ) ) ;
#7525 = CARTESIAN_POINT ( 'NONE',  ( -31.88319856737524205, 439.4127412706010887, 23.53498064488175956 ) ) ;
#7526 = CARTESIAN_POINT ( 'NONE',  ( 23.13516888326557108, 27.39820858062318365, 33.20617127781017786 ) ) ;
#7527 = CARTESIAN_POINT ( 'NONE',  ( -33.52518095673029563, 327.1007879220064751, -3.538621449569222310 ) ) ;
#7528 = CARTESIAN_POINT ( 'NONE',  ( 2.125394136664333633, -69.49483494517815529, 12.89457257817287328 ) ) ;
#7529 = CARTESIAN_POINT ( 'NONE',  ( 77.80177750690549487, -60.00000000000000711, 192.4143508859149279 ) ) ;
#7530 = EDGE_CURVE ( 'NONE', #24961, #31711, #100596, .T. ) ;
#7531 = CONICAL_SURFACE ( 'NONE', #102261, 4.000000000000001776, 0.9599310885968774798 ) ;
#7532 = CIRCLE ( 'NONE', #81357, 35.82893434829263413 ) ;
#7533 = CARTESIAN_POINT ( 'NONE',  ( 18.00050007014547759, 45.00000000000000000, 62.56698010746755756 ) ) ;
#7534 = ORIENTED_EDGE ( 'NONE', *, *, #35573, .F. ) ;
#7535 = CARTESIAN_POINT ( 'NONE',  ( 58.62522138716740727, -46.43623924511926049, 71.88277463636357822 ) ) ;
#7536 = EDGE_CURVE ( 'NONE', #25659, #82981, #3056, .T. ) ;
#7537 = CARTESIAN_POINT ( 'NONE',  ( -24.97190087653902424, 295.6134355416385233, -1.836602347154774550 ) ) ;
#7538 = CARTESIAN_POINT ( 'NONE',  ( 9.171181789971550202, -52.95185826047487154, 30.98656384792473162 ) ) ;
#7539 = CARTESIAN_POINT ( 'NONE',  ( -6.440906041033002793, -5.000000000000000000, -15.34892902906475420 ) ) ;
#7540 = ORIENTED_EDGE ( 'NONE', *, *, #43975, .F. ) ;
#7541 = B_SPLINE_CURVE_WITH_KNOTS ( 'NONE', 3,
 ( #40408, #25324, #31295, #72765 ),
 .UNSPECIFIED., .F., .F.,
 ( 4, 4 ),
 ( 6.938893903907228378E-18, 0.001632242847431727550 ),
 .UNSPECIFIED. ) ;
#7543 = CARTESIAN_POINT ( 'NONE',  ( -9.820360545668073371, -50.41108204965477313, 28.90271669672396726 ) ) ;
#7542 = CARTESIAN_POINT ( 'NONE',  ( -90.93871753736571861, -38.40505638326484927, -12.93646735681355864 ) ) ;
#7544 = CARTESIAN_POINT ( 'NONE',  ( 46.00000000000000000, 500.0000000000002274, 0.000000000000000000 ) ) ;
#7545 = CARTESIAN_POINT ( 'NONE',  ( 24.84269077136356074, 307.1603884938444367, 9.459414721148165839 ) ) ;
#7546 = DIRECTION ( 'NONE',  ( -1.000000000000000000, -1.224606353822377258E-16, -0.000000000000000000 ) ) ;
#7547 = CARTESIAN_POINT ( 'NONE',  ( 3.313708498984762496, -30.78124999999999289, 7.999999999999998224 ) ) ;
#7548 = DIRECTION ( 'NONE',  ( -0.8191520442889974607, 0.000000000000000000, -0.5735764363510380548 ) ) ;
#7549 = EDGE_CURVE ( 'NONE', #76235, #87758, #9278, .T. ) ;
#7550 = ADVANCED_FACE ( 'NONE', ( #59089 ), #45180, .T. ) ;
#7551 = CARTESIAN_POINT ( 'NONE',  ( 65.20309930813584742, 48.00000000000002132, 0.3961530819213638921 ) ) ;
#7552 = ORIENTED_EDGE ( 'NONE', *, *, #90121, .T. ) ;
#7553 = CARTESIAN_POINT ( 'NONE',  ( 85.66145762413124487, -21.90510868169506509, 168.0986262888999647 ) ) ;
#7554 = CARTESIAN_POINT ( 'NONE',  ( -27.10511071441192144, -1.200000000000000030E-05, -10.05698433968589178 ) ) ;
#7555 = LINE ( 'NONE', #50154, #45415 ) ;
#7556 = VERTEX_POINT ( 'NONE', #43434 ) ;
#7557 = DIRECTION ( 'NONE',  ( -1.000000000000000000, -0.000000000000000000, -0.000000000000000000 ) ) ;
#7559 = EDGE_CURVE ( 'NONE', #85705, #78207, #78796, .T. ) ;
#7558 = VECTOR ( 'NONE', #91947, 1000.000000000000227 ) ;
#7560 = CARTESIAN_POINT ( 'NONE',  ( 0.000000000000000000, 0.000000000000000000, 0.000000000000000000 ) ) ;
#7561 = CARTESIAN_POINT ( 'NONE',  ( 14.11595029532510104, 2.410436752314617959, -5.024000119269091513 ) ) ;
#7562 = CARTESIAN_POINT ( 'NONE',  ( 0.000000000000000000, -1.200000000000000030E-05, 9.000000000000000000 ) ) ;
#7563 = CYLINDRICAL_SURFACE ( 'NONE', #80148, 4.000000000000000000 ) ;
#7564 = CIRCLE ( 'NONE', #66171, 4.172000000000009479 ) ;
#7565 = AXIS2_PLACEMENT_3D ( 'NONE', #65932, #23374, #33062 ) ;
#7566 = CARTESIAN_POINT ( 'NONE',  ( 6.500000000000000000, -2.723981882618820904, -6.224051986859710617 ) ) ;
#7567 = CARTESIAN_POINT ( 'NONE',  ( 27.33349330513380693, 1.593028355512270962E-15, 0.000000000000000000 ) ) ;
#7569 = CARTESIAN_POINT ( 'NONE',  ( -11.45800518213875563, 9.451812037517163034, -9.373485686765249625 ) ) ;
#7568 = CARTESIAN_POINT ( 'NONE',  ( -23.47407494167467945, -28.00280731361893771, 37.76335220153635674 ) ) ;
#7570 = CARTESIAN_POINT ( 'NONE',  ( -2.977408999572650039, -15.68750000204838457, -7.188101187500001821 ) ) ;
#7571 = CARTESIAN_POINT ( 'NONE',  ( -65.26738680892601963, 40.83906611473079806, 0.8120011907944293394 ) ) ;
#7572 = LINE ( 'NONE', #32432, #39716 ) ;
#7573 = CONTEXT_DEPENDENT_SHAPE_REPRESENTATION ( #98303, #71806 ) ;
#7574 = EDGE_LOOP ( 'NONE', ( #83506, #41165, #36261, #87356, #51452 ) ) ;
#7575 = CARTESIAN_POINT ( 'NONE',  ( -17.50000000000202860, 49.80818831227223598, 62.14041309008910474 ) ) ;
#7576 = DIRECTION ( 'NONE',  ( 0.000000000000000000, 0.000000000000000000, -1.000000000000000000 ) ) ;
#7577 = CARTESIAN_POINT ( 'NONE',  ( -9.434261306447488948, 141.8831429914396836, 0.000000000000000000 ) ) ;
#7578 = DIRECTION ( 'NONE',  ( -1.000000000000000000, -1.224606353822377258E-16, -0.000000000000000000 ) ) ;
#7579 = EDGE_CURVE ( 'NONE', #81756, #94819, #47760, .T. ) ;
#7580 = DIRECTION ( 'NONE',  ( 0.000000000000000000, -1.000000000000000000, 0.000000000000000000 ) ) ;
#7581 = CIRCLE ( 'NONE', #55847, 4.000000000000007105 ) ;
#7582 = VERTEX_POINT ( 'NONE', #84427 ) ;
#7583 = CARTESIAN_POINT ( 'NONE',  ( -4.497431761510337189, -85.54098124251034108, -3.972160586670088200 ) ) ;
#7584 = CARTESIAN_POINT ( 'NONE',  ( 4.000000000000000000, 4.898587196589412829E-16, -1.161000000000000032 ) ) ;
#7585 = ORIENTED_EDGE ( 'NONE', *, *, #12565, .T. ) ;
#7586 = EDGE_CURVE ( 'NONE', #66822, #19762, #13345, .T. ) ;
#7587 = SURFACE_SIDE_STYLE ('',( #57203 ) ) ;
#7588 = CARTESIAN_POINT ( 'NONE',  ( 0.000000000000000000, 0.000000000000000000, 0.000000000000000000 ) ) ;
#7589 = CARTESIAN_POINT ( 'NONE',  ( -19.79304829293588952, 41.85759246273495648, -79.99079158153486446 ) ) ;
#7590 = CONICAL_SURFACE ( 'NONE', #28529, 4.000000000000001776, 0.9599310885968808105 ) ;
#7591 = CARTESIAN_POINT ( 'NONE',  ( -110.1325006654252689, -60.00000000000000711, 144.5141837704236991 ) ) ;
#7592 = CARTESIAN_POINT ( 'NONE',  ( 29.59455828143345002, 18.41848238274120675, -39.60535821593530414 ) ) ;
#7593 = CARTESIAN_POINT ( 'NONE',  ( -13.36289530936645953, 41.70153063405961547, -78.00930164889606999 ) ) ;
#7594 = CARTESIAN_POINT ( 'NONE',  ( 0.000000000000000000, 81.00000000000000000, 0.000000000000000000 ) ) ;
#7595 = CARTESIAN_POINT ( 'NONE',  ( 6.936184427528457874, 0.000000000000000000, 0.000000000000000000 ) ) ;
#7597 = CARTESIAN_POINT ( 'NONE',  ( 29.99999999999999289, 488.6917380704417724, 8.883757572940274017 ) ) ;
#7596 = CARTESIAN_POINT ( 'NONE',  ( 8.737863884122765157, -5.000000000000000888, -79.96381019769943066 ) ) ;
#7598 = CARTESIAN_POINT ( 'NONE',  ( -82.69763864773811690, -46.48872540907822781, 177.5893064810508122 ) ) ;
#7599 = VERTEX_POINT ( 'NONE', #76314 ) ;
#7600 = COLOUR_RGB ( '', 0.66274510, 0.83137255, 0.94901961) ;
#7601 = SURFACE_STYLE_USAGE ( .BOTH. , #39478 ) ;
#7602 = ORIENTED_EDGE ( 'NONE', *, *, #98176, .F. ) ;
#7603 = EDGE_LOOP ( 'NONE', ( #57407, #42936, #68682, #86439 ) ) ;
#7604 = DIRECTION ( 'NONE',  ( 0.000000000000000000, 1.000000000000000000, 0.000000000000000000 ) ) ;
#7605 = ADVANCED_FACE ( 'NONE', ( #52569 ), #37644, .T. ) ;
#7606 = CARTESIAN_POINT ( 'NONE',  ( 43.88846153846154152, 4.172000000000003261, 5.109226446042759579E-16 ) ) ;
#7607 = DIRECTION ( 'NONE',  ( -1.000000000000000000, -1.224606353822377258E-16, -0.000000000000000000 ) ) ;
#7608 = CARTESIAN_POINT ( 'NONE',  ( -15.82318872385282127, 4.444012391137944995, -4.874853782837179850 ) ) ;
#7609 = CARTESIAN_POINT ( 'NONE',  ( 8.588478090878989946, 23.79665183991722799, -4.999999999999385381 ) ) ;
#7610 = CARTESIAN_POINT ( 'NONE',  ( 2.370139314397876618, -5.000000000000000000, -97.83572313320559033 ) ) ;
#7611 = DIRECTION ( 'NONE',  ( 0.000000000000000000, 0.000000000000000000, 1.000000000000000000 ) ) ;
#7612 = CARTESIAN_POINT ( 'NONE',  ( 114.5925949185997439, -60.00000000000001421, 172.8113841322393682 ) ) ;
#7613 = CARTESIAN_POINT ( 'NONE',  ( -114.5724197576058714, -60.00000000000000000, 174.9505165961822684 ) ) ;
#7614 = EDGE_CURVE ( 'NONE', #35363, #102690, #19167, .T. ) ;
#7615 = CARTESIAN_POINT ( 'NONE',  ( -62.23155850973583370, -46.43999065396062775, 81.73006897967107420 ) ) ;
#7616 = VERTEX_POINT ( 'NONE', #13166 ) ;
#7617 = CARTESIAN_POINT ( 'NONE',  ( 20.10874767230411209, 38.95312827010130974, 60.47886685784197169 ) ) ;
#7618 = CARTESIAN_POINT ( 'NONE',  ( 107.8446305798313887, -59.99999999999507594, 199.8152282391069150 ) ) ;
#7619 = ORIENTED_EDGE ( 'NONE', *, *, #68254, .T. ) ;
#7620 = CARTESIAN_POINT ( 'NONE',  ( 13.48753244636324489, -55.04205951323852730, 23.24642415514733429 ) ) ;
#7621 = CARTESIAN_POINT ( 'NONE',  ( 5.082755093536325930, -11.84375000204838635, -5.082755093536325042 ) ) ;
#7622 = LINE ( 'NONE', #98762, #82157 ) ;
#7623 = ORIENTED_EDGE ( 'NONE', *, *, #7944, .F. ) ;
#7624 = CARTESIAN_POINT ( 'NONE',  ( 6.999999999999993783, -46.00000000000000000, 102.2532056551910387 ) ) ;
#7625 = ORIENTED_EDGE ( 'NONE', *, *, #84601, .F. ) ;
#7626 = FILL_AREA_STYLE ('',( #99295 ) ) ;
#7627 = AXIS2_PLACEMENT_3D ( 'NONE', #8507, #23135, #99100 ) ;
#7628 = CARTESIAN_POINT ( 'NONE',  ( 30.59999999999999787, 3.309500000000003439, 0.000000000000000000 ) ) ;
#7629 = CARTESIAN_POINT ( 'NONE',  ( -111.9904110614580190, -59.99999999999998579, 164.0997730435657047 ) ) ;
#7630 = CARTESIAN_POINT ( 'NONE',  ( 4.401442555609581635E-16, -28.15625000204838813, -7.188101187500000044 ) ) ;
#7631 = CARTESIAN_POINT ( 'NONE',  ( 33.00000000000000000, 485.0303364503728289, 0.9535057477322557151 ) ) ;
#7632 = CARTESIAN_POINT ( 'NONE',  ( 17.39155808811583981, 43.47117665187093394, -4.393666077417568872 ) ) ;
#7633 =( BOUNDED_CURVE ( )  B_SPLINE_CURVE ( 1, ( #18672, #33780 ),
 .UNSPECIFIED., .F., .T. ) 
 B_SPLINE_CURVE_WITH_KNOTS ( ( 2, 2 ),
 ( 0.000000000000000000, 1.000000000000000000 ),
 .UNSPECIFIED. ) 
 CURVE ( )  GEOMETRIC_REPRESENTATION_ITEM ( )  RATIONAL_B_SPLINE_CURVE ( ( 0.9660719911230173373, 0.9660719911230173373 ) ) 
 REPRESENTATION_ITEM ( '' )  );
#7634 = AXIS2_PLACEMENT_3D ( 'NONE', #5973, #30289, #64759 ) ;
#7635 = CARTESIAN_POINT ( 'NONE',  ( -5.290067270632214047, 53.47475093287474124, -8.531152949374821048 ) ) ;
#7636 = CARTESIAN_POINT ( 'NONE',  ( 16.08349330513380337, 1.593028355512270962E-15, 0.000000000000000000 ) ) ;
#7637 = CARTESIAN_POINT ( 'NONE',  ( -32.21797308369322366, 464.6987731533837405, 10.77720717743534173 ) ) ;
#7638 = FILL_AREA_STYLE_COLOUR ( '', #83452 ) ;
#7639 = ADVANCED_FACE ( 'NONE', ( #38031, #103782 ), #63879, .T. ) ;
#7640 = CARTESIAN_POINT ( 'NONE',  ( 29.34999999999999787, 3.309500000000003439, 0.000000000000000000 ) ) ;
#7641 = CARTESIAN_POINT ( 'NONE',  ( 87.00825156440252783, -60.00000000000000000, -8.027590136533380161 ) ) ;
#7642 = MECHANICAL_DESIGN_GEOMETRIC_PRESENTATION_REPRESENTATION (  '', ( #52453 ), #86909 ) ;
#7643 = CARTESIAN_POINT ( 'NONE',  ( -32.66505120407880725, -53.37625315817673766, 36.73532806000678619 ) ) ;
#7644 = CARTESIAN_POINT ( 'NONE',  ( -2.894864961504455270, -49.53440618355075031, 103.3614437639316463 ) ) ;
#7645 = CARTESIAN_POINT ( 'NONE',  ( 39.50165778835835084, -46.43035749859290462, 39.79999272029177604 ) ) ;
#7646 = CARTESIAN_POINT ( 'NONE',  ( 76.12557658274099026, -38.35599704320051018, -28.58424740099938077 ) ) ;
#7647 = ORIENTED_EDGE ( 'NONE', *, *, #27581, .F. ) ;
#7648 = CARTESIAN_POINT ( 'NONE',  ( -7.896165657598944065, 88.78911131371972942, -1.307894402814553825 ) ) ;
#7649 = CARTESIAN_POINT ( 'NONE',  ( -80.19950985152857470, -38.79610194437496062, 193.3420121686260700 ) ) ;
#7650 = ORIENTED_EDGE ( 'NONE', *, *, #36643, .F. ) ;
#7652 = CARTESIAN_POINT ( 'NONE',  ( -31.21933008645656926, 405.2090764464551853, 25.56980379099173817 ) ) ;
#7651 = CARTESIAN_POINT ( 'NONE',  ( 29.68315524076925982, 18.29184282782464166, -39.60535821593530414 ) ) ;
#7653 = CARTESIAN_POINT ( 'NONE',  ( -10.07965646519730996, 12.76099312266119057, 10.57234460686555089 ) ) ;
#7654 = CARTESIAN_POINT ( 'NONE',  ( -33.04853154822947658, 439.4047662902898423, 23.83380291423519282 ) ) ;
#7655 = CARTESIAN_POINT ( 'NONE',  ( 6.207999833770000642, 1.336757187206258024, 6.499999999999995559 ) ) ;
#7656 = CARTESIAN_POINT ( 'NONE',  ( 20.77592568779148863, -5.000000000000000888, 6.123233995736769241E-16 ) ) ;
#7657 = DIRECTION ( 'NONE',  ( 0.000000000000000000, -1.000000000000000000, 0.000000000000000000 ) ) ;
#7658 = CARTESIAN_POINT ( 'NONE',  ( 5.382954851612917757, -87.99987491489449098, -2.657971597726724866 ) ) ;
#7659 = DIRECTION ( 'NONE',  ( 0.000000000000000000, -1.000000000000000000, 0.000000000000000000 ) ) ;
#7660 = CARTESIAN_POINT ( 'NONE',  ( 92.01769393557711396, -60.00000000000000000, 18.81140579558686454 ) ) ;
#7661 = CARTESIAN_POINT ( 'NONE',  ( 37.06438722625302518, 1.482358050883964840E-15, 0.000000000000000000 ) ) ;
#7662 =( LENGTH_UNIT ( ) NAMED_UNIT ( * ) SI_UNIT ( .MILLI., .METRE. ) );
#7663 = ORIENTED_EDGE ( 'NONE', *, *, #24892, .T. ) ;
#7664 = EDGE_CURVE ( 'NONE', #37699, #89169, #86353, .T. ) ;
#7665 = AXIS2_PLACEMENT_3D ( 'NONE', #3169, #100262, #59291 ) ;
#7666 = CARTESIAN_POINT ( 'NONE',  ( -92.80508788735930636, -29.99999999999979039, 191.0773401206811286 ) ) ;
#7667 = ORIENTED_EDGE ( 'NONE', *, *, #93922, .T. ) ;
#7668 = CYLINDRICAL_SURFACE ( 'NONE', #21195, 15.00000000000000711 ) ;
#7669 = CARTESIAN_POINT ( 'NONE',  ( 4.258978623649388950, 11.59436199737384676, 5.000000000000000000 ) ) ;
#7670 = FACE_BOUND ( 'NONE', #84723, .T. ) ;
#7671 = CARTESIAN_POINT ( 'NONE',  ( -21.97121321732668520, 28.05118154993451896, -31.83013537814909100 ) ) ;
#7672 = CARTESIAN_POINT ( 'NONE',  ( 5.082755093536325930, -23.84375000204838457, -5.082755093536325042 ) ) ;
#7673 = SURFACE_STYLE_FILL_AREA ( #48667 ) ;
#7675 = ADVANCED_FACE ( 'NONE', ( #21841 ), #54683, .F. ) ;
#7674 = CARTESIAN_POINT ( 'NONE',  ( 6.763062899848484300, 41.48827110285979813, -70.48955655334555104 ) ) ;
#7676 = ORIENTED_EDGE ( 'NONE', *, *, #85240, .T. ) ;
#7678 = B_SPLINE_CURVE_WITH_KNOTS ( 'NONE', 3,
 ( #28389, #87136, #93628, #12156 ),
 .UNSPECIFIED., .F., .F.,
 ( 4, 4 ),
 ( 0.000000000000000000, 1.000000000000000000 ),
 .UNSPECIFIED. ) ;
#7677 = CIRCLE ( 'NONE', #23193, 0.9999999999999793499 ) ;
#7679 = CIRCLE ( 'NONE', #67980, 63.00000000000000000 ) ;
#7680 =( GEOMETRIC_REPRESENTATION_CONTEXT ( 3 ) GLOBAL_UNCERTAINTY_ASSIGNED_CONTEXT ( ( #105251 ) ) GLOBAL_UNIT_ASSIGNED_CONTEXT ( ( #679, #17460, #34189 ) ) REPRESENTATION_CONTEXT ( 'NONE', 'WORKASPACE' ) );
#7681 = COLOUR_RGB ( '', 0.09019608, 0.27058824, 0.51372549) ;
#7683 = EDGE_LOOP ( 'NONE', ( #69214, #76926, #83246, #86329 ) ) ;
#7682 = DIRECTION ( 'NONE',  ( 0.000000000000000000, 1.000000000000000000, 0.000000000000000000 ) ) ;
#7684 = CARTESIAN_POINT ( 'NONE',  ( 79.19591562604769308, -60.32219928206144743, 166.8364905889302747 ) ) ;
#7685 = CARTESIAN_POINT ( 'NONE',  ( -56.90650429242394637, 38.95383793067070854, -28.99688671941349583 ) ) ;
#7686 = VECTOR ( 'NONE', #91595, 1000.000000000000000 ) ;
#7687 = CARTESIAN_POINT ( 'NONE',  ( 0.000000000000000000, 0.000000000000000000, 4.000000000000000888 ) ) ;
#7688 = VERTEX_POINT ( 'NONE', #4566 ) ;
#7689 = EDGE_CURVE ( 'NONE', #83796, #78825, #39833, .T. ) ;
#7690 = DIRECTION ( 'NONE',  ( 0.000000000000000000, -1.000000000000000000, 0.000000000000000000 ) ) ;
#7691 = CARTESIAN_POINT ( 'NONE',  ( -14.68536286785258405, 1.589102881333048334, -3.051189359061289963 ) ) ;
#7692 = CARTESIAN_POINT ( 'NONE',  ( 4.401442555609581635E-16, -12.78125000204838280, -7.188101187500000044 ) ) ;
#7693 = CARTESIAN_POINT ( 'NONE',  ( 7.619701877737481865, 26.82557840467232424, -2.447562251315978266 ) ) ;
#7694 =( GEOMETRIC_REPRESENTATION_CONTEXT ( 3 ) GLOBAL_UNCERTAINTY_ASSIGNED_CONTEXT ( ( #29725 ) ) GLOBAL_UNIT_ASSIGNED_CONTEXT ( ( #4652, #21390, #47208 ) ) REPRESENTATION_CONTEXT ( 'NONE', 'WORKASPACE' ) );
#7695 = CARTESIAN_POINT ( 'NONE',  ( -53.00057554449748665, -60.00000000000002842, -31.41244228210902278 ) ) ;
#7696 = CARTESIAN_POINT ( 'NONE',  ( -36.61061158941262761, -57.69633519219438966, 50.91350493295865931 ) ) ;
#7697 = DIRECTION ( 'NONE',  ( 0.000000000000000000, -1.000000000000000000, 0.000000000000000000 ) ) ;
#7698 = ORIENTED_EDGE ( 'NONE', *, *, #9619, .T. ) ;
#7699 =( LENGTH_UNIT ( ) NAMED_UNIT ( * ) SI_UNIT ( .MILLI., .METRE. ) );
#7700 = CARTESIAN_POINT ( 'NONE',  ( 4.678819457397886517, 143.9212778189118467, 5.000000000000000000 ) ) ;
#7701 = CARTESIAN_POINT ( 'NONE',  ( 37.29474511894786559, 18.64284798592629500, -9.274907802241656896 ) ) ;
#7702 = CARTESIAN_POINT ( 'NONE',  ( 9.797174393178825657E-16, -3.035766082959412415E-15, -8.000000000000000000 ) ) ;
#7703 = ORIENTED_EDGE ( 'NONE', *, *, #34461, .T. ) ;
#7704 = CARTESIAN_POINT ( 'NONE',  ( 5.082755093536324154, -29.84375000204838813, 5.082755093536326818 ) ) ;
#7705 = CARTESIAN_POINT ( 'NONE',  ( 44.47534377888507606, -38.31160956920668070, 57.00192013341546016 ) ) ;
#7706 =( NAMED_UNIT ( * ) PLANE_ANGLE_UNIT ( ) SI_UNIT ( $, .RADIAN. ) );
#7707 = DIRECTION ( 'NONE',  ( 0.000000000000000000, -1.000000000000000000, 0.000000000000000000 ) ) ;
#7708 = EDGE_CURVE ( 'NONE', #80843, #6442, #98853, .T. ) ;
#7709 = CARTESIAN_POINT ( 'NONE',  ( 35.50943207940664337, 439.1423799595334572, 24.07278252408766761 ) ) ;
#7710 = SHAPE_DEFINITION_REPRESENTATION ( #3693, #58557 ) ;
#7711 = DIRECTION ( 'NONE',  ( 0.000000000000000000, 0.000000000000000000, 1.000000000000000000 ) ) ;
#7712 = ORIENTED_EDGE ( 'NONE', *, *, #69802, .T. ) ;
#7713 = CARTESIAN_POINT ( 'NONE',  ( 11.12982131476287151, 43.17719099323872456, 15.08403851094887393 ) ) ;
#7714 = CARTESIAN_POINT ( 'NONE',  ( -4.582575694955839829, 15.00000000000000000, 9.999999999999998224 ) ) ;
#7715 = PLANE ( 'NONE',  #32536 ) ;
#7716 = MECHANICAL_DESIGN_GEOMETRIC_PRESENTATION_REPRESENTATION (  '', ( #66318 ), #68019 ) ;
#7717 = CARTESIAN_POINT ( 'NONE',  ( 62.84259819506511491, -37.71647027193530732, -33.49470327681527948 ) ) ;
#7718 = CARTESIAN_POINT ( 'NONE',  ( -3.505862197715600814, -49.11848138796074892, 103.6125913840231902 ) ) ;
#7719 = CARTESIAN_POINT ( 'NONE',  ( 31.08349330513380693, 4.000000000000002665, 0.000000000000000000 ) ) ;
#7720 = EDGE_CURVE ( 'NONE', #28736, #29611, #72331, .T. ) ;
#7721 = DIRECTION ( 'NONE',  ( 0.000000000000000000, 1.000000000000000000, 0.000000000000000000 ) ) ;
#7722 = ORIENTED_EDGE ( 'NONE', *, *, #5394, .F. ) ;
#7723 = B_SPLINE_CURVE_WITH_KNOTS ( 'NONE', 3,
 ( #89340, #74191, #48320, #75252, #1353, #34315, #81214, #270, #33237, #25153, #19740, #26236, #83886, #12121, #100601, #42905, #27301, #100069, #35922, #101141, #10525, #52577, #51517, #35380, #10000, #3515, #84961, #11047, #84435, #2433 ),
 .UNSPECIFIED., .F., .F.,
 ( 4, 2, 2, 2, 2, 2, 2, 2, 2, 2, 2, 2, 2, 2, 4 ),
 ( 0.01423689679755356548, 0.01470129771271625439, 0.01493349817029759712, 0.01516569862787893984, 0.01539789908546028256, 0.01563009954304162355, 0.01586230000062296627, 0.01609450045820430900, 0.01655890137336699444, 0.01702330228852967989, 0.01795210411885506466, 0.01888090594918044943, 0.01980970777950582726, 0.02073850960983120856, 0.02166731144015658639 ),
 .UNSPECIFIED. ) ;
#7724 = CARTESIAN_POINT ( 'NONE',  ( 9.999999999999996447, 15.00000000000000000, -10.00000000000000000 ) ) ;
#7725 = CARTESIAN_POINT ( 'NONE',  ( 112.0160167646016163, -57.67108196866938385, 191.2727973919889166 ) ) ;
#7726 = ADVANCED_FACE ( 'NONE', ( #8797 ), #84561, .T. ) ;
#7727 = FILL_AREA_STYLE ('',( #58420 ) ) ;
#7728 = CARTESIAN_POINT ( 'NONE',  ( -9.538807954918411269, 51.45370039332727430, -1.987949993770493640 ) ) ;
#7729 = CARTESIAN_POINT ( 'NONE',  ( 32.33349330513380693, 4.000000000000003553, 0.000000000000000000 ) ) ;
#7730 = CARTESIAN_POINT ( 'NONE',  ( 60.62677696759038781, 40.83906611471993386, 24.18439664994441074 ) ) ;
#7731 = CARTESIAN_POINT ( 'NONE',  ( -73.05323961714354652, -60.00000000000000000, 162.9460430220049716 ) ) ;
#7732 = CARTESIAN_POINT ( 'NONE',  ( -43.29658055318886767, 324.1952503670673877, -2.852919881210743913 ) ) ;
#7733 =( NAMED_UNIT ( * ) SI_UNIT ( $, .STERADIAN. ) SOLID_ANGLE_UNIT ( ) );
#7734 = CARTESIAN_POINT ( 'NONE',  ( -37.04388863813380794, 311.3287000699716032, 13.89786840526617517 ) ) ;
#7735 = CARTESIAN_POINT ( 'NONE',  ( -84.26296102854614389, -50.17790333388872170, 187.6082884815264151 ) ) ;
#7736 = ORIENTED_EDGE ( 'NONE', *, *, #39875, .F. ) ;
#7737 = CARTESIAN_POINT ( 'NONE',  ( 29.41762786570794219, 308.7428865632042516, -8.884592557111700373 ) ) ;
#7738 = VERTEX_POINT ( 'NONE', #97804 ) ;
#7739 = DIRECTION ( 'NONE',  ( 0.5564727496918392413, -0.8308658609248571469, 0.000000000000000000 ) ) ;
#7740 = EDGE_CURVE ( 'NONE', #78219, #23042, #74587, .T. ) ;
#7742 = DIRECTION ( 'NONE',  ( -1.000000000000000000, -0.000000000000000000, -0.000000000000000000 ) ) ;
#7741 = AXIS2_PLACEMENT_3D ( 'NONE', #88085, #23365, #14165 ) ;
#7743 = CARTESIAN_POINT ( 'NONE',  ( -85.74469220476173348, -52.74251783766182911, -7.704084915169921111 ) ) ;
#7744 = FACE_OUTER_BOUND ( 'NONE', #99770, .T. ) ;
#7745 = DIRECTION ( 'NONE',  ( -1.000000000000000000, 0.000000000000000000, 0.000000000000000000 ) ) ;
#7746 = ORIENTED_EDGE ( 'NONE', *, *, #89325, .T. ) ;
#7747 = AXIS2_PLACEMENT_3D ( 'NONE', #41901, #32782, #24167 ) ;
#7748 = CARTESIAN_POINT ( 'NONE',  ( 11.53713417953937537, 7.347077458742750089, -9.367700058475382008 ) ) ;
#7749 = CARTESIAN_POINT ( 'NONE',  ( 21.65942590380565491, 2.899645552008857721E-12, 5.820808985964478488 ) ) ;
#7750 = CARTESIAN_POINT ( 'NONE',  ( -36.64367452218617416, 437.9806829953259921, 4.218857897671346002 ) ) ;
#7751 = CARTESIAN_POINT ( 'NONE',  ( 52.80879785486305167, -14.21045842199441722, -31.95559855168728092 ) ) ;
#7752 = CARTESIAN_POINT ( 'NONE',  ( -79.18173105286311397, -29.08793685032101806, 131.2448686397106599 ) ) ;
#7753 = VECTOR ( 'NONE', #73946, 1000.000000000000227 ) ;
#7754 = ORIENTED_EDGE ( 'NONE', *, *, #12253, .F. ) ;
#7755 = CARTESIAN_POINT ( 'NONE',  ( 55.43986775084101737, -14.21045842199435860, 70.80752230913886081 ) ) ;
#7756 = CARTESIAN_POINT ( 'NONE',  ( 7.413471587080149305, 87.64352159168325329, -3.013058070223553209 ) ) ;
#7757 = CARTESIAN_POINT ( 'NONE',  ( 93.02311254871766266, -57.65591657365690281, -17.17379135556295111 ) ) ;
#7758 = AXIS2_PLACEMENT_3D ( 'NONE', #51567, #846, #93100 ) ;
#7760 = ORIENTED_EDGE ( 'NONE', *, *, #99351, .F. ) ;
#7759 = CIRCLE ( 'NONE', #99073, 4.000000000000007105 ) ;
#7761 = CARTESIAN_POINT ( 'NONE',  ( 27.71747584658618990, 34.52906169721746465, 7.705713108082328233 ) ) ;
#7762 = CONICAL_SURFACE ( 'NONE', #87028, 4.000000000000007105, 0.9599310885968835860 ) ;
#7763 = DIRECTION ( 'NONE',  ( 0.000000000000000000, -1.000000000000000000, 0.000000000000000000 ) ) ;
#7764 = ORIENTED_EDGE ( 'NONE', *, *, #88020, .F. ) ;
#7765 = CIRCLE ( 'NONE', #100775, 3.309500000000001663 ) ;
#7766 = DIRECTION ( 'NONE',  ( 1.224646799147349509E-16, 0.000000000000000000, -1.000000000000000000 ) ) ;
#7767 =( NAMED_UNIT ( * ) PLANE_ANGLE_UNIT ( ) SI_UNIT ( $, .RADIAN. ) );
#7768 = CYLINDRICAL_SURFACE ( 'NONE', #100058, 8.000000000000000000 ) ;
#7769 = CARTESIAN_POINT ( 'NONE',  ( 5.082755093536325930, -20.46875000204838813, -5.082755093536325042 ) ) ;
#7770 = CARTESIAN_POINT ( 'NONE',  ( 43.60560354499546065, 484.6927786831506637, 3.665222855544667979 ) ) ;
#7771 = CARTESIAN_POINT ( 'NONE',  ( 9.253583916535173870, 83.70196091994968413, 3.792462592445555725 ) ) ;
#7772 = DIRECTION ( 'NONE',  ( -1.000000000000000000, -1.224606353822377258E-16, -0.000000000000000000 ) ) ;
#7773 = CARTESIAN_POINT ( 'NONE',  ( -7.500000000000000000, -0.7729939684968888391, -7.026407045654482708 ) ) ;
#7774 = CARTESIAN_POINT ( 'NONE',  ( -5.656854249492381470, -13.25000000409676915, 5.656854249492379694 ) ) ;
#7775 = EDGE_LOOP ( 'NONE', ( #99410, #67049, #60869, #92434, #64147, #60514 ) ) ;
#7776 = CARTESIAN_POINT ( 'NONE',  ( -7.125691916582566954, 41.67430808341742932, -69.26730091582949456 ) ) ;
#7778 = CARTESIAN_POINT ( 'NONE',  ( 28.55559703281400985, -39.48181379216788400, 32.65655774942846534 ) ) ;
#7777 = CARTESIAN_POINT ( 'NONE',  ( -1.385021579957316007, -30.00000000000000000, 37.00000000000000711 ) ) ;
#7779 = CARTESIAN_POINT ( 'NONE',  ( 29.45101819180745650, 310.9056806215746747, -7.594963747789880593 ) ) ;
#7780 = EDGE_LOOP ( 'NONE', ( #6318, #102256 ) ) ;
#7781 = ORIENTED_EDGE ( 'NONE', *, *, #47769, .T. ) ;
#7783 = CARTESIAN_POINT ( 'NONE',  ( 0.7145311798163219708, 4.618802153517003184, -8.000000000000000000 ) ) ;
#7782 = CARTESIAN_POINT ( 'NONE',  ( 42.40769230769231513, 1.411358822780289120E-15, 0.000000000000000000 ) ) ;
#7784 = DIRECTION ( 'NONE',  ( 0.000000000000000000, 0.000000000000000000, -1.000000000000000000 ) ) ;
#7785 = CARTESIAN_POINT ( 'NONE',  ( -17.09932871081075589, 294.5833313981810875, -2.056789631266450424 ) ) ;
#7786 = DIRECTION ( 'NONE',  ( 0.5735764363510470476, -0.8191520442889911324, 1.003171929053524007E-16 ) ) ;
#7787 = CARTESIAN_POINT ( 'NONE',  ( -33.00000000000000711, 484.0323588803976804, 1.017072797580844679 ) ) ;
#7788 = CARTESIAN_POINT ( 'NONE',  ( -36.52561726181225055, 463.3029834606193731, 20.13286708880156084 ) ) ;
#7789 = VERTEX_POINT ( 'NONE', #82692 ) ;
#7790 = CARTESIAN_POINT ( 'NONE',  ( 49.70935196047673088, -60.00000000000000711, -37.96160376868289887 ) ) ;
#7791 = CARTESIAN_POINT ( 'NONE',  ( -1.469576158976823947E-15, -13.06250000409676915, 8.000000000000000000 ) ) ;
#7792 = CARTESIAN_POINT ( 'NONE',  ( 6.563035550597769330, -3.302680408004405432, 6.845819698387219709 ) ) ;
#7793 = MECHANICAL_DESIGN_GEOMETRIC_PRESENTATION_REPRESENTATION (  '', ( #97340 ), #74992 ) ;
#7794 = CARTESIAN_POINT ( 'NONE',  ( 47.36504548439808104, 12.99580092579926394, -14.54285468146550286 ) ) ;
#7795 = ORIENTED_EDGE ( 'NONE', *, *, #105654, .F. ) ;
#7796 = ADVANCED_FACE ( 'NONE', ( #8263 ), #33110, .T. ) ;
#7797 = EDGE_CURVE ( 'NONE', #77091, #45005, #96641, .T. ) ;
#7798 = ORIENTED_EDGE ( 'NONE', *, *, #13852, .T. ) ;
#7799 = ORIENTED_EDGE ( 'NONE', *, *, #71051, .T. ) ;
#7800 = CARTESIAN_POINT ( 'NONE',  ( 0.8381057929850254107, 54.17571162905289839, 8.069066988206341051 ) ) ;
#7801 = CARTESIAN_POINT ( 'NONE',  ( 44.13004363183722489, 485.1789828605022876, 0.5705925370718127887 ) ) ;
#7802 = CARTESIAN_POINT ( 'NONE',  ( -35.52817563886351593, 439.1305428102971291, 24.06292914475137579 ) ) ;
#7803 = CARTESIAN_POINT ( 'NONE',  ( 25.40899158128945601, 304.9361475457282040, 10.40122582195319545 ) ) ;
#7804 = CARTESIAN_POINT ( 'NONE',  ( -37.50484670062839143, 362.5590287838574568, 3.193838888351949734 ) ) ;
#7805 = CARTESIAN_POINT ( 'NONE',  ( -3.175070672093349700, -70.04843617429949632, 13.36307156052828127 ) ) ;
#7806 = ADVANCED_FACE ( 'NONE', ( #16909 ), #57333, .F. ) ;
#7807 = CARTESIAN_POINT ( 'NONE',  ( 12.50000000000000711, 27.24691889344157403, -44.79063170920220927 ) ) ;
#7808 = ORIENTED_EDGE ( 'NONE', *, *, #38803, .T. ) ;
#7810 = EDGE_CURVE ( 'NONE', #99732, #99463, #100094, .T. ) ;
#7809 = CARTESIAN_POINT ( 'NONE',  ( 30.82780738024936795, 10.08347807711982647, 40.33814864067983308 ) ) ;
#7811 = ORIENTED_EDGE ( 'NONE', *, *, #69806, .T. ) ;
#7812 = CARTESIAN_POINT ( 'NONE',  ( 9.538609665898690082, 51.45378591545190972, -1.987744869269434167 ) ) ;
#7813 = CARTESIAN_POINT ( 'NONE',  ( -39.08667504521157809, 48.00000000000000000, -56.76470588235294912 ) ) ;
#7814 = PRESENTATION_STYLE_ASSIGNMENT (( #90342 ) ) ;
#7815 = EDGE_CURVE ( 'NONE', #56223, #95054, #37616, .T. ) ;
#7816 = DIRECTION ( 'NONE',  ( -0.000000000000000000, -1.000000000000000000, -0.000000000000000000 ) ) ;
#7817 = CARTESIAN_POINT ( 'NONE',  ( 65.02905820690668293, -29.05409441471111975, 80.86375735356135408 ) ) ;
#7818 = CIRCLE ( 'NONE', #6122, 9.500000000000000000 ) ;
#7819 = EDGE_LOOP ( 'NONE', ( #101008, #25574, #97499 ) ) ;
#7820 = EDGE_CURVE ( 'NONE', #1287, #103615, #5171, .T. ) ;
#7821 = CARTESIAN_POINT ( 'NONE',  ( 17.50000000000003197, 48.99424772499676806, 64.05279666586571352 ) ) ;
#7822 = DIRECTION ( 'NONE',  ( 0.000000000000000000, -1.000000000000000000, 0.000000000000000000 ) ) ;
#7823 = CARTESIAN_POINT ( 'NONE',  ( -55.77313467663169888, -57.67115539668835567, -38.70230501811910528 ) ) ;
#7824 = VECTOR ( 'NONE', #51059, 1000.000000000000000 ) ;
#7825 = ORIENTED_EDGE ( 'NONE', *, *, #37630, .T. ) ;
#7826 = CARTESIAN_POINT ( 'NONE',  ( 46.86404804693373194, 18.87323894068634544, 15.14441118170455702 ) ) ;
#7827 = VECTOR ( 'NONE', #51569, 1000.000000000000000 ) ;
#7828 = TOROIDAL_SURFACE ( 'NONE', #76732, 9.500000000000000000, 2.000000000000000000 ) ;
#7829 = CARTESIAN_POINT ( 'NONE',  ( -35.47838770905752881, 490.5979824476968361, 12.29204623667650864 ) ) ;
#7830 = B_SPLINE_CURVE_WITH_KNOTS ( 'NONE', 3,
 ( #42871, #75769, #18628, #51487 ),
 .UNSPECIFIED., .F., .F.,
 ( 4, 4 ),
 ( 0.000000000000000000, 1.000000000000000000 ),
 .UNSPECIFIED. ) ;
#7831 = CARTESIAN_POINT ( 'NONE',  ( 7.999999999999998224, -24.78125000409677270, 3.313708498984766493 ) ) ;
#7832 = CARTESIAN_POINT ( 'NONE',  ( 8.922269033012840467, -5.000000000000000000, 5.219866590718108768 ) ) ;
#7833 = AXIS2_PLACEMENT_3D ( 'NONE', #40799, #50875, #56436 ) ;
#7834 = AXIS2_PLACEMENT_3D ( 'NONE', #55095, #96115, #64285 ) ;
#7835 = CARTESIAN_POINT ( 'NONE',  ( 0.000000000000000000, 0.000000000000000000, 5.000000000000000000 ) ) ;
#7836 = CARTESIAN_POINT ( 'NONE',  ( -10.16315516181093237, 7.266990280869978669, 0.000000000000000000 ) ) ;
#7837 = AXIS2_PLACEMENT_3D ( 'NONE', #27361, #60240, #52108 ) ;
#7838 = CARTESIAN_POINT ( 'NONE',  ( 13.50000000000000178, 3.304540750553671469, -0.2220019300505709781 ) ) ;
#7839 = PRESENTATION_STYLE_ASSIGNMENT (( #15945 ) ) ;
#7840 = CARTESIAN_POINT ( 'NONE',  ( -3.487646406147736133, 15.95332971149351842, -9.373884331925221858 ) ) ;
#7841 = VERTEX_POINT ( 'NONE', #44910 ) ;
#7842 = DIRECTION ( 'NONE',  ( 1.000000000000000000, 1.224606353822377258E-16, 0.000000000000000000 ) ) ;
#7843 = CARTESIAN_POINT ( 'NONE',  ( 0.01372220897661434458, 5.309964801958107827, -3.802871176606132497 ) ) ;
#7844 = CARTESIAN_POINT ( 'NONE',  ( 10.73176661990081371, -5.000000000000000000, 0.000000000000000000 ) ) ;
#7845 = CARTESIAN_POINT ( 'NONE',  ( -92.60287565247158170, -30.00000000000000000, 191.0277603200695751 ) ) ;
#7846 = EDGE_CURVE ( 'NONE', #56292, #38550, #3644, .T. ) ;
#7847 = B_SPLINE_CURVE_WITH_KNOTS ( 'NONE', 3,
 ( #6949, #30740, #89480, #96515, #48989, #80299, #39867, #63080, #98088, #72739 ),
 .UNSPECIFIED., .F., .F.,
 ( 4, 2, 2, 2, 4 ),
 ( -2.000195913693996610E-05, 0.001085800244612921545, 0.002191602448362782625, 0.003297404652112645440, 0.004403206855862508255 ),
 .UNSPECIFIED. ) ;
#7848 = DIRECTION ( 'NONE',  ( 0.000000000000000000, 0.000000000000000000, -1.000000000000000000 ) ) ;
#7849 = CARTESIAN_POINT ( 'NONE',  ( 45.07112015427507856, -57.68308583978475923, 65.31626219697243130 ) ) ;
#7851 = CARTESIAN_POINT ( 'NONE',  ( -9.001830022268279663, 6.775897538200406522, 3.303914975154940148 ) ) ;
#7850 = CARTESIAN_POINT ( 'NONE',  ( 6.542885630808934927, 41.77241054322398384, -59.03854290128418825 ) ) ;
#7852 = EDGE_CURVE ( 'NONE', #56430, #653, #92970, .T. ) ;
#7853 = ADVANCED_FACE ( 'NONE', ( #28751 ), #35780, .F. ) ;
#7854 = CARTESIAN_POINT ( 'NONE',  ( 17.35462159048412545, -24.88231629494887187, -38.51483657780791958 ) ) ;
#7855 = DIRECTION ( 'NONE',  ( 0.000000000000000000, -1.000000000000000000, 0.000000000000000000 ) ) ;
#7856 = CARTESIAN_POINT ( 'NONE',  ( -28.73687143290147361, -60.00000000000000000, 42.44963378108809593 ) ) ;
#7857 = CARTESIAN_POINT ( 'NONE',  ( 12.67395752198872572, 18.60270564220093448, 8.290360506785944494 ) ) ;
#7858 = DIRECTION ( 'NONE',  ( -0.000000000000000000, -0.000000000000000000, -1.000000000000000000 ) ) ;
#7859 = CARTESIAN_POINT ( 'NONE',  ( -86.51918189808866089, -17.01178005999074827, 184.3026545482127290 ) ) ;
#7860 = ORIENTED_EDGE ( 'NONE', *, *, #69895, .T. ) ;
#7861 = CARTESIAN_POINT ( 'NONE',  ( 17.49999999999238298, 50.03761058181454047, 61.36442103422039196 ) ) ;
#7862 = PLANE ( 'NONE',  #10850 ) ;
#7863 = CARTESIAN_POINT ( 'NONE',  ( -9.249882429003642770, -42.95773840073744765, 31.05202513958081312 ) ) ;
#7864 = AXIS2_PLACEMENT_3D ( 'NONE', #30488, #6713, #96800 ) ;
#7866 = CARTESIAN_POINT ( 'NONE',  ( 0.8749999999999992228, -70.58759490697438821, 13.02737050516260098 ) ) ;
#7865 = CARTESIAN_POINT ( 'NONE',  ( -103.2741708893823898, -60.00000000000002842, 192.3304520135565951 ) ) ;
#7867 = ORIENTED_EDGE ( 'NONE', *, *, #59257, .F. ) ;
#7868 = ADVANCED_FACE ( 'NONE', ( #63744 ), #105015, .T. ) ;
#7869 = CARTESIAN_POINT ( 'NONE',  ( 5.175365594622103771, 41.93912328290134184, -69.86374199123662265 ) ) ;
#7870 = CARTESIAN_POINT ( 'NONE',  ( -7.092880029132369479, -4.030086327916265532, -17.38322132480382720 ) ) ;
#7871 = CARTESIAN_POINT ( 'NONE',  ( 16.58796880667331664, 35.02769128435444657, 21.80698433968581185 ) ) ;
#7872 = CARTESIAN_POINT ( 'NONE',  ( 28.83990699788477841, 306.5324003088252880, -9.174548767398087890 ) ) ;
#7873 = CARTESIAN_POINT ( 'NONE',  ( 3.857142857142850101, -48.79941684889506348, 103.1763305333244176 ) ) ;
#7874 = EDGE_CURVE ( 'NONE', #102684, #5546, #12505, .T. ) ;
#7875 = CARTESIAN_POINT ( 'NONE',  ( 69.60542681594449732, -59.99999999999999289, 139.2651478594983701 ) ) ;
#7876 = CARTESIAN_POINT ( 'NONE',  ( 113.3390500081078613, -59.99999999999998579, 187.7085336688584221 ) ) ;
#7877 = FACE_OUTER_BOUND ( 'NONE', #63942, .T. ) ;
#7878 = VERTEX_POINT ( 'NONE', #103133 ) ;
#7879 = CARTESIAN_POINT ( 'NONE',  ( -6.638433539294970487, -30.00000000000000711, 3.894772332383715785 ) ) ;
#7880 = DIRECTION ( 'NONE',  ( -1.000000000000000000, -1.224606353822377258E-16, -0.000000000000000000 ) ) ;
#7881 = DIRECTION ( 'NONE',  ( -1.000000000000000000, -0.000000000000000000, -0.000000000000000000 ) ) ;
#7882 = CARTESIAN_POINT ( 'NONE',  ( 91.37578371391791165, 6.123233995736582872E-16, -5.000000000000011546 ) ) ;
#7883 = EDGE_CURVE ( 'NONE', #70259, #4931, #29283, .T. ) ;
#7884 = CARTESIAN_POINT ( 'NONE',  ( 48.02835407290504577, -1.200000000000000030E-05, -15.60535821593549954 ) ) ;
#7885 = DIRECTION ( 'NONE',  ( 0.000000000000000000, -1.000000000000000000, 0.000000000000000000 ) ) ;
#7886 = ORIENTED_EDGE ( 'NONE', *, *, #6746, .T. ) ;
#7887 = CONICAL_SURFACE ( 'NONE', #45789, 16.09658290236430389, 0.7509290623979402168 ) ;
#7888 = CARTESIAN_POINT ( 'NONE',  ( -22.02345313010431838, 305.2775641474292456, 10.02869406391017648 ) ) ;
#7889 = EDGE_LOOP ( 'NONE', ( #29118, #28576, #11638, #100553, #86715 ) ) ;
#7890 = CARTESIAN_POINT ( 'NONE',  ( 32.87494462546104756, 485.1684504739468480, 5.618872456256310599 ) ) ;
#7891 = CARTESIAN_POINT ( 'NONE',  ( 31.06723445740051659, 439.4129214212010197, 22.80782786576363108 ) ) ;
#7892 = CARTESIAN_POINT ( 'NONE',  ( 93.97977184163765685, 1.030564683017419500E-14, 0.000000000000000000 ) ) ;
#7893 = CARTESIAN_POINT ( 'NONE',  ( 10.11986806485398382, 46.15873290010524954, 12.90779740156148847 ) ) ;
#7894 = VERTEX_POINT ( 'NONE', #54021 ) ;
#7895 =( GEOMETRIC_REPRESENTATION_CONTEXT ( 3 ) GLOBAL_UNCERTAINTY_ASSIGNED_CONTEXT ( ( #827 ) ) GLOBAL_UNIT_ASSIGNED_CONTEXT ( ( #38778, #95951, #94897 ) ) REPRESENTATION_CONTEXT ( 'NONE', 'WORKASPACE' ) );
#7896 = CARTESIAN_POINT ( 'NONE',  ( 51.78317192861597107, 50.00000000002003731, 39.73656039222791492 ) ) ;
#7897 = CARTESIAN_POINT ( 'NONE',  ( -9.864719719466185310, 7.401937201847157866, -1.292133144274320911 ) ) ;
#7898 = CARTESIAN_POINT ( 'NONE',  ( -47.33438562141003558, -59.99999999996092015, 71.44327096003375743 ) ) ;
#7899 = CARTESIAN_POINT ( 'NONE',  ( 95.42421628608209971, 1.030564683017419500E-14, 0.000000000000000000 ) ) ;
#7900 = CARTESIAN_POINT ( 'NONE',  ( 91.63563106630719801, -60.00000000000001421, 202.3019666817567099 ) ) ;
#7902 = CARTESIAN_POINT ( 'NONE',  ( 15.78057381398083336, -46.43467002123828991, 31.81701378920458012 ) ) ;
#7901 = CARTESIAN_POINT ( 'NONE',  ( -109.5313977869038098, -29.99999999999998934, 176.4136249138144876 ) ) ;
#7904 = CARTESIAN_POINT ( 'NONE',  ( 98.14827422455367412, -37.99999999999972999, 192.4855505147021688 ) ) ;
#7903 = UNCERTAINTY_MEASURE_WITH_UNIT (LENGTH_MEASURE( 1.000000000000000082E-05 ), #56106, 'distance_accuracy_value', 'NONE');
#7905 = CARTESIAN_POINT ( 'NONE',  ( -7.199040112754230057E-19, 54.30758622938872549, -7.749999999999999112 ) ) ;
#7906 = CARTESIAN_POINT ( 'NONE',  ( -47.01862296229795390, -42.98688433404485920, 47.24448534941780053 ) ) ;
#7907 = CARTESIAN_POINT ( 'NONE',  ( 0.000000000000000000, 0.9999999999999970024, 0.000000000000000000 ) ) ;
#7908 = AXIS2_PLACEMENT_3D ( 'NONE', #102885, #19887, #103410 ) ;
#7909 = ORIENTED_EDGE ( 'NONE', *, *, #91862, .T. ) ;
#7910 = AXIS2_PLACEMENT_3D ( 'NONE', #42163, #17912, #83674 ) ;
#7911 = SURFACE_STYLE_FILL_AREA ( #81787 ) ;
#7912 = VECTOR ( 'NONE', #91247, 1000.000000000000000 ) ;
#7913 = DIRECTION ( 'NONE',  ( -1.000000000000000000, -1.224606353822377258E-16, -0.000000000000000000 ) ) ;
#7914 = CARTESIAN_POINT ( 'NONE',  ( 6.033336773385737040, -14.92884390011191975, 14.31563199681414034 ) ) ;
#7915 = VECTOR ( 'NONE', #23048, 1000.000000000000000 ) ;
#7916 = CARTESIAN_POINT ( 'NONE',  ( 0.2573354458087825369, 6.889406814520509847, -1.067197363239225760 ) ) ;
#7917 = CARTESIAN_POINT ( 'NONE',  ( 6.683837171061806082, 7.911893696991936231, -4.595687358162529387E-16 ) ) ;
#7918 = CARTESIAN_POINT ( 'NONE',  ( 35.44563196690202744, 355.0508310518326311, 1.542887188955126110 ) ) ;
#7919 = ORIENTED_EDGE ( 'NONE', *, *, #26509, .F. ) ;
#7920 = CARTESIAN_POINT ( 'NONE',  ( 5.374793246923686318, -47.77528324145958294, 104.0614974883207680 ) ) ;
#7921 = B_SPLINE_CURVE_WITH_KNOTS ( 'NONE', 3,
 ( #15127, #23789, #98168, #56639 ),
 .UNSPECIFIED., .F., .F.,
 ( 4, 4 ),
 ( 0.000000000000000000, 0.002232172794123124613 ),
 .UNSPECIFIED. ) ;
#7922 = ORIENTED_EDGE ( 'NONE', *, *, #77308, .T. ) ;
#7923 = CARTESIAN_POINT ( 'NONE',  ( 80.72706426431642512, -30.00000000000003553, 14.39622326674284203 ) ) ;
#7924 = CARTESIAN_POINT ( 'NONE',  ( 23.79146510329413644, 41.63428640024510230, -74.58727699534063049 ) ) ;
#7925 = CARTESIAN_POINT ( 'NONE',  ( 24.35704318349077724, 25.22446577928139533, -32.47660146702440187 ) ) ;
#7926 = CARTESIAN_POINT ( 'NONE',  ( 2.500000000000000000, 7.216878364870322748, -7.063244554130003294 ) ) ;
#7927 = CARTESIAN_POINT ( 'NONE',  ( 92.38323657685867829, -30.00000000000000000, 102.4159884044749873 ) ) ;
#7928 = CARTESIAN_POINT ( 'NONE',  ( 7.002619243997876275, 103.9499268198618154, -3.868708944013000028 ) ) ;
#7929 = ORIENTED_EDGE ( 'NONE', *, *, #66113, .F. ) ;
#7930 = ADVANCED_FACE ( 'NONE', ( #13031 ), #34777, .F. ) ;
#7931 = ORIENTED_EDGE ( 'NONE', *, *, #60282, .F. ) ;
#7932 = VERTEX_POINT ( 'NONE', #82010 ) ;
#7933 = CARTESIAN_POINT ( 'NONE',  ( 33.11890921805852628, 438.9412750689605787, 23.90522689637583653 ) ) ;
#7934 = CARTESIAN_POINT ( 'NONE',  ( -2.680466883780622034, -7.322484912031441695, -13.10124357497377012 ) ) ;
#7935 = EDGE_CURVE ( 'NONE', #6102, #87544, #15693, .T. ) ;
#7936 = ORIENTED_EDGE ( 'NONE', *, *, #29499, .T. ) ;
#7938 = EDGE_CURVE ( 'NONE', #34348, #64513, #2002, .T. ) ;
#7937 = FILL_AREA_STYLE_COLOUR ( '', #15023 ) ;
#7939 = VERTEX_POINT ( 'NONE', #57204 ) ;
#7940 = DIRECTION ( 'NONE',  ( -1.000000000000000000, -1.224606353822377258E-16, -0.000000000000000000 ) ) ;
#7941 = CARTESIAN_POINT ( 'NONE',  ( 82.78759144455818841, -38.81844165587003914, 196.7277647683693260 ) ) ;
#7942 = CARTESIAN_POINT ( 'NONE',  ( 33.00540147335379260, 487.4196752801331627, 9.523982417622169905 ) ) ;
#7943 = CARTESIAN_POINT ( 'NONE',  ( 36.51610996680960142, 309.5552553936822164, 13.45073210680923026 ) ) ;
#7944 = EDGE_CURVE ( 'NONE', #75855, #59443, #19246, .T. ) ;
#7945 = STYLED_ITEM ( 'NONE', ( #20410 ), #28364 ) ;
#7946 = CARTESIAN_POINT ( 'NONE',  ( -10.00000000000000000, 15.00000000000000000, 10.00000000000000000 ) ) ;
#7947 = ADVANCED_FACE ( 'NONE', ( #58281 ), #8131, .T. ) ;
#7948 = AXIS2_PLACEMENT_3D ( 'NONE', #1244, #100499, #58995 ) ;
#7949 = CARTESIAN_POINT ( 'NONE',  ( -41.75908120488647768, 460.3944608375931011, 2.386179269091041721 ) ) ;
#7950 = CARTESIAN_POINT ( 'NONE',  ( -4.792515968931544634, -47.29776092521724706, 102.4138677444032055 ) ) ;
#7951 = DIRECTION ( 'NONE',  ( -1.000000000000000000, -1.224606353822377258E-16, -0.000000000000000000 ) ) ;
#7952 = CARTESIAN_POINT ( 'NONE',  ( 0.000000000000000000, 152.0000000000000000, 0.000000000000000000 ) ) ;
#7953 = VERTEX_POINT ( 'NONE', #73924 ) ;
#7954 = CARTESIAN_POINT ( 'NONE',  ( 2.505859880111868332, -49.58693854473261808, 103.1328899680561904 ) ) ;
#7956 = CARTESIAN_POINT ( 'NONE',  ( -28.21399895733517127, 296.8976392795444212, 2.382931296657796683 ) ) ;
#7955 = DIRECTION ( 'NONE',  ( 0.000000000000000000, 0.000000000000000000, 1.000000000000000000 ) ) ;
#7957 = CARTESIAN_POINT ( 'NONE',  ( 7.308187696580947801, 54.29028184318244143, -2.719951076200258555 ) ) ;
#7958 = CARTESIAN_POINT ( 'NONE',  ( 0.000000000000000000, 200.0000000000000000, 2.000000000000011102 ) ) ;
#7959 = CARTESIAN_POINT ( 'NONE',  ( -3.313708498984765161, -11.46874999999999289, 7.999999999999998224 ) ) ;
#7960 = FACE_OUTER_BOUND ( 'NONE', #50183, .T. ) ;
#7961 = CARTESIAN_POINT ( 'NONE',  ( -6.944031699373470090, 104.4653934544386971, 3.972913591453824278 ) ) ;
#7962 = ORIENTED_EDGE ( 'NONE', *, *, #38290, .T. ) ;
#7963 = CARTESIAN_POINT ( 'NONE',  ( 84.09387693237994199, -53.78933109331524776, 189.0839742466992561 ) ) ;
#7964 = DIRECTION ( 'NONE',  ( -0.5000000000000019984, -0.8660254037844374864, 0.000000000000000000 ) ) ;
#7965 = VECTOR ( 'NONE', #82912, 1000.000000000000227 ) ;
#7966 = CARTESIAN_POINT ( 'NONE',  ( -4.468441761983152460, 142.4699803267851621, 5.000000000000002665 ) ) ;
#7967 = ORIENTED_EDGE ( 'NONE', *, *, #25364, .T. ) ;
#7968 = CARTESIAN_POINT ( 'NONE',  ( 83.03225564478651677, -57.67107390234919251, -28.38291099116899829 ) ) ;
#7969 = LINE ( 'NONE', #10106, #95271 ) ;
#7970 = FACE_OUTER_BOUND ( 'NONE', #3129, .T. ) ;
#7971 = CARTESIAN_POINT ( 'NONE',  ( 52.56491209535275999, 39.42572890907100458, -38.23519342730396176 ) ) ;
#7972 =( BOUNDED_CURVE ( )  B_SPLINE_CURVE ( 2, ( #35728, #20631, #78788, #52933, #53975, #68605, #103606, #53471, #29757 ),
 .UNSPECIFIED., .F., .F. ) 
 B_SPLINE_CURVE_WITH_KNOTS ( ( 3, 2, 2, 2, 3 ),
 ( 0.5147058823529413463, 0.5220588235294120194, 0.5294117647058824705, 0.5367647058823530326, 0.5441176470588235947 ),
 .UNSPECIFIED. ) 
 CURVE ( )  GEOMETRIC_REPRESENTATION_ITEM ( )  RATIONAL_B_SPLINE_CURVE ( ( 0.9999999999999976685, 0.9238795325112890700, 1.000000000000000000, 0.9238795325112867385, 1.000000000000000000, 0.9238795325112867385, 1.000000000000000000, 0.9238795325112856283, 1.000000000000001110 ) ) 
 REPRESENTATION_ITEM ( '' )  );
#7973 = CARTESIAN_POINT ( 'NONE',  ( -81.02059387440468186, -29.99999999999999645, 21.32526539110572728 ) ) ;
#7974 = AXIS2_PLACEMENT_3D ( 'NONE', #20395, #65563, #97925 ) ;
#7975 = AXIS2_PLACEMENT_3D ( 'NONE', #99931, #16359, #67054 ) ;
#7976 = CARTESIAN_POINT ( 'NONE',  ( -76.43706498987678799, -37.99999999999996447, 125.5496669823371860 ) ) ;
#7977 = CARTESIAN_POINT ( 'NONE',  ( 0.000000000000000000, -3.000000000000000000, 8.000000000000000000 ) ) ;
#7978 = FACE_OUTER_BOUND ( 'NONE', #45317, .T. ) ;
#7980 = DIRECTION ( 'NONE',  ( 0.000000000000000000, -1.000000000000000000, 0.000000000000000000 ) ) ;
#7979 = CARTESIAN_POINT ( 'NONE',  ( 0.000000000000000000, 43.19193163660326462, 0.000000000000000000 ) ) ;
#7981 = EDGE_CURVE ( 'NONE', #25938, #57232, #15789, .T. ) ;
#7982 = FACE_OUTER_BOUND ( 'NONE', #24291, .T. ) ;
#7983 = CARTESIAN_POINT ( 'NONE',  ( -31.74546804893367380, 439.0126127266693175, 23.49846720828339386 ) ) ;
#7984 = AXIS2_PLACEMENT_3D ( 'NONE', #38624, #6759, #24046 ) ;
#7985 = AXIS2_PLACEMENT_3D ( 'NONE', #89132, #105832, #81531 ) ;
#7986 = CARTESIAN_POINT ( 'NONE',  ( -43.00000000000000000, 500.0000000000002274, 0.000000000000000000 ) ) ;
#7987 = CARTESIAN_POINT ( 'NONE',  ( -22.64062017603108501, -27.31223983661013222, -30.38885495092308986 ) ) ;
#7988 = DIRECTION ( 'NONE',  ( -1.000000000000000000, -0.000000000000000000, -0.000000000000000000 ) ) ;
#7989 = CONICAL_SURFACE ( 'NONE', #32125, 3.309500000000001663, 0.9599310885968770357 ) ;
#7990 = CIRCLE ( 'NONE', #45895, 15.00000000000000178 ) ;
#7991 = AXIS2_PLACEMENT_3D ( 'NONE', #18961, #83114, #28113 ) ;
#7992 = CARTESIAN_POINT ( 'NONE',  ( -100.8624366425310512, -38.00000000000002132, 188.7450187321335022 ) ) ;
#7993 = ORIENTED_EDGE ( 'NONE', *, *, #65157, .F. ) ;
#7994 = CARTESIAN_POINT ( 'NONE',  ( -6.458864185833882665, -0.2568716777371773397, 15.39536780018543993 ) ) ;
#7995 = AXIS2_PLACEMENT_3D ( 'NONE', #89206, #8802, #48192 ) ;
#7996 = CARTESIAN_POINT ( 'NONE',  ( 7.500000000000003553, 18.65452285268503729, -40.72535638072048414 ) ) ;
#7997 = CARTESIAN_POINT ( 'NONE',  ( 8.061685236282825271E-09, -15.39512265162600535, -35.22781471665102515 ) ) ;
#7999 = CARTESIAN_POINT ( 'NONE',  ( -35.59171129655433674, -60.22815248269157706, -34.49232045672559366 ) ) ;
#7998 = CARTESIAN_POINT ( 'NONE',  ( 0.000000000000000000, 6.123233995736767268E-16, -5.000000000000000888 ) ) ;
#8000 = ORIENTED_EDGE ( 'NONE', *, *, #80652, .T. ) ;
#8001 = EDGE_LOOP ( 'NONE', ( #11212, #6616, #75140, #85150 ) ) ;
#8002 = CARTESIAN_POINT ( 'NONE',  ( 0.5805565836007617886, -3.752776749732566142, 6.499999999999999112 ) ) ;
#8003 = CARTESIAN_POINT ( 'NONE',  ( -8.000000000000000000, -29.74999999999999645, -9.797174393178825657E-16 ) ) ;
#8004 = DIRECTION ( 'NONE',  ( -1.000000000000000000, 0.000000000000000000, 0.000000000000000000 ) ) ;
#8005 = CARTESIAN_POINT ( 'NONE',  ( -47.29246454944256328, -59.99999999999999289, -38.43485023766499609 ) ) ;
#8006 = EDGE_LOOP ( 'NONE', ( #45604, #27234, #103690, #61023, #39753 ) ) ;
#8007 = CARTESIAN_POINT ( 'NONE',  ( 3.241669456190960030, -22.04828166566017345, -30.53834172389159818 ) ) ;
#8008 = CARTESIAN_POINT ( 'NONE',  ( 15.12883790376646509, 3.606441264071186037, -4.265930408067698743 ) ) ;
#8009 = CARTESIAN_POINT ( 'NONE',  ( 98.41711723305866144, -52.80332669457988004, 194.9895706369884749 ) ) ;
#8011 = CARTESIAN_POINT ( 'NONE',  ( 35.58361799548379167, 1.482358050883964840E-15, 0.000000000000000000 ) ) ;
#8010 = CARTESIAN_POINT ( 'NONE',  ( 56.22793774957824553, -4.000000000000000000, 4.898587196589421703E-16 ) ) ;
#8012 = ADVANCED_FACE ( 'NONE', ( #16763 ), #103640, .T. ) ;
#8013 = EDGE_LOOP ( 'NONE', ( #93128, #6645, #75969, #7795 ) ) ;
#8014 = ORIENTED_EDGE ( 'NONE', *, *, #77722, .F. ) ;
#8015 = VECTOR ( 'NONE', #3699, 1000.000000000000000 ) ;
#8016 = ORIENTED_EDGE ( 'NONE', *, *, #54369, .F. ) ;
#8017 = CARTESIAN_POINT ( 'NONE',  ( 29.49295069903413591, 326.6849569854988431, 15.30827334355864799 ) ) ;
#8018 = CARTESIAN_POINT ( 'NONE',  ( -5.000000000000039968, -14.59885031841968228, 13.58543933205532817 ) ) ;
#8019 = VERTEX_POINT ( 'NONE', #39986 ) ;
#8020 = CARTESIAN_POINT ( 'NONE',  ( 31.08349330513380337, -7.703719777548943412E-31, 4.000000000000001776 ) ) ;
#8021 = CARTESIAN_POINT ( 'NONE',  ( -4.088397730506703056E-15, 46.03420836107012093, 33.38430095398285147 ) ) ;
#8022 = CARTESIAN_POINT ( 'NONE',  ( -32.65817089032885434, 465.7881089174890690, 12.85132715801033854 ) ) ;
#8023 = CARTESIAN_POINT ( 'NONE',  ( -72.09688937032439071, -57.67332965070641393, 173.0313604384042776 ) ) ;
#8024 = CARTESIAN_POINT ( 'NONE',  ( 2.977408999572650927, -32.37500000204838813, -7.188101187500001821 ) ) ;
#8025 = CARTESIAN_POINT ( 'NONE',  ( 7.414580834929597408, -67.64656280281481315, 3.010264818013837385 ) ) ;
#8026 = CARTESIAN_POINT ( 'NONE',  ( -1.011932115878593219, 25.89208366899141822, 38.74812953189098153 ) ) ;
#8027 = CYLINDRICAL_SURFACE ( 'NONE', #53713, 6.000000000000000888 ) ;
#8028 = CARTESIAN_POINT ( 'NONE',  ( 17.10006063058271053, -59.99999999999996447, -44.43597027717249404 ) ) ;
#8029 = CARTESIAN_POINT ( 'NONE',  ( -20.75616973061526949, -30.00000000000004263, 37.60198765588109637 ) ) ;
#8030 = B_SPLINE_CURVE_WITH_KNOTS ( 'NONE', 3,
 ( #86999, #6573, #21747, #5526, #29838, #38970, #7108, #45999, #96667, #40023, #13604, #31432, #38451, #64308, #71843, #6043, #104212, #14131, #72894, #95605, #31944, #97179 ),
 .UNSPECIFIED., .F., .F.,
 ( 4, 2, 2, 2, 2, 2, 2, 2, 2, 2, 4 ),
 ( 0.004989850371616175867, 0.005493891472670150294, 0.005997932573724123854, 0.006501973674778097415, 0.007006014775832071842, 0.007258035326359059056, 0.007510055876886046269, 0.008014096977940018962, 0.008518138078993993390, 0.008770158629520980603, 0.009022179180047967817 ),
 .UNSPECIFIED. ) ;
#8031 = CARTESIAN_POINT ( 'NONE',  ( -52.40170964977422585, -53.37735564585817372, 60.21222595448364956 ) ) ;
#8032 = DIRECTION ( 'NONE',  ( -1.000000000000000000, -1.224606353822377258E-16, -0.000000000000000000 ) ) ;
#8033 = PRODUCT_DEFINITION ( 'UNKNOWN', '', #50753, #33814 ) ;
#8034 = VERTEX_POINT ( 'NONE', #72857 ) ;
#8035 = CARTESIAN_POINT ( 'NONE',  ( -99.38960187038392746, -45.25186168038769097, 193.0844496258347931 ) ) ;
#8036 =( REPRESENTATION_RELATIONSHIP ('NONE','NONE', #69581, #22031 ) REPRESENTATION_RELATIONSHIP_WITH_TRANSFORMATION ( #104697 )SHAPE_REPRESENTATION_RELATIONSHIP( ) );
#8037 = CARTESIAN_POINT ( 'NONE',  ( -1.249646147729365664, 294.8475419170777059, -9.939938411486226144 ) ) ;
#8038 = B_SPLINE_CURVE_WITH_KNOTS ( 'NONE', 3,
 ( #104218, #96147, #94572, #29846 ),
 .UNSPECIFIED., .F., .F.,
 ( 4, 4 ),
 ( 5.721958498152796815E-17, 0.001000218973298496470 ),
 .UNSPECIFIED. ) ;
#8039 = CARTESIAN_POINT ( 'NONE',  ( 13.57536397604353340, 1.208058863777641267, 14.95207728893323562 ) ) ;
#8040 = ORIENTED_EDGE ( 'NONE', *, *, #99417, .T. ) ;
#8041 = CARTESIAN_POINT ( 'NONE',  ( -16.91676434013897889, 34.22373756221627161, -24.29887300997501143 ) ) ;
#8042 = AXIS2_PLACEMENT_3D ( 'NONE', #47746, #80645, #23520 ) ;
#8043 = CARTESIAN_POINT ( 'NONE',  ( 109.8608637664040515, -38.35600155330774186, 186.7385511336370314 ) ) ;
#8044 = LINE ( 'NONE', #90033, #105303 ) ;
#8045 = CARTESIAN_POINT ( 'NONE',  ( -6.528653810299468674, 51.53967708196228870, -6.914260884958386200 ) ) ;
#8046 =( LENGTH_UNIT ( ) NAMED_UNIT ( * ) SI_UNIT ( .MILLI., .METRE. ) );
#8047 = LINE ( 'NONE', #80875, #92775 ) ;
#8048 = CARTESIAN_POINT ( 'NONE',  ( 80.64605670160975137, -30.00000000000000000, 138.0219786762299918 ) ) ;
#8049 = CARTESIAN_POINT ( 'NONE',  ( -4.000000000000000000, 0.000000000000000000, -6.838999999999999524 ) ) ;
#8050 = CARTESIAN_POINT ( 'NONE',  ( -32.28552837373656814, 464.7648866755938570, 15.30384310834764428 ) ) ;
#8051 = DIRECTION ( 'NONE',  ( -1.000000000000000000, -1.224606353822377258E-16, -0.000000000000000000 ) ) ;
#8052 = B_SPLINE_CURVE_WITH_KNOTS ( 'NONE', 3,
 ( #70350, #80014, #95683, #31507, #87602, #5604, #55720, #64388, #72459, #6661, #47115, #23409, #62277, #6124, #95164, #48173, #29392, #78959, #54134, #96751 ),
 .UNSPECIFIED., .F., .F.,
 ( 4, 2, 2, 2, 2, 2, 2, 2, 2, 4 ),
 ( 0.003115351416494580722, 0.003619732534144853853, 0.004124113651795126984, 0.004628494769445400114, 0.005132875887095674113, 0.005385066445920808076, 0.005637257004745941172, 0.006141638122396208231, 0.006646019240046476158, 0.007150400357696743217 ),
 .UNSPECIFIED. ) ;
#8053 = ORIENTED_EDGE ( 'NONE', *, *, #57855, .T. ) ;
#8054 = VERTEX_POINT ( 'NONE', #57732 ) ;
#8055 = CARTESIAN_POINT ( 'NONE',  ( 48.89013321113019117, -22.21369756360278203, 43.54071997640996017 ) ) ;
#8056 = CONICAL_SURFACE ( 'NONE', #16691, 3.309500000000001663, 0.9599310885968770357 ) ;
#8057 = CARTESIAN_POINT ( 'NONE',  ( 6.568714581474836223, 41.61374591157808567, -58.74117443926016335 ) ) ;
#8058 = AXIS2_PLACEMENT_3D ( 'NONE', #86590, #52587, #44520 ) ;
#8059 = CARTESIAN_POINT ( 'NONE',  ( 63.07777777777777573, 6.915964383211875250E-15, 0.000000000000000000 ) ) ;
#8060 = ADVANCED_FACE ( 'NONE', ( #73384 ), #106281, .T. ) ;
#8061 = ORIENTED_EDGE ( 'NONE', *, *, #60748, .F. ) ;
#8062 = CARTESIAN_POINT ( 'NONE',  ( -93.44691131992647115, -38.35488852157141082, 46.93959257640000970 ) ) ;
#8063 = ORIENTED_EDGE ( 'NONE', *, *, #89598, .F. ) ;
#8064 = CARTESIAN_POINT ( 'NONE',  ( 27.42290749620547174, 34.64384839456566567, -7.587773793964464275 ) ) ;
#8065 = CARTESIAN_POINT ( 'NONE',  ( 92.04617479045300854, -38.35408004050898256, 35.18142690402697781 ) ) ;
#8066 = CARTESIAN_POINT ( 'NONE',  ( 11.77243489797928611, 11.38584543533899662, -9.872918751301874352 ) ) ;
#8067 = CARTESIAN_POINT ( 'NONE',  ( 0.000000000000000000, 303.8518027762758038, 9.936999415352289589 ) ) ;
#8069 = CARTESIAN_POINT ( 'NONE',  ( 103.7134520183080326, -60.15124960079525351, 139.5371650122951621 ) ) ;
#8068 = MECHANICAL_DESIGN_GEOMETRIC_PRESENTATION_REPRESENTATION (  '', ( #2912 ), #92454 ) ;
#8070 = VECTOR ( 'NONE', #26884, 1000.000000000000000 ) ;
#8071 = DIRECTION ( 'NONE',  ( 0.000000000000000000, 1.000000000000000000, 0.000000000000000000 ) ) ;
#8073 = CIRCLE ( 'NONE', #9832, 5.000000000000011546 ) ;
#8072 = CARTESIAN_POINT ( 'NONE',  ( -34.81734560031965486, 344.2880855494414050, 0.4170339163263865334 ) ) ;
#8074 = CARTESIAN_POINT ( 'NONE',  ( 4.225954871949793912, -66.94789023181898813, 13.14696679065552765 ) ) ;
#8075 = CARTESIAN_POINT ( 'NONE',  ( 74.36397108531809863, -59.99999999999999289, 175.8240678876071570 ) ) ;
#8076 = CONICAL_SURFACE ( 'NONE', #64909, 5.000000000000001776, 0.9599310885968803664 ) ;
#8077 = VECTOR ( 'NONE', #10387, 1000.000000000000114 ) ;
#8078 = EDGE_CURVE ( 'NONE', #6505, #72376, #17314, .T. ) ;
#8079 = CARTESIAN_POINT ( 'NONE',  ( -30.00000000000000000, 490.5636507776930557, 7.413185101875094496 ) ) ;
#8080 = ORIENTED_EDGE ( 'NONE', *, *, #103768, .F. ) ;
#8081 = CARTESIAN_POINT ( 'NONE',  ( 60.91963193027662982, -32.53835347950492718, 71.34319023294183637 ) ) ;
#8082 = ADVANCED_FACE ( 'NONE', ( #48052 ), #23833, .T. ) ;
#8083 = CARTESIAN_POINT ( 'NONE',  ( -25.60610463954871463, 295.7997949935824522, -1.796194680006651945 ) ) ;
#8084 = CARTESIAN_POINT ( 'NONE',  ( 9.215420734788356327, -54.00000000000000000, 23.11721482942554928 ) ) ;
#8085 = CARTESIAN_POINT ( 'NONE',  ( 4.898587196589412829E-16, -15.31250000409677092, -8.000000000000000000 ) ) ;
#8087 = CARTESIAN_POINT ( 'NONE',  ( -4.063605838664956948, 54.18614975339210105, 6.989214199201114752 ) ) ;
#8086 = CARTESIAN_POINT ( 'NONE',  ( -86.45048231984965525, -38.36235641012063979, -21.45451331935682049 ) ) ;
#8088 = CARTESIAN_POINT ( 'NONE',  ( -32.57492934538399965, 345.3439590197779125, 19.85777474157123024 ) ) ;
#8089 = FACE_OUTER_BOUND ( 'NONE', #48617, .T. ) ;
#8090 = CARTESIAN_POINT ( 'NONE',  ( 32.33349330513380693, 4.898587196589411843E-16, -4.000000000000001776 ) ) ;
#8091 = CARTESIAN_POINT ( 'NONE',  ( 8.000000000000000000, -34.90625000000000000, -3.313708498984761608 ) ) ;
#8092 = CARTESIAN_POINT ( 'NONE',  ( 6.289692432696784685, -1.240516797660047330E-13, -6.828989928337167115 ) ) ;
#8093 = VERTEX_POINT ( 'NONE', #15166 ) ;
#8094 = CARTESIAN_POINT ( 'NONE',  ( 82.21186757432916181, -49.98570124988022201, 178.5498643125555702 ) ) ;
#8096 = AXIS2_PLACEMENT_3D ( 'NONE', #95213, #88702, #54185 ) ;
#8095 = CARTESIAN_POINT ( 'NONE',  ( 5.833333333333329485, -46.00000000000000000, 103.8776713793258608 ) ) ;
#8097 = CARTESIAN_POINT ( 'NONE',  ( -41.20375261497546404, 436.5366665730131785, 21.37241632499251764 ) ) ;
#8098 = VERTEX_POINT ( 'NONE', #98207 ) ;
#8099 = CARTESIAN_POINT ( 'NONE',  ( 19.70764564238371719, 304.7954121406193622, 9.925013215726785631 ) ) ;
#8100 = CARTESIAN_POINT ( 'NONE',  ( -32.89862776688993762, 464.9311084009894444, 10.99515925127032467 ) ) ;
#8101 = PRESENTATION_STYLE_ASSIGNMENT (( #81979 ) ) ;
#8102 = CARTESIAN_POINT ( 'NONE',  ( -46.86302342948793864, 41.03834671688476732, -46.07399435196477100 ) ) ;
#8103 = COLOUR_RGB ( '', 0.08235294, 0.09019608, 0.10196078) ;
#8104 = CARTESIAN_POINT ( 'NONE',  ( -28.56337834059306857, 13.37291324415824967, -40.29174292248585942 ) ) ;
#8105 =( NAMED_UNIT ( * ) SI_UNIT ( $, .STERADIAN. ) SOLID_ANGLE_UNIT ( ) );
#8106 = CARTESIAN_POINT ( 'NONE',  ( 38.11263331122286502, 25.30373840940857733, 13.33358277375596934 ) ) ;
#8107 = SURFACE_SIDE_STYLE ('',( #48562 ) ) ;
#8109 = CARTESIAN_POINT ( 'NONE',  ( -13.59364004637736123, 24.77274705659938547, 0.5873110997852482029 ) ) ;
#8108 = CARTESIAN_POINT ( 'NONE',  ( -8.467721648720655025, -19.61993625497054694, 35.26688575358691935 ) ) ;
#8110 = EDGE_CURVE ( 'NONE', #47541, #96607, #88104, .T. ) ;
#8111 = CARTESIAN_POINT ( 'NONE',  ( -5.082755093536326818, -13.71875000204838457, 5.082755093536325042 ) ) ;
#8112 = CARTESIAN_POINT ( 'NONE',  ( 6.516354785991091835E-11, 40.83842593836580903, 65.00000000086684793 ) ) ;
#8113 = CARTESIAN_POINT ( 'NONE',  ( -6.318250223874061420E-16, 9.147862274876551680, -8.047472243342934206 ) ) ;
#8114 = EDGE_LOOP ( 'NONE', ( #70024, #74343, #13491, #10170, #36410 ) ) ;
#8115 = AXIS2_PLACEMENT_3D ( 'NONE', #65937, #6098, #97236 ) ;
#8116 = ORIENTED_EDGE ( 'NONE', *, *, #94745, .F. ) ;
#8117 = CARTESIAN_POINT ( 'NONE',  ( -17.50000000000100897, 49.16280683614362346, 62.52714020843506404 ) ) ;
#8118 = CARTESIAN_POINT ( 'NONE',  ( 7.499999999999999112, 4.652409454067512051, -7.929128589908465585 ) ) ;
#8119 = FACE_OUTER_BOUND ( 'NONE', #60005, .T. ) ;
#8120 = EDGE_CURVE ( 'NONE', #52389, #93666, #55347, .T. ) ;
#8121 = CARTESIAN_POINT ( 'NONE',  ( 4.981862520314373377, 0.000000000000000000, -0.01270000000000090501 ) ) ;
#8123 = CARTESIAN_POINT ( 'NONE',  ( 65.50959194424925158, -21.77022000568248927, -21.27195586255206194 ) ) ;
#8122 = CARTESIAN_POINT ( 'NONE',  ( 4.080491234651538512, 53.97779284277786616, 7.633990763273022395 ) ) ;
#8124 = EDGE_LOOP ( 'NONE', ( #17862, #35310, #103852, #28932, #19631 ) ) ;
#8125 = CARTESIAN_POINT ( 'NONE',  ( -5.999511540169428336, -88.99926730885431425, -0.2833228702578375335 ) ) ;
#8126 = CARTESIAN_POINT ( 'NONE',  ( -4.188615833753505768, 52.12906257371965779, 6.684248842317088268 ) ) ;
#8127 = STYLED_ITEM ( 'NONE', ( #75941 ), #26207 ) ;
#8128 = CIRCLE ( 'NONE', #87387, 4.000000000000000888 ) ;
#8129 = ORIENTED_EDGE ( 'NONE', *, *, #30072, .F. ) ;
#8130 = PRESENTATION_STYLE_ASSIGNMENT (( #90122 ) ) ;
#8131 = CYLINDRICAL_SURFACE ( 'NONE', #22679, 5.000000000000000888 ) ;
#8132 = CARTESIAN_POINT ( 'NONE',  ( -30.67017305325112275, 40.99855314031348286, -65.37930749121261442 ) ) ;
#8133 = CARTESIAN_POINT ( 'NONE',  ( -98.13052083946277548, -59.99999999999999289, 69.73258326240120653 ) ) ;
#8134 = AXIS2_PLACEMENT_3D ( 'NONE', #7544, #14048, #38369 ) ;
#8135 = CONICAL_SURFACE ( 'NONE', #102943, 8.000000000000000000, 0.9599310885968911355 ) ;
#8136 = CARTESIAN_POINT ( 'NONE',  ( 28.43341640144443616, 17.76796145515717384, -40.78017990900054457 ) ) ;
#8137 = AXIS2_PLACEMENT_3D ( 'NONE', #52860, #28097, #85788 ) ;
#8138 = CARTESIAN_POINT ( 'NONE',  ( -2.303522549047186516E-06, -22.06787374684229874, 27.56762891740942578 ) ) ;
#8139 = COLOUR_RGB ( '', 0.08235294, 0.09019608, 0.10196078) ;
#8140 = PLANE ( 'NONE',  #15669 ) ;
#8141 = FACE_OUTER_BOUND ( 'NONE', #14606, .T. ) ;
#8143 = CARTESIAN_POINT ( 'NONE',  ( -6.464976092152494580, 41.32132943617850174, -58.37832475197549797 ) ) ;
#8142 = CARTESIAN_POINT ( 'NONE',  ( -6.145467200813103936, -5.000000000008177459, -92.99666842290147883 ) ) ;
#8144 = EDGE_CURVE ( 'NONE', #57214, #1618, #77783, .T. ) ;
#8145 = CARTESIAN_POINT ( 'NONE',  ( -84.12058219282783966, -35.94476431650669213, 174.7674332474302048 ) ) ;
#8146 = ORIENTED_EDGE ( 'NONE', *, *, #71855, .F. ) ;
#8147 = AXIS2_PLACEMENT_3D ( 'NONE', #6624, #71894, #62761 ) ;
#8148 = VERTEX_POINT ( 'NONE', #85778 ) ;
#8149 = ORIENTED_EDGE ( 'NONE', *, *, #6867, .F. ) ;
#8150 = STYLED_ITEM ( 'NONE', ( #88848 ), #8942 ) ;
#8151 = CARTESIAN_POINT ( 'NONE',  ( -44.14911905790387436, 464.3766534541992996, 9.623404994945699897 ) ) ;
#8152 = EDGE_CURVE ( 'NONE', #63779, #74653, #101928, .T. ) ;
#8153 = CARTESIAN_POINT ( 'NONE',  ( 34.10284876471455817, -5.000000000000000888, 6.123233995736769241E-16 ) ) ;
#8154 = ORIENTED_EDGE ( 'NONE', *, *, #11882, .T. ) ;
#8155 = CARTESIAN_POINT ( 'NONE',  ( 69.67238219402268840, -4.000000000000000888, 4.898587196589422689E-16 ) ) ;
#8156 = CARTESIAN_POINT ( 'NONE',  ( -14.05937931246655026, -57.67120694556813731, -44.20476115079929258 ) ) ;
#8157 = CARTESIAN_POINT ( 'NONE',  ( 6.275044998973871913, 53.84125641896091707, 6.495149306109316178 ) ) ;
#8158 = CARTESIAN_POINT ( 'NONE',  ( 8.361479372589355918, 30.82354577482341895, -1.227442566772675775E-12 ) ) ;
#8159 = CARTESIAN_POINT ( 'NONE',  ( 4.692671595817627939, -5.000000000000000000, -97.18017958146204194 ) ) ;
#8160 = DIRECTION ( 'NONE',  ( -1.000000000000000000, -0.000000000000000000, -0.000000000000000000 ) ) ;
#8161 = CARTESIAN_POINT ( 'NONE',  ( 112.0515757376121542, -60.00000000000002842, 140.8507904390172598 ) ) ;
#8162 = CARTESIAN_POINT ( 'NONE',  ( -109.5675793427969040, -29.99999999999999289, 170.1817020036065742 ) ) ;
#8163 = CARTESIAN_POINT ( 'NONE',  ( -62.60069042062036004, -29.05980936889960020, 74.09822019150450956 ) ) ;
#8164 = AXIS2_PLACEMENT_3D ( 'NONE', #22312, #20208, #44984 ) ;
#8165 = ORIENTED_EDGE ( 'NONE', *, *, #77851, .F. ) ;
#8166 = FACE_OUTER_BOUND ( 'NONE', #88022, .T. ) ;
#8167 = CARTESIAN_POINT ( 'NONE',  ( 113.9027919867113923, -60.00000000001953282, 157.6317976075506238 ) ) ;
#8168 = ORIENTED_EDGE ( 'NONE', *, *, #48102, .T. ) ;
#8169 = CARTESIAN_POINT ( 'NONE',  ( 0.9942926288455912198, -29.02944133723623921, 28.72789018247508608 ) ) ;
#8170 = CARTESIAN_POINT ( 'NONE',  ( -5.082755093536326818, -14.09375000204838457, 5.082755093536325042 ) ) ;
#8171 =( NAMED_UNIT ( * ) PLANE_ANGLE_UNIT ( ) SI_UNIT ( $, .RADIAN. ) );
#8172 = EDGE_LOOP ( 'NONE', ( #12389, #50517, #66629, #30330 ) ) ;
#8173 = VECTOR ( 'NONE', #88452, 1000.000000000000114 ) ;
#8174 = DIRECTION ( 'NONE',  ( 0.000000000000000000, -1.000000000000000000, 0.000000000000000000 ) ) ;
#8175 = ORIENTED_EDGE ( 'NONE', *, *, #47294, .F. ) ;
#8176 = ADVANCED_FACE ( 'NONE', ( #18936 ), #93098, .T. ) ;
#8177 = CARTESIAN_POINT ( 'NONE',  ( -110.5340683299488234, -60.00000000000001421, 189.3070748394261500 ) ) ;
#8178 = CARTESIAN_POINT ( 'NONE',  ( 9.215420734788356327, -54.00000000000000000, 23.11721482942554928 ) ) ;
#8179 = CARTESIAN_POINT ( 'NONE',  ( 2.977408999572650927, -25.25000000204839523, -7.188101187500001821 ) ) ;
#8180 = CARTESIAN_POINT ( 'NONE',  ( 46.00000000000000000, 459.9277931459795354, 6.461582622334325343 ) ) ;
#8181 = CIRCLE ( 'NONE', #15107, 5.000000000000001776 ) ;
#8182 = CARTESIAN_POINT ( 'NONE',  ( 17.73120223245296856, 43.18351831125497853, -6.029418843961513730 ) ) ;
#8183 = DIRECTION ( 'NONE',  ( -1.000000000000000000, -1.224606353822377258E-16, -0.000000000000000000 ) ) ;
#8184 = CARTESIAN_POINT ( 'NONE',  ( 13.50000000000000355, -7.794228634059974681, -13.00000000000000000 ) ) ;
#8185 = DIRECTION ( 'NONE',  ( -0.000000000000000000, 1.000000000000000000, -0.000000000000000000 ) ) ;
#8186 =( NAMED_UNIT ( * ) PLANE_ANGLE_UNIT ( ) SI_UNIT ( $, .RADIAN. ) );
#8187 = CARTESIAN_POINT ( 'NONE',  ( -24.43733964430245464, 27.40365649514079394, 32.24112188980101479 ) ) ;
#8188 = DIRECTION ( 'NONE',  ( -0.5735764363510512664, 0.8191520442889881348, 1.003171929053520309E-16 ) ) ;
#8189 = CARTESIAN_POINT ( 'NONE',  ( -33.54301527992964793, -46.43411393437603607, 35.89697790901694674 ) ) ;
#8190 = CARTESIAN_POINT ( 'NONE',  ( 40.77236552497750921, -29.15239929701842669, 36.95769491155581932 ) ) ;
#8191 = DIRECTION ( 'NONE',  ( 0.000000000000000000, -1.000000000000000000, 0.000000000000000000 ) ) ;
#8192 = ORIENTED_EDGE ( 'NONE', *, *, #51398, .T. ) ;
#8194 = AXIS2_PLACEMENT_3D ( 'NONE', #38587, #73436, #70417 ) ;
#8193 = CARTESIAN_POINT ( 'NONE',  ( 44.21332904831284338, 435.2494715644501184, 14.45449769377390581 ) ) ;
#8195 = CARTESIAN_POINT ( 'NONE',  ( -80.08624693268845363, -38.78840980346092238, 193.1431129205759305 ) ) ;
#8196 = ORIENTED_EDGE ( 'NONE', *, *, #5359, .T. ) ;
#8197 = CARTESIAN_POINT ( 'NONE',  ( 4.852941176470592310, -3.000000000000002665, -70.80672828634229177 ) ) ;
#8198 = CARTESIAN_POINT ( 'NONE',  ( -11.54938679239317345, 7.303627399110830254, 9.359616978869953030 ) ) ;
#8199 = CARTESIAN_POINT ( 'NONE',  ( -49.22360526642673051, 7.740778690624813940, -15.97911514197237004 ) ) ;
#8200 = CARTESIAN_POINT ( 'NONE',  ( -7.190574406385736417, 41.61619605049727255, -59.53992226565166135 ) ) ;
#8201 = CARTESIAN_POINT ( 'NONE',  ( 18.09999999999999787, 3.309500000000003439, 4.052968581778167743E-16 ) ) ;
#8202 = CARTESIAN_POINT ( 'NONE',  ( -37.56673239365849781, 25.47613764497371136, 13.45617127781066280 ) ) ;
#8204 = CIRCLE ( 'NONE', #37507, 5.000000000000011546 ) ;
#8203 = CARTESIAN_POINT ( 'NONE',  ( 4.472135954999579610, -85.00000000000000000, -4.000000000000001776 ) ) ;
#8205 = CARTESIAN_POINT ( 'NONE',  ( 0.000000000000000000, 43.00000000000000000, 0.000000000000000000 ) ) ;
#8206 = CARTESIAN_POINT ( 'NONE',  ( 110.9949313104018529, -60.00000000000000711, 152.0878044361085699 ) ) ;
#8207 = CIRCLE ( 'NONE', #34123, 1.000000000000001998 ) ;
#8208 = CARTESIAN_POINT ( 'NONE',  ( -0.7777777777777781232, -54.00000000000000711, 40.97837836547555668 ) ) ;
#8209 = PRESENTATION_STYLE_ASSIGNMENT (( #42171 ) ) ;
#8210 = ORIENTED_EDGE ( 'NONE', *, *, #38510, .T. ) ;
#8211 = EDGE_CURVE ( 'NONE', #98501, #23399, #41662, .T. ) ;
#8212 = CARTESIAN_POINT ( 'NONE',  ( -87.91185205471116149, -30.00000000000008171, 186.5683232776123930 ) ) ;
#8213 = ORIENTED_EDGE ( 'NONE', *, *, #36258, .F. ) ;
#8214 = CARTESIAN_POINT ( 'NONE',  ( -9.901690565149895207, -57.79096752242128332, 28.42036373910763558 ) ) ;
#8215 = CARTESIAN_POINT ( 'NONE',  ( -15.94096206886600875, 3.082184004823651957, -0.3571785271768571635 ) ) ;
#8216 = CARTESIAN_POINT ( 'NONE',  ( 9.300689189976646176, 140.6377497889584447, 5.000000000000000000 ) ) ;
#8217 = CARTESIAN_POINT ( 'NONE',  ( 15.59999999999999787, 1.533819458162526451E-15, 0.000000000000000000 ) ) ;
#8218 = CARTESIAN_POINT ( 'NONE',  ( -22.37441460685026229, 28.20471216883542809, -31.02949312230854417 ) ) ;
#8219 = AXIS2_PLACEMENT_3D ( 'NONE', #99821, #91745, #51258 ) ;
#8220 = CARTESIAN_POINT ( 'NONE',  ( 2.977408999572651815, -27.31250000204838457, 7.188101187500000933 ) ) ;
#8222 = EDGE_CURVE ( 'NONE', #66339, #31268, #41425, .T. ) ;
#8221 = DIRECTION ( 'NONE',  ( 0.000000000000000000, -1.000000000000000000, 0.000000000000000000 ) ) ;
#8223 = CARTESIAN_POINT ( 'NONE',  ( 6.930184121914609641, 41.27136526567599617, -70.62329949176377397 ) ) ;
#8224 = VERTEX_POINT ( 'NONE', #28088 ) ;
#8225 = AXIS2_PLACEMENT_3D ( 'NONE', #44438, #3977, #56067 ) ;
#8227 = ORIENTED_EDGE ( 'NONE', *, *, #99870, .F. ) ;
#8226 = CARTESIAN_POINT ( 'NONE',  ( 83.86866073052654258, 1.030564683017419500E-14, 0.000000000000000000 ) ) ;
#8228 = CARTESIAN_POINT ( 'NONE',  ( 80.86233901923861822, -46.43849059710549199, 160.9666562290477430 ) ) ;
#8229 = SURFACE_STYLE_USAGE ( .BOTH. , #74551 ) ;
#8230 =( NAMED_UNIT ( * ) SI_UNIT ( $, .STERADIAN. ) SOLID_ANGLE_UNIT ( ) );
#8231 = ORIENTED_EDGE ( 'NONE', *, *, #88367, .F. ) ;
#8232 = CARTESIAN_POINT ( 'NONE',  ( -14.99580413333973539, 1.250310433696842249, 0.8744943966991981510 ) ) ;
#8233 = CARTESIAN_POINT ( 'NONE',  ( 2.977408999572650927, -11.37500000204838635, -7.188101187500000933 ) ) ;
#8234 = CARTESIAN_POINT ( 'NONE',  ( 7.002619243997879828, 28.94992681986182248, -3.868708944012997808 ) ) ;
#8235 = CARTESIAN_POINT ( 'NONE',  ( -48.45695174840996344, -59.99999999999997158, -32.35430574311584451 ) ) ;
#8236 = CARTESIAN_POINT ( 'NONE',  ( -25.66200995656152273, 305.1858995196985802, 10.45951546437543733 ) ) ;
#8237 =( LENGTH_UNIT ( ) NAMED_UNIT ( * ) SI_UNIT ( .MILLI., .METRE. ) );
#8238 = EDGE_LOOP ( 'NONE', ( #86373, #25861, #26791, #86002 ) ) ;
#8239 = CIRCLE ( 'NONE', #61628, 4.171999999999999709 ) ;
#8240 = CARTESIAN_POINT ( 'NONE',  ( 3.641358249959614657, 129.8026804635382234, 5.000000000000000888 ) ) ;
#8241 = DIRECTION ( 'NONE',  ( 0.000000000000000000, -1.000000000000000000, 0.000000000000000000 ) ) ;
#8242 = CARTESIAN_POINT ( 'NONE',  ( 0.1685512285012792377, 34.17188553058026912, -29.75000000000017408 ) ) ;
#8243 = EDGE_CURVE ( 'NONE', #59988, #65549, #36187, .T. ) ;
#8244 = CARTESIAN_POINT ( 'NONE',  ( 7.188101187499999156, -31.25000000204838813, 2.977408999572654924 ) ) ;
#8245 = CARTESIAN_POINT ( 'NONE',  ( 22.50849985115188545, -27.35376444295244625, 37.47483747969673118 ) ) ;
#8246 = CARTESIAN_POINT ( 'NONE',  ( 2.500000000000013767, -30.00000000000000355, -31.87333685190803223 ) ) ;
#8247 = ADVANCED_FACE ( 'NONE', ( #35646 ), #19476, .T. ) ;
#8248 = CARTESIAN_POINT ( 'NONE',  ( 40.98595185921475803, 438.0930894115431897, 22.33269956591867356 ) ) ;
#8249 = APPLICATION_PROTOCOL_DEFINITION ( 'draft international standard', 'automotive_design', 1998, #10721 ) ;
#8250 = CARTESIAN_POINT ( 'NONE',  ( 48.69610342378920365, 8.416294429711179248, 16.66514711138992766 ) ) ;
#8251 = ORIENTED_EDGE ( 'NONE', *, *, #84159, .F. ) ;
#8252 = FACE_OUTER_BOUND ( 'NONE', #11027, .T. ) ;
#8253 = CARTESIAN_POINT ( 'NONE',  ( 104.0908829527487711, 5.000000000000021316, 0.000000000000000000 ) ) ;
#8254 = CARTESIAN_POINT ( 'NONE',  ( -3.454253436624922458, -49.15858197120396511, 103.7259032015043090 ) ) ;
#8255 = EDGE_CURVE ( 'NONE', #100726, #74863, #98240, .T. ) ;
#8256 = CARTESIAN_POINT ( 'NONE',  ( 34.12349128637390550, 490.1895789250395978, 12.63944770676189933 ) ) ;
#8257 = VERTEX_POINT ( 'NONE', #60444 ) ;
#8258 = CIRCLE ( 'NONE', #87503, 4.000000000000000000 ) ;
#8259 = SURFACE_STYLE_USAGE ( .BOTH. , #41172 ) ;
#8260 = CARTESIAN_POINT ( 'NONE',  ( 112.0975676531185030, -57.67108666598051059, 191.0081396353801040 ) ) ;
#8261 = CIRCLE ( 'NONE', #34111, 3.309500000000001663 ) ;
#8262 = CARTESIAN_POINT ( 'NONE',  ( 37.43130592803709078, 464.0780360860962901, 19.48660943767455223 ) ) ;
#8263 = FACE_OUTER_BOUND ( 'NONE', #76176, .T. ) ;
#8264 = DIRECTION ( 'NONE',  ( 0.000000000000000000, 1.000000000000000000, 0.000000000000000000 ) ) ;
#8265 = CARTESIAN_POINT ( 'NONE',  ( 36.95213568995131226, 25.70510572952699846, 13.30629215880022542 ) ) ;
#8266 = CARTESIAN_POINT ( 'NONE',  ( -76.28233775379571568, -60.00000000000000000, 188.0959844134463310 ) ) ;
#8267 = CARTESIAN_POINT ( 'NONE',  ( -38.68218982724705057, 320.0845437455996603, 16.10279619727025135 ) ) ;
#8268 = EDGE_CURVE ( 'NONE', #60267, #86235, #49205, .T. ) ;
#8269 = CARTESIAN_POINT ( 'NONE',  ( -33.56345473223404241, 299.9083031499212666, -8.874823776838020706 ) ) ;
#8270 =( GEOMETRIC_REPRESENTATION_CONTEXT ( 3 ) GLOBAL_UNCERTAINTY_ASSIGNED_CONTEXT ( ( #24646 ) ) GLOBAL_UNIT_ASSIGNED_CONTEXT ( ( #17419, #75087, #68081 ) ) REPRESENTATION_CONTEXT ( 'NONE', 'WORKASPACE' ) );
#8271 = CARTESIAN_POINT ( 'NONE',  ( -86.06194670869818708, -28.35369527726857442, 182.3419248918959852 ) ) ;
#8272 = EDGE_LOOP ( 'NONE', ( #72872, #75943, #27788, #39354 ) ) ;
#8273 = CARTESIAN_POINT ( 'NONE',  ( 29.15784866723035051, 310.4008174516520171, -7.717995496960369906 ) ) ;
#8274 =( BOUNDED_SURFACE ( )  B_SPLINE_SURFACE ( 3, 2, ( 
 ( #53320, #78117, #102929 ),
 ( #86769, #98016, #64083 ),
 ( #32783, #91006, #55929 ),
 ( #88871, #41902, #96958 ) ),
 .UNSPECIFIED., .F., .F., .F. ) 
 B_SPLINE_SURFACE_WITH_KNOTS ( ( 4, 4 ),
 ( 3, 3 ),
 ( 6.071532165918824830E-18, 0.002491432948284471368 ),
 ( 0.000000000000000000, 1.000000000000000000 ),
 .UNSPECIFIED. ) 
 GEOMETRIC_REPRESENTATION_ITEM ( )  RATIONAL_B_SPLINE_SURFACE ( (
 ( 1.000000000000000000, 0.7978714159192654698, 1.000000000000000000),
 ( 1.000000000000000000, 0.8097755972629270271, 1.000000000000000000),
 ( 1.000000000000000000, 0.8213938805858149728, 1.000000000000000000),
 ( 1.000000000000000000, 0.8328393170029660952, 1.000000000000000000) ) ) 
 REPRESENTATION_ITEM ( '' )  SURFACE ( )  );
#8275 = ORIENTED_EDGE ( 'NONE', *, *, #68395, .F. ) ;
#8276 = CARTESIAN_POINT ( 'NONE',  ( -8.000086790516059310, -14.00017358106007137, 0.2639471549312823462 ) ) ;
#8277 = EDGE_CURVE ( 'NONE', #78054, #84082, #70995, .T. ) ;
#8278 = DIRECTION ( 'NONE',  ( -1.000000000000000000, -1.224606353822377258E-16, -0.000000000000000000 ) ) ;
#8279 = CARTESIAN_POINT ( 'NONE',  ( -85.48360261714907438, -52.75149282529780947, -10.94374517246983025 ) ) ;
#8280 = DIRECTION ( 'NONE',  ( 0.000000000000000000, -1.000000000000000000, 0.000000000000000000 ) ) ;
#8281 = DIRECTION ( 'NONE',  ( 0.8191520442889974607, 1.003171929053531649E-16, -0.5735764363510379438 ) ) ;
#8282 = AXIS2_PLACEMENT_3D ( 'NONE', #11201, #77018, #5266 ) ;
#8283 = ORIENTED_EDGE ( 'NONE', *, *, #52147, .F. ) ;
#8285 = DIRECTION ( 'NONE',  ( 0.000000000000000000, -1.000000000000000000, 0.000000000000000000 ) ) ;
#8284 = AXIS2_PLACEMENT_3D ( 'NONE', #50459, #82305, #40782 ) ;
#8286 = DIRECTION ( 'NONE',  ( 6.051620703560613215E-16, 0.3488521823429523994, -0.9371777605526925292 ) ) ;
#8287 = EDGE_CURVE ( 'NONE', #84621, #33159, #69582, .T. ) ;
#8288 = CARTESIAN_POINT ( 'NONE',  ( 4.453875240779016309, -1.734723475976807094E-15, -16.57301948837565675 ) ) ;
#8289 = SURFACE_STYLE_USAGE ( .BOTH. , #82173 ) ;
#8290 = CARTESIAN_POINT ( 'NONE',  ( 53.63839714946880832, -30.00000000000003553, -34.46733499188162853 ) ) ;
#8291 = CARTESIAN_POINT ( 'NONE',  ( -77.45270157673813571, -42.96733943251651056, 134.7326920116138922 ) ) ;
#8292 = VERTEX_POINT ( 'NONE', #4838 ) ;
#8293 = CARTESIAN_POINT ( 'NONE',  ( 77.87328754808491738, -14.21045842199420228, 157.7472683744473159 ) ) ;
#8294 = CARTESIAN_POINT ( 'NONE',  ( 7.619135598915500296, 88.17305367784679504, 2.449260492474792716 ) ) ;
#8295 = CARTESIAN_POINT ( 'NONE',  ( 113.0765498504955247, -57.67120308272065898, 186.9763648898224915 ) ) ;
#8296 = COLOUR_RGB ( '', 0.31764706, 0.68627451, 0.89019608) ;
#8297 = VERTEX_POINT ( 'NONE', #21065 ) ;
#8298 = CARTESIAN_POINT ( 'NONE',  ( 28.32642421089389728, 34.16878765831202713, 9.122000601312000967 ) ) ;
#8299 = DIRECTION ( 'NONE',  ( -1.000000000000000000, -1.224606353822377258E-16, -0.000000000000000000 ) ) ;
#8300 = ORIENTED_EDGE ( 'NONE', *, *, #28946, .F. ) ;
#8301 = B_SPLINE_CURVE_WITH_KNOTS ( 'NONE', 3,
 ( #5656, #64440, #4608, #97314, #29450, #54720, #58461, #90833, #17484, #24531, #99424, #8304, #25054, #89771, #105931, #41737, #8833, #16948, #56849, #41208 ),
 .UNSPECIFIED., .F., .F.,
 ( 4, 2, 2, 2, 2, 2, 2, 2, 2, 4 ),
 ( 0.007810650867913536757, 0.008315688271542333657, 0.008820725675171128821, 0.009073244376985522067, 0.009325763078799911843, 0.009830800482428691395, 0.01033583788605746748, 0.01084087528968624703, 0.01134591269331502485, 0.01185095009694380266 ),
 .UNSPECIFIED. ) ;
#8302 = CARTESIAN_POINT ( 'NONE',  ( 3.972805511173104875, 17.31670332531925283, -5.763756076061313571 ) ) ;
#8303 = DIRECTION ( 'NONE',  ( 0.000000000000000000, 0.000000000000000000, 1.000000000000000000 ) ) ;
#8304 = CARTESIAN_POINT ( 'NONE',  ( 15.39690552766064613, 44.03715051710484119, 5.599647415943061368 ) ) ;
#8305 = CARTESIAN_POINT ( 'NONE',  ( -1.320432766682874540E-15, -19.53125000204838457, 7.188101187500000044 ) ) ;
#8306 = CARTESIAN_POINT ( 'NONE',  ( 99.17777777777777715, -4.171999999999998820, 0.000000000000000000 ) ) ;
#8307 = SURFACE_STYLE_USAGE ( .BOTH. , #82190 ) ;
#8308 = CARTESIAN_POINT ( 'NONE',  ( 4.250000000000000000, 0.000000000000000000, -9.449444346342716017 ) ) ;
#8309 = DIRECTION ( 'NONE',  ( 0.000000000000000000, -1.000000000000000000, 0.000000000000000000 ) ) ;
#8310 = AXIS2_PLACEMENT_3D ( 'NONE', #62683, #53520, #46488 ) ;
#8311 = ORIENTED_EDGE ( 'NONE', *, *, #69339, .F. ) ;
#8312 = CARTESIAN_POINT ( 'NONE',  ( -7.044111875035700798, 41.04202977231933147, -70.72791807316478696 ) ) ;
#8314 = CARTESIAN_POINT ( 'NONE',  ( 29.95423130063162986, -42.95837386160915372, 33.73428810424631763 ) ) ;
#8313 = DIRECTION ( 'NONE',  ( 0.000000000000000000, -1.000000000000000000, 0.000000000000000000 ) ) ;
#8315 = CARTESIAN_POINT ( 'NONE',  ( -4.189401774500377762, 52.12935225592999444, -6.682816396052760233 ) ) ;
#8316 = EDGE_LOOP ( 'NONE', ( #30025, #45259, #76709, #69377 ) ) ;
#8317 = CARTESIAN_POINT ( 'NONE',  ( 0.000000000000000000, 2.999999999999992895, -7.000000000000024869 ) ) ;
#8318 = VECTOR ( 'NONE', #47721, 1000.000000000000114 ) ;
#8319 = ORIENTED_EDGE ( 'NONE', *, *, #102147, .F. ) ;
#8321 = CARTESIAN_POINT ( 'NONE',  ( 0.1699848995827469844, 52.17551178379408583, 7.758783086627383696 ) ) ;
#8320 = CARTESIAN_POINT ( 'NONE',  ( 0.000000000000000000, 7.960204194457794491E-16, -6.499999999999999112 ) ) ;
#8322 = CARTESIAN_POINT ( 'NONE',  ( 39.34999999999999432, 1.533819458162526451E-15, 0.000000000000000000 ) ) ;
#8323 = CARTESIAN_POINT ( 'NONE',  ( -9.740083726531054253, 294.6493269980090872, -10.04303756037258566 ) ) ;
#8324 = FACE_OUTER_BOUND ( 'NONE', #26455, .T. ) ;
#8325 = CARTESIAN_POINT ( 'NONE',  ( 0.08468841732357029750, 45.30391365246045154, 18.75000000000001066 ) ) ;
#8326 = LINE ( 'NONE', #41760, #72760 ) ;
#8328 = EDGE_LOOP ( 'NONE', ( #99980, #42592, #54426, #52255 ) ) ;
#8327 = AXIS2_PLACEMENT_3D ( 'NONE', #79707, #30662, #87285 ) ;
#8329 = CARTESIAN_POINT ( 'NONE',  ( 87.60640540356948236, -60.00000000000002132, -22.02487886544127704 ) ) ;
#8330 = CARTESIAN_POINT ( 'NONE',  ( -9.658328022721306638, 45.55814826547296548, 15.25063005797924021 ) ) ;
#8331 = CARTESIAN_POINT ( 'NONE',  ( -15.83718408913613374, -1.753567716153235923, 14.89780694040802267 ) ) ;
#8332 = CARTESIAN_POINT ( 'NONE',  ( 6.289692432696784685, 1.244853941008388061E-13, 6.828989928337166226 ) ) ;
#8333 = CARTESIAN_POINT ( 'NONE',  ( 47.14566430936571351, 12.03638540833419057, -16.50097935118144221 ) ) ;
#8334 = ORIENTED_EDGE ( 'NONE', *, *, #47314, .F. ) ;
#8335 = EDGE_CURVE ( 'NONE', #76065, #65523, #12379, .T. ) ;
#8336 = LINE ( 'NONE', #59033, #78038 ) ;
#8337 = ORIENTED_EDGE ( 'NONE', *, *, #73986, .F. ) ;
#8339 = B_SPLINE_CURVE_WITH_KNOTS ( 'NONE', 3,
 ( #23621, #56474, #74258, #7928, #99053, #90999, #72667, #97464, #89403, #31707, #106085, #105568, #74785, #81277, #7394, #81801, #335, #98534, #33842, #73178, #32233, #98008, #17110, #25220, #58074, #24162, #864, #82892, #57007, #89922, #66715, #8990, #23087, #55922 ),
 .UNSPECIFIED., .F., .F.,
 ( 4, 2, 2, 2, 2, 2, 2, 2, 2, 2, 2, 2, 2, 2, 2, 2, 4 ),
 ( 0.000000000000000000, 0.0007951492273476391814, 0.001590298454695278363, 0.002385447682042917544, 0.003180596909390556726, 0.003975746136738195907, 0.004770895364085835089, 0.005566044591433473403, 0.006361193818781111717, 0.007156343046128750031, 0.007951492273476388345, 0.008746641500824025792, 0.009541790728171663238, 0.01033693995551930069, 0.01113208918286693987, 0.01192723841021457558, 0.01272238763756221476 ),
 .UNSPECIFIED. ) ;
#8338 = AXIS2_PLACEMENT_3D ( 'NONE', #12377, #93844, #27561 ) ;
#8340 = ORIENTED_EDGE ( 'NONE', *, *, #3616, .T. ) ;
#8341 = CARTESIAN_POINT ( 'NONE',  ( 0.1686817482576933591, 53.39766064372319221, 10.25000000000005862 ) ) ;
#8342 = CARTESIAN_POINT ( 'NONE',  ( 31.73032761413494640, 329.8498846259531092, 16.53112576517208865 ) ) ;
#8343 = CARTESIAN_POINT ( 'NONE',  ( -36.41465019936182301, 334.9862706725128305, -2.190136381357836282 ) ) ;
#8344 = CARTESIAN_POINT ( 'NONE',  ( -2.907876107285823686, -69.03782668178834570, 13.00348232047688768 ) ) ;
#8345 = CARTESIAN_POINT ( 'NONE',  ( 2.705399370281704297, -49.45330424000481173, 103.4497616813456631 ) ) ;
#8347 = ADVANCED_FACE ( 'NONE', ( #5877, #53903, #70633, #79775, #95435 ), #93331, .T. ) ;
#8346 = CARTESIAN_POINT ( 'NONE',  ( 12.50000000000000355, 41.59226156894002457, -76.70843802411151557 ) ) ;
#8348 = CIRCLE ( 'NONE', #41067, 7.500000000000000888 ) ;
#8349 = VERTEX_POINT ( 'NONE', #45307 ) ;
#8350 = CARTESIAN_POINT ( 'NONE',  ( 30.90161637171750897, 8.443258198712152662, 41.14563328228290118 ) ) ;
#8351 = B_SPLINE_CURVE_WITH_KNOTS ( 'NONE', 3,
 ( #74134, #6755, #218, #105454, #31595, #40182, #64480, #57947, #81681, #15376, #73060, #7803, #56347, #80108, #15909, #90872, #97349, #39675, #23502, #24570, #89282, #104936, #48263, #40711, #64994, #33182, #66054, #16439, #105968, #8342, #6210, #98931, #97887, #73599, #39149, #31078, #72549, #63957, #96843, #22972, #24042, #32112, #88744, #56883, #14837, #89809, #47733, #90331 ),
 .UNSPECIFIED., .F., .F.,
 ( 4, 2, 2, 2, 2, 2, 2, 2, 2, 2, 2, 2, 2, 2, 2, 2, 2, 2, 2, 2, 2, 2, 2, 4 ),
 ( -6.000000001701573511E-08, 0.001117306459296872004, 0.002234672918593761000, 0.003352039377890650429, 0.004469405837187538991, 0.005586772296484427552, 0.006704138755781317849, 0.007821505215078206411, 0.008938871674375094972, 0.01117360459296873505, 0.01340833751156237687, 0.01787780334874965876, 0.02234726918593694239, 0.02681673502312422255, 0.03128620086031150965, 0.03575566669749879328, 0.04469459837187320095, 0.05363353004624760167, 0.07151139339499641701, 0.08045032506937090100, 0.08938925674374539887, 0.1072671200924942003, 0.1251449834412430295, 0.1430228467899918310 ),
 .UNSPECIFIED. ) ;
#8352 = ORIENTED_EDGE ( 'NONE', *, *, #36655, .T. ) ;
#8353 = DIRECTION ( 'NONE',  ( -1.000000000000000000, -1.224606353822377258E-16, -0.000000000000000000 ) ) ;
#8354 = CARTESIAN_POINT ( 'NONE',  ( -6.746558653882563483, -3.895127454922790999, -6.526045885145577152 ) ) ;
#8355 = CARTESIAN_POINT ( 'NONE',  ( 41.32430911664878437, 464.3530259918923662, 17.56657173514240711 ) ) ;
#8356 = AXIS2_PLACEMENT_3D ( 'NONE', #17616, #32751, #34354 ) ;
#8358 = VERTEX_POINT ( 'NONE', #86834 ) ;
#8357 = CARTESIAN_POINT ( 'NONE',  ( -47.21131606613124632, -59.99999999999997868, 52.59714937887711272 ) ) ;
#8359 = CARTESIAN_POINT ( 'NONE',  ( 69.72252812878896577, -56.85553266303294606, 111.2983125885081392 ) ) ;
#8360 = STYLED_ITEM ( 'NONE', ( #136 ), #68626 ) ;
#8361 = ORIENTED_EDGE ( 'NONE', *, *, #42042, .F. ) ;
#8362 = LINE ( 'NONE', #26196, #92688 ) ;
#8363 = CARTESIAN_POINT ( 'NONE',  ( -6.925180474901644345, 9.132181797818848423, 1.053794444618463721 ) ) ;
#8364 = CARTESIAN_POINT ( 'NONE',  ( -110.1907765348834403, -57.67120634471875462, 130.2639824976604643 ) ) ;
#8365 = ADVANCED_FACE ( 'NONE', ( #13437 ), #21576, .F. ) ;
#8366 = VERTEX_POINT ( 'NONE', #36717 ) ;
#8367 = CARTESIAN_POINT ( 'NONE',  ( 0.000000000000000000, 0.000000000000000000, -9.449444346342716017 ) ) ;
#8368 = AXIS2_PLACEMENT_3D ( 'NONE', #50334, #48734, #74609 ) ;
#8369 = CARTESIAN_POINT ( 'NONE',  ( -36.28158941437202145, 490.9587137816652671, 12.45622313966492101 ) ) ;
#8370 = CARTESIAN_POINT ( 'NONE',  ( -19.50000000000000000, 12.99999999999999289, -7.500000000000000000 ) ) ;
#8371 = CARTESIAN_POINT ( 'NONE',  ( -3.313708498984760720, -22.71875000409677270, -8.000000000000000000 ) ) ;
#8372 = CARTESIAN_POINT ( 'NONE',  ( -1.902012483059531411E-15, 5.788408252967903955, 2.974182810908594377 ) ) ;
#8373 = CARTESIAN_POINT ( 'NONE',  ( 32.94539137534210482, 488.0149952105423381, 9.145905951749446317 ) ) ;
#8374 =( LENGTH_UNIT ( ) NAMED_UNIT ( * ) SI_UNIT ( .MILLI., .METRE. ) );
#8375 = CARTESIAN_POINT ( 'NONE',  ( -10.03543110037283093, 7.449399144625812319, 0.000000000000000000 ) ) ;
#8376 = CARTESIAN_POINT ( 'NONE',  ( -3.364021409948656505, 294.8518027753228807, 9.936999415087239385 ) ) ;
#8377 = CARTESIAN_POINT ( 'NONE',  ( -1.005505455502474499, -29.99999999999999645, -7.776392279229293436 ) ) ;
#8378 = ORIENTED_EDGE ( 'NONE', *, *, #1576, .F. ) ;
#8379 = FILL_AREA_STYLE_COLOUR ( '', #98946 ) ;
#8380 = CARTESIAN_POINT ( 'NONE',  ( 44.21332904831284338, 435.2494715644500616, 14.45449769377396976 ) ) ;
#8381 = LINE ( 'NONE', #7310, #22132 ) ;
#8382 = CARTESIAN_POINT ( 'NONE',  ( -97.58700215924690724, -30.00000000000000000, 190.8409573115993112 ) ) ;
#8383 = ADVANCED_FACE ( 'NONE', ( #29677 ), #53358, .F. ) ;
#8384 = AXIS2_PLACEMENT_3D ( 'NONE', #78315, #96105, #38421 ) ;
#8385 = CIRCLE ( 'NONE', #25689, 6.500000000000000000 ) ;
#8386 = CARTESIAN_POINT ( 'NONE',  ( 2.342558418285032307, -49.77031626379333318, 44.62063500984325515 ) ) ;
#8387 = CARTESIAN_POINT ( 'NONE',  ( 70.36692166205514809, -57.68251006697582284, 157.0214156919219022 ) ) ;
#8389 = CARTESIAN_POINT ( 'NONE',  ( -9.773376050962504280, 53.39758879002604175, 3.091049154870361360 ) ) ;
#8388 = CARTESIAN_POINT ( 'NONE',  ( -1.219174438273753269, 25.73254055012321118, -39.18059869567464659 ) ) ;
#8390 = CIRCLE ( 'NONE', #79151, 5.000000000000011546 ) ;
#8391 = AXIS2_PLACEMENT_3D ( 'NONE', #5608, #5087, #38020 ) ;
#8392 = CARTESIAN_POINT ( 'NONE',  ( -40.36516081889102026, 459.8940149412733831, 1.928085546549958451 ) ) ;
#8393 = CARTESIAN_POINT ( 'NONE',  ( -0.6444474511539225459, 44.02069286197071563, 16.41606151047013640 ) ) ;
#8394 =( NAMED_UNIT ( * ) SI_UNIT ( $, .STERADIAN. ) SOLID_ANGLE_UNIT ( ) );
#8395 = CARTESIAN_POINT ( 'NONE',  ( -10.39312431003531856, -60.00000000000000711, 39.65367113221718398 ) ) ;
#8396 = CARTESIAN_POINT ( 'NONE',  ( 11.69515844949617644, 11.66155101967946983, 9.916752703385080636 ) ) ;
#8397 = VECTOR ( 'NONE', #25453, 999.9999999999998863 ) ;
#8398 = CARTESIAN_POINT ( 'NONE',  ( 37.72536826885050232, 463.3861702155475086, 19.97111768659700815 ) ) ;
#8399 = CARTESIAN_POINT ( 'NONE',  ( -86.73280396411435333, -42.80135120255732772, 189.5378547483240368 ) ) ;
#8400 = ORIENTED_EDGE ( 'NONE', *, *, #53247, .T. ) ;
#8401 = CARTESIAN_POINT ( 'NONE',  ( 18.95009564030317506, 49.33583170005577045, 62.02326760999128652 ) ) ;
#8402 = CARTESIAN_POINT ( 'NONE',  ( 4.699999999999999289, 3.752776749732553263, -6.499999999999999112 ) ) ;
#8403 = CARTESIAN_POINT ( 'NONE',  ( -7.130835401559076026, -39.47599328887858405, 30.45931887943757133 ) ) ;
#8405 = CARTESIAN_POINT ( 'NONE',  ( 4.472061920348587627, -67.30643333997242905, 13.71894798482393441 ) ) ;
#8404 = CARTESIAN_POINT ( 'NONE',  ( 0.8808064505786505904, -6.997019658119629781, -5.875704392893251082 ) ) ;
#8406 = EDGE_CURVE ( 'NONE', #18742, #9380, #22101, .T. ) ;
#8407 = ORIENTED_EDGE ( 'NONE', *, *, #44864, .T. ) ;
#8408 = CARTESIAN_POINT ( 'NONE',  ( 4.966176485634622217, 41.64999999999998437, -70.47555195150158625 ) ) ;
#8409 = CONICAL_SURFACE ( 'NONE', #22230, 8.500000000000000000, 0.7853981633974504994 ) ;
#8410 = CARTESIAN_POINT ( 'NONE',  ( -5.318172249955896547, -5.000000000000039968, -15.46996282977505999 ) ) ;
#8411 = CARTESIAN_POINT ( 'NONE',  ( 15.96818781713877122, 35.08569730947720444, 22.06864763194606738 ) ) ;
#8412 = CARTESIAN_POINT ( 'NONE',  ( 28.76128244818236013, 306.4537308956344077, -9.192937457247751354 ) ) ;
#8413 = CARTESIAN_POINT ( 'NONE',  ( 7.531577814756222656E-15, 48.00000000000000000, -61.50000000000000000 ) ) ;
#8414 = EDGE_CURVE ( 'NONE', #41582, #22823, #12166, .T. ) ;
#8415 =( LENGTH_UNIT ( ) NAMED_UNIT ( * ) SI_UNIT ( .MILLI., .METRE. ) );
#8416 = CARTESIAN_POINT ( 'NONE',  ( -43.71037717921252863, 462.3391554988666599, 4.824299547746595529 ) ) ;
#8417 = CARTESIAN_POINT ( 'NONE',  ( 113.7193001496157052, -60.00000000000001421, 185.6034734595149871 ) ) ;
#8418 = CARTESIAN_POINT ( 'NONE',  ( -28.21644434148578640, 308.7733337496239301, -9.112255642778066544 ) ) ;
#8419 = ORIENTED_EDGE ( 'NONE', *, *, #87474, .F. ) ;
#8420 = CARTESIAN_POINT ( 'NONE',  ( -4.160433058848811427, -29.99999999999997513, 6.232720532359338428 ) ) ;
#8421 = CARTESIAN_POINT ( 'NONE',  ( -9.177080501238330967, 250.5334694285427020, -3.972956046786637607 ) ) ;
#8422 = DIRECTION ( 'NONE',  ( -0.8400944247696989775, 0.000000000000000000, 0.5424401879201693477 ) ) ;
#8423 = DIRECTION ( 'NONE',  ( 0.000000000000000000, -1.000000000000000000, 0.000000000000000000 ) ) ;
#8424 = FACE_OUTER_BOUND ( 'NONE', #86846, .T. ) ;
#8425 = CARTESIAN_POINT ( 'NONE',  ( 6.463481858019718196, -7.246446802359425732, 1.128819432756289265 ) ) ;
#8426 = ORIENTED_EDGE ( 'NONE', *, *, #71393, .F. ) ;
#8427 = UNCERTAINTY_MEASURE_WITH_UNIT (LENGTH_MEASURE( 1.000000000000000082E-05 ), #25031, 'distance_accuracy_value', 'NONE');
#8428 = EDGE_CURVE ( 'NONE', #9982, #49600, #73654, .T. ) ;
#8429 = CARTESIAN_POINT ( 'NONE',  ( -5.656854249492381470, -22.06249999999999289, 5.656854249492379694 ) ) ;
#8430 = VERTEX_POINT ( 'NONE', #105638 ) ;
#8431 = DIRECTION ( 'NONE',  ( -1.000000000000000000, -1.224606353822377258E-16, -0.000000000000000000 ) ) ;
#8432 =( NAMED_UNIT ( * ) PLANE_ANGLE_UNIT ( ) SI_UNIT ( $, .RADIAN. ) );
#8433 = CARTESIAN_POINT ( 'NONE',  ( 9.268669127170699795, 46.19464124546547623, 13.41262564492488529 ) ) ;
#8434 = EDGE_LOOP ( 'NONE', ( #19804, #40270 ) ) ;
#8435 = CARTESIAN_POINT ( 'NONE',  ( 64.91565662647984425, 48.00000000000000000, 6.815324757469506167 ) ) ;
#8436 = CARTESIAN_POINT ( 'NONE',  ( 5.988549711970140521, -14.40160760345763435, 14.13124080977622476 ) ) ;
#8437 = CARTESIAN_POINT ( 'NONE',  ( -25.93098123902086982, -59.99999999999020872, 43.86977658264649449 ) ) ;
#8438 = CARTESIAN_POINT ( 'NONE',  ( 0.000000000000000000, 0.000000000000000000, 0.000000000000000000 ) ) ;
#8439 = VERTEX_POINT ( 'NONE', #24756 ) ;
#8440 = CARTESIAN_POINT ( 'NONE',  ( 109.4462915750694236, -60.00000000000001421, 192.7655176299684001 ) ) ;
#8442 = CARTESIAN_POINT ( 'NONE',  ( 13.27489365765825191, -25.54879520240182345, 28.22250578733302717 ) ) ;
#8441 = CARTESIAN_POINT ( 'NONE',  ( -105.6361520504002840, -30.00000000000002132, 194.5259906914266139 ) ) ;
#8443 = CIRCLE ( 'NONE', #96326, 4.000000000000007105 ) ;
#8444 = PRESENTATION_STYLE_ASSIGNMENT (( #82335 ) ) ;
#8445 = DIRECTION ( 'NONE',  ( 0.000000000000000000, 0.000000000000000000, -1.000000000000000000 ) ) ;
#8446 = CARTESIAN_POINT ( 'NONE',  ( -42.25929233593898715, -42.98302630092105403, 41.54187495367473559 ) ) ;
#8447 = DIRECTION ( 'NONE',  ( 0.000000000000000000, -1.000000000000000000, 0.000000000000000000 ) ) ;
#8448 = VERTEX_POINT ( 'NONE', #105123 ) ;
#8449 = SURFACE_STYLE_FILL_AREA ( #48893 ) ;
#8450 = AXIS2_PLACEMENT_3D ( 'NONE', #94386, #11305, #45303 ) ;
#8451 = CARTESIAN_POINT ( 'NONE',  ( 16.14595037822608603, 20.73084165115993827, 4.192529328850663539 ) ) ;
#8452 = CARTESIAN_POINT ( 'NONE',  ( 27.57151080649627417, 314.0751515626058676, 12.18133379269485239 ) ) ;
#8453 = LINE ( 'NONE', #89909, #21499 ) ;
#8454 = CARTESIAN_POINT ( 'NONE',  ( 20.21880305278364887, 304.8280059657581091, -9.005058168222342729 ) ) ;
#8455 = DIRECTION ( 'NONE',  ( 0.000000000000000000, 1.000000000000000000, 0.000000000000000000 ) ) ;
#8456 = ORIENTED_EDGE ( 'NONE', *, *, #106767, .F. ) ;
#8457 = CARTESIAN_POINT ( 'NONE',  ( 4.051286199644062336, -48.60127012969240923, 103.8758286790404952 ) ) ;
#8458 = ORIENTED_EDGE ( 'NONE', *, *, #95898, .T. ) ;
#8459 = CARTESIAN_POINT ( 'NONE',  ( 80.89399687007842488, -29.99999999999999289, -12.17736764248747861 ) ) ;
#8460 = CARTESIAN_POINT ( 'NONE',  ( 47.36715592893483517, 12.99186701195487537, 14.54160185453288001 ) ) ;
#8461 = UNCERTAINTY_MEASURE_WITH_UNIT (LENGTH_MEASURE( 1.000000000000000082E-05 ), #21937, 'distance_accuracy_value', 'NONE');
#8462 = CARTESIAN_POINT ( 'NONE',  ( 4.250000000000000000, 0.000000000000000000, -0.9215586320570148260 ) ) ;
#8463 = CARTESIAN_POINT ( 'NONE',  ( 94.31146389850853495, -30.00000000000000355, 113.8352357902896586 ) ) ;
#8464 = CARTESIAN_POINT ( 'NONE',  ( 25.59999999999999787, 1.533819458162526451E-15, 0.000000000000000000 ) ) ;
#8465 = ORIENTED_EDGE ( 'NONE', *, *, #19065, .T. ) ;
#8466 = ADVANCED_FACE ( 'NONE', ( #89476 ), #77072, .F. ) ;
#8467 = ORIENTED_EDGE ( 'NONE', *, *, #38306, .F. ) ;
#8468 = VERTEX_POINT ( 'NONE', #65726 ) ;
#8469 = CARTESIAN_POINT ( 'NONE',  ( 23.58349330513380337, 1.593028355512270567E-15, 0.000000000000000000 ) ) ;
#8470 = CARTESIAN_POINT ( 'NONE',  ( -6.478079992187136149, 41.41225026867109449, -70.77206710307365256 ) ) ;
#8471 = EDGE_CURVE ( 'NONE', #13222, #95845, #68531, .T. ) ;
#8472 = CARTESIAN_POINT ( 'NONE',  ( -32.16580085343982631, 416.1844688050518357, 25.51939514139120746 ) ) ;
#8473 = EDGE_CURVE ( 'NONE', #75630, #85144, #73589, .T. ) ;
#8475 = ORIENTED_EDGE ( 'NONE', *, *, #76436, .F. ) ;
#8474 = AXIS2_PLACEMENT_3D ( 'NONE', #94505, #86422, #68639 ) ;
#8476 = CARTESIAN_POINT ( 'NONE',  ( 9.381394091586567896, 107.0134960558160628, 3.465950112474264433 ) ) ;
#8477 = ORIENTED_EDGE ( 'NONE', *, *, #17687, .T. ) ;
#8478 = DIRECTION ( 'NONE',  ( 0.000000000000000000, 0.000000000000000000, 1.000000000000000000 ) ) ;
#8479 = CARTESIAN_POINT ( 'NONE',  ( 79.03758757855014494, -38.69423318788795996, 191.0234865722444511 ) ) ;
#8480 = CARTESIAN_POINT ( 'NONE',  ( 32.30597388339071330, 435.2336684711225985, 15.38768761833313903 ) ) ;
#8481 = CARTESIAN_POINT ( 'NONE',  ( 31.41235438697622584, 299.6634614727072972, 11.01818356005949440 ) ) ;
#8482 = CARTESIAN_POINT ( 'NONE',  ( 0.000000000000000000, 35.00000000000000000, 0.000000000000000000 ) ) ;
#8483 = CIRCLE ( 'NONE', #70479, 4.000000000000007105 ) ;
#8484 = CARTESIAN_POINT ( 'NONE',  ( 0.05533025579362397389, -4.993776679985862721, -4.350525068611871049 ) ) ;
#8485 = DIRECTION ( 'NONE',  ( 1.000000000000000000, 0.000000000000000000, 0.000000000000000000 ) ) ;
#8486 = CARTESIAN_POINT ( 'NONE',  ( -5.164787682159340143, -48.11244280217349001, 104.1470044518086837 ) ) ;
#8487 = DIRECTION ( 'NONE',  ( 0.000000000000000000, -1.000000000000000000, 0.000000000000000000 ) ) ;
#8488 = EDGE_CURVE ( 'NONE', #18153, #57343, #96834, .T. ) ;
#8489 = CARTESIAN_POINT ( 'NONE',  ( -30.00000000000000000, 450.0000000000002274, 13.20242257375370976 ) ) ;
#8490 = VERTEX_POINT ( 'NONE', #19751 ) ;
#8491 = CIRCLE ( 'NONE', #22316, 4.000000000000001776 ) ;
#8492 = CARTESIAN_POINT ( 'NONE',  ( -24.48781666683216685, 295.5147073160107425, 2.079262953486592735 ) ) ;
#8493 = CARTESIAN_POINT ( 'NONE',  ( 7.739116699011762357, 54.23361630046057513, -1.834387929005254048 ) ) ;
#8494 = UNCERTAINTY_MEASURE_WITH_UNIT (LENGTH_MEASURE( 1.000000000000000082E-05 ), #12194, 'distance_accuracy_value', 'NONE');
#8495 = SURFACE_STYLE_FILL_AREA ( #40336 ) ;
#8496 = CARTESIAN_POINT ( 'NONE',  ( -8.000000000000000000, -10.24999999999999112, -9.797174393178825657E-16 ) ) ;
#8497 = CARTESIAN_POINT ( 'NONE',  ( -13.53089024472542334, -21.84174497847139662, 35.70596031949021665 ) ) ;
#8498 = CARTESIAN_POINT ( 'NONE',  ( 8.090408256587625857, 295.7505182605545997, 5.908160356365994126 ) ) ;
#8499 = B_SPLINE_CURVE_WITH_KNOTS ( 'NONE', 3,
 ( #14773, #5113, #78989, #6686, #5632, #62301, #29938, #22909, #38044, #40124, #88155, #96779, #95193, #80566, #87627, #54695, #29425, #70905, #103795, #14238, #105392, #21326, #62822, #63889, #22387, #87104 ),
 .UNSPECIFIED., .F., .F.,
 ( 4, 2, 2, 2, 2, 2, 1, 1, 2, 2, 2, 2, 2, 4 ),
 ( 0.000000000000000000, 0.06250000000001112999, 0.1250000000000222600, 0.2500000000000450751, 0.3750000000000678901, 0.4375000000000812683, 0.4687500000000897060, 0.4843750000000930922, 0.4921875000000922040, 0.5000000000000912603, 0.6250000000000683897, 0.7500000000000456302, 0.8750000000000227596, 1.000000000000000000 ),
 .UNSPECIFIED. ) ;
#8500 = CARTESIAN_POINT ( 'NONE',  ( -16.64348903516521005, -1.200000000000000030E-05, -5.407797401561534656 ) ) ;
#8501 = CARTESIAN_POINT ( 'NONE',  ( 86.39215313046445033, -17.36952503152258842, 179.6808971095037748 ) ) ;
#8502 = CARTESIAN_POINT ( 'NONE',  ( -76.12537862032631608, -38.35598417008158378, -28.58435412235099804 ) ) ;
#8503 = CARTESIAN_POINT ( 'NONE',  ( -9.229740628749548037, 139.8534222827520068, -1.734723476015833818E-15 ) ) ;
#8504 = ORIENTED_EDGE ( 'NONE', *, *, #42229, .T. ) ;
#8505 = CARTESIAN_POINT ( 'NONE',  ( 91.85898906140822362, -57.66094271643867586, -19.56282458869456775 ) ) ;
#8506 = DIRECTION ( 'NONE',  ( 0.000000000000000000, -1.000000000000000000, 0.000000000000000000 ) ) ;
#8507 = CARTESIAN_POINT ( 'NONE',  ( 37.33349330513379982, 1.593028355512270962E-15, 0.000000000000000000 ) ) ;
#8508 = DIRECTION ( 'NONE',  ( 0.000000000000000000, 0.000000000000000000, -1.000000000000000000 ) ) ;
#8509 = CARTESIAN_POINT ( 'NONE',  ( -81.37858232197777397, -30.00000000000001421, -1.651955541798732385 ) ) ;
#8510 = CARTESIAN_POINT ( 'NONE',  ( 28.77636872657296863, 18.82904586931653768, 39.99174360897747960 ) ) ;
#8511 = CARTESIAN_POINT ( 'NONE',  ( 23.21751746555144180, 27.38103382803512176, -33.20617127781698485 ) ) ;
#8512 = CYLINDRICAL_SURFACE ( 'NONE', #53225, 15.00000000000000711 ) ;
#8513 = AXIS2_PLACEMENT_3D ( 'NONE', #89838, #98446, #49354 ) ;
#8515 = FACE_OUTER_BOUND ( 'NONE', #34719, .T. ) ;
#8514 = CARTESIAN_POINT ( 'NONE',  ( 0.05533025579362068486, 4.993776679985853839, 4.350525068611871049 ) ) ;
#8516 = CARTESIAN_POINT ( 'NONE',  ( 33.00000000000000000, 450.0000000000002274, 1.202422573753698876 ) ) ;
#8517 = DIRECTION ( 'NONE',  ( 0.000000000000000000, -1.000000000000000000, 0.000000000000000000 ) ) ;
#8518 = CARTESIAN_POINT ( 'NONE',  ( -12.50000000000000000, -3.000000000000000000, -8.595933841506989026 ) ) ;
#8519 = CARTESIAN_POINT ( 'NONE',  ( 5.192560085536412906, -82.35694557368756819, 3.013051918867554413 ) ) ;
#8520 = DIRECTION ( 'NONE',  ( 0.000000000000000000, 0.000000000000000000, 1.000000000000000000 ) ) ;
#8521 = CARTESIAN_POINT ( 'NONE',  ( 6.999999999999993783, -50.00000000000000000, 102.2532056551910387 ) ) ;
#8522 = VECTOR ( 'NONE', #27763, 1000.000000000000000 ) ;
#8523 = CARTESIAN_POINT ( 'NONE',  ( 33.09999999999999432, 1.533819458162526451E-15, 0.000000000000000000 ) ) ;
#8524 = EDGE_LOOP ( 'NONE', ( #62623, #49928, #10563, #77833 ) ) ;
#8525 = DIRECTION ( 'NONE',  ( 0.000000000000000000, -1.000000000000000000, 0.000000000000000000 ) ) ;
#8526 = DIRECTION ( 'NONE',  ( -0.000000000000000000, 1.000000000000000000, -0.000000000000000000 ) ) ;
#8527 = CARTESIAN_POINT ( 'NONE',  ( -55.09674501162535876, -28.50739436101074276, -26.55108529303278075 ) ) ;
#8529 = CARTESIAN_POINT ( 'NONE',  ( -66.87664816687141922, -21.77013672081559292, -20.76364936843571130 ) ) ;
#8528 = DIRECTION ( 'NONE',  ( 0.000000000000000000, -1.000000000000000000, 0.000000000000000000 ) ) ;
#8530 = EDGE_CURVE ( 'NONE', #75683, #21601, #20318, .T. ) ;
#8531 = ORIENTED_EDGE ( 'NONE', *, *, #29602, .T. ) ;
#8532 = STYLED_ITEM ( 'NONE', ( #97380 ), #6345 ) ;
#8533 = ORIENTED_EDGE ( 'NONE', *, *, #75469, .T. ) ;
#8534 = CARTESIAN_POINT ( 'NONE',  ( -26.94399930113149466, 34.53233444631757010, 10.05698433968616001 ) ) ;
#8535 = EDGE_CURVE ( 'NONE', #76618, #35844, #25444, .T. ) ;
#8536 = AXIS2_PLACEMENT_3D ( 'NONE', #25827, #40892, #75915 ) ;
#8537 = ADVANCED_FACE ( 'NONE', ( #52586 ), #11615, .T. ) ;
#8538 = CARTESIAN_POINT ( 'NONE',  ( 1.078140322363270668E-05, -30.00000000000000000, 28.88964995960238014 ) ) ;
#8539 = CARTESIAN_POINT ( 'NONE',  ( -30.64178597908914625, -60.00000000000001421, -40.84433097566444815 ) ) ;
#8540 = VERTEX_POINT ( 'NONE', #102746 ) ;
#8541 = CARTESIAN_POINT ( 'NONE',  ( 0.06682554136338023087, -4.993536075455418555, 4.350941807883115686 ) ) ;
#8542 = CARTESIAN_POINT ( 'NONE',  ( 15.30823401445614884, 3.112986885589654751, 3.167215778812773941 ) ) ;
#8543 = CARTESIAN_POINT ( 'NONE',  ( 100.2342046845623855, -45.27551373043147720, 192.3669307444947094 ) ) ;
#8544 = EDGE_CURVE ( 'NONE', #6569, #25032, #97683, .T. ) ;
#8545 = CARTESIAN_POINT ( 'NONE',  ( -46.79100380508925383, 13.36652303332998670, 15.81652940118016204 ) ) ;
#8546 = AXIS2_PLACEMENT_3D ( 'NONE', #2202, #68020, #33546 ) ;
#8547 = EDGE_CURVE ( 'NONE', #6290, #79598, #11055, .T. ) ;
#8548 = ORIENTED_EDGE ( 'NONE', *, *, #45419, .T. ) ;
#8549 = EDGE_CURVE ( 'NONE', #112, #14702, #51183, .T. ) ;
#8550 = ORIENTED_EDGE ( 'NONE', *, *, #33675, .T. ) ;
#8551 = ORIENTED_EDGE ( 'NONE', *, *, #16169, .T. ) ;
#8552 = CARTESIAN_POINT ( 'NONE',  ( 31.42152527681154339, 380.7394937707176723, 23.45597763386094314 ) ) ;
#8553 = AXIS2_PLACEMENT_3D ( 'NONE', #2606, #12295, #70553 ) ;
#8554 = CARTESIAN_POINT ( 'NONE',  ( -5.000000000000000000, -13.89959410955659891, 11.33893914917399925 ) ) ;
#8555 = CARTESIAN_POINT ( 'NONE',  ( 15.88324666189021350, 46.12968798971461837, 4.401569153914933530 ) ) ;
#8556 = EDGE_LOOP ( 'NONE', ( #17501, #73272, #94404, #4290 ) ) ;
#8557 = DIRECTION ( 'NONE',  ( 0.000000000000000000, 0.000000000000000000, -1.000000000000000000 ) ) ;
#8558 = CARTESIAN_POINT ( 'NONE',  ( -30.00000000000000000, 0.000000000000000000, -11.00000000000000000 ) ) ;
#8559 = CARTESIAN_POINT ( 'NONE',  ( 0.000000000000000000, 0.000000000000000000, -6.235812796514431433 ) ) ;
#8560 = CARTESIAN_POINT ( 'NONE',  ( -57.91314980999670325, -57.67646044164155228, 100.3416927154360536 ) ) ;
#8561 = CARTESIAN_POINT ( 'NONE',  ( 2.977408999572651815, -28.43750000204839168, 7.188101187500000933 ) ) ;
#8562 = TOROIDAL_SURFACE ( 'NONE', #82643, 12.00000000000001066, 3.000000000000000000 ) ;
#8563 = CARTESIAN_POINT ( 'NONE',  ( -30.36547348172779692, 16.93923362554432899, 39.80091097816897161 ) ) ;
#8564 = FACE_OUTER_BOUND ( 'NONE', #18414, .T. ) ;
#8565 = CARTESIAN_POINT ( 'NONE',  ( 0.000000000000000000, 50.50000000000000000, 64.50000000000000000 ) ) ;
#8566 = CARTESIAN_POINT ( 'NONE',  ( -61.70175965769652748, -30.00000000000001066, -32.45223383460360367 ) ) ;
#8567 = DIRECTION ( 'NONE',  ( -0.000000000000000000, -0.000000000000000000, 1.000000000000000000 ) ) ;
#8568 = CARTESIAN_POINT ( 'NONE',  ( -49.82526758650133303, -56.83439142156854729, 56.29054524400240922 ) ) ;
#8569 = AXIS2_PLACEMENT_3D ( 'NONE', #41618, #65888, #65363 ) ;
#8570 = LINE ( 'NONE', #15067, #41803 ) ;
#8571 = ORIENTED_EDGE ( 'NONE', *, *, #89960, .F. ) ;
#8572 = CARTESIAN_POINT ( 'NONE',  ( -98.68288091466004630, -37.75495276146958901, 192.1257439368163489 ) ) ;
#8573 = CARTESIAN_POINT ( 'NONE',  ( -0.7515601776302233139, 295.1017350047013110, -10.00017833058035599 ) ) ;
#8574 = AXIS2_PLACEMENT_3D ( 'NONE', #40128, #65994, #97825 ) ;
#8575 = CARTESIAN_POINT ( 'NONE',  ( 12.41126668015367862, -3.690571904192825325, 20.54162461381810090 ) ) ;
#8576 = ORIENTED_EDGE ( 'NONE', *, *, #61439, .F. ) ;
#8577 = CARTESIAN_POINT ( 'NONE',  ( -17.39136371670011627, 43.47128242272506782, 4.393265579572654289 ) ) ;
#8578 = CARTESIAN_POINT ( 'NONE',  ( 90.84051608033718139, -38.50738636110989432, 200.7712009872789167 ) ) ;
#8579 = CARTESIAN_POINT ( 'NONE',  ( 27.10511071441176867, -1.200000000000000030E-05, -7.556984339686343866 ) ) ;
#8580 = LINE ( 'NONE', #32890, #66288 ) ;
#8581 = DIRECTION ( 'NONE',  ( 0.000000000000000000, 0.000000000000000000, -1.000000000000000000 ) ) ;
#8582 = CARTESIAN_POINT ( 'NONE',  ( -90.56128410203886858, 42.00000000000000000, -11.85444436786843703 ) ) ;
#8584 = CARTESIAN_POINT ( 'NONE',  ( 81.59702955527144752, -30.00000000000000000, 143.4499623754424533 ) ) ;
#8583 = UNCERTAINTY_MEASURE_WITH_UNIT (LENGTH_MEASURE( 1.000000000000000082E-05 ), #97329, 'distance_accuracy_value', 'NONE');
#8585 = CARTESIAN_POINT ( 'NONE',  ( 104.9555555555555486, 1.023464760207051730E-14, 0.000000000000000000 ) ) ;
#8586 = DIRECTION ( 'NONE',  ( 0.000000000000000000, 0.000000000000000000, -1.000000000000000000 ) ) ;
#8587 = CARTESIAN_POINT ( 'NONE',  ( 29.66054107240687543, 1.482358050883964840E-15, 0.000000000000000000 ) ) ;
#8588 = EDGE_LOOP ( 'NONE', ( #31358, #421, #38366, #28637, #12046, #37330 ) ) ;
#8589 = EDGE_LOOP ( 'NONE', ( #27059, #102351, #73348, #102889, #66390 ) ) ;
#8590 = CARTESIAN_POINT ( 'NONE',  ( 52.50523195933924114, -18.71259018865586654, 47.73583290201036533 ) ) ;
#8591 = CARTESIAN_POINT ( 'NONE',  ( 5.896197027862030815, 41.78011521630541125, -58.83937651719745787 ) ) ;
#8592 = AXIS2_PLACEMENT_3D ( 'NONE', #61197, #62273, #77907 ) ;
#8593 = CARTESIAN_POINT ( 'NONE',  ( 36.64247849049904460, 27.97083273922043389, -13.05156522269073882 ) ) ;
#8594 = EDGE_CURVE ( 'NONE', #58641, #103962, #70382, .T. ) ;
#8595 = ORIENTED_EDGE ( 'NONE', *, *, #29745, .F. ) ;
#8596 = CARTESIAN_POINT ( 'NONE',  ( -99.29559146798845859, -38.35572756809536088, 84.31528695177730981 ) ) ;
#8597 = ORIENTED_EDGE ( 'NONE', *, *, #25694, .T. ) ;
#8598 = DIRECTION ( 'NONE',  ( 0.000000000000000000, 0.000000000000000000, 1.000000000000000000 ) ) ;
#8599 = CARTESIAN_POINT ( 'NONE',  ( 98.48521771324512031, -38.35583637768242227, 79.51923348961499016 ) ) ;
#8600 = CARTESIAN_POINT ( 'NONE',  ( 12.93869051862456310, 23.58149963681356454, -4.611847144011028909 ) ) ;
#8601 = CARTESIAN_POINT ( 'NONE',  ( 92.22087313427753941, -52.71700789290898825, 76.94303511423174768 ) ) ;
#8602 = CARTESIAN_POINT ( 'NONE',  ( -31.35596682365704524, 438.0939828603719661, 22.55458131664422439 ) ) ;
#8603 = SURFACE_STYLE_FILL_AREA ( #32384 ) ;
#8604 = CARTESIAN_POINT ( 'NONE',  ( -32.89619668145245868, 321.6758930293437402, -5.892485756851701950 ) ) ;
#8605 = DIRECTION ( 'NONE',  ( 0.000000000000000000, 0.000000000000000000, -1.000000000000000000 ) ) ;
#8606 = ADVANCED_FACE ( 'NONE', ( #4052 ), #49500, .T. ) ;
#8607 = CARTESIAN_POINT ( 'NONE',  ( 76.36385995988143804, -59.99999999999999289, 188.3995559568122360 ) ) ;
#8608 = CARTESIAN_POINT ( 'NONE',  ( 18.28997961183965160, 45.00000000000000711, 62.41113724044252109 ) ) ;
#8609 = ADVANCED_FACE ( 'NONE', ( #76865 ), #80524, .T. ) ;
#8610 = EDGE_LOOP ( 'NONE', ( #47719, #68315, #103042, #23791 ) ) ;
#8611 = CARTESIAN_POINT ( 'NONE',  ( 62.60020664644493138, -29.05810901319667394, 74.09607312414506453 ) ) ;
#8612 = CARTESIAN_POINT ( 'NONE',  ( -25.88003106869689418, 295.8060735027391956, -9.795024457689359920 ) ) ;
#8613 = CARTESIAN_POINT ( 'NONE',  ( 9.336538098104073313, -51.98968743527834846, 30.58506923019146839 ) ) ;
#8614 =( GEOMETRIC_REPRESENTATION_CONTEXT ( 3 ) GLOBAL_UNCERTAINTY_ASSIGNED_CONTEXT ( ( #64625 ) ) GLOBAL_UNIT_ASSIGNED_CONTEXT ( ( #65092, #82336, #39774 ) ) REPRESENTATION_CONTEXT ( 'NONE', 'WORKASPACE' ) );
#8615 = CARTESIAN_POINT ( 'NONE',  ( -9.308639103300027529, -5.000000000000000888, -18.31521250230575149 ) ) ;
#8617 = CARTESIAN_POINT ( 'NONE',  ( -37.69778599684636333, 484.8925473506873800, -3.622119997864802876 ) ) ;
#8616 = CARTESIAN_POINT ( 'NONE',  ( -48.99521034380500595, -29.99999999995976552, 62.69765256684991073 ) ) ;
#8618 = CARTESIAN_POINT ( 'NONE',  ( -41.32756079954049255, 330.3955937106402985, 10.56840023132855499 ) ) ;
#8619 = CARTESIAN_POINT ( 'NONE',  ( -1.250000000000000222, -7.938566201357373231, -7.198902722707432922 ) ) ;
#8620 = CARTESIAN_POINT ( 'NONE',  ( 0.000000000000000000, 0.000000000000000000, 0.000000000000000000 ) ) ;
#8621 = CARTESIAN_POINT ( 'NONE',  ( 7.999999999999998224, -24.59374999999999289, 3.313708498984766493 ) ) ;
#8622 = FACE_BOUND ( 'NONE', #56341, .T. ) ;
#8623 = CIRCLE ( 'NONE', #22456, 0.4999999999999987232 ) ;
#8624 = ADVANCED_FACE ( 'NONE', ( #3523 ), #27147, .T. ) ;
#8625 = CARTESIAN_POINT ( 'NONE',  ( 20.77592568779148863, 1.482358050883964840E-15, 0.000000000000000000 ) ) ;
#8626 = ORIENTED_EDGE ( 'NONE', *, *, #101510, .F. ) ;
#8627 = CARTESIAN_POINT ( 'NONE',  ( 85.41191359320438892, -28.71737910575176400, 176.9201489232353026 ) ) ;
#8628 = EDGE_CURVE ( 'NONE', #45785, #49640, #35930, .T. ) ;
#8629 = CARTESIAN_POINT ( 'NONE',  ( 5.683639242321874896, -47.06573826195068477, 103.9372442403038548 ) ) ;
#8630 = CARTESIAN_POINT ( 'NONE',  ( -40.61431708406630747, 438.3130824198840969, 22.61094925422919388 ) ) ;
#8631 = ORIENTED_EDGE ( 'NONE', *, *, #87659, .F. ) ;
#8632 = DIRECTION ( 'NONE',  ( 0.000000000000000000, 0.000000000000000000, -1.000000000000000000 ) ) ;
#8633 = CIRCLE ( 'NONE', #60560, 3.309500000000001663 ) ;
#8634 = CARTESIAN_POINT ( 'NONE',  ( 43.00000000000000000, 436.0987441542287115, 7.567257455462732096 ) ) ;
#8635 = CARTESIAN_POINT ( 'NONE',  ( -32.19135603494724762, 464.6890496749877002, 10.76801839735351329 ) ) ;
#8636 = CARTESIAN_POINT ( 'NONE',  ( 5.499265899526156076, -3.000000000000002665, -99.22427370006747083 ) ) ;
#8637 = CARTESIAN_POINT ( 'NONE',  ( -10.18570692333505256, -0.7115926177181285395, 20.11367956310897753 ) ) ;
#8638 = AXIS2_PLACEMENT_3D ( 'NONE', #95116, #6608, #87551 ) ;
#8639 = AXIS2_PLACEMENT_3D ( 'NONE', #77776, #10365, #76696 ) ;
#8640 = CARTESIAN_POINT ( 'NONE',  ( 39.30609551598629281, -60.00000000000000000, 51.14711558221264198 ) ) ;
#8641 = DIRECTION ( 'NONE',  ( 0.5735764363510554853, 0.8191520442889852482, 0.000000000000000000 ) ) ;
#8642 = CARTESIAN_POINT ( 'NONE',  ( -8.542937654374686218, 1.046208125374536008E-15, -6.800000000000000711 ) ) ;
#8644 = CARTESIAN_POINT ( 'NONE',  ( -13.04265871945630728, 19.29919692355796457, -7.785367473261247007 ) ) ;
#8643 = CARTESIAN_POINT ( 'NONE',  ( -22.78844821391956188, -27.54187850787782565, 37.55836683131646225 ) ) ;
#8645 = VECTOR ( 'NONE', #34236, 1000.000000000000000 ) ;
#8646 = B_SPLINE_CURVE_WITH_KNOTS ( 'NONE', 3,
 ( #26988, #20518, #27526, #19441, #53352, #51201, #12346, #45272 ),
 .UNSPECIFIED., .F., .F.,
 ( 4, 2, 2, 4 ),
 ( 0.02058604435327386628, 0.02618835850023638195, 0.03179067264719889763, 0.04299530094112392897 ),
 .UNSPECIFIED. ) ;
#8647 = CARTESIAN_POINT ( 'NONE',  ( 7.188101187500001821, -16.06250000204838457, -2.977408999572650483 ) ) ;
#8648 = CARTESIAN_POINT ( 'NONE',  ( 21.29975379448946171, 294.8969325209483259, -1.990407376643353210 ) ) ;
#8649 = ORIENTED_EDGE ( 'NONE', *, *, #87986, .T. ) ;
#8650 = AXIS2_PLACEMENT_3D ( 'NONE', #48877, #41330, #81767 ) ;
#8651 = CARTESIAN_POINT ( 'NONE',  ( -19.49736279435545327, 49.99988902982538974, 59.96655211255967544 ) ) ;
#8652 = CARTESIAN_POINT ( 'NONE',  ( 7.499999999999999112, 3.105728215500127565, -7.659336188854855898 ) ) ;
#8653 = CARTESIAN_POINT ( 'NONE',  ( 37.52575628271135599, 438.0832219636473042, 4.091974619413631054 ) ) ;
#8655 = CARTESIAN_POINT ( 'NONE',  ( 34.70318342342385165, -34.58950113560386086, -30.29887370229810628 ) ) ;
#8654 = CARTESIAN_POINT ( 'NONE',  ( -46.00000000000000000, 450.0000000000002274, 8.202422573753707979 ) ) ;
#8656 = ORIENTED_EDGE ( 'NONE', *, *, #3338, .F. ) ;
#8657 = CARTESIAN_POINT ( 'NONE',  ( 12.15290226144649566, 17.45440320673788293, -8.961931909917964845 ) ) ;
#8658 = ADVANCED_FACE ( 'NONE', ( #86054 ), #93372, .F. ) ;
#8659 = CARTESIAN_POINT ( 'NONE',  ( -4.330505743362791371, 52.16474262961963149, 6.475687689770104782 ) ) ;
#8660 = EDGE_LOOP ( 'NONE', ( #86905, #26600, #39392, #66116, #14813, #42557 ) ) ;
#8661 = AXIS2_PLACEMENT_3D ( 'NONE', #98191, #5993, #72330 ) ;
#8662 = EDGE_CURVE ( 'NONE', #17532, #67283, #85718, .T. ) ;
#8663 =( LENGTH_UNIT ( ) NAMED_UNIT ( * ) SI_UNIT ( .MILLI., .METRE. ) );
#8664 = ADVANCED_FACE ( 'NONE', ( #63892 ), #30777, .F. ) ;
#8665 = DIRECTION ( 'NONE',  ( 0.000000000000000000, 0.000000000000000000, -1.000000000000000000 ) ) ;
#8666 = AXIS2_PLACEMENT_3D ( 'NONE', #81814, #16040, #97475 ) ;
#8667 = CARTESIAN_POINT ( 'NONE',  ( -33.10434277953672222, 40.69601545704099266, -62.12919646516525063 ) ) ;
#8668 = CARTESIAN_POINT ( 'NONE',  ( -100.3149285850330159, -60.00000000000000711, 82.88046306574433686 ) ) ;
#8669 = DIRECTION ( 'NONE',  ( -1.000000000000000000, 0.000000000000000000, 0.000000000000000000 ) ) ;
#8670 = CARTESIAN_POINT ( 'NONE',  ( 6.326416241096633364, 1.324101276589543907, 6.831531844319975733 ) ) ;
#8671 = CARTESIAN_POINT ( 'NONE',  ( 42.09158233638500235, 465.7816406625409513, 14.79318349170030089 ) ) ;
#8673 = CARTESIAN_POINT ( 'NONE',  ( -43.00000000000000000, 465.8747179598608454, 15.20075430169035968 ) ) ;
#8672 =( REPRESENTATION_RELATIONSHIP ('NONE','NONE', #69581, #16335 ) REPRESENTATION_RELATIONSHIP_WITH_TRANSFORMATION ( #96750 )SHAPE_REPRESENTATION_RELATIONSHIP( ) );
#8675 = CARTESIAN_POINT ( 'NONE',  ( 30.00000000000000355, 489.4338083968374349, 5.745752720320034257 ) ) ;
#8674 = CARTESIAN_POINT ( 'NONE',  ( 6.043427762771891310, -5.000000000000002665, -74.51456333905348117 ) ) ;
#8676 = CARTESIAN_POINT ( 'NONE',  ( -85.91925276215749818, -18.46748765878107434, 164.5932108442251547 ) ) ;
#8677 = ORIENTED_EDGE ( 'NONE', *, *, #56086, .T. ) ;
#8678 = CARTESIAN_POINT ( 'NONE',  ( 7.500000000000005329, -5.250000000000005329, -71.71180648257555390 ) ) ;
#8679 = EDGE_CURVE ( 'NONE', #21783, #36385, #1528, .T. ) ;
#8680 = ORIENTED_EDGE ( 'NONE', *, *, #5337, .T. ) ;
#8681 = ORIENTED_EDGE ( 'NONE', *, *, #94898, .F. ) ;
#8682 = CARTESIAN_POINT ( 'NONE',  ( -18.99999999999999289, 4.000000000000000888, -1.500000000000001332 ) ) ;
#8683 = CARTESIAN_POINT ( 'NONE',  ( -10.00000000000000355, 85.00000000000000000, -4.000000000000000000 ) ) ;
#8684 = EDGE_LOOP ( 'NONE', ( #14507, #15686, #51905, #106627 ) ) ;
#8685 = AXIS2_PLACEMENT_3D ( 'NONE', #37824, #22150, #39391 ) ;
#8686 = CARTESIAN_POINT ( 'NONE',  ( 109.3513501059324255, -38.00000000000000000, 179.6549720493207190 ) ) ;
#8687 = DIRECTION ( 'NONE',  ( -1.000000000000000000, -1.224606353822377258E-16, -0.000000000000000000 ) ) ;
#8688 = CARTESIAN_POINT ( 'NONE',  ( -18.91791044776116237, 45.00000000000000711, 62.18611311450884926 ) ) ;
#8689 = CARTESIAN_POINT ( 'NONE',  ( 43.64071296021040069, 465.1114042828264701, 8.837889712622711613 ) ) ;
#8690 = CARTESIAN_POINT ( 'NONE',  ( 12.98455676797003022, -5.000000000000000000, -86.33387663731812722 ) ) ;
#8691 = DIRECTION ( 'NONE',  ( 0.000000000000000000, -1.000000000000000000, 0.000000000000000000 ) ) ;
#8692 = CARTESIAN_POINT ( 'NONE',  ( 111.4777457387739048, -59.99999999999993605, 136.6117272317642630 ) ) ;
#8693 = CARTESIAN_POINT ( 'NONE',  ( -113.5293469826316084, -59.99999999999994316, 153.5981017735323633 ) ) ;
#8694 = CARTESIAN_POINT ( 'NONE',  ( -61.80134322767651867, -53.39308551080091547, 84.00808285357440752 ) ) ;
#8695 = EDGE_LOOP ( 'NONE', ( #29852, #52762, #66387 ) ) ;
#8696 = CARTESIAN_POINT ( 'NONE',  ( -42.76627839262699382, 38.95206895324334795, 47.52996633003031235 ) ) ;
#8697 = CARTESIAN_POINT ( 'NONE',  ( 110.6310860903329285, -59.99999999998527045, 195.7736967744526737 ) ) ;
#8698 = ORIENTED_EDGE ( 'NONE', *, *, #86060, .F. ) ;
#8699 = CARTESIAN_POINT ( 'NONE',  ( 5.016252133114435630, -29.02926342023009454, 28.71829084836867452 ) ) ;
#8700 = CARTESIAN_POINT ( 'NONE',  ( -103.3843560967306701, -45.26539566788723334, 158.7060436347484824 ) ) ;
#8701 = CARTESIAN_POINT ( 'NONE',  ( 7.188101187500000044, -10.53125000204838457, 0.000000000000000000 ) ) ;
#8702 = CARTESIAN_POINT ( 'NONE',  ( 55.00571552735602410, -4.000000000000000888, 4.898587196589422689E-16 ) ) ;
#8703 = ORIENTED_EDGE ( 'NONE', *, *, #22621, .F. ) ;
#8704 = DIRECTION ( 'NONE',  ( 0.000000000000000000, 1.000000000000000000, 0.000000000000000000 ) ) ;
#8705 = ORIENTED_EDGE ( 'NONE', *, *, #94307, .T. ) ;
#8706 = DIRECTION ( 'NONE',  ( 0.5735764363510470476, -0.8191520442889911324, 1.003171929053524007E-16 ) ) ;
#8707 = CARTESIAN_POINT ( 'NONE',  ( -37.19345962173282771, -60.00000000000000000, 48.57494274058771566 ) ) ;
#8708 = CARTESIAN_POINT ( 'NONE',  ( 9.820360545668073371, -57.58891795034524108, 28.90271669672396726 ) ) ;
#8709 = CARTESIAN_POINT ( 'NONE',  ( -5.082755093536326818, -21.59375000204838457, 5.082755093536325042 ) ) ;
#8710 = CIRCLE ( 'NONE', #20874, 4.000000000000000888 ) ;
#8711 = CARTESIAN_POINT ( 'NONE',  ( 35.62292360717185602, 485.2979424254040737, -2.983350328823797692 ) ) ;
#8712 = LINE ( 'NONE', #68018, #20269 ) ;
#8713 = CARTESIAN_POINT ( 'NONE',  ( -7.922281120364393914, -4.573931137438282057, -8.047472243342934206 ) ) ;
#8714 = CARTESIAN_POINT ( 'NONE',  ( 55.00571552735602410, 4.898587196589294500E-16, -4.000000000000007105 ) ) ;
#8715 = CARTESIAN_POINT ( 'NONE',  ( 32.14406631781839252, 464.7180616791956709, 11.03187369810257046 ) ) ;
#8716 = CARTESIAN_POINT ( 'NONE',  ( -24.00241574749204432, 27.29294457708168409, 32.94367910540178457 ) ) ;
#8717 = CARTESIAN_POINT ( 'NONE',  ( 86.44524746911137925, -60.00000000000003553, 22.58426570472127182 ) ) ;
#8718 = CARTESIAN_POINT ( 'NONE',  ( -32.39963873073048717, -25.61850230709818277, 31.48490130413751587 ) ) ;
#8719 = CIRCLE ( 'NONE', #24312, 3.309500000000001663 ) ;
#8720 = CARTESIAN_POINT ( 'NONE',  ( -1.544427540536530316E-15, -4.285714285714290916, 25.22241582816893057 ) ) ;
#8721 = CARTESIAN_POINT ( 'NONE',  ( 40.48067620657982957, -46.43136235810992218, 40.68172795048424462 ) ) ;
#8722 = CARTESIAN_POINT ( 'NONE',  ( 71.80342808059909032, -30.00000000000000000, -19.71766482350836469 ) ) ;
#8723 = EDGE_LOOP ( 'NONE', ( #7498, #27513, #57294, #66828 ) ) ;
#8724 = CARTESIAN_POINT ( 'NONE',  ( 43.11534632275464674, 435.4435433140300233, 9.329549855361735311 ) ) ;
#8725 = ADVANCED_FACE ( 'NONE', ( #84066 ), #26407, .T. ) ;
#8726 = CARTESIAN_POINT ( 'NONE',  ( -82.83498824252026793, -38.82036250731917448, 196.8018683164616789 ) ) ;
#8727 = ORIENTED_EDGE ( 'NONE', *, *, #86547, .T. ) ;
#8729 = CARTESIAN_POINT ( 'NONE',  ( 40.75641113481592726, 360.0948485545300741, 24.37153223514695100 ) ) ;
#8728 = CARTESIAN_POINT ( 'NONE',  ( 89.93133926947346879, 1.016364837396684119E-14, 0.000000000000000000 ) ) ;
#8730 = CARTESIAN_POINT ( 'NONE',  ( 35.47391375821870696, -59.99999999999999289, 39.53917635555357890 ) ) ;
#8731 = FACE_OUTER_BOUND ( 'NONE', #32713, .T. ) ;
#8732 = CARTESIAN_POINT ( 'NONE',  ( 6.172110426325241761, -1.395451528107193750, 6.499999999999999112 ) ) ;
#8733 = CARTESIAN_POINT ( 'NONE',  ( 7.004291983109769859, 40.56179000455576045, -71.01843131752761451 ) ) ;
#8734 = CARTESIAN_POINT ( 'NONE',  ( -4.250000000000000000, 5.204748896376250699E-16, -7.657127082228716297 ) ) ;
#8735 = CARTESIAN_POINT ( 'NONE',  ( -30.23256681546976665, 333.1711909956446220, 15.81959552928561052 ) ) ;
#8736 =( GEOMETRIC_REPRESENTATION_CONTEXT ( 3 ) GLOBAL_UNCERTAINTY_ASSIGNED_CONTEXT ( ( #19244 ) ) GLOBAL_UNIT_ASSIGNED_CONTEXT ( ( #68826, #2462, #92541 ) ) REPRESENTATION_CONTEXT ( 'NONE', 'WORKASPACE' ) );
#8737 = CARTESIAN_POINT ( 'NONE',  ( 109.9064092654975155, -60.00000000000000711, 142.7128145035794375 ) ) ;
#8738 = DIRECTION ( 'NONE',  ( -1.000000000000000000, -1.224606353822377258E-16, -0.000000000000000000 ) ) ;
#8739 = CARTESIAN_POINT ( 'NONE',  ( -7.046289519167719284, -66.30591819944378074, -3.789821819998816288 ) ) ;
#8740 = EDGE_CURVE ( 'NONE', #20995, #90030, #77034, .T. ) ;
#8741 = ORIENTED_EDGE ( 'NONE', *, *, #16783, .F. ) ;
#8742 = CARTESIAN_POINT ( 'NONE',  ( -91.63847879749884839, -29.99999999999996447, 190.7599629194617421 ) ) ;
#8743 = ORIENTED_EDGE ( 'NONE', *, *, #84944, .T. ) ;
#8744 = CARTESIAN_POINT ( 'NONE',  ( 25.85221525804374920, 37.20477182923430348, -8.663606034466162953 ) ) ;
#8745 = CARTESIAN_POINT ( 'NONE',  ( 42.89089171630051567, 462.3282028664104928, 4.511925770464189966 ) ) ;
#8746 = CARTESIAN_POINT ( 'NONE',  ( 8.167412539197048460, 112.7208733012629125, 0.000000000000000000 ) ) ;
#8747 = CARTESIAN_POINT ( 'NONE',  ( 59.41111111111111143, 6.915964383211875250E-15, 0.000000000000000000 ) ) ;
#8748 = CARTESIAN_POINT ( 'NONE',  ( -33.74271564777242816, 484.1802673187708592, 2.058285076122308155 ) ) ;
#8749 = CARTESIAN_POINT ( 'NONE',  ( 5.082755093536325930, -19.34375000204838457, -5.082755093536325042 ) ) ;
#8750 = AXIS2_PLACEMENT_3D ( 'NONE', #20177, #68144, #51947 ) ;
#8751 = DIRECTION ( 'NONE',  ( 1.000000000000000000, 1.224606353822377258E-16, 0.000000000000000000 ) ) ;
#8752 = CARTESIAN_POINT ( 'NONE',  ( 6.890281281981907924, 41.03680257675737408, -70.85895802599645776 ) ) ;
#8753 = CIRCLE ( 'NONE', #41472, 2.000000000000001776 ) ;
#8754 = EDGE_CURVE ( 'NONE', #54320, #71171, #10688, .T. ) ;
#8756 = VERTEX_POINT ( 'NONE', #42533 ) ;
#8755 = SURFACE_STYLE_USAGE ( .BOTH. , #16868 ) ;
#8757 = CARTESIAN_POINT ( 'NONE',  ( 85.23626010823490162, -18.61825805347759655, 157.3731097714332634 ) ) ;
#8758 = EDGE_CURVE ( 'NONE', #77582, #21651, #6451, .T. ) ;
#8759 = CYLINDRICAL_SURFACE ( 'NONE', #84185, 15.00000000000001421 ) ;
#8760 = CARTESIAN_POINT ( 'NONE',  ( 9.221216839714873714, 86.04759748168980593, 3.869414262756989853 ) ) ;
#8761 = ORIENTED_EDGE ( 'NONE', *, *, #57096, .T. ) ;
#8762 = CARTESIAN_POINT ( 'NONE',  ( -0.1547218309332313857, 18.85536929889913083, -49.25755043093464991 ) ) ;
#8763 = LINE ( 'NONE', #50803, #102353 ) ;
#8764 = FACE_OUTER_BOUND ( 'NONE', #41937, .T. ) ;
#8765 = CARTESIAN_POINT ( 'NONE',  ( 5.430765937255434217, -60.00000000000000000, -36.83649123861827945 ) ) ;
#8766 = CARTESIAN_POINT ( 'NONE',  ( -33.15900708678776709, 406.2917883087327482, 25.90049563504663510 ) ) ;
#8767 = EDGE_CURVE ( 'NONE', #66436, #24664, #24593, .T. ) ;
#8768 = CARTESIAN_POINT ( 'NONE',  ( -9.500000000000000000, -5.000000000000000000, -20.99851272547259384 ) ) ;
#8769 = EDGE_LOOP ( 'NONE', ( #53741, #38687 ) ) ;
#8770 =( NAMED_UNIT ( * ) PLANE_ANGLE_UNIT ( ) SI_UNIT ( $, .RADIAN. ) );
#8771 = CIRCLE ( 'NONE', #60467, 5.000000000000001776 ) ;
#8772 = CARTESIAN_POINT ( 'NONE',  ( 72.11682663846713126, -4.000000000000000888, 4.898587196589422689E-16 ) ) ;
#8774 = CARTESIAN_POINT ( 'NONE',  ( 7.386518197476049430, 41.27037547458987632, -59.50133886764230340 ) ) ;
#8773 =( BOUNDED_SURFACE ( )  B_SPLINE_SURFACE ( 3, 2, ( 
 ( #43390, #27783, #1840 ),
 ( #35867, #68743, #85445 ),
 ( #44455, #76273, #101088 ),
 ( #75199, #51466, #91931 ) ),
 .UNSPECIFIED., .F., .F., .F. ) 
 B_SPLINE_SURFACE_WITH_KNOTS ( ( 4, 4 ),
 ( 3, 3 ),
 ( -1.647987302177966740E-17, 0.001448708294673844077 ),
 ( 0.000000000000000000, 1.000000000000000000 ),
 .UNSPECIFIED. ) 
 GEOMETRIC_REPRESENTATION_ITEM ( )  RATIONAL_B_SPLINE_SURFACE ( (
 ( 1.000000000000000000, 0.7788880963805115965, 1.000000000000000000),
 ( 1.000000000000000000, 0.7852432470597578984, 1.000000000000000000),
 ( 1.000000000000000000, 0.7915643316728345757, 1.000000000000000000),
 ( 1.000000000000000000, 0.7978714159192749067, 1.000000000000000000) ) ) 
 REPRESENTATION_ITEM ( '' )  SURFACE ( )  );
#8775 = CARTESIAN_POINT ( 'NONE',  ( 86.74269761982320404, -39.11688401941764681, 188.5944613561505321 ) ) ;
#8776 = DIRECTION ( 'NONE',  ( -1.000000000000000000, 0.000000000000000000, 0.000000000000000000 ) ) ;
#8777 = CARTESIAN_POINT ( 'NONE',  ( -7.188101187500000044, -30.40625000204838813, -8.802885111219163269E-16 ) ) ;
#8778 = CARTESIAN_POINT ( 'NONE',  ( 8.238386871430398273, 51.94821137183647863, 1.562230139517037486 ) ) ;
#8779 = DIRECTION ( 'NONE',  ( 1.000000000000000000, -0.000000000000000000, -0.000000000000000000 ) ) ;
#8780 = CARTESIAN_POINT ( 'NONE',  ( 48.28061695858884406, 9.217865022612262038, 16.83796839065893991 ) ) ;
#8781 = EDGE_LOOP ( 'NONE', ( #45126, #62112, #91018, #29371, #103413 ) ) ;
#8782 = AXIS2_PLACEMENT_3D ( 'NONE', #65453, #89737, #25564 ) ;
#8783 = VECTOR ( 'NONE', #104796, 1000.000000000000000 ) ;
#8784 = CARTESIAN_POINT ( 'NONE',  ( -34.47678062873981020, 437.1474145881089157, 5.468662283310369077 ) ) ;
#8785 = CARTESIAN_POINT ( 'NONE',  ( 18.09999999999999787, 3.309500000000003439, 0.000000000000000000 ) ) ;
#8786 =( GEOMETRIC_REPRESENTATION_CONTEXT ( 3 ) GLOBAL_UNCERTAINTY_ASSIGNED_CONTEXT ( ( #58103 ) ) GLOBAL_UNIT_ASSIGNED_CONTEXT ( ( #75743, #56887, #89814 ) ) REPRESENTATION_CONTEXT ( 'NONE', 'WORKASPACE' ) );
#8787 = DIRECTION ( 'NONE',  ( 0.000000000000000000, -1.000000000000000000, 0.000000000000000000 ) ) ;
#8788 = FACE_OUTER_BOUND ( 'NONE', #9821, .T. ) ;
#8789 = VERTEX_POINT ( 'NONE', #18293 ) ;
#8790 = AXIS2_PLACEMENT_3D ( 'NONE', #51226, #45299, #60435 ) ;
#8791 = SURFACE_SIDE_STYLE ('',( #41699 ) ) ;
#8792 = CARTESIAN_POINT ( 'NONE',  ( -43.71037717921241494, 462.3391554988664325, 4.824299547746271344 ) ) ;
#8793 = CARTESIAN_POINT ( 'NONE',  ( 105.5514723802492512, -57.67109349774979421, 101.8026348850644638 ) ) ;
#8794 = MECHANICAL_DESIGN_GEOMETRIC_PRESENTATION_REPRESENTATION (  '', ( #41525 ), #13943 ) ;
#8796 = CARTESIAN_POINT ( 'NONE',  ( 10.11650669486618881, 1.474610560812782335E-15, 0.000000000000000000 ) ) ;
#8795 = CIRCLE ( 'NONE', #5425, 60.00000000000000000 ) ;
#8797 = FACE_OUTER_BOUND ( 'NONE', #36057, .T. ) ;
#8798 = CARTESIAN_POINT ( 'NONE',  ( 6.692326732991420724E-21, 18.87382441218278828, -49.25000000000000000 ) ) ;
#8799 = CARTESIAN_POINT ( 'NONE',  ( 7.981862520314372489, 0.000000000000000000, -0.01269999999999830292 ) ) ;
#8800 = CARTESIAN_POINT ( 'NONE',  ( -82.70757079118186539, -59.99999999999999289, 198.6122815915291255 ) ) ;
#8801 = CARTESIAN_POINT ( 'NONE',  ( -39.84233570596349949, 333.3323931548420660, 19.23895789620553032 ) ) ;
#8802 = DIRECTION ( 'NONE',  ( 1.000000000000000000, 1.224606353822377258E-16, 0.000000000000000000 ) ) ;
#8803 = CARTESIAN_POINT ( 'NONE',  ( -33.08751701378358945, 301.6823158026044780, 11.49690784967660662 ) ) ;
#8804 = CARTESIAN_POINT ( 'NONE',  ( -85.78836534190880059, -32.04508190827686320, 182.7537413317583912 ) ) ;
#8805 = ORIENTED_EDGE ( 'NONE', *, *, #72338, .F. ) ;
#8806 = CARTESIAN_POINT ( 'NONE',  ( 24.69596357296672906, 306.0113623816489508, -9.748045212393256165 ) ) ;
#8807 = EDGE_CURVE ( 'NONE', #50100, #53546, #67223, .T. ) ;
#8808 = EDGE_LOOP ( 'NONE', ( #8576, #36368, #52052, #61773, #84999, #42351 ) ) ;
#8809 = CARTESIAN_POINT ( 'NONE',  ( -7.743982712349853692, -13.46213014760737181, 2.020119794285908377 ) ) ;
#8810 = ADVANCED_FACE ( 'NONE', ( #44146 ), #40885, .T. ) ;
#8811 = FACE_OUTER_BOUND ( 'NONE', #419, .T. ) ;
#8812 = CARTESIAN_POINT ( 'NONE',  ( -86.78291921055377145, -60.23020244905906395, -10.97695437812392782 ) ) ;
#8813 = CIRCLE ( 'NONE', #72571, 2.000000000000000888 ) ;
#8814 = CARTESIAN_POINT ( 'NONE',  ( -4.483615626739970494, 9.381785226897060070, -5.000000000000000000 ) ) ;
#8815 = FACE_OUTER_BOUND ( 'NONE', #24146, .T. ) ;
#8816 = CARTESIAN_POINT ( 'NONE',  ( -33.00496812084341514, 465.6658704666166386, 15.15901827095481735 ) ) ;
#8817 = EDGE_CURVE ( 'NONE', #80767, #26711, #38718, .T. ) ;
#8818 = CARTESIAN_POINT ( 'NONE',  ( 10.05028520371290490, 14.77158978979456272, -10.42891015365750995 ) ) ;
#8819 = CARTESIAN_POINT ( 'NONE',  ( -6.011841252072294266E-15, 27.55047179872464724, 49.09040922050319011 ) ) ;
#8820 = LINE ( 'NONE', #83765, #18737 ) ;
#8821 = CARTESIAN_POINT ( 'NONE',  ( -17.09952670627316706, -60.00000000000001421, -44.43607591113852351 ) ) ;
#8822 = AXIS2_PLACEMENT_3D ( 'NONE', #39201, #54273, #79109 ) ;
#8823 = CARTESIAN_POINT ( 'NONE',  ( -78.52260771847107890, -22.14211393470201017, 122.4770835781163782 ) ) ;
#8824 = ORIENTED_EDGE ( 'NONE', *, *, #52102, .T. ) ;
#8825 = CARTESIAN_POINT ( 'NONE',  ( 76.24208907273079205, -14.21045842199436571, 145.5826741442930086 ) ) ;
#8826 = CARTESIAN_POINT ( 'NONE',  ( 7.896254658894418021, 88.78929182754201577, 1.307282859663297936 ) ) ;
#8827 = CARTESIAN_POINT ( 'NONE',  ( 95.00826987541751123, -57.67190437205294984, 32.63624362569164106 ) ) ;
#8828 = VERTEX_POINT ( 'NONE', #12818 ) ;
#8829 = CARTESIAN_POINT ( 'NONE',  ( -17.49999999999997513, 50.00000000000000000, 100.0000000000000000 ) ) ;
#8830 = DIRECTION ( 'NONE',  ( 0.000000000000000000, -1.000000000000000000, 0.000000000000000000 ) ) ;
#8831 = ORIENTED_EDGE ( 'NONE', *, *, #87345, .F. ) ;
#8832 =( NAMED_UNIT ( * ) PLANE_ANGLE_UNIT ( ) SI_UNIT ( $, .RADIAN. ) );
#8833 = CARTESIAN_POINT ( 'NONE',  ( 16.02985501006017444, 43.70305530208896982, 6.508335557365128032 ) ) ;
#8834 = CARTESIAN_POINT ( 'NONE',  ( -1.320432766682874540E-15, -10.53125000204838457, 7.188101187500000044 ) ) ;
#8835 = CARTESIAN_POINT ( 'NONE',  ( 43.51067860848580438, 485.4417974898075272, 3.909400899863179735 ) ) ;
#8836 = CARTESIAN_POINT ( 'NONE',  ( -29.68315524077004852, -1.200000000000000030E-05, -40.85535821593474282 ) ) ;
#8837 = SURFACE_STYLE_USAGE ( .BOTH. , #83264 ) ;
#8838 = CARTESIAN_POINT ( 'NONE',  ( 9.833493305133801599, 4.000000000000003553, 0.000000000000000000 ) ) ;
#8839 = DIRECTION ( 'NONE',  ( 0.000000000000000000, 0.000000000000000000, 1.000000000000000000 ) ) ;
#8840 = VECTOR ( 'NONE', #106493, 1000.000000000000000 ) ;
#8841 = ORIENTED_EDGE ( 'NONE', *, *, #47129, .F. ) ;
#8842 = CARTESIAN_POINT ( 'NONE',  ( -7.078150683205035598, 41.46400356776579343, -70.18186705553098648 ) ) ;
#8844 = CARTESIAN_POINT ( 'NONE',  ( 28.86447232581024025, -46.43248914764336632, 33.96989350538401453 ) ) ;
#8843 = SURFACE_STYLE_FILL_AREA ( #2346 ) ;
#8845 = CARTESIAN_POINT ( 'NONE',  ( -32.62396605173334763, 486.1273723460411134, 7.520682129455360965 ) ) ;
#8846 = EDGE_LOOP ( 'NONE', ( #19422, #9725, #76243, #73531 ) ) ;
#8847 = CARTESIAN_POINT ( 'NONE',  ( -0.5340012606292878772, 13.17865866240859241, 51.63689604381274734 ) ) ;
#8848 = EDGE_CURVE ( 'NONE', #66028, #81895, #34062, .T. ) ;
#8849 = ORIENTED_EDGE ( 'NONE', *, *, #36673, .F. ) ;
#8851 = SURFACE_STYLE_USAGE ( .BOTH. , #51439 ) ;
#8850 = DIRECTION ( 'NONE',  ( 0.000000000000000000, 0.000000000000000000, 1.000000000000000000 ) ) ;
#8852 = DIRECTION ( 'NONE',  ( 1.871721906610600077E-16, 0.000000000000000000, -1.000000000000000000 ) ) ;
#8853 = CARTESIAN_POINT ( 'NONE',  ( -9.789044728064858703, 294.6486233851414909, -2.043184600578024757 ) ) ;
#8854 = CARTESIAN_POINT ( 'NONE',  ( 33.00496812083873976, 465.6658704666190829, 15.15901827093887810 ) ) ;
#8855 = CARTESIAN_POINT ( 'NONE',  ( 0.6252597638487128462, 13.29621446636062210, -51.58647352287361798 ) ) ;
#8856 = ORIENTED_EDGE ( 'NONE', *, *, #23714, .F. ) ;
#8857 = CARTESIAN_POINT ( 'NONE',  ( 92.20132009836827081, -60.00000000000002132, -13.14806591022434290 ) ) ;
#8858 = LINE ( 'NONE', #207, #55018 ) ;
#8860 = CARTESIAN_POINT ( 'NONE',  ( -15.90614609307868399, -3.157894736842107530, 14.66382285868950675 ) ) ;
#8859 = CIRCLE ( 'NONE', #32987, 4.000000000000000888 ) ;
#8861 = CARTESIAN_POINT ( 'NONE',  ( 29.34999999999999787, 1.533819458162526451E-15, 0.000000000000000000 ) ) ;
#8862 = MECHANICAL_DESIGN_GEOMETRIC_PRESENTATION_REPRESENTATION (  '', ( #79548 ), #38240 ) ;
#8863 = CARTESIAN_POINT ( 'NONE',  ( -46.92723468898989125, 18.82863087225937448, -15.00902207511727404 ) ) ;
#8864 = ADVANCED_FACE ( 'NONE', ( #53814 ), #59850, .T. ) ;
#8865 = EDGE_LOOP ( 'NONE', ( #31554, #29797 ) ) ;
#8866 = CONICAL_SURFACE ( 'NONE', #82702, 6.500000000000000000, 1.047197551196600296 ) ;
#8867 = DIRECTION ( 'NONE',  ( -1.000000000000000000, -0.000000000000000000, -0.000000000000000000 ) ) ;
#8868 = EDGE_LOOP ( 'NONE', ( #19880, #87937, #5202, #95447, #13761 ) ) ;
#8869 = VERTEX_POINT ( 'NONE', #46793 ) ;
#8870 = CARTESIAN_POINT ( 'NONE',  ( 4.898587196589412829E-16, -10.62499999999999289, -8.000000000000000000 ) ) ;
#8871 = PRESENTATION_STYLE_ASSIGNMENT (( #82768 ) ) ;
#8872 = DIRECTION ( 'NONE',  ( 0.000000000000000000, -1.000000000000000000, 0.000000000000000000 ) ) ;
#8873 = DIRECTION ( 'NONE',  ( 1.000000000000000000, 1.224606353822377258E-16, 0.000000000000000000 ) ) ;
#8874 = CARTESIAN_POINT ( 'NONE',  ( 83.16664753440134916, -37.83434465694476501, -3.567909543517462367 ) ) ;
#8876 =( GEOMETRIC_REPRESENTATION_CONTEXT ( 3 ) GLOBAL_UNCERTAINTY_ASSIGNED_CONTEXT ( ( #33296 ) ) GLOBAL_UNIT_ASSIGNED_CONTEXT ( ( #73148, #64561, #30621 ) ) REPRESENTATION_CONTEXT ( 'NONE', 'WORKASPACE' ) );
#8875 = CARTESIAN_POINT ( 'NONE',  ( -41.96602095134714716, 327.8757771672179615, 6.048261806728006285 ) ) ;
#8877 = CARTESIAN_POINT ( 'NONE',  ( -2.914466931036500341, -69.57166512993157426, 13.30289308728773001 ) ) ;
#8878 = VERTEX_POINT ( 'NONE', #30102 ) ;
#8879 = DIRECTION ( 'NONE',  ( 0.000000000000000000, -0.3420201433256733758, -0.9396926207859066515 ) ) ;
#8880 = ORIENTED_EDGE ( 'NONE', *, *, #94659, .F. ) ;
#8881 = CARTESIAN_POINT ( 'NONE',  ( 0.000000000000000000, 1.005902684993156715, 0.000000000000000000 ) ) ;
#8882 = CARTESIAN_POINT ( 'NONE',  ( -75.45824100956336622, -38.34912970864160542, 173.9041770547032968 ) ) ;
#8883 = CARTESIAN_POINT ( 'NONE',  ( 38.45306524269546600, 463.5271487759612796, 19.68908736396432246 ) ) ;
#8885 = ORIENTED_EDGE ( 'NONE', *, *, #22997, .T. ) ;
#8884 = CARTESIAN_POINT ( 'NONE',  ( -76.77023017917504433, -60.00000000000002842, 146.8812870064044489 ) ) ;
#8886 = CARTESIAN_POINT ( 'NONE',  ( 66.25591572988753342, -36.00678726784801142, 88.05794226510028011 ) ) ;
#8887 = ADVANCED_FACE ( 'NONE', ( #94837 ), #15082, .T. ) ;
#8888 = ORIENTED_EDGE ( 'NONE', *, *, #87726, .F. ) ;
#8889 = CARTESIAN_POINT ( 'NONE',  ( -33.95156263172582101, 464.5083255208627975, 6.608064661821575037 ) ) ;
#8890 = CARTESIAN_POINT ( 'NONE',  ( -5.082755093536326818, -22.71875000204838457, 5.082755093536325042 ) ) ;
#8891 = CARTESIAN_POINT ( 'NONE',  ( -113.5700743903323087, -57.67116359713492812, 158.3188924881959849 ) ) ;
#8892 = EDGE_CURVE ( 'NONE', #49207, #26696, #70011, .T. ) ;
#8893 = ORIENTED_EDGE ( 'NONE', *, *, #72319, .F. ) ;
#8894 = DIRECTION ( 'NONE',  ( -0.000000000000000000, -0.000000000000000000, -1.000000000000000000 ) ) ;
#8895 = PRESENTATION_LAYER_ASSIGNMENT (  '', '', ( #95071 ) ) ;
#8896 = EDGE_CURVE ( 'NONE', #79894, #48783, #55484, .T. ) ;
#8897 = CARTESIAN_POINT ( 'NONE',  ( -35.58515402554202467, 490.6697164559567454, 12.32566724388538049 ) ) ;
#8898 = CARTESIAN_POINT ( 'NONE',  ( 7.500000000000000888, -3.000671055698259870, -20.99923901233272971 ) ) ;
#8899 = CARTESIAN_POINT ( 'NONE',  ( -8.000000000000000000, -23.93750000409677270, -9.797174393178825657E-16 ) ) ;
#8900 = EDGE_CURVE ( 'NONE', #653, #56430, #101751, .T. ) ;
#8901 = DIRECTION ( 'NONE',  ( 0.000000000000000000, -1.000000000000000000, 0.000000000000000000 ) ) ;
#8902 = CARTESIAN_POINT ( 'NONE',  ( 9.176803346051531918, 249.4705284420255680, 3.973598758023531019 ) ) ;
#8903 = CARTESIAN_POINT ( 'NONE',  ( -7.320805857562880270, 41.41776710089564517, -59.82972164228972645 ) ) ;
#8904 = CARTESIAN_POINT ( 'NONE',  ( 9.333555687487613994, 31.78102696608970490, 3.591168747312691423 ) ) ;
#8905 = DIRECTION ( 'NONE',  ( -1.000000000000000000, -0.000000000000000000, -0.000000000000000000 ) ) ;
#8906 = SURFACE_STYLE_USAGE ( .BOTH. , #1326 ) ;
#8907 = ORIENTED_EDGE ( 'NONE', *, *, #6251, .T. ) ;
#8908 = CARTESIAN_POINT ( 'NONE',  ( 43.59756234217299209, 434.3244621007144133, 14.55946156040475614 ) ) ;
#8909 = SURFACE_SIDE_STYLE ('',( #75779 ) ) ;
#8911 = CARTESIAN_POINT ( 'NONE',  ( -5.000000000000000000, -60.71953810597282342, 12.61250543006821978 ) ) ;
#8910 =( BOUNDED_CURVE ( )  B_SPLINE_CURVE ( 2, ( #25173, #75274, #24116 ),
 .UNSPECIFIED., .F., .F. ) 
 B_SPLINE_CURVE_WITH_KNOTS ( ( 3, 3 ),
 ( 0.000000000000000000, 1.000000000000000000 ),
 .UNSPECIFIED. ) 
 CURVE ( )  GEOMETRIC_REPRESENTATION_ITEM ( )  RATIONAL_B_SPLINE_CURVE ( ( 1.000000000000000000, 1.857142857142858317, 1.000000000000000000 ) ) 
 REPRESENTATION_ITEM ( '' )  );
#8912 = CARTESIAN_POINT ( 'NONE',  ( -95.21340098042236377, -29.99999999999999645, 191.3393382648713441 ) ) ;
#8913 = VERTEX_POINT ( 'NONE', #56457 ) ;
#8914 = CARTESIAN_POINT ( 'NONE',  ( 38.75698381667141490, 25.16721628702945424, -12.59717980438506224 ) ) ;
#8915 = CARTESIAN_POINT ( 'NONE',  ( 62.96112565841632858, -57.67852246553200501, 118.3385123048287397 ) ) ;
#8917 = DIRECTION ( 'NONE',  ( -1.000000000000000000, -1.224606353822377258E-16, -0.000000000000000000 ) ) ;
#8916 = CARTESIAN_POINT ( 'NONE',  ( 5.656854249492378806, -15.87500000409677092, 5.656854249492381470 ) ) ;
#8918 = CARTESIAN_POINT ( 'NONE',  ( 14.84396807590208311, -24.03113400032698621, -38.53105962718119315 ) ) ;
#8919 = CARTESIAN_POINT ( 'NONE',  ( -7.500000000000000000, -1.486698507076798847, -0.09861472150523799274 ) ) ;
#8920 = FACE_OUTER_BOUND ( 'NONE', #21393, .T. ) ;
#8921 = CARTESIAN_POINT ( 'NONE',  ( -38.99177359176184865, -60.00000000000002132, 50.73434467415564342 ) ) ;
#8922 = CARTESIAN_POINT ( 'NONE',  ( 11.48424297320331888, 12.75586303188949522, 10.00391324386538550 ) ) ;
#8923 = DIRECTION ( 'NONE',  ( -1.000000000000000000, 0.000000000000000000, 0.000000000000000000 ) ) ;
#8924 = CARTESIAN_POINT ( 'NONE',  ( -86.12441050467187154, -61.04151491554013376, 194.3981187559223827 ) ) ;
#8925 = CIRCLE ( 'NONE', #17579, 4.000000000000000888 ) ;
#8926 = ORIENTED_EDGE ( 'NONE', *, *, #70173, .T. ) ;
#8927 = FACE_OUTER_BOUND ( 'NONE', #57363, .T. ) ;
#8928 = CARTESIAN_POINT ( 'NONE',  ( -1.469576158976823947E-15, -12.87499999999999467, 8.000000000000000000 ) ) ;
#8929 = CARTESIAN_POINT ( 'NONE',  ( -7.081050772456690012, -32.51271769174685033, 29.29877307394730224 ) ) ;
#8930 = CARTESIAN_POINT ( 'NONE',  ( -5.908324243937765452, 41.91795894114439136, -59.12627178481003654 ) ) ;
#8931 = AXIS2_PLACEMENT_3D ( 'NONE', #58109, #73759, #57561 ) ;
#8932 = CARTESIAN_POINT ( 'NONE',  ( 87.14793098496349444, -38.00000000001091394, 189.0872956505646414 ) ) ;
#8934 = CARTESIAN_POINT ( 'NONE',  ( 5.624554194580569266, -65.83898597127696917, 14.17938030110289560 ) ) ;
#8933 = DIRECTION ( 'NONE',  ( 0.000000000000000000, 0.000000000000000000, 1.000000000000000000 ) ) ;
#8935 = EDGE_CURVE ( 'NONE', #44704, #23042, #75367, .T. ) ;
#8936 = ORIENTED_EDGE ( 'NONE', *, *, #18048, .F. ) ;
#8937 = FACE_OUTER_BOUND ( 'NONE', #58035, .T. ) ;
#8938 = LINE ( 'NONE', #74729, #75194 ) ;
#8939 = CARTESIAN_POINT ( 'NONE',  ( 16.12370107433553201, 34.43117400368613801, 24.14989126905659944 ) ) ;
#8940 =( GEOMETRIC_REPRESENTATION_CONTEXT ( 3 ) GLOBAL_UNCERTAINTY_ASSIGNED_CONTEXT ( ( #17105 ) ) GLOBAL_UNIT_ASSIGNED_CONTEXT ( ( #57913, #106465, #98384 ) ) REPRESENTATION_CONTEXT ( 'NONE', 'WORKASPACE' ) );
#8941 = CARTESIAN_POINT ( 'NONE',  ( 33.03761854510200635, 300.1793615339376515, -0.8055793472020765789 ) ) ;
#8942 = ADVANCED_FACE ( 'NONE', ( #48372 ), #70151, .F. ) ;
#8943 = DIRECTION ( 'NONE',  ( 0.000000000000000000, -0.000000000000000000, 1.000000000000000000 ) ) ;
#8944 = CIRCLE ( 'NONE', #84802, 4.000000000000000000 ) ;
#8945 = SURFACE_STYLE_FILL_AREA ( #81229 ) ;
#8946 = CARTESIAN_POINT ( 'NONE',  ( 106.4003153237399459, -14.21045842199437281, 159.7124754531589019 ) ) ;
#8947 = VERTEX_POINT ( 'NONE', #97448 ) ;
#8948 = FACE_OUTER_BOUND ( 'NONE', #65687, .T. ) ;
#8949 = CARTESIAN_POINT ( 'NONE',  ( 4.472135954999581386, -10.00000000000000888, -4.000000000000000000 ) ) ;
#8950 = CYLINDRICAL_SURFACE ( 'NONE', #32197, 5.000000000000002665 ) ;
#8951 = CARTESIAN_POINT ( 'NONE',  ( 35.11650669486618170, 4.000000000000003553, 4.898587196589414801E-16 ) ) ;
#8952 = CARTESIAN_POINT ( 'NONE',  ( 6.683837171061806970, -7.911893696991936231, 5.688671339918660213E-17 ) ) ;
#8953 = EDGE_LOOP ( 'NONE', ( #29346, #56609, #36486, #53269 ) ) ;
#8954 = CARTESIAN_POINT ( 'NONE',  ( 36.36650669486618881, 4.000000000000003553, 4.898587196589414801E-16 ) ) ;
#8955 = ORIENTED_EDGE ( 'NONE', *, *, #94181, .T. ) ;
#8956 = CARTESIAN_POINT ( 'NONE',  ( 34.05209713062498622, 485.0008159996403378, 0.6776390644912295702 ) ) ;
#8957 = CARTESIAN_POINT ( 'NONE',  ( 31.35484960135613619, 439.6865637981555324, 23.41922880401698137 ) ) ;
#8958 = CARTESIAN_POINT ( 'NONE',  ( 32.68648381767908973, 486.2785269687594223, 6.276066868107815999 ) ) ;
#8959 = CARTESIAN_POINT ( 'NONE',  ( 5.000000000000000888, -14.19087030043145603, 13.37859801196370313 ) ) ;
#8961 = CARTESIAN_POINT ( 'NONE',  ( -35.47086896947185153, -60.00000000000493827, 50.14652216712747190 ) ) ;
#8960 = AXIS2_PLACEMENT_3D ( 'NONE', #54857, #46784, #87787 ) ;
#8962 = DIRECTION ( 'NONE',  ( -1.000000000000000000, -1.224606353822377258E-16, -0.000000000000000000 ) ) ;
#8963 = VERTEX_POINT ( 'NONE', #15482 ) ;
#8964 = CARTESIAN_POINT ( 'NONE',  ( 111.5499265342648840, -60.00000000000001421, 157.8294912153404255 ) ) ;
#8965 = CIRCLE ( 'NONE', #22784, 4.000000000000000888 ) ;
#8967 = CARTESIAN_POINT ( 'NONE',  ( 13.47176107517659638, -39.47274912387565848, 30.55088658083724695 ) ) ;
#8966 = CARTESIAN_POINT ( 'NONE',  ( -78.82101707352518360, -14.21045842199447584, 187.8153594499050882 ) ) ;
#8968 = PRODUCT_DEFINITION_CONTEXT ( 'detailed design', #38327, 'design' ) ;
#8969 = DIRECTION ( 'NONE',  ( 1.000000000000000000, 0.000000000000000000, 0.000000000000000000 ) ) ;
#8970 = CARTESIAN_POINT ( 'NONE',  ( -42.69126397430579800, -56.80055262131805449, 45.33095584542797241 ) ) ;
#8971 = PRESENTATION_LAYER_ASSIGNMENT (  '', '', ( #41704 ) ) ;
#8972 = EDGE_CURVE ( 'NONE', #103169, #11929, #83920, .T. ) ;
#8973 = DIRECTION ( 'NONE',  ( -0.000000000000000000, -1.000000000000000000, -0.000000000000000000 ) ) ;
#8974 = VERTEX_POINT ( 'NONE', #57518 ) ;
#8975 = FILL_AREA_STYLE ('',( #27887 ) ) ;
#8976 = CARTESIAN_POINT ( 'NONE',  ( 8.241142027370402801, 54.07563880005658774, 1.561398477666883888 ) ) ;
#8977 = CARTESIAN_POINT ( 'NONE',  ( 5.979482036612520979, -14.26481676427871470, 14.07238976267240815 ) ) ;
#8978 = DIRECTION ( 'NONE',  ( -1.000000000000000000, -1.224606353822377258E-16, -0.000000000000000000 ) ) ;
#8979 = CARTESIAN_POINT ( 'NONE',  ( 18.59882702213898753, 304.6205295274080527, -9.049158645989061611 ) ) ;
#8980 = CARTESIAN_POINT ( 'NONE',  ( 18.13561277374696701, 1.340359594676612611E-15, 0.000000000000000000 ) ) ;
#8981 = EDGE_LOOP ( 'NONE', ( #16881, #51707, #69251, #45826 ) ) ;
#8982 = CARTESIAN_POINT ( 'NONE',  ( 0.000000000000000000, 0.000000000000000000, -2.575493252495433261 ) ) ;
#8983 = CARTESIAN_POINT ( 'NONE',  ( 16.98789274048672127, 303.5779513886026280, -10.05824692440026169 ) ) ;
#8984 = ORIENTED_EDGE ( 'NONE', *, *, #91225, .T. ) ;
#8985 = CARTESIAN_POINT ( 'NONE',  ( 60.59444657107560772, -30.00000000001982059, 93.60444982598512809 ) ) ;
#8986 = CARTESIAN_POINT ( 'NONE',  ( 19.43279966247120072, 41.87228345916210515, -80.47899240423528511 ) ) ;
#8987 = CARTESIAN_POINT ( 'NONE',  ( 7.899999792244757124, -11.02739026146943857, -1.226164894445325171E-14 ) ) ;
#8988 = DIRECTION ( 'NONE',  ( -0.000000000000000000, -0.000000000000000000, -1.000000000000000000 ) ) ;
#8989 = CARTESIAN_POINT ( 'NONE',  ( 80.76851621713109353, -30.00000000000000355, 10.64488254787337063 ) ) ;
#8990 = CARTESIAN_POINT ( 'NONE',  ( 6.943482370013978944, 104.4715162973927534, 3.973876482044368164 ) ) ;
#8991 = EDGE_CURVE ( 'NONE', #17004, #34393, #97768, .T. ) ;
#8992 = ORIENTED_EDGE ( 'NONE', *, *, #19213, .T. ) ;
#8993 = EDGE_CURVE ( 'NONE', #22326, #19286, #92620, .T. ) ;
#8994 = ORIENTED_EDGE ( 'NONE', *, *, #79912, .T. ) ;
#8995 = ORIENTED_EDGE ( 'NONE', *, *, #86330, .T. ) ;
#8996 = FACE_OUTER_BOUND ( 'NONE', #42730, .T. ) ;
#8997 = CARTESIAN_POINT ( 'NONE',  ( -6.701893397842001221, 41.44328394191487774, -70.59544911652842814 ) ) ;
#8998 = DIRECTION ( 'NONE',  ( 0.000000000000000000, -1.000000000000000000, 0.000000000000000000 ) ) ;
#8999 = CARTESIAN_POINT ( 'NONE',  ( -40.70972807814067096, 464.1553110665033159, 18.16976512832724922 ) ) ;
#9000 = CARTESIAN_POINT ( 'NONE',  ( -31.16305316186402408, 374.7586899056589118, 23.86554239046190418 ) ) ;
#9001 = CARTESIAN_POINT ( 'NONE',  ( 0.000000000000000000, -80.00000000000000000, 27.00000000000000000 ) ) ;
#9002 = VERTEX_POINT ( 'NONE', #32762 ) ;
#9003 = CARTESIAN_POINT ( 'NONE',  ( 9.646032546913144046, 108.0128032847436401, 2.644051433538247231 ) ) ;
#9004 = ORIENTED_EDGE ( 'NONE', *, *, #83556, .F. ) ;
#9005 = CARTESIAN_POINT ( 'NONE',  ( 72.37206225042174879, 6.856755485862130937E-15, 0.000000000000000000 ) ) ;
#9006 = CARTESIAN_POINT ( 'NONE',  ( 71.58809529799425775, -38.32751537232760342, 143.4284849665567094 ) ) ;
#9007 = CARTESIAN_POINT ( 'NONE',  ( 6.585468679846620432, 3.617797563910807312, -6.733790807807556789 ) ) ;
#9008 = CARTESIAN_POINT ( 'NONE',  ( 25.99470359582689838, 305.5572448969162451, 10.54713035941321131 ) ) ;
#9009 = DIRECTION ( 'NONE',  ( 0.000000000000000000, -1.000000000000000000, 0.000000000000000000 ) ) ;
#9010 = MECHANICAL_DESIGN_GEOMETRIC_PRESENTATION_REPRESENTATION (  '', ( #98550 ), #81362 ) ;
#9011 = CARTESIAN_POINT ( 'NONE',  ( -28.04617107623481331, 34.20660251098871640, -9.634014743738612552 ) ) ;
#9012 = CARTESIAN_POINT ( 'NONE',  ( 42.41247034190681831, 353.4773973720574531, 15.30157164444485574 ) ) ;
#9013 = FACE_OUTER_BOUND ( 'NONE', #89613, .T. ) ;
#9014 = EDGE_CURVE ( 'NONE', #98734, #7404, #4785, .T. ) ;
#9015 = B_SPLINE_CURVE_WITH_KNOTS ( 'NONE', 3,
 ( #80607, #97859, #46661, #104912, #89781, #31051, #79559, #63406, #23479, #5673, #71459, #6731, #104358, #15351, #30506, #48237, #39655, #96300, #22425, #72525 ),
 .UNSPECIFIED., .F., .F.,
 ( 4, 2, 2, 2, 2, 2, 2, 2, 2, 4 ),
 ( 0.006849800839412230336, 0.007353416717026173451, 0.007857032594640116566, 0.008864264349868001061, 0.009116072288674979124, 0.009367880227481957187, 0.009619688166288935249, 0.009871496105095911577, 0.01037511198270986770, 0.01087872786032382383 ),
 .UNSPECIFIED. ) ;
#9016 = VERTEX_POINT ( 'NONE', #32217 ) ;
#9017 = CARTESIAN_POINT ( 'NONE',  ( -20.64401833605449355, 302.8990037343777999, 9.947032289444299735 ) ) ;
#9018 = CARTESIAN_POINT ( 'NONE',  ( 18.86650669486618881, -3.999999999999998224, 0.000000000000000000 ) ) ;
#9019 = DIRECTION ( 'NONE',  ( 0.9086146812045996501, 0.000000000000000000, 0.4176354404255748221 ) ) ;
#9020 = CARTESIAN_POINT ( 'NONE',  ( 41.97104496162273790, -38.13452990356884698, 52.68411854546428685 ) ) ;
#9021 = CIRCLE ( 'NONE', #38318, 4.000000000000001776 ) ;
#9022 = ADVANCED_FACE ( 'NONE', ( #47833 ), #64062, .F. ) ;
#9023 = CARTESIAN_POINT ( 'NONE',  ( 7.726405549742459300, 296.0527277817394634, 6.373329964583255958 ) ) ;
#9024 = FACE_OUTER_BOUND ( 'NONE', #92995, .T. ) ;
#9025 = CARTESIAN_POINT ( 'NONE',  ( 86.20875240452089372, -24.70518494214491767, 181.2918537991968435 ) ) ;
#9026 = CARTESIAN_POINT ( 'NONE',  ( 17.99842623603791480, 36.44670248777274679, -23.18063615129692678 ) ) ;
#9027 = DIRECTION ( 'NONE',  ( -1.000000000000000000, -1.224606353822377258E-16, -0.000000000000000000 ) ) ;
#9028 = ORIENTED_EDGE ( 'NONE', *, *, #17009, .F. ) ;
#9029 = CARTESIAN_POINT ( 'NONE',  ( 85.73719764786143571, -57.67053834193623629, -26.44931048121824091 ) ) ;
#9030 = ADVANCED_FACE ( 'NONE', ( #93099 ), #19272, .T. ) ;
#9031 = FACE_OUTER_BOUND ( 'NONE', #58296, .T. ) ;
#9032 = CARTESIAN_POINT ( 'NONE',  ( 8.673617379884035472E-16, 7.505553499465148271, -0.7999999999999977129 ) ) ;
#9033 = CARTESIAN_POINT ( 'NONE',  ( 8.000000000000000000, -18.40624999999999289, -3.313708498984761164 ) ) ;
#9034 = CONICAL_SURFACE ( 'NONE', #76258, 4.172000000000001485, 0.9599310885968750373 ) ;
#9035 = CARTESIAN_POINT ( 'NONE',  ( -81.36514358934235247, -30.00000000000001066, -1.450368654527133039 ) ) ;
#9036 = MECHANICAL_DESIGN_GEOMETRIC_PRESENTATION_REPRESENTATION (  '', ( #53857 ), #41770 ) ;
#9037 = AXIS2_PLACEMENT_3D ( 'NONE', #28148, #3843, #75592 ) ;
#9038 = DIRECTION ( 'NONE',  ( -1.000000000000000000, -1.224606353822377258E-16, -0.000000000000000000 ) ) ;
#9039 = CARTESIAN_POINT ( 'NONE',  ( -6.701893397842001221, 41.44328394191487774, -70.59544911652842814 ) ) ;
#9040 = CARTESIAN_POINT ( 'NONE',  ( 29.34999999999999787, -3.309499999999999886, 0.000000000000000000 ) ) ;
#9042 = CARTESIAN_POINT ( 'NONE',  ( 0.06730325657375685333, -1.557442666578433776, -8.000000000000000000 ) ) ;
#9041 = LINE ( 'NONE', #82943, #89730 ) ;
#9043 = DIRECTION ( 'NONE',  ( -1.000000000000000000, -1.224606353822377258E-16, -0.000000000000000000 ) ) ;
#9044 = CARTESIAN_POINT ( 'NONE',  ( -29.27137781856736609, 18.74786498819646496, 39.67318581983477088 ) ) ;
#9045 = CARTESIAN_POINT ( 'NONE',  ( -12.50000000000000711, -4.999999999999999112, -80.60844091781802945 ) ) ;
#9046 = LINE ( 'NONE', #41952, #70107 ) ;
#9047 = DIRECTION ( 'NONE',  ( -1.000000000000000000, -1.224606353822377258E-16, -0.000000000000000000 ) ) ;
#9048 = CARTESIAN_POINT ( 'NONE',  ( 101.2019940638598854, -5.000000000000000000, 6.123233995736778115E-16 ) ) ;
#9049 = CARTESIAN_POINT ( 'NONE',  ( 14.34999999999999787, -3.309499999999999886, 4.475777889183790779E-16 ) ) ;
#9050 = B_SPLINE_CURVE_WITH_KNOTS ( 'NONE', 3,
 ( #62125, #78795, #78273, #69663 ),
 .UNSPECIFIED., .F., .F.,
 ( 4, 4 ),
 ( 5.721958498152796815E-17, 0.001448684797825249872 ),
 .UNSPECIFIED. ) ;
#9051 = EDGE_LOOP ( 'NONE', ( #26158, #69384, #51202, #99964 ) ) ;
#9052 = DIRECTION ( 'NONE',  ( 0.000000000000000000, -1.000000000000000000, 0.000000000000000000 ) ) ;
#9053 = FILL_AREA_STYLE ('',( #89985 ) ) ;
#9054 = CARTESIAN_POINT ( 'NONE',  ( -8.000113193197767814, 80.99977361354139305, -0.2613481123984612853 ) ) ;
#9055 = CARTESIAN_POINT ( 'NONE',  ( -63.92444039710895254, -29.66271673368065365, -23.50404950011429506 ) ) ;
#9057 = CARTESIAN_POINT ( 'NONE',  ( 0.000000000000000000, -1.000000000000000000, 15.43455230191221261 ) ) ;
#9056 = CARTESIAN_POINT ( 'NONE',  ( 8.000000000000000000, 9.797174393178825657E-16, -7.424942857142857733 ) ) ;
#9058 = EDGE_CURVE ( 'NONE', #89315, #24456, #49575, .T. ) ;
#9059 = ORIENTED_EDGE ( 'NONE', *, *, #14452, .F. ) ;
#9060 = B_SPLINE_CURVE_WITH_KNOTS ( 'NONE', 3,
 ( #60797, #26335, #36019, #93149 ),
 .UNSPECIFIED., .F., .F.,
 ( 4, 4 ),
 ( 0.000000000000000000, 0.0002642584603507367683 ),
 .UNSPECIFIED. ) ;
#9061 = ORIENTED_EDGE ( 'NONE', *, *, #23207, .F. ) ;
#9062 = CARTESIAN_POINT ( 'NONE',  ( -2.499999999999995559, -30.00000000000000000, -14.79019945774903810 ) ) ;
#9063 = EDGE_CURVE ( 'NONE', #84468, #80603, #54724, .T. ) ;
#9064 = CARTESIAN_POINT ( 'NONE',  ( 39.59239511134280320, 490.2207323505293175, 11.38527476693367646 ) ) ;
#9065 = SURFACE_STYLE_USAGE ( .BOTH. , #73805 ) ;
#9066 = CARTESIAN_POINT ( 'NONE',  ( -19.54990280911475509, -60.00000000000001421, -41.86024675016059859 ) ) ;
#9067 = VERTEX_POINT ( 'NONE', #18163 ) ;
#9068 = PRESENTATION_STYLE_ASSIGNMENT (( #92119 ) ) ;
#9069 = CARTESIAN_POINT ( 'NONE',  ( -4.404494731813556108, 294.7962499846886431, -8.995593899024026285 ) ) ;
#9070 = CARTESIAN_POINT ( 'NONE',  ( 101.6834587361868927, -52.72719984991043418, 192.5473745686417715 ) ) ;
#9071 = AXIS2_PLACEMENT_3D ( 'NONE', #18840, #92143, #52216 ) ;
#9073 = CARTESIAN_POINT ( 'NONE',  ( -47.90347347824249624, 10.05236241843093481, 16.85535821593516559 ) ) ;
#9072 = CARTESIAN_POINT ( 'NONE',  ( 0.000000000000000000, 15.00000000000000000, 0.000000000000000000 ) ) ;
#9074 = ADVANCED_FACE ( 'NONE', ( #92029 ), #42412, .F. ) ;
#9075 = ORIENTED_EDGE ( 'NONE', *, *, #30298, .T. ) ;
#9076 = ORIENTED_EDGE ( 'NONE', *, *, #34757, .F. ) ;
#9077 = COLOUR_RGB ( '', 0.09019608, 0.27058824, 0.51372549) ;
#9078 = ORIENTED_EDGE ( 'NONE', *, *, #61209, .T. ) ;
#9079 = CARTESIAN_POINT ( 'NONE',  ( 30.46151443478357024, 326.5429411037146679, 15.51295837324801141 ) ) ;
#9080 = DIRECTION ( 'NONE',  ( 0.5735764363510462704, 0.8191520442889915765, 0.000000000000000000 ) ) ;
#9081 = CARTESIAN_POINT ( 'NONE',  ( 69.92761780597730592, 6.856755485862130937E-15, 0.000000000000000000 ) ) ;
#9082 = ORIENTED_EDGE ( 'NONE', *, *, #44161, .T. ) ;
#9083 = CARTESIAN_POINT ( 'NONE',  ( 10.73176661990081371, 1.340359594676612611E-15, 0.000000000000000000 ) ) ;
#9084 = CARTESIAN_POINT ( 'NONE',  ( 32.33349330513380693, 1.593028355512270962E-15, 0.000000000000000000 ) ) ;
#9085 = CARTESIAN_POINT ( 'NONE',  ( -5.651997800604014799, -57.67124204504380458, 41.59089347824649252 ) ) ;
#9086 = CARTESIAN_POINT ( 'NONE',  ( -7.188101187500001821, -32.00000000204838813, -2.977408999572651371 ) ) ;
#9087 = CARTESIAN_POINT ( 'NONE',  ( -30.59538916938590702, 12.96143355072256753, 41.71318167414145961 ) ) ;
#9088 = CARTESIAN_POINT ( 'NONE',  ( -31.11679462788039530, 441.4271381875185511, 23.27438508043199406 ) ) ;
#9089 = CARTESIAN_POINT ( 'NONE',  ( -6.784953749642196996, 41.67963440881483450, -59.00226708758491156 ) ) ;
#9090 = MECHANICAL_DESIGN_GEOMETRIC_PRESENTATION_REPRESENTATION (  '', ( #57200 ), #50429 ) ;
#9091 = CARTESIAN_POINT ( 'NONE',  ( -81.17775171884230190, -14.21045842199422005, -20.84891578014651259 ) ) ;
#9092 = CARTESIAN_POINT ( 'NONE',  ( 1.295095875561511761E-05, -30.00000000000000000, 37.00000000000000711 ) ) ;
#9093 = B_SPLINE_CURVE_WITH_KNOTS ( 'NONE', 3,
 ( #15359, #24025, #6736, #80615 ),
 .UNSPECIFIED., .F., .F.,
 ( 4, 4 ),
 ( 8.420559318810145779E-18, 0.001259908249732933022 ),
 .UNSPECIFIED. ) ;
#9094 = CARTESIAN_POINT ( 'NONE',  ( -49.49064989153462335, -46.44333672598879303, 52.19747830327506222 ) ) ;
#9095 = DIRECTION ( 'NONE',  ( -0.000000000000000000, -0.000000000000000000, 1.000000000000000000 ) ) ;
#9096 = EDGE_LOOP ( 'NONE', ( #88332, #60119 ) ) ;
#9097 = CARTESIAN_POINT ( 'NONE',  ( -100.5716031806942397, -52.74657777821607851, 193.7722495540973568 ) ) ;
#9098 = CARTESIAN_POINT ( 'NONE',  ( -3.947200809147736411, 295.9771890841169011, -10.00641236124439715 ) ) ;
#9099 = CARTESIAN_POINT ( 'NONE',  ( 9.587897109658308992, -3.381009470459365840, 14.88767535522079122 ) ) ;
#9100 = ORIENTED_EDGE ( 'NONE', *, *, #59454, .F. ) ;
#9101 = CARTESIAN_POINT ( 'NONE',  ( -16.64348903516517098, 43.47556584774767430, 6.657797401561654560 ) ) ;
#9102 = CARTESIAN_POINT ( 'NONE',  ( 78.23225470723293995, -38.60547359199907191, 189.0516081268614244 ) ) ;
#9103 =( NAMED_UNIT ( * ) PLANE_ANGLE_UNIT ( ) SI_UNIT ( $, .RADIAN. ) );
#9104 = CARTESIAN_POINT ( 'NONE',  ( 15.11650669486618881, 1.474610560812782335E-15, 0.000000000000000000 ) ) ;
#9105 = CARTESIAN_POINT ( 'NONE',  ( -7.898269865231990039, -11.02838903529593573, -12.97150009825808503 ) ) ;
#9106 = CARTESIAN_POINT ( 'NONE',  ( -45.60838156032659896, 42.00000000000000000, 79.13121736029036413 ) ) ;
#9107 = CARTESIAN_POINT ( 'NONE',  ( 90.60055052440634427, -30.00000000000000000, 190.2884839676575268 ) ) ;
#9108 = AXIS2_PLACEMENT_3D ( 'NONE', #27955, #52168, #85623 ) ;
#9109 = CARTESIAN_POINT ( 'NONE',  ( 35.43142158411064457, 491.1302584545976515, 12.10548931029503983 ) ) ;
#9110 = FILL_AREA_STYLE ('',( #66297 ) ) ;
#9111 = CARTESIAN_POINT ( 'NONE',  ( 36.48461538461538822, 1.411358822780289120E-15, 0.000000000000000000 ) ) ;
#9112 = EDGE_LOOP ( 'NONE', ( #56861, #75835, #64307, #94961 ) ) ;
#9113 = ORIENTED_EDGE ( 'NONE', *, *, #57976, .F. ) ;
#9114 = CARTESIAN_POINT ( 'NONE',  ( 51.71506308164819643, -25.64903502818010139, 48.87485861820827182 ) ) ;
#9115 = AXIS2_PLACEMENT_3D ( 'NONE', #48798, #81689, #73610 ) ;
#9116 = CARTESIAN_POINT ( 'NONE',  ( 6.492511067189948193, 41.78432740739263096, -59.03547063838887965 ) ) ;
#9117 = CARTESIAN_POINT ( 'NONE',  ( 36.94526041798086169, 28.08663898282346949, -11.10947391786501193 ) ) ;
#9118 = VERTEX_POINT ( 'NONE', #34896 ) ;
#9119 = CARTESIAN_POINT ( 'NONE',  ( -109.8761471886628414, -38.35606193139696529, 153.1324815485978093 ) ) ;
#9120 = VERTEX_POINT ( 'NONE', #52098 ) ;
#9121 = CARTESIAN_POINT ( 'NONE',  ( 15.64030048137865947, 6.456385560668104873, 7.561819230143442816 ) ) ;
#9122 = CARTESIAN_POINT ( 'NONE',  ( 109.6530265699404509, -38.35603087673744938, 151.1878659942163949 ) ) ;
#9123 = CARTESIAN_POINT ( 'NONE',  ( 13.75587262240292930, 20.47468597617315567, -6.665350514229143819 ) ) ;
#9124 = CARTESIAN_POINT ( 'NONE',  ( 95.06247054295488397, -60.15120782134928845, 86.15213186706492365 ) ) ;
#9125 = CARTESIAN_POINT ( 'NONE',  ( -31.13499213488098505, 439.5204445682307437, 23.00710445961532358 ) ) ;
#9126 = CARTESIAN_POINT ( 'NONE',  ( -1.010142498354813734, 46.02241059309989879, -16.74584960336704498 ) ) ;
#9127 = CARTESIAN_POINT ( 'NONE',  ( -28.57185684847394569, 309.4411263248405817, -7.951019538551619803 ) ) ;
#9128 = CARTESIAN_POINT ( 'NONE',  ( 4.586505539341392712, -65.62869095158480093, 13.11449450926818905 ) ) ;
#9129 = CARTESIAN_POINT ( 'NONE',  ( 73.97498551117102750, -60.00000000000000000, 171.9667912108089922 ) ) ;
#9130 = CARTESIAN_POINT ( 'NONE',  ( -2.499999999999963141, -18.83381654053417620, 27.02533567785737034 ) ) ;
#9131 = CARTESIAN_POINT ( 'NONE',  ( 17.51085981868257591, 45.00000000000000000, 63.60668009671144318 ) ) ;
#9132 = ORIENTED_EDGE ( 'NONE', *, *, #2691, .F. ) ;
#9133 = CARTESIAN_POINT ( 'NONE',  ( 58.97917396427931891, -53.38380800473449739, 76.07987900925265023 ) ) ;
#9134 = CARTESIAN_POINT ( 'NONE',  ( -26.35358385847169416, 295.9512351630701232, -9.763468370421369613 ) ) ;
#9135 = CARTESIAN_POINT ( 'NONE',  ( 0.1685051182689021043, 36.30322183991232521, 29.74144779452618792 ) ) ;
#9136 = ADVANCED_FACE ( 'NONE', ( #17629 ), #1944, .T. ) ;
#9137 = CARTESIAN_POINT ( 'NONE',  ( 63.07777777777777573, -3.309500000000000774, 4.475777889183797681E-16 ) ) ;
#9139 = CARTESIAN_POINT ( 'NONE',  ( -35.85122874546545546, 485.1582092647775539, -2.238595989622043092 ) ) ;
#9138 = CARTESIAN_POINT ( 'NONE',  ( -74.98372929288009914, -30.00000000032233416, 156.5717653030027918 ) ) ;
#9140 = CARTESIAN_POINT ( 'NONE',  ( -41.13637439020717324, 328.1376453396359238, 10.03865748547844561 ) ) ;
#9141 = CARTESIAN_POINT ( 'NONE',  ( -5.000000000000000000, 0.000000000000000000, -2.868028571428571372 ) ) ;
#9142 = DIRECTION ( 'NONE',  ( -1.000000000000000000, -0.000000000000000000, -0.000000000000000000 ) ) ;
#9143 = CARTESIAN_POINT ( 'NONE',  ( -8.000000000000001776, -26.65624999999999645, 3.313708498984758943 ) ) ;
#9144 = CARTESIAN_POINT ( 'NONE',  ( -18.91791044776116237, 45.90000000000000568, 62.18611311450883505 ) ) ;
#9145 = EDGE_CURVE ( 'NONE', #60319, #16386, #56408, .T. ) ;
#9146 = CARTESIAN_POINT ( 'NONE',  ( 41.61668529618731327, 47.99999999999999289, 50.19614130198702640 ) ) ;
#9147 = CIRCLE ( 'NONE', #5768, 2.999999999999999112 ) ;
#9148 = VERTEX_POINT ( 'NONE', #1401 ) ;
#9149 = CARTESIAN_POINT ( 'NONE',  ( 84.10407772408511562, -39.43706024606296978, 178.9938989443399748 ) ) ;
#9150 = DIRECTION ( 'NONE',  ( 0.000000000000000000, 0.000000000000000000, 1.000000000000000000 ) ) ;
#9151 = CARTESIAN_POINT ( 'NONE',  ( -5.656854249492379694, -9.125000004096769146, -5.656854249492380582 ) ) ;
#9152 = ORIENTED_EDGE ( 'NONE', *, *, #25446, .F. ) ;
#9153 = CARTESIAN_POINT ( 'NONE',  ( 93.39999999999999147, -4.171999999999998820, 0.000000000000000000 ) ) ;
#9154 = EDGE_CURVE ( 'NONE', #59570, #96186, #51565, .T. ) ;
#9155 = LINE ( 'NONE', #99772, #82033 ) ;
#9156 = DIRECTION ( 'NONE',  ( 0.000000000000000000, 0.000000000000000000, 1.000000000000000000 ) ) ;
#9157 =( NAMED_UNIT ( * ) PLANE_ANGLE_UNIT ( ) SI_UNIT ( $, .RADIAN. ) );
#9158 = CARTESIAN_POINT ( 'NONE',  ( -15.69138703980276262, -24.30991770495803905, -38.52719090127629897 ) ) ;
#9159 = DIRECTION ( 'NONE',  ( 0.5735764363510462704, 0.8191520442889915765, 0.000000000000000000 ) ) ;
#9160 = CARTESIAN_POINT ( 'NONE',  ( 56.79672723872580775, -60.00000000000000000, 90.54572580908420321 ) ) ;
#9161 = FACE_OUTER_BOUND ( 'NONE', #99135, .T. ) ;
#9163 = CARTESIAN_POINT ( 'NONE',  ( -12.78782033920715833, 21.25124815179102811, -5.673828052979907000 ) ) ;
#9162 = CARTESIAN_POINT ( 'NONE',  ( -26.71188838280077960, -30.21239539108677619, 38.94092172635536997 ) ) ;
#9164 = CARTESIAN_POINT ( 'NONE',  ( -9.698972129396508990, 88.17629712741940295, -2.445345647270319667 ) ) ;
#9165 = CARTESIAN_POINT ( 'NONE',  ( -7.188101187500002709, -10.81250000204838457, 2.977408999572648707 ) ) ;
#9166 = DIRECTION ( 'NONE',  ( 0.000000000000000000, 0.000000000000000000, 1.000000000000000000 ) ) ;
#9167 = DIRECTION ( 'NONE',  ( 0.5735764363510470476, -0.8191520442889911324, 1.003171929053524007E-16 ) ) ;
#9168 = EDGE_LOOP ( 'NONE', ( #70085, #29767, #81179, #71520, #89635 ) ) ;
#9169 = CARTESIAN_POINT ( 'NONE',  ( -17.50000000000507683, 48.51938947813042091, 62.60970113051429564 ) ) ;
#9170 = CIRCLE ( 'NONE', #43612, 4.172000000000001485 ) ;
#9171 = VECTOR ( 'NONE', #87564, 1000.000000000000114 ) ;
#9173 = CARTESIAN_POINT ( 'NONE',  ( 44.04518021092881952, -34.58949428284888228, -28.87998162211279052 ) ) ;
#9172 = CARTESIAN_POINT ( 'NONE',  ( 4.329523338144593225, 54.29298348168710930, 6.476737974868277625 ) ) ;
#9174 = EDGE_CURVE ( 'NONE', #86580, #4466, #57982, .T. ) ;
#9175 = STYLED_ITEM ( 'NONE', ( #100970 ), #7337 ) ;
#9176 = ORIENTED_EDGE ( 'NONE', *, *, #1113, .F. ) ;
#9177 = VECTOR ( 'NONE', #780, 1000.000000000000000 ) ;
#9178 = CARTESIAN_POINT ( 'NONE',  ( -5.855777637195783925, -88.78106496758448429, -1.331220292256681592 ) ) ;
#9179 = SURFACE_STYLE_FILL_AREA ( #82558 ) ;
#9180 = AXIS2_PLACEMENT_3D ( 'NONE', #6895, #360, #91032 ) ;
#9181 = ORIENTED_EDGE ( 'NONE', *, *, #61082, .F. ) ;
#9182 = ADVANCED_FACE ( 'NONE', ( #71463 ), #60752, .F. ) ;
#9183 = DIRECTION ( 'NONE',  ( -1.000000000000000000, -0.000000000000000000, -0.000000000000000000 ) ) ;
#9184 = EDGE_CURVE ( 'NONE', #231, #101774, #25116, .T. ) ;
#9185 = CARTESIAN_POINT ( 'NONE',  ( 52.56483885390523625, 48.00000000000000000, -38.23529411764706509 ) ) ;
#9186 = CARTESIAN_POINT ( 'NONE',  ( -19.44323342421834866, 41.87186953726217098, -80.46484636551333836 ) ) ;
#9187 = CARTESIAN_POINT ( 'NONE',  ( -95.54720156996677360, -59.99999999999999289, 52.92735314107190447 ) ) ;
#9188 = FACE_OUTER_BOUND ( 'NONE', #34576, .T. ) ;
#9189 = CARTESIAN_POINT ( 'NONE',  ( -1.843253007570911225E-16, -9.147862274876562338, -8.047472243342939535 ) ) ;
#9190 = CARTESIAN_POINT ( 'NONE',  ( 32.54922218626916930, 319.8023524069591303, -6.363686095274232457 ) ) ;
#9191 = CARTESIAN_POINT ( 'NONE',  ( 41.35053930177047476, 461.4196900451150327, 2.572867796617790415 ) ) ;
#9193 = CARTESIAN_POINT ( 'NONE',  ( 19.61638200451619696, 1.340359594676612611E-15, 0.000000000000000000 ) ) ;
#9192 = CARTESIAN_POINT ( 'NONE',  ( -33.13449099605734460, 435.1334182590073851, 11.13154690284580894 ) ) ;
#9194 = CARTESIAN_POINT ( 'NONE',  ( -82.39419631509804276, -46.47357755561642989, 175.1841951907930479 ) ) ;
#9195 = EDGE_LOOP ( 'NONE', ( #95142, #99144, #68812, #62307 ) ) ;
#9196 = DIRECTION ( 'NONE',  ( 0.000000000000000000, -0.9746667163790341259, 0.2236622274388584686 ) ) ;
#9197 = ORIENTED_EDGE ( 'NONE', *, *, #42849, .T. ) ;
#9198 =( BOUNDED_CURVE ( )  B_SPLINE_CURVE ( 2, ( #80835, #31783, #65194 ),
 .UNSPECIFIED., .F., .F. ) 
 B_SPLINE_CURVE_WITH_KNOTS ( ( 3, 3 ),
 ( 0.000000000000000000, 1.000000000000000000 ),
 .UNSPECIFIED. ) 
 CURVE ( )  GEOMETRIC_REPRESENTATION_ITEM ( )  RATIONAL_B_SPLINE_CURVE ( ( 1.000000000000000000, 1.857142857142858317, 1.000000000000000000 ) ) 
 REPRESENTATION_ITEM ( '' )  );
#9199 = ORIENTED_EDGE ( 'NONE', *, *, #66561, .T. ) ;
#9201 = ADVANCED_FACE ( 'NONE', ( #3563 ), #86458, .F. ) ;
#9200 = CARTESIAN_POINT ( 'NONE',  ( 28.86650669486618881, -3.999999999999998224, 0.000000000000000000 ) ) ;
#9202 = DIRECTION ( 'NONE',  ( -0.000000000000000000, -0.000000000000000000, -1.000000000000000000 ) ) ;
#9203 = VERTEX_POINT ( 'NONE', #7783 ) ;
#9204 = EDGE_CURVE ( 'NONE', #94380, #96401, #85373, .T. ) ;
#9205 = CARTESIAN_POINT ( 'NONE',  ( -19.73463816634106038, 304.7971333121957969, 8.925379062039111133 ) ) ;
#9206 = CARTESIAN_POINT ( 'NONE',  ( -2.499999999999963141, -18.83381654053417620, 27.02533567785737034 ) ) ;
#9207 = CARTESIAN_POINT ( 'NONE',  ( 39.83349330513380693, 1.593028355512270567E-15, 0.000000000000000000 ) ) ;
#9208 = CARTESIAN_POINT ( 'NONE',  ( -7.213352437320215138, -62.98163526992318850, -3.463014597543483841 ) ) ;
#9209 = CARTESIAN_POINT ( 'NONE',  ( -0.7844422002871876964, 53.48242548866619472, 9.987131087015052699 ) ) ;
#9210 = CARTESIAN_POINT ( 'NONE',  ( -13.76576316043658643, -50.82162839084075756, 29.55959131405483475 ) ) ;
#9211 = CARTESIAN_POINT ( 'NONE',  ( -43.18779636046989623, 464.9503604947622648, 14.53715779820235099 ) ) ;
#9212 = CARTESIAN_POINT ( 'NONE',  ( 113.8520663817495233, -59.99999999999995026, 157.1483003829898450 ) ) ;
#9213 = EDGE_CURVE ( 'NONE', #101, #25485, #59350, .T. ) ;
#9214 = CARTESIAN_POINT ( 'NONE',  ( -109.0818456041877766, -30.00000000000003908, 182.6288557207085148 ) ) ;
#9215 = CARTESIAN_POINT ( 'NONE',  ( -59.14235056471916607, -22.12910259080065600, 62.21584231372889917 ) ) ;
#9216 = EDGE_LOOP ( 'NONE', ( #84480, #32244 ) ) ;
#9217 = CARTESIAN_POINT ( 'NONE',  ( -43.60637357072565834, 484.6919820420359315, 3.661610076652439094 ) ) ;
#9218 = CARTESIAN_POINT ( 'NONE',  ( 94.49474166934638220, -59.99999999997076117, 21.48900165056691591 ) ) ;
#9219 = ORIENTED_EDGE ( 'NONE', *, *, #77028, .F. ) ;
#9220 = CARTESIAN_POINT ( 'NONE',  ( 7.230429965541936177, -53.39678090435286606, 32.77949809094599232 ) ) ;
#9221 = CARTESIAN_POINT ( 'NONE',  ( -104.6318941305285932, -52.71024081308034681, 158.7339107473082152 ) ) ;
#9222 = CARTESIAN_POINT ( 'NONE',  ( -7.188101187500002709, -15.68750000204838635, 2.977408999572647819 ) ) ;
#9223 = CIRCLE ( 'NONE', #21370, 5.000000000000010658 ) ;
#9224 = ADVANCED_FACE ( 'NONE', ( #32094, #105950, #15356, #96304, #31059, #14817 ), #64972, .T. ) ;
#9225 = FILL_AREA_STYLE ('',( #66959 ) ) ;
#9226 = DIRECTION ( 'NONE',  ( -0.000000000000000000, -0.000000000000000000, 1.000000000000000000 ) ) ;
#9227 = ORIENTED_EDGE ( 'NONE', *, *, #22034, .T. ) ;
#9228 = CARTESIAN_POINT ( 'NONE',  ( -43.47770857297121694, 484.8227827122652229, 4.253339224812703101 ) ) ;
#9229 = COLOUR_RGB ( '', 0.08235294, 0.09019608, 0.10196078) ;
#9230 = CARTESIAN_POINT ( 'NONE',  ( -29.60599819566758129, -60.00000000000002132, 42.84210040572467904 ) ) ;
#9231 = CARTESIAN_POINT ( 'NONE',  ( -3.423905177083978568, -0.8279751000748389878, 103.8439100969757902 ) ) ;
#9232 = CARTESIAN_POINT ( 'NONE',  ( -2.977408999572654480, -20.00000000204838813, 7.188101187499999156 ) ) ;
#9233 = DIRECTION ( 'NONE',  ( -0.5735764363510459374, -0.8191520442889919096, 0.000000000000000000 ) ) ;
#9234 = DIRECTION ( 'NONE',  ( -0.000000000000000000, 1.000000000000000000, -0.000000000000000000 ) ) ;
#9235 = CARTESIAN_POINT ( 'NONE',  ( 15.29459302239697216, 0.000000000000000000, 7.540142361539030169 ) ) ;
#9236 = DIRECTION ( 'NONE',  ( 0.000000000000000000, 1.000000000000000000, 0.000000000000000000 ) ) ;
#9237 = CARTESIAN_POINT ( 'NONE',  ( 32.85560242642285544, 465.7063348014125950, 11.00043030342014028 ) ) ;
#9238 =( BOUNDED_SURFACE ( )  B_SPLINE_SURFACE ( 3, 2, ( 
 ( #79061, #62892, #20358 ),
 ( #95784, #12192, #45123 ),
 ( #28975, #20888, #78519 ),
 ( #53721, #86651, #45643 ),
 ( #37585, #70448, #72552 ),
 ( #39677, #89812, #55810 ),
 ( #90333, #64482, #97351 ),
 ( #31597, #8877, #7805 ),
 ( #8344, #105457, #82231 ),
 ( #98934, #81166, #49867 ),
 ( #16441, #96846, #22974 ),
 ( #23505, #222, #73601 ),
 ( #56885, #82773, #25094 ),
 ( #15912, #47735, #48790 ),
 ( #80634, #98420, #41248 ),
 ( #7276, #49324, #41781 ),
 ( #74137, #81683, #33186 ),
 ( #56349, #15378, #73062 ),
 ( #89284, #97889, #57951 ),
 ( #90875, #40713, #16989 ),
 ( #48265, #40184, #6757 ),
 ( #106505, #105970, #66057 ),
 ( #74663, #32661, #88746 ),
 ( #24572, #32114, #24044 ) ),
 .UNSPECIFIED., .F., .F., .F. ) 
 B_SPLINE_SURFACE_WITH_KNOTS ( ( 4, 2, 2, 2, 2, 2, 2, 2, 2, 2, 2, 4 ),
 ( 3, 3 ),
 ( -4.813857645835639687E-17, 0.0008230535544303435634, 0.001646107108860735265, 0.002469160663291127076, 0.003292214217721518670, 0.004115267772151910697, 0.004938321326582301857, 0.006584428435443085911, 0.008230535544303869966, 0.009876642653164652286, 0.01152274976202543634, 0.01316885687088622039 ),
 ( 0.000000000000000000, 1.000000000000000000 ),
 .UNSPECIFIED. ) 
 GEOMETRIC_REPRESENTATION_ITEM ( )  RATIONAL_B_SPLINE_SURFACE ( (
 ( 1.000000000000000000, 0.9661530732048738690, 1.000000000000000000),
 ( 1.000000000000000000, 0.9666063512417644166, 1.000000000000000000),
 ( 1.000000000000000000, 0.9668885125913321277, 1.000000000000000000),
 ( 1.000000000000000000, 0.9671064463919448739, 1.000000000000000000),
 ( 1.000000000000000000, 0.9670400754974565194, 1.000000000000000000),
 ( 1.000000000000000000, 0.9665156221367009470, 1.000000000000000000),
 ( 1.000000000000000000, 0.9660635237047728863, 1.000000000000000000),
 ( 1.000000000000000000, 0.9647383115599591497, 1.000000000000000000),
 ( 1.000000000000000000, 0.9638533720310250574, 1.000000000000000000),
 ( 1.000000000000000000, 0.9616640248515039291, 1.000000000000000000),
 ( 1.000000000000000000, 0.9603588023342733981, 1.000000000000000000),
 ( 1.000000000000000000, 0.9572958383012356576, 1.000000000000000000),
 ( 1.000000000000000000, 0.9555348605131571693, 1.000000000000000000),
 ( 1.000000000000000000, 0.9497070466053008087, 1.000000000000000000),
 ( 1.000000000000000000, 0.9450513559736188895, 1.000000000000000000),
 ( 1.000000000000000000, 0.9341981514132724485, 1.000000000000000000),
 ( 1.000000000000000000, 0.9281422303525033168, 1.000000000000000000),
 ( 1.000000000000000000, 0.9149199938659065001, 1.000000000000000000),
 ( 1.000000000000000000, 0.9077435111970268977, 1.000000000000000000),
 ( 1.000000000000000000, 0.8923013556734193941, 1.000000000000000000),
 ( 1.000000000000000000, 0.8840358383164468314, 1.000000000000000000),
 ( 1.000000000000000000, 0.8666181798904939448, 1.000000000000000000),
 ( 1.000000000000000000, 0.8574420302237928393, 1.000000000000000000),
 ( 1.000000000000000000, 0.8477912478909354066, 1.000000000000000000) ) ) 
 REPRESENTATION_ITEM ( '' )  SURFACE ( )  );
#9239 = CARTESIAN_POINT ( 'NONE',  ( 6.838568993993028755, -6.773438558311645430, 13.91365169226505927 ) ) ;
#9240 = CARTESIAN_POINT ( 'NONE',  ( -24.41759963816039303, 295.4108152942529841, -1.881177368969137786 ) ) ;
#9241 = CARTESIAN_POINT ( 'NONE',  ( 86.95153870091223780, -59.99999999999995737, -4.620851249272444505 ) ) ;
#9242 = CARTESIAN_POINT ( 'NONE',  ( -31.08105070400566916, -53.38287997746494540, 36.01393495271150869 ) ) ;
#9243 = CARTESIAN_POINT ( 'NONE',  ( -3.215218824033913680, -48.98362140152097766, 104.3206516315225940 ) ) ;
#9244 = CARTESIAN_POINT ( 'NONE',  ( 46.27822564134725525, -36.07043649651712514, 44.25496614335602885 ) ) ;
#9245 = DIRECTION ( 'NONE',  ( 0.000000000000000000, 0.000000000000000000, 1.000000000000000000 ) ) ;
#9246 = ORIENTED_EDGE ( 'NONE', *, *, #73938, .T. ) ;
#9247 = CARTESIAN_POINT ( 'NONE',  ( -7.046289519167721060, 86.30591819944379495, -3.789821819998813623 ) ) ;
#9248 = CARTESIAN_POINT ( 'NONE',  ( -80.07567166459625696, -38.78766219017933992, 193.1244021680591345 ) ) ;
#9249 = VERTEX_POINT ( 'NONE', #47713 ) ;
#9251 = PRESENTATION_STYLE_ASSIGNMENT (( #26040 ) ) ;
#9250 = DIRECTION ( 'NONE',  ( 1.734723475976806108E-16, -1.000000000000000000, 0.000000000000000000 ) ) ;
#9252 = CARTESIAN_POINT ( 'NONE',  ( 42.70433196527829978, -60.00000000000005684, 46.14154939129071664 ) ) ;
#9253 = CARTESIAN_POINT ( 'NONE',  ( 16.19972009820076053, 36.53460074923752643, 24.18132016187593081 ) ) ;
#9254 = CARTESIAN_POINT ( 'NONE',  ( 6.692428679880671361, -4.002209756868625234, 6.852332176615682613 ) ) ;
#9255 = CARTESIAN_POINT ( 'NONE',  ( 33.00000000000000000, 463.5362553048592531, 6.739467187734345721 ) ) ;
#9256 = CARTESIAN_POINT ( 'NONE',  ( 0.000000000000000000, 1.502314598737160017E-15, -6.500000000000000000 ) ) ;
#9257 = CARTESIAN_POINT ( 'NONE',  ( 5.981691436642414317, -88.97269099194117814, -0.5384679144502629855 ) ) ;
#9258 = CARTESIAN_POINT ( 'NONE',  ( 16.80257523370087114, 45.55115703057131782, 6.650239426131699716 ) ) ;
#9259 = CARTESIAN_POINT ( 'NONE',  ( 106.2279738410354071, -60.00000000000002842, 117.8309344228806168 ) ) ;
#9260 = B_SPLINE_CURVE_WITH_KNOTS ( 'NONE', 3,
 ( #46402, #4882, #81267, #40292, #64582, #12949 ),
 .UNSPECIFIED., .F., .F.,
 ( 4, 2, 4 ),
 ( 0.000000000000000000, 0.0003491763592121701330, 0.0006983527184243402660 ),
 .UNSPECIFIED. ) ;
#9261 = B_SPLINE_CURVE_WITH_KNOTS ( 'NONE', 3,
 ( #83279, #42823, #18578, #41755, #76246, #91907, #59555, #34770 ),
 .UNSPECIFIED., .F., .F.,
 ( 4, 2, 2, 4 ),
 ( 0.000000000000000000, 0.2500000000000000000, 0.5000000000000000000, 1.000000000000000000 ),
 .UNSPECIFIED. ) ;
#9262 = DIRECTION ( 'NONE',  ( -1.000000000000000000, -1.224606353822377258E-16, -0.000000000000000000 ) ) ;
#9263 = CARTESIAN_POINT ( 'NONE',  ( 30.59999999999999787, 1.533819458162526451E-15, 0.000000000000000000 ) ) ;
#9264 = ORIENTED_EDGE ( 'NONE', *, *, #36499, .T. ) ;
#9265 = EDGE_CURVE ( 'NONE', #66067, #59308, #10419, .T. ) ;
#9266 = VECTOR ( 'NONE', #31864, 1000.000000000000000 ) ;
#9267 = CARTESIAN_POINT ( 'NONE',  ( -101.1191644727027352, -29.99999999999999289, 171.1750318645146649 ) ) ;
#9268 = ORIENTED_EDGE ( 'NONE', *, *, #102948, .T. ) ;
#9269 = CARTESIAN_POINT ( 'NONE',  ( 26.94613272717667485, 36.94238820718163652, -7.556984339686274588 ) ) ;
#9270 = CARTESIAN_POINT ( 'NONE',  ( 0.000000000000000000, 0.000000000000000000, 0.000000000000000000 ) ) ;
#9271 = FACE_OUTER_BOUND ( 'NONE', #21002, .T. ) ;
#9272 = CARTESIAN_POINT ( 'NONE',  ( 9.918579450955565591, 26.20696087031312160, 1.297207292923859834 ) ) ;
#9273 = AXIS2_PLACEMENT_3D ( 'NONE', #57695, #74420, #42060 ) ;
#9274 = CARTESIAN_POINT ( 'NONE',  ( 7.188101187500000044, -16.53125000204838813, 0.000000000000000000 ) ) ;
#9275 = ADVANCED_FACE ( 'NONE', ( #82749 ), #2667, .T. ) ;
#9276 = EDGE_CURVE ( 'NONE', #69972, #62753, #81880, .T. ) ;
#9278 = B_SPLINE_CURVE_WITH_KNOTS ( 'NONE', 3,
 ( #74182, #82280, #98460, #26228, #41295 ),
 .UNSPECIFIED., .F., .F.,
 ( 4, 1, 4 ),
 ( 0.000000000000000000, 0.003752776749732572668, 0.007505553499465145335 ),
 .UNSPECIFIED. ) ;
#9277 = CARTESIAN_POINT ( 'NONE',  ( 29.68315524076925982, 18.29184282782464166, -39.60535821593530414 ) ) ;
#9279 = VERTEX_POINT ( 'NONE', #60105 ) ;
#9280 = CARTESIAN_POINT ( 'NONE',  ( 83.03340579700397939, -32.54870090252141779, 159.1926985072703928 ) ) ;
#9281 = CARTESIAN_POINT ( 'NONE',  ( -50.91589357081878120, 38.95383793066859113, 39.12903940707597883 ) ) ;
#9282 = PRESENTATION_STYLE_ASSIGNMENT (( #58924 ) ) ;
#9283 = ORIENTED_EDGE ( 'NONE', *, *, #1210, .T. ) ;
#9284 = ADVANCED_FACE ( 'NONE', ( #68163 ), #7828, .F. ) ;
#9285 = CARTESIAN_POINT ( 'NONE',  ( 10.00000000000000000, 0.000000000000000000, 10.00000000000000178 ) ) ;
#9286 = CARTESIAN_POINT ( 'NONE',  ( -16.75187969033532553, -1.200000000000000030E-05, 21.80698433968612093 ) ) ;
#9287 = CARTESIAN_POINT ( 'NONE',  ( 10.45249458729220571, 46.08328249563464141, 12.90779740156148847 ) ) ;
#9288 = EDGE_LOOP ( 'NONE', ( #60258, #100269 ) ) ;
#9289 = STYLED_ITEM ( 'NONE', ( #94566 ), #61420 ) ;
#9290 = B_SPLINE_CURVE_WITH_KNOTS ( 'NONE', 3,
 ( #77429, #93077, #102765, #21347 ),
 .UNSPECIFIED., .F., .F.,
 ( 4, 4 ),
 ( 3.469446951953614189E-18, 0.002190562081053277436 ),
 .UNSPECIFIED. ) ;
#9291 = UNCERTAINTY_MEASURE_WITH_UNIT (LENGTH_MEASURE( 1.000000000000000082E-05 ), #43931, 'distance_accuracy_value', 'NONE');
#9292 = CARTESIAN_POINT ( 'NONE',  ( 45.94900261086841198, -5.000000000000000888, 6.123233995736769241E-16 ) ) ;
#9293 = CARTESIAN_POINT ( 'NONE',  ( -5.000000000000000888, -67.36501624949291056, 11.52273887431363697 ) ) ;
#9294 = CARTESIAN_POINT ( 'NONE',  ( 14.88745091283334077, 23.11123547206230811, 0.5085106042973103202 ) ) ;
#9295 = DIRECTION ( 'NONE',  ( 1.000000000000000000, 1.224606353822377258E-16, 0.000000000000000000 ) ) ;
#9296 = CARTESIAN_POINT ( 'NONE',  ( 7.188101187500001821, -32.56250000204838813, -2.977408999572650483 ) ) ;
#9297 = LINE ( 'NONE', #33612, #90499 ) ;
#9298 = AXIS2_PLACEMENT_3D ( 'NONE', #38170, #79644, #39734 ) ;
#9299 = CARTESIAN_POINT ( 'NONE',  ( 8.000000000000000000, 0.000000000000000000, -25.03750572909317285 ) ) ;
#9300 = CARTESIAN_POINT ( 'NONE',  ( 38.28801327779752484, 438.9528884713969319, 23.36340610710418986 ) ) ;
#9301 = COLOUR_RGB ( '', 0.40784314, 0.44705882, 0.49803922) ;
#9302 = CARTESIAN_POINT ( 'NONE',  ( 49.13582233779577280, 7.783546568855205017, 16.18978396958228672 ) ) ;
#9303 = ORIENTED_EDGE ( 'NONE', *, *, #27591, .F. ) ;
#9304 = CARTESIAN_POINT ( 'NONE',  ( 0.3342801499821536626, 44.06880204852024718, 16.29260926128794651 ) ) ;
#9305 = FILL_AREA_STYLE ('',( #83209 ) ) ;
#9306 = CARTESIAN_POINT ( 'NONE',  ( -9.993183759207806105, 7.509940706527443943, 0.000000000000000000 ) ) ;
#9307 = ORIENTED_EDGE ( 'NONE', *, *, #91001, .F. ) ;
#9308 = CARTESIAN_POINT ( 'NONE',  ( 0.000000000000000000, 35.00000000000000000, 0.000000000000000000 ) ) ;
#9309 = DIRECTION ( 'NONE',  ( 0.000000000000000000, 0.000000000000000000, 1.000000000000000000 ) ) ;
#9310 = CARTESIAN_POINT ( 'NONE',  ( 107.5610214307659476, -57.67122956308984527, 113.7628399357034397 ) ) ;
#9311 = EDGE_CURVE ( 'NONE', #53673, #7244, #79963, .T. ) ;
#9312 = CARTESIAN_POINT ( 'NONE',  ( 32.82923647385615595, 434.9827616338783400, 12.60812312004859237 ) ) ;
#9313 = CARTESIAN_POINT ( 'NONE',  ( 3.972742726731588458, 17.31622427227530636, 5.763799860841350764 ) ) ;
#9314 = CARTESIAN_POINT ( 'NONE',  ( -2.499999999999999556, -8.000000000000000000, 17.89626171146327493 ) ) ;
#9315 = SURFACE_STYLE_USAGE ( .BOTH. , #17450 ) ;
#9316 = CARTESIAN_POINT ( 'NONE',  ( -82.35766411969579792, -59.99999999999999289, 198.3413902865526381 ) ) ;
#9317 = CARTESIAN_POINT ( 'NONE',  ( 9.083636026015101450, 43.76992373826562499, -14.50792011570289830 ) ) ;
#9318 = CARTESIAN_POINT ( 'NONE',  ( 44.83349330513380693, 4.898587196589405926E-16, -4.000000000000001776 ) ) ;
#9319 = CARTESIAN_POINT ( 'NONE',  ( -43.74855578046756222, 328.6220886837048170, -1.765109843966993441 ) ) ;
#9320 = CARTESIAN_POINT ( 'NONE',  ( -82.59538156006668430, -60.84729630826085867, 189.6675515197301252 ) ) ;
#9322 = ORIENTED_EDGE ( 'NONE', *, *, #59087, .F. ) ;
#9321 = VECTOR ( 'NONE', #84543, 1000.000000000000000 ) ;
#9323 = ORIENTED_EDGE ( 'NONE', *, *, #97404, .T. ) ;
#9325 = EDGE_CURVE ( 'NONE', #30487, #10693, #78, .T. ) ;
#9324 = CARTESIAN_POINT ( 'NONE',  ( 45.59999999999999432, -3.309499999999999886, 4.475777889183790779E-16 ) ) ;
#9326 = MECHANICAL_DESIGN_GEOMETRIC_PRESENTATION_REPRESENTATION (  '', ( #763 ), #5955 ) ;
#9327 = PRESENTATION_LAYER_ASSIGNMENT (  '', '', ( #52453 ) ) ;
#9328 = CARTESIAN_POINT ( 'NONE',  ( -85.75585748537427833, -52.73827868327173007, -6.687191420894485816 ) ) ;
#9329 = CYLINDRICAL_SURFACE ( 'NONE', #63293, 4.000000000000000000 ) ;
#9330 = CARTESIAN_POINT ( 'NONE',  ( -15.66802374774660045, 43.86792895834400952, 6.193618902369640189 ) ) ;
#9331 = CARTESIAN_POINT ( 'NONE',  ( -13.85357083679006251, -8.697779628897517767, 12.23407158846710985 ) ) ;
#9332 = CARTESIAN_POINT ( 'NONE',  ( 6.463344223170839342, 4.601472318010338292, -5.710032555828796319 ) ) ;
#9333 = CARTESIAN_POINT ( 'NONE',  ( 45.60838156035057978, 42.00000000000004263, -79.13121736032620390 ) ) ;
#9334 = CARTESIAN_POINT ( 'NONE',  ( 69.67238219402268840, 4.000000000000013323, 0.000000000000000000 ) ) ;
#9335 = CARTESIAN_POINT ( 'NONE',  ( 37.62958953315902022, -14.21045842199429288, 41.24408864243086015 ) ) ;
#9336 = CARTESIAN_POINT ( 'NONE',  ( -35.50215413661368302, 437.6258544849081886, 4.714593920598203702 ) ) ;
#9337 = CARTESIAN_POINT ( 'NONE',  ( -59.37491258674359784, -59.99999999999998579, -38.24906085379748788 ) ) ;
#9338 = CARTESIAN_POINT ( 'NONE',  ( -66.84523826069663244, -46.43835352555290541, 95.56956660544847182 ) ) ;
#9339 = ORIENTED_EDGE ( 'NONE', *, *, #18724, .T. ) ;
#9340 = CARTESIAN_POINT ( 'NONE',  ( 70.38659604113041723, -14.21045842199445808, 117.5484250040930050 ) ) ;
#9341 = SURFACE_STYLE_FILL_AREA ( #24525 ) ;
#9342 = CARTESIAN_POINT ( 'NONE',  ( 94.71150925245034102, -57.65915928951965697, -7.875939490799622966 ) ) ;
#9343 = ORIENTED_EDGE ( 'NONE', *, *, #64885, .T. ) ;
#9344 = CARTESIAN_POINT ( 'NONE',  ( 15.61654987365426983, -4.700132877332916514, 14.24804686413672528 ) ) ;
#9345 = EDGE_CURVE ( 'NONE', #65882, #94111, #37430, .T. ) ;
#9346 = FACE_BOUND ( 'NONE', #101062, .T. ) ;
#9347 = ORIENTED_EDGE ( 'NONE', *, *, #12253, .T. ) ;
#9348 = CARTESIAN_POINT ( 'NONE',  ( 80.40000000000000568, 1.023464760207051730E-14, 0.000000000000000000 ) ) ;
#9349 = DIRECTION ( 'NONE',  ( 0.000000000000000000, 0.000000000000000000, -1.000000000000000000 ) ) ;
#9350 = DIRECTION ( 'NONE',  ( -1.000000000000000000, 0.000000000000000000, 0.000000000000000000 ) ) ;
#9351 = CARTESIAN_POINT ( 'NONE',  ( 5.082755093536324154, -13.34375000204838457, 5.082755093536326818 ) ) ;
#9352 = DIRECTION ( 'NONE',  ( -0.000000000000000000, -0.000000000000000000, -1.000000000000000000 ) ) ;
#9353 = DIRECTION ( 'NONE',  ( 0.000000000000000000, 0.000000000000000000, -1.000000000000000000 ) ) ;
#9354 = CARTESIAN_POINT ( 'NONE',  ( 43.97709758272655733, 485.9234630640622186, 4.765357663000028943 ) ) ;
#9355 = DIRECTION ( 'NONE',  ( 1.150791560227848297E-16, -0.3420201433256725987, 0.9396926207859068736 ) ) ;
#9356 = CARTESIAN_POINT ( 'NONE',  ( 28.09999999999999787, 1.533819458162526451E-15, 0.000000000000000000 ) ) ;
#9357 = CARTESIAN_POINT ( 'NONE',  ( 0.000000000000000000, 60.00000000000000000, 6.999999999999992895 ) ) ;
#9358 = CIRCLE ( 'NONE', #100609, 5.000000000000002665 ) ;
#9359 = EDGE_LOOP ( 'NONE', ( #15153, #33270, #6637, #13882, #35722 ) ) ;
#9360 = CARTESIAN_POINT ( 'NONE',  ( -7.398496323958707599, 40.00000000002496137, -70.41867143398266649 ) ) ;
#9361 = CARTESIAN_POINT ( 'NONE',  ( 31.57827475542996609, -32.54814147035259708, 32.45590311695885788 ) ) ;
#9362 = CARTESIAN_POINT ( 'NONE',  ( 29.77392050318139383, 311.5487359906569509, -7.436788483390921023 ) ) ;
#9363 = VERTEX_POINT ( 'NONE', #4493 ) ;
#9364 = PLANE ( 'NONE',  #42669 ) ;
#9365 =( GEOMETRIC_REPRESENTATION_CONTEXT ( 3 ) GLOBAL_UNCERTAINTY_ASSIGNED_CONTEXT ( ( #101586 ) ) GLOBAL_UNIT_ASSIGNED_CONTEXT ( ( #85448, #77353, #12072 ) ) REPRESENTATION_CONTEXT ( 'NONE', 'WORKASPACE' ) );
#9366 = VERTEX_POINT ( 'NONE', #70296 ) ;
#9367 = DIRECTION ( 'NONE',  ( 0.000000000000000000, -1.000000000000000000, 0.000000000000000000 ) ) ;
#9368 = CARTESIAN_POINT ( 'NONE',  ( 0.5805565836007701153, -7.505553499465148271, -1.383738442504732931E-16 ) ) ;
#9369 = CARTESIAN_POINT ( 'NONE',  ( -17.66251776275359475, 294.6000992765483488, -10.05350143900042781 ) ) ;
#9370 = AXIS2_PLACEMENT_3D ( 'NONE', #103702, #46009, #4480 ) ;
#9371 = CIRCLE ( 'NONE', #5992, 3.309500000000001663 ) ;
#9372 = CARTESIAN_POINT ( 'NONE',  ( 0.000000000000000000, -4.000000000000003553, 27.00000000000000000 ) ) ;
#9373 = AXIS2_PLACEMENT_3D ( 'NONE', #76479, #83510, #19374 ) ;
#9374 = CARTESIAN_POINT ( 'NONE',  ( 0.7722239243178034007, 18.23336398057940499, -49.51275493678145523 ) ) ;
#9375 = ORIENTED_EDGE ( 'NONE', *, *, #93605, .F. ) ;
#9376 = CARTESIAN_POINT ( 'NONE',  ( 81.07743897483196349, -60.00000000000000711, -27.28973066995784436 ) ) ;
#9377 = CARTESIAN_POINT ( 'NONE',  ( 23.05228496585736053, 26.02496755577630694, -30.70617127781075695 ) ) ;
#9378 = AXIS2_PLACEMENT_3D ( 'NONE', #101982, #61018, #76641 ) ;
#9379 = CARTESIAN_POINT ( 'NONE',  ( -47.57405721301101664, 17.76112721455490373, -14.43871205879859687 ) ) ;
#9380 = VERTEX_POINT ( 'NONE', #70824 ) ;
#9381 = DIRECTION ( 'NONE',  ( 0.000000000000000000, 1.000000000000000000, 0.000000000000000000 ) ) ;
#9382 = EDGE_LOOP ( 'NONE', ( #101256, #63652, #3205, #91433 ) ) ;
#9383 = VERTEX_POINT ( 'NONE', #102659 ) ;
#9384 = CARTESIAN_POINT ( 'NONE',  ( -1.469576158976823947E-15, -11.37499999999999289, 8.000000000000000000 ) ) ;
#9385 = DIRECTION ( 'NONE',  ( 0.000000000000000000, 0.000000000000000000, 1.000000000000000000 ) ) ;
#9386 = CARTESIAN_POINT ( 'NONE',  ( 0.000000000000000000, 4.898587196589413815E-16, -4.000000000000000888 ) ) ;
#9387 = CYLINDRICAL_SURFACE ( 'NONE', #19077, 7.000000000000000000 ) ;
#9388 = CARTESIAN_POINT ( 'NONE',  ( 84.49172617919205663, -45.28678258021372471, -6.204812034688317546 ) ) ;
#9389 = CARTESIAN_POINT ( 'NONE',  ( -36.12596508061012202, 304.2006385358498051, 0.1548427460391987032 ) ) ;
#9390 = DIRECTION ( 'NONE',  ( 0.6505632072693934287, 0.6639782930160490482, 0.3686466326319202125 ) ) ;
#9391 = CARTESIAN_POINT ( 'NONE',  ( 12.50000000000000533, 24.98774108567306840, -42.39486677989071950 ) ) ;
#9392 = VERTEX_POINT ( 'NONE', #44971 ) ;
#9393 =( BOUNDED_SURFACE ( )  B_SPLINE_SURFACE ( 3, 2, ( 
 ( #56755, #63822, #23372 ),
 ( #72425, #80501, #79455 ),
 ( #39012, #64355, #104795 ),
 ( #97223, #22319, #6622 ),
 ( #39549, #105329, #7669 ),
 ( #14705, #31472, #72938 ),
 ( #89682, #22848, #15249 ),
 ( #15780, #48136, #40588 ),
 ( #81033, #48662, #7149 ),
 ( #79976, #71356, #106365 ),
 ( #40061, #81547, #5566 ),
 ( #104256, #32530, #30402 ),
 ( #57283, #63289, #96189 ),
 ( #96712, #55164, #30945 ),
 ( #88093, #47077, #55682 ),
 ( #93795, #52254, #28557 ),
 ( #26964, #77610, #84639 ),
 ( #3186, #68999, #92718 ),
 ( #85167, #59849, #44182 ),
 ( #76002, #90741, #18879 ),
 ( #16857, #49737, #19421 ),
 ( #43640, #98809, #11253 ),
 ( #76529, #61441, #94333 ),
 ( #8746, #101875, #35052 ),
 ( #51722, #28034, #10724 ),
 ( #2639, #93259, #82646 ),
 ( #77071, #57818, #35585 ),
 ( #102414, #68461, #36132 ),
 ( #27507, #24963, #43114 ),
 ( #49197, #101353, #60383 ),
 ( #2100, #60906, #67918 ),
 ( #19952, #52793, #85717 ),
 ( #100805, #41125, #11791 ),
 ( #44722, #3728, #82097 ),
 ( #36658, #8216, #69522 ),
 ( #74009, #91, #33060 ),
 ( #65930, #37722, #14438 ),
 ( #30140, #5830, #95921 ) ),
 .UNSPECIFIED., .F., .F., .F. ) 
 B_SPLINE_SURFACE_WITH_KNOTS ( ( 4, 2, 2, 2, 2, 2, 2, 2, 2, 2, 2, 2, 2, 2, 2, 2, 2, 2, 4 ),
 ( 3, 3 ),
 ( 0.06375477930561529449, 0.06591736287010073470, 0.06807994643458617490, 0.07240511356355705530, 0.07673028069252793570, 0.08105544782149880223, 0.08970578207944054916, 0.09835611633738230997, 0.1156567848532658177, 0.1329574533691493254, 0.1502581218850328193, 0.1675587904009163132, 0.1762091246588580740, 0.1848594589167998348, 0.1891846260457707152, 0.1935097931747415956, 0.1978349603037124482, 0.1999975438681979023, 0.2021601274326833286 ),
 ( 0.000000000000000000, 1.000000000000000000 ),
 .UNSPECIFIED. ) 
 GEOMETRIC_REPRESENTATION_ITEM ( )  RATIONAL_B_SPLINE_SURFACE ( (
 ( 1.000000000000000000, 0.7071067811865475727, 1.000000000000000000),
 ( 1.000000000000000000, 0.7071067811865475727, 1.000000000000000000),
 ( 1.000000000000000000, 0.7071067811865474617, 1.000000000000000000),
 ( 1.000000000000000000, 0.7071067811865474617, 1.000000000000000000),
 ( 1.000000000000000000, 0.7071067811865475727, 1.000000000000000000),
 ( 1.000000000000000000, 0.7071067811865475727, 1.000000000000000000),
 ( 1.000000000000000000, 0.7071067811865475727, 1.000000000000000000),
 ( 1.000000000000000000, 0.7071067811865475727, 1.000000000000000000),
 ( 1.000000000000000000, 0.7071067811865475727, 1.000000000000000000),
 ( 1.000000000000000000, 0.7071067811865475727, 1.000000000000000000),
 ( 1.000000000000000000, 0.7071067811865474617, 1.000000000000000000),
 ( 1.000000000000000000, 0.7071067811865474617, 1.000000000000000000),
 ( 1.000000000000000000, 0.7071067811865475727, 1.000000000000000000),
 ( 1.000000000000000000, 0.7071067811865475727, 1.000000000000000000),
 ( 1.000000000000000000, 0.7071067811865475727, 1.000000000000000000),
 ( 1.000000000000000000, 0.7071067811865475727, 1.000000000000000000),
 ( 1.000000000000000000, 0.7071067811865475727, 1.000000000000000000),
 ( 1.000000000000000000, 0.7071067811865475727, 1.000000000000000000),
 ( 1.000000000000000000, 0.7071067811865475727, 1.000000000000000000),
 ( 1.000000000000000000, 0.7071067811865475727, 1.000000000000000000),
 ( 1.000000000000000000, 0.7071067811865475727, 1.000000000000000000),
 ( 1.000000000000000000, 0.7071067811865475727, 1.000000000000000000),
 ( 1.000000000000000000, 0.7071067811865475727, 1.000000000000000000),
 ( 1.000000000000000000, 0.7071067811865475727, 1.000000000000000000),
 ( 1.000000000000000000, 0.7071067811865475727, 1.000000000000000000),
 ( 1.000000000000000000, 0.7071067811865475727, 1.000000000000000000),
 ( 1.000000000000000000, 0.7071067811865475727, 1.000000000000000000),
 ( 1.000000000000000000, 0.7071067811865475727, 1.000000000000000000),
 ( 1.000000000000000000, 0.7071067811865474617, 1.000000000000000000),
 ( 1.000000000000000000, 0.7071067811865474617, 1.000000000000000000),
 ( 1.000000000000000000, 0.7071067811865474617, 1.000000000000000000),
 ( 1.000000000000000000, 0.7071067811865474617, 1.000000000000000000),
 ( 1.000000000000000000, 0.7071067811865475727, 1.000000000000000000),
 ( 1.000000000000000000, 0.7071067811865475727, 1.000000000000000000),
 ( 1.000000000000000000, 0.7071067811865474617, 1.000000000000000000),
 ( 1.000000000000000000, 0.7071067811865474617, 1.000000000000000000),
 ( 1.000000000000000000, 0.7071067811865475727, 1.000000000000000000),
 ( 1.000000000000000000, 0.7071067811865475727, 1.000000000000000000) ) ) 
 REPRESENTATION_ITEM ( '' )  SURFACE ( )  );
#9394 = DIRECTION ( 'NONE',  ( -0.000000000000000000, -0.000000000000000000, -1.000000000000000000 ) ) ;
#9395 = EDGE_CURVE ( 'NONE', #70791, #9016, #95696, .T. ) ;
#9396 = VERTEX_POINT ( 'NONE', #35836 ) ;
#9397 = CARTESIAN_POINT ( 'NONE',  ( 9.781924074846555683, 51.26649690293741912, -3.092456821203221740 ) ) ;
#9399 = ORIENTED_EDGE ( 'NONE', *, *, #86875, .F. ) ;
#9398 = CARTESIAN_POINT ( 'NONE',  ( 55.00571552735602410, 6.975173280561618775E-15, 0.000000000000000000 ) ) ;
#9400 = CARTESIAN_POINT ( 'NONE',  ( 75.39868036955950004, -36.01852124489236218, 119.8304219598088309 ) ) ;
#9401 = ORIENTED_EDGE ( 'NONE', *, *, #75895, .F. ) ;
#9402 = CARTESIAN_POINT ( 'NONE',  ( 63.67138272020815037, 38.95383793066860534, -8.334564508068659450 ) ) ;
#9403 = EDGE_CURVE ( 'NONE', #105843, #72225, #88944, .T. ) ;
#9404 = CARTESIAN_POINT ( 'NONE',  ( -7.188101187500000044, -27.40625000204838813, -8.802885111219163269E-16 ) ) ;
#9405 = CIRCLE ( 'NONE', #69717, 4.000000000000001776 ) ;
#9406 = EDGE_CURVE ( 'NONE', #37873, #93842, #74802, .T. ) ;
#9407 = CARTESIAN_POINT ( 'NONE',  ( -94.30414684669057124, -57.67279326051714605, 1.132156541063573441 ) ) ;
#9408 = CARTESIAN_POINT ( 'NONE',  ( 24.31833665363000918, 25.57798547635034581, 31.28409169986229443 ) ) ;
#9409 = EDGE_LOOP ( 'NONE', ( #55011, #34874, #87903, #31229 ) ) ;
#9410 = B_SPLINE_CURVE_WITH_KNOTS ( 'NONE', 3,
 ( #58302, #59388, #42114, #1093, #75548, #100351, #67996, #43190 ),
 .UNSPECIFIED., .F., .F.,
 ( 4, 2, 2, 4 ),
 ( 2.862293735361731706E-17, 0.002162274530409172366, 0.003243411795613744888, 0.004324549060818317844 ),
 .UNSPECIFIED. ) ;
#9411 = DIRECTION ( 'NONE',  ( -0.000000000000000000, -0.000000000000000000, -1.000000000000000000 ) ) ;
#9412 = CARTESIAN_POINT ( 'NONE',  ( 106.2181247233446300, -60.15136654602780197, 163.5236569256875043 ) ) ;
#9413 = CARTESIAN_POINT ( 'NONE',  ( -36.56974102123706416, 28.18271022055501263, -11.43420612882628618 ) ) ;
#9414 = DIRECTION ( 'NONE',  ( 0.000000000000000000, -1.000000000000000000, 0.000000000000000000 ) ) ;
#9415 = CARTESIAN_POINT ( 'NONE',  ( 8.000000000000000000, -23.09375000409676915, -3.313708498984761608 ) ) ;
#9416 = DIRECTION ( 'NONE',  ( 0.000000000000000000, -1.000000000000000000, 0.000000000000000000 ) ) ;
#9417 = CARTESIAN_POINT ( 'NONE',  ( 14.29190075645217028, 19.61368180395370331, 4.501023549821925762 ) ) ;
#9418 = CARTESIAN_POINT ( 'NONE',  ( 33.00000000000000000, 450.0000000000002274, 13.20242257375370976 ) ) ;
#9419 = CARTESIAN_POINT ( 'NONE',  ( 6.849999999999999645, -4.618802153516998743, 7.999999999999998224 ) ) ;
#9420 = B_SPLINE_CURVE_WITH_KNOTS ( 'NONE', 3,
 ( #53048, #84352, #10445, #76244, #27754, #52496, #92421, #68162, #69243, #43359, #36897, #102116, #51965, #102658, #76776, #100521, #11499, #2352, #28273, #44425, #85415, #20737 ),
 .UNSPECIFIED., .F., .F.,
 ( 4, 2, 2, 2, 2, 2, 2, 2, 2, 2, 4 ),
 ( 0.003020842387534908389, 0.003273441169516790126, 0.003526039951498671863, 0.003778638733480553600, 0.004031237515462435771, 0.004536435079426195775, 0.005041632643389954913, 0.005546830207353714917, 0.006052027771317474922, 0.006557225335281234926, 0.007062422899244994931 ),
 .UNSPECIFIED. ) ;
#9421 = CARTESIAN_POINT ( 'NONE',  ( -12.19423397773156736, 304.5852035401753710, 9.880331998383338643 ) ) ;
#9422 = CARTESIAN_POINT ( 'NONE',  ( 69.88291765283146617, 258.1183258647171215, 182.1969486012846460 ) ) ;
#9423 = CARTESIAN_POINT ( 'NONE',  ( -1.404490565848831141, 15.46725112412266512, -9.926810856659471938 ) ) ;
#9424 = ORIENTED_EDGE ( 'NONE', *, *, #52022, .T. ) ;
#9425 = DIRECTION ( 'NONE',  ( 0.000000000000000000, -1.000000000000000000, 0.000000000000000000 ) ) ;
#9426 = DIRECTION ( 'NONE',  ( 0.000000000000000000, 0.000000000000000000, -1.000000000000000000 ) ) ;
#9427 = DIRECTION ( 'NONE',  ( 1.000000000000000000, 0.000000000000000000, 0.000000000000000000 ) ) ;
#9428 = CARTESIAN_POINT ( 'NONE',  ( -90.03084723851439719, -30.00000000000000000, 189.8964335926784770 ) ) ;
#9429 = VECTOR ( 'NONE', #95370, 1000.000000000000000 ) ;
#9430 = ORIENTED_EDGE ( 'NONE', *, *, #92820, .T. ) ;
#9431 = CARTESIAN_POINT ( 'NONE',  ( 4.855129149332425342, -47.10165964154809615, 42.75273515042984229 ) ) ;
#9432 = CARTESIAN_POINT ( 'NONE',  ( 71.49051955128589952, -57.67963396668447729, 166.9361842711434747 ) ) ;
#9434 = CARTESIAN_POINT ( 'NONE',  ( -96.81748461682487061, -38.00000000001091394, 192.8978395531862020 ) ) ;
#9433 = SURFACE_STYLE_USAGE ( .BOTH. , #100059 ) ;
#9435 = ADVANCED_FACE ( 'NONE', ( #103194 ), #103715, .T. ) ;
#9436 = CARTESIAN_POINT ( 'NONE',  ( 19.07582147746917300, -25.49993130453409407, -38.49573148241584164 ) ) ;
#9437 = CARTESIAN_POINT ( 'NONE',  ( -1.011134924304563754, 43.89348651028122816, 16.74734961794866095 ) ) ;
#9438 = CIRCLE ( 'NONE', #12906, 0.9999999999999967804 ) ;
#9439 = CARTESIAN_POINT ( 'NONE',  ( -43.02621584241282449, 434.6128289108255558, 16.97888786059002086 ) ) ;
#9440 = CARTESIAN_POINT ( 'NONE',  ( -41.05948510805755802, -59.99999999999999289, 53.66256863961316981 ) ) ;
#9441 = VECTOR ( 'NONE', #17095, 1000.000000000000000 ) ;
#9442 = AXIS2_PLACEMENT_3D ( 'NONE', #53530, #54564, #36853 ) ;
#9443 =( REPRESENTATION_RELATIONSHIP ('NONE','NONE', #69581, #103287 ) REPRESENTATION_RELATIONSHIP_WITH_TRANSFORMATION ( #4415 )SHAPE_REPRESENTATION_RELATIONSHIP( ) );
#9444 = AXIS2_PLACEMENT_3D ( 'NONE', #101680, #2970, #93594 ) ;
#9445 = DIRECTION ( 'NONE',  ( 0.000000000000000000, -0.1492727218618817575, -0.9887960631535429590 ) ) ;
#9446 = DIRECTION ( 'NONE',  ( 0.000000000000000000, -0.9221233147934838614, -0.3868961001538753219 ) ) ;
#9447 = B_SPLINE_CURVE_WITH_KNOTS ( 'NONE', 3,
 ( #85399, #53029, #3419, #43867, #99973, #83783, #76759, #85952, #67090, #51421, #18014, #9896, #67626, #93501, #19648, #35820, #42804, #34753, #12023, #52481, #68701, #10428, #44955, #68146, #28258, #11482, #44410, #1248, #43344, #101040 ),
 .UNSPECIFIED., .F., .F.,
 ( 4, 2, 2, 2, 2, 2, 2, 2, 2, 2, 2, 2, 2, 2, 4 ),
 ( 0.01036701337735790318, 0.01128271447499395834, 0.01219841557263001523, 0.01311411667026607039, 0.01357196721908409884, 0.01402981776790212555, 0.01448766831672015400, 0.01471659359112916995, 0.01494551886553818418, 0.01517444413994720187, 0.01540336941435621609, 0.01586121996317423760, 0.01631907051199225911, 0.01677692106081028062, 0.01769262215844630975 ),
 .UNSPECIFIED. ) ;
#9448 = VECTOR ( 'NONE', #38726, 1000.000000000000000 ) ;
#9449 = CARTESIAN_POINT ( 'NONE',  ( -86.45611204286437612, -17.05227200858531234, 183.4756348703512572 ) ) ;
#9450 = ORIENTED_EDGE ( 'NONE', *, *, #94664, .F. ) ;
#9451 = CARTESIAN_POINT ( 'NONE',  ( 26.69900261086841198, 1.482358050883964840E-15, 0.000000000000000000 ) ) ;
#9452 = CARTESIAN_POINT ( 'NONE',  ( -6.099882006367853826, -39.47594237312841869, 30.45917207147936168 ) ) ;
#9453 = AXIS2_PLACEMENT_3D ( 'NONE', #83985, #58660, #9019 ) ;
#9454 = CARTESIAN_POINT ( 'NONE',  ( 84.73333333333332007, -4.171999999999998820, 5.616230220889773285E-16 ) ) ;
#9455 = CARTESIAN_POINT ( 'NONE',  ( 86.23711656224473643, -45.40185197806301431, 189.5298877258528023 ) ) ;
#9458 = ADVANCED_FACE ( 'NONE', ( #69765 ), #24799, .F. ) ;
#9457 = CARTESIAN_POINT ( 'NONE',  ( 6.125000001138555028, -61.81780766021304885, 14.41094225185805477 ) ) ;
#9456 = CARTESIAN_POINT ( 'NONE',  ( -34.62641242406925812, 302.5981200378967060, 3.709061959311505063 ) ) ;
#9459 = EDGE_CURVE ( 'NONE', #22473, #92048, #14682, .T. ) ;
#9460 = ORIENTED_EDGE ( 'NONE', *, *, #101734, .T. ) ;
#9461 = CARTESIAN_POINT ( 'NONE',  ( 30.59999999999999787, 1.533819458162526451E-15, 0.000000000000000000 ) ) ;
#9462 = CARTESIAN_POINT ( 'NONE',  ( -5.314078508931081579, -5.000000000000359712, -15.45392136113532366 ) ) ;
#9463 = CARTESIAN_POINT ( 'NONE',  ( -7.551437640244099470, 33.00872462522908535, -2.648272645923380519 ) ) ;
#9464 = CARTESIAN_POINT ( 'NONE',  ( 33.38386847897551490, 300.5334109687220234, -0.7226634255821527963 ) ) ;
#9465 = FACE_OUTER_BOUND ( 'NONE', #24791, .T. ) ;
#9466 = FILL_AREA_STYLE_COLOUR ( '', #49553 ) ;
#9467 = CARTESIAN_POINT ( 'NONE',  ( 106.5496036037455809, -14.21045842199433373, 161.7522804960935900 ) ) ;
#9468 = CARTESIAN_POINT ( 'NONE',  ( -81.09901249779620969, -49.92721230687652678, 168.6194323894324896 ) ) ;
#9469 = ORIENTED_EDGE ( 'NONE', *, *, #65165, .T. ) ;
#9470 = CARTESIAN_POINT ( 'NONE',  ( 29.98176661990081371, 5.000000000000004441, 6.123233995736770227E-16 ) ) ;
#9471 = CARTESIAN_POINT ( 'NONE',  ( -9.165151389911699198, 249.9999999999999716, -4.000000000000002665 ) ) ;
#9472 = DIRECTION ( 'NONE',  ( 1.000000000000000000, 1.224606353822377258E-16, 0.000000000000000000 ) ) ;
#9473 = CARTESIAN_POINT ( 'NONE',  ( 43.61934421053724975, 427.3517207320185776, 15.28054217563496842 ) ) ;
#9474 = EDGE_CURVE ( 'NONE', #88304, #6711, #64658, .T. ) ;
#9475 = DIRECTION ( 'NONE',  ( 0.000000000000000000, 1.000000000000000000, 0.000000000000000000 ) ) ;
#9476 = EDGE_LOOP ( 'NONE', ( #85383, #97446 ) ) ;
#9477 = UNCERTAINTY_MEASURE_WITH_UNIT (LENGTH_MEASURE( 1.000000000000000082E-05 ), #50185, 'distance_accuracy_value', 'NONE');
#9478 = CARTESIAN_POINT ( 'NONE',  ( -22.84042588457585765, 304.5089447765301998, 10.07913915037610053 ) ) ;
#9479 = ORIENTED_EDGE ( 'NONE', *, *, #76890, .T. ) ;
#9480 = DIRECTION ( 'NONE',  ( 1.000000000000000000, 1.224606353822377258E-16, 0.000000000000000000 ) ) ;
#9481 = VECTOR ( 'NONE', #60677, 1000.000000000000000 ) ;
#9483 = ADVANCED_FACE ( 'NONE', ( #47587 ), #91127, .F. ) ;
#9482 = CARTESIAN_POINT ( 'NONE',  ( 1.404490565848997230, 15.46725112412266512, 9.926810856659436411 ) ) ;
#9484 = CARTESIAN_POINT ( 'NONE',  ( 32.62589942841201207, 485.9514140855832238, 7.203752716018509972 ) ) ;
#9485 = CARTESIAN_POINT ( 'NONE',  ( 23.38163988262877879, 50.00000000002003731, 60.94087333794557537 ) ) ;
#9486 = CARTESIAN_POINT ( 'NONE',  ( 5.000000000000040856, -13.35938963217494724, 12.71467713436114799 ) ) ;
#9487 = CARTESIAN_POINT ( 'NONE',  ( 46.00000000000002842, 436.0961602813633249, 11.28239370168154032 ) ) ;
#9488 = VERTEX_POINT ( 'NONE', #50763 ) ;
#9489 = CARTESIAN_POINT ( 'NONE',  ( 112.2483500844232651, -60.00000000000000000, 174.7240955042347821 ) ) ;
#9491 = CARTESIAN_POINT ( 'NONE',  ( 16.50575907406394549, -25.54973315577406723, 28.36482997719511445 ) ) ;
#9490 = CARTESIAN_POINT ( 'NONE',  ( -96.06797501213969781, -14.21045842199444564, 198.0637310406154938 ) ) ;
#9492 = EDGE_CURVE ( 'NONE', #4508, #74667, #99318, .T. ) ;
#9493 = CARTESIAN_POINT ( 'NONE',  ( 36.69945015609330596, 461.9657866046125037, 3.159955898139067187 ) ) ;
#9494 = FACE_OUTER_BOUND ( 'NONE', #71118, .T. ) ;
#9495 = CARTESIAN_POINT ( 'NONE',  ( -40.90326834193143668, -56.80365015598610512, 43.40273101573804837 ) ) ;
#9496 = ADVANCED_FACE ( 'NONE', ( #58349 ), #90460, .T. ) ;
#9497 = DIRECTION ( 'NONE',  ( 0.000000000000000000, 1.000000000000000000, 0.000000000000000000 ) ) ;
#9498 = UNCERTAINTY_MEASURE_WITH_UNIT (LENGTH_MEASURE( 1.000000000000000082E-05 ), #37526, 'distance_accuracy_value', 'NONE');
#9499 = ORIENTED_EDGE ( 'NONE', *, *, #12477, .F. ) ;
#9500 = CARTESIAN_POINT ( 'NONE',  ( -3.301565691951523718, -4.285714285714295357, 25.05982991920904368 ) ) ;
#9501 = CARTESIAN_POINT ( 'NONE',  ( 8.559508646656407649, 53.96349637827586321, 1.531152949374444239 ) ) ;
#9502 = CARTESIAN_POINT ( 'NONE',  ( 31.14694070047868735, 432.3293837220155069, 24.29762062537629319 ) ) ;
#9503 = CARTESIAN_POINT ( 'NONE',  ( 6.562934840145638660, 4.277581483015135966, 6.282640795011893431 ) ) ;
#9504 = DIRECTION ( 'NONE',  ( -1.000000000000000000, -1.224606353822377258E-16, -0.000000000000000000 ) ) ;
#9505 = EDGE_LOOP ( 'NONE', ( #106211, #96691, #95778, #4962, #32234 ) ) ;
#9506 = DIRECTION ( 'NONE',  ( 1.000000000000000000, 1.224606353822377258E-16, 0.000000000000000000 ) ) ;
#9507 = ORIENTED_EDGE ( 'NONE', *, *, #85508, .T. ) ;
#9508 = VECTOR ( 'NONE', #55206, 1000.000000000000000 ) ;
#9509 = CARTESIAN_POINT ( 'NONE',  ( 80.48472413805814085, -30.00000000000003197, -13.06866816408327381 ) ) ;
#9510 = CARTESIAN_POINT ( 'NONE',  ( 47.50656546823845616, 12.72630541683656702, 14.46671989142039472 ) ) ;
#9511 = UNCERTAINTY_MEASURE_WITH_UNIT (LENGTH_MEASURE( 1.000000000000000082E-05 ), #65286, 'distance_accuracy_value', 'NONE');
#9512 = ADVANCED_FACE ( 'NONE', ( #92294 ), #12079, .F. ) ;
#9513 = CARTESIAN_POINT ( 'NONE',  ( 65.03872891708842019, 6.856755485862130937E-15, 0.000000000000000000 ) ) ;
#9514 = CARTESIAN_POINT ( 'NONE',  ( 0.6249999999999998890, 8.299410119600874935, -7.298562697733109061 ) ) ;
#9515 = CARTESIAN_POINT ( 'NONE',  ( 83.28278898132033703, -30.00000000000000711, 45.15681117069227923 ) ) ;
#9516 = PRESENTATION_STYLE_ASSIGNMENT (( #1418 ) ) ;
#9517 = ORIENTED_EDGE ( 'NONE', *, *, #37779, .F. ) ;
#9518 = STYLED_ITEM ( 'NONE', ( #8209 ), #63047 ) ;
#9519 = EDGE_LOOP ( 'NONE', ( #21705, #16002, #69929, #38654, #84351, #9450 ) ) ;
#9520 = ORIENTED_EDGE ( 'NONE', *, *, #59820, .T. ) ;
#9521 = CARTESIAN_POINT ( 'NONE',  ( -47.36715592893472859, 12.99186701195485938, -14.54160185453320331 ) ) ;
#9522 = PRESENTATION_STYLE_ASSIGNMENT (( #42434 ) ) ;
#9523 = CIRCLE ( 'NONE', #59453, 4.000000000000000000 ) ;
#9524 = CARTESIAN_POINT ( 'NONE',  ( 40.92167885334222888, 438.1321558251088959, 22.38353683390997517 ) ) ;
#9525 = CARTESIAN_POINT ( 'NONE',  ( -31.19216271077053548, 416.1733914895696671, 25.29150983624480631 ) ) ;
#9526 = SURFACE_STYLE_FILL_AREA ( #344 ) ;
#9527 = EDGE_LOOP ( 'NONE', ( #95964, #40541 ) ) ;
#9528 = CARTESIAN_POINT ( 'NONE',  ( 3.140974613990258568, 50.00000000000000000, -96.68767211932436112 ) ) ;
#9529 = ORIENTED_EDGE ( 'NONE', *, *, #57916, .F. ) ;
#9530 = CARTESIAN_POINT ( 'NONE',  ( 62.33904886068935980, 6.975173280561618775E-15, 0.000000000000000000 ) ) ;
#9531 = CARTESIAN_POINT ( 'NONE',  ( 75.48692410520401097, -38.35222609583806275, 174.0895271288090100 ) ) ;
#9532 = DIRECTION ( 'NONE',  ( 1.000000000000000000, 1.224606353822377258E-16, 0.000000000000000000 ) ) ;
#9533 = AXIS2_PLACEMENT_3D ( 'NONE', #49299, #104363, #47186 ) ;
#9534 = CARTESIAN_POINT ( 'NONE',  ( 34.86560210343121469, 302.9523858308785975, 3.794354053605914157 ) ) ;
#9535 = AXIS2_PLACEMENT_3D ( 'NONE', #19895, #12800, #45716 ) ;
#9536 = MECHANICAL_DESIGN_GEOMETRIC_PRESENTATION_REPRESENTATION (  '', ( #85313 ), #55945 ) ;
#9537 = CARTESIAN_POINT ( 'NONE',  ( -4.903871675326607615, 247.9791419269849087, -3.461400506969853019 ) ) ;
#9538 = AXIS2_PLACEMENT_3D ( 'NONE', #56489, #105581, #96449 ) ;
#9539 = ORIENTED_EDGE ( 'NONE', *, *, #29584, .F. ) ;
#9540 = CARTESIAN_POINT ( 'NONE',  ( 43.58349330513380693, 4.000000000000002665, 0.000000000000000000 ) ) ;
#9541 = CYLINDRICAL_SURFACE ( 'NONE', #35177, 3.400000000000000355 ) ;
#9542 =( BOUNDED_CURVE ( )  B_SPLINE_CURVE ( 3, ( #34268, #74677, #100026, #759, #9402, #41263, #73616, #105983, #33726, #56898, #33198, #17005, #90348, #82787 ),
 .UNSPECIFIED., .F., .F. ) 
 B_SPLINE_CURVE_WITH_KNOTS ( ( 4, 2, 2, 2, 2, 2, 4 ),
 ( 0.000000000000000000, 0.05368345394220581934, 0.1429467631537782168, 0.2322100723653506005, 0.3214733815769227343, 0.4107366907884949514, 0.5000000000031382674 ),
 .UNSPECIFIED. ) 
 CURVE ( )  GEOMETRIC_REPRESENTATION_ITEM ( )  RATIONAL_B_SPLINE_CURVE ( ( 1.420262811277154924, 1.420262811277154924, 1.420262811277154924, 1.420262811277154924, 1.420262811277154924, 1.420262811277154924, 1.420262811277154924, 1.420262811277154924, 1.420262811277154924, 1.420262811277154924, 1.420262811277154924, 1.420262811277154924, 1.420262811277154924, 1.420262811277154924 ) ) 
 REPRESENTATION_ITEM ( '' )  );
#9543 = EDGE_CURVE ( 'NONE', #32861, #39589, #4384, .T. ) ;
#9544 = DIRECTION ( 'NONE',  ( 0.000000000000000000, 0.000000000000000000, -1.000000000000000000 ) ) ;
#9545 = CARTESIAN_POINT ( 'NONE',  ( 14.89734172081147179, 1.349300515449291193, -1.760806480387048012 ) ) ;
#9546 = ORIENTED_EDGE ( 'NONE', *, *, #12276, .F. ) ;
#9547 = CARTESIAN_POINT ( 'NONE',  ( -22.72024110750421144, 303.4016505345416590, 10.05551265021215102 ) ) ;
#9548 = CARTESIAN_POINT ( 'NONE',  ( 6.849999999999999645, 4.618802153517004960, 7.999999999999998224 ) ) ;
#9549 = UNCERTAINTY_MEASURE_WITH_UNIT (LENGTH_MEASURE( 1.000000000000000082E-05 ), #65546, 'distance_accuracy_value', 'NONE');
#9550 = CARTESIAN_POINT ( 'NONE',  ( 5.700000000000000178, 0.000000000000000000, 0.000000000000000000 ) ) ;
#9551 = DIRECTION ( 'NONE',  ( -1.000000000000000000, -0.000000000000000000, -0.000000000000000000 ) ) ;
#9552 = CARTESIAN_POINT ( 'NONE',  ( 0.000000000000000000, 299.9999999999999432, 0.000000000000000000 ) ) ;
#9553 = EDGE_CURVE ( 'NONE', #90138, #30441, #22575, .T. ) ;
#9554 = CARTESIAN_POINT ( 'NONE',  ( 1.128086991930825622, 302.6818553553993070, 9.936167255975588475 ) ) ;
#9555 = DIRECTION ( 'NONE',  ( 0.000000000000000000, -1.000000000000000000, 0.000000000000000000 ) ) ;
#9556 = CARTESIAN_POINT ( 'NONE',  ( 86.25580709159085302, -24.66185776332405766, 181.7623954071263199 ) ) ;
#9557 =( NAMED_UNIT ( * ) PLANE_ANGLE_UNIT ( ) SI_UNIT ( $, .RADIAN. ) );
#9558 = CARTESIAN_POINT ( 'NONE',  ( 0.000000000000000000, -19.99999999999998934, 0.000000000000000000 ) ) ;
#9559 = ORIENTED_EDGE ( 'NONE', *, *, #56319, .F. ) ;
#9560 = CARTESIAN_POINT ( 'NONE',  ( 94.58869087161561140, -57.65564386714318346, -10.20074617627543212 ) ) ;
#9561 = CARTESIAN_POINT ( 'NONE',  ( -5.075741750048029743, -4.332638003024074536, -17.09621982684887698 ) ) ;
#9562 = DIRECTION ( 'NONE',  ( 1.000000000000000000, 0.000000000000000000, 0.000000000000000000 ) ) ;
#9563 = CARTESIAN_POINT ( 'NONE',  ( -3.482999479109682994E-15, 5.309483803148794756, 3.803704290982253600 ) ) ;
#9564 = COLOUR_RGB ( '', 0.66274510, 0.83137255, 0.94901961) ;
#9565 = CARTESIAN_POINT ( 'NONE',  ( -81.40749646105963677, -30.00000000000000711, -10.00555188706439580 ) ) ;
#9566 = DIRECTION ( 'NONE',  ( -1.000000000000000000, -1.224606353822377258E-16, -0.000000000000000000 ) ) ;
#9567 = CARTESIAN_POINT ( 'NONE',  ( 0.000000000000000000, 7.505553499465140277, -3.755786496842903002E-16 ) ) ;
#9569 = SURFACE_SIDE_STYLE ('',( #30712 ) ) ;
#9568 = FACE_OUTER_BOUND ( 'NONE', #74486, .T. ) ;
#9570 = EDGE_CURVE ( 'NONE', #49798, #85237, #66347, .T. ) ;
#9571 = DIRECTION ( 'NONE',  ( 0.000000000000000000, -1.000000000000000000, 0.000000000000000000 ) ) ;
#9572 = CARTESIAN_POINT ( 'NONE',  ( 18.13561277374696701, 5.000000000000004441, 6.123233995736770227E-16 ) ) ;
#9573 = CARTESIAN_POINT ( 'NONE',  ( -19.44294908207561434, 50.00000000000000000, 59.98229726226637126 ) ) ;
#9574 = CARTESIAN_POINT ( 'NONE',  ( 4.590682673078522846, -83.93208242687842358, 3.864023243754608483 ) ) ;
#9575 = DIRECTION ( 'NONE',  ( 0.000000000000000000, -1.000000000000000000, 0.000000000000000000 ) ) ;
#9576 = DIRECTION ( 'NONE',  ( 1.000000000000000000, 1.224606353822377258E-16, 0.000000000000000000 ) ) ;
#9577 = CARTESIAN_POINT ( 'NONE',  ( 14.70186166385661686, -17.16666514262621845, -34.37153611367288164 ) ) ;
#9578 = AXIS2_PLACEMENT_3D ( 'NONE', #52720, #10659, #18261 ) ;
#9579 = ORIENTED_EDGE ( 'NONE', *, *, #70245, .T. ) ;
#9580 = LINE ( 'NONE', #66234, #78919 ) ;
#9581 = LINE ( 'NONE', #43039, #30136 ) ;
#9582 = CARTESIAN_POINT ( 'NONE',  ( -52.11016065996651037, -27.94326923599848911, -27.40981600032927190 ) ) ;
#9585 = EDGE_CURVE ( 'NONE', #59429, #58935, #104228, .T. ) ;
#9584 = DIRECTION ( 'NONE',  ( 1.000000000000000000, -0.000000000000000000, -0.000000000000000000 ) ) ;
#9583 = CARTESIAN_POINT ( 'NONE',  ( -5.601730134768055258, 12.35429686688392259, -0.02849990174189845002 ) ) ;
#9586 = ADVANCED_FACE ( 'NONE', ( #63007 ), #871, .T. ) ;
#9587 = EDGE_LOOP ( 'NONE', ( #76088, #8626, #71562, #64861 ) ) ;
#9588 = LINE ( 'NONE', #18806, #32429 ) ;
#9589 = ORIENTED_EDGE ( 'NONE', *, *, #75414, .F. ) ;
#9590 = CARTESIAN_POINT ( 'NONE',  ( 0.000000000000000000, 0.000000000000000000, 0.000000000000000000 ) ) ;
#9591 = CARTESIAN_POINT ( 'NONE',  ( 15.92744347757530221, 3.245128719855334243, 1.809264762061174148 ) ) ;
#9592 = CARTESIAN_POINT ( 'NONE',  ( -49.87223528229673519, -60.00000000000000711, -37.92974157021075143 ) ) ;
#9593 = ORIENTED_EDGE ( 'NONE', *, *, #33326, .T. ) ;
#9594 = FACE_OUTER_BOUND ( 'NONE', #33994, .T. ) ;
#9595 = CARTESIAN_POINT ( 'NONE',  ( 15.19414944962543501, 3.422781246271796807, 3.910013010458846860 ) ) ;
#9596 = AXIS2_PLACEMENT_3D ( 'NONE', #10151, #58720, #99694 ) ;
#9597 = CARTESIAN_POINT ( 'NONE',  ( 99.16506380945328658, -37.81309594716023526, 191.7295361414442709 ) ) ;
#9599 = CARTESIAN_POINT ( 'NONE',  ( -19.50000000000000000, 12.99999999999999289, -6.999999999999999112 ) ) ;
#9598 = CARTESIAN_POINT ( 'NONE',  ( 1.140108047462715213, 294.8483045722556994, -9.950907916673100928 ) ) ;
#9600 = VERTEX_POINT ( 'NONE', #35710 ) ;
#9601 = ORIENTED_EDGE ( 'NONE', *, *, #53684, .F. ) ;
#9602 = AXIS2_PLACEMENT_3D ( 'NONE', #7191, #56259, #8787 ) ;
#9603 = ORIENTED_EDGE ( 'NONE', *, *, #27926, .F. ) ;
#9604 = CARTESIAN_POINT ( 'NONE',  ( 28.08241411638673313, 315.5964502779369241, 11.56403391043465767 ) ) ;
#9605 = EDGE_CURVE ( 'NONE', #30104, #18278, #40481, .T. ) ;
#9606 = CARTESIAN_POINT ( 'NONE',  ( -13.50000000000000000, 7.794228634059985339, -11.79422863405993382 ) ) ;
#9607 = DIRECTION ( 'NONE',  ( 0.000000000000000000, 0.000000000000000000, -1.000000000000000000 ) ) ;
#9608 = ORIENTED_EDGE ( 'NONE', *, *, #27451, .F. ) ;
#9609 = DIRECTION ( 'NONE',  ( 0.000000000000000000, -1.000000000000000000, 0.000000000000000000 ) ) ;
#9610 = CARTESIAN_POINT ( 'NONE',  ( 6.683837171061802529, 3.955946848495962787, 6.851900933636986935 ) ) ;
#9611 = CARTESIAN_POINT ( 'NONE',  ( -18.91791044776116237, 46.00000000000000000, 62.18611311450884926 ) ) ;
#9612 = CARTESIAN_POINT ( 'NONE',  ( -5.653151814788443197, -60.00000000000000000, -44.93963918615513364 ) ) ;
#9613 = CARTESIAN_POINT ( 'NONE',  ( 6.269955739554009533, 4.268932597852935551, -6.443844059477446429 ) ) ;
#9614 = CIRCLE ( 'NONE', #38986, 8.000000000000000000 ) ;
#9615 = CARTESIAN_POINT ( 'NONE',  ( -25.95507789760542039, 309.1386286255022924, 10.94030088463808070 ) ) ;
#9616 = CARTESIAN_POINT ( 'NONE',  ( -6.563169324595991228, 41.73030616478934007, -58.95245868007680201 ) ) ;
#9617 = EDGE_CURVE ( 'NONE', #94562, #86521, #83774, .T. ) ;
#9618 = CARTESIAN_POINT ( 'NONE',  ( -78.96607584984282369, -14.21045842199439946, -22.44766605243856361 ) ) ;
#9619 = EDGE_CURVE ( 'NONE', #90133, #100942, #18186, .T. ) ;
#9620 = CYLINDRICAL_SURFACE ( 'NONE', #34456, 4.000000000000000000 ) ;
#9621 = CARTESIAN_POINT ( 'NONE',  ( -50.61134058422784676, -46.44362122540161408, 54.16156104182443443 ) ) ;
#9622 = DIRECTION ( 'NONE',  ( -1.000000000000000000, 0.000000000000000000, 0.000000000000000000 ) ) ;
#9623 = B_SPLINE_CURVE_WITH_KNOTS ( 'NONE', 3,
 ( #51793, #87240, #79130, #5255 ),
 .UNSPECIFIED., .F., .F.,
 ( 4, 4 ),
 ( 0.000000000000000000, 1.000000000000000000 ),
 .UNSPECIFIED. ) ;
#9624 = EDGE_LOOP ( 'NONE', ( #84174, #83832, #27247, #77449 ) ) ;
#9625 = CARTESIAN_POINT ( 'NONE',  ( -5.656854249492379694, -13.43749999999999112, -5.656854249492380582 ) ) ;
#9626 = CARTESIAN_POINT ( 'NONE',  ( -9.297673743024688520, 295.3592874400207506, -10.03978397955126312 ) ) ;
#9627 = CARTESIAN_POINT ( 'NONE',  ( 12.16009604706015779, -2.477469372512389967, 20.68467756193690121 ) ) ;
#9628 = ORIENTED_EDGE ( 'NONE', *, *, #88665, .T. ) ;
#9629 = CARTESIAN_POINT ( 'NONE',  ( 5.727189096784626621, 246.4213012475125311, -1.806430436190365585 ) ) ;
#9630 = CARTESIAN_POINT ( 'NONE',  ( 104.9507826212073951, -38.39463534192324801, 197.5418619574190870 ) ) ;
#9631 = DIRECTION ( 'NONE',  ( -1.000000000000000000, -0.000000000000000000, -0.000000000000000000 ) ) ;
#9632 = ADVANCED_FACE ( 'NONE', ( #39271 ), #93912, .F. ) ;
#9633 = CARTESIAN_POINT ( 'NONE',  ( -21.19348424345039206, 294.8901562694577478, 1.945151701991078896 ) ) ;
#9634 = CONICAL_SURFACE ( 'NONE', #6248, 4.000000000000001776, 0.9599310885968808105 ) ;
#9635 =( NAMED_UNIT ( * ) SI_UNIT ( $, .STERADIAN. ) SOLID_ANGLE_UNIT ( ) );
#9636 = CARTESIAN_POINT ( 'NONE',  ( 91.73269967366050537, -29.99999999999999289, 190.7761219706676172 ) ) ;
#9637 = CARTESIAN_POINT ( 'NONE',  ( 21.08349330513380337, 4.000000000000003553, 0.000000000000000000 ) ) ;
#9638 =( LENGTH_UNIT ( ) NAMED_UNIT ( * ) SI_UNIT ( .MILLI., .METRE. ) );
#9639 = PLANE ( 'NONE',  #31218 ) ;
#9640 = ORIENTED_EDGE ( 'NONE', *, *, #59985, .F. ) ;
#9641 = VERTEX_POINT ( 'NONE', #87283 ) ;
#9642 = CARTESIAN_POINT ( 'NONE',  ( 52.74211290327268387, -29.10573497541706089, 51.84957213115916375 ) ) ;
#9643 = CARTESIAN_POINT ( 'NONE',  ( 6.390966725705288454, 41.59892189792125095, -58.65495604877497726 ) ) ;
#9644 = CARTESIAN_POINT ( 'NONE',  ( -5.500000000000006217, 42.00000000000000000, -62.89165061483231511 ) ) ;
#9645 = VERTEX_POINT ( 'NONE', #46287 ) ;
#9646 = CARTESIAN_POINT ( 'NONE',  ( -105.0815908665296945, -38.35658034820646378, 118.4378099064370105 ) ) ;
#9647 = EDGE_LOOP ( 'NONE', ( #53158, #84044, #103854, #20826 ) ) ;
#9648 = DIRECTION ( 'NONE',  ( 0.000000000000000000, -1.000000000000000000, 0.000000000000000000 ) ) ;
#9649 = CARTESIAN_POINT ( 'NONE',  ( 110.8582216372020923, -38.35606662024349589, 166.2350381741399019 ) ) ;
#9650 = CARTESIAN_POINT ( 'NONE',  ( 13.55851780043528443, 24.71083649413047212, -1.216380116763536856 ) ) ;
#9651 = CARTESIAN_POINT ( 'NONE',  ( 84.26382309112767643, -37.84986900746150695, 39.36842225124562589 ) ) ;
#9652 = CARTESIAN_POINT ( 'NONE',  ( 35.22756082728740523, 435.7361056000421513, 6.213820150723853075 ) ) ;
#9653 = CARTESIAN_POINT ( 'NONE',  ( -2.617478843592807358, -3.000000000000003109, -75.26027323331685182 ) ) ;
#9654 = CARTESIAN_POINT ( 'NONE',  ( 3.783418949173140255, -11.62946060510860313, -10.57964823094882512 ) ) ;
#9655 = CARTESIAN_POINT ( 'NONE',  ( 74.83933575179801778, -60.00000000000000000, 180.0232458328126199 ) ) ;
#9656 = LINE ( 'NONE', #42568, #28868 ) ;
#9657 = AXIS2_PLACEMENT_3D ( 'NONE', #37888, #30306, #88528 ) ;
#9658 = CARTESIAN_POINT ( 'NONE',  ( 17.53980351349540356, 45.00000000000001421, 63.37883192130072985 ) ) ;
#9659 = VERTEX_POINT ( 'NONE', #10836 ) ;
#9660 = CARTESIAN_POINT ( 'NONE',  ( 61.52822294692849425, -22.11542171271097601, 67.98225717687230940 ) ) ;
#9661 = ADVANCED_FACE ( 'NONE', ( #43756 ), #68588, .F. ) ;
#9662 = DIRECTION ( 'NONE',  ( 1.000000000000000000, 0.000000000000000000, 0.000000000000000000 ) ) ;
#9663 = AXIS2_PLACEMENT_3D ( 'NONE', #106670, #64125, #6915 ) ;
#9664 = CARTESIAN_POINT ( 'NONE',  ( -8.786332869125764944, -4.999999999999999112, -16.86266621361376750 ) ) ;
#9665 = CARTESIAN_POINT ( 'NONE',  ( -36.70909933119551027, 484.6513994032500818, -2.859602155942893020 ) ) ;
#9666 = CARTESIAN_POINT ( 'NONE',  ( -40.63912328307429078, 353.8711978207421112, 23.30721375645484983 ) ) ;
#9667 = DIRECTION ( 'NONE',  ( 0.000000000000000000, 1.000000000000000000, 0.000000000000000000 ) ) ;
#9668 = DIRECTION ( 'NONE',  ( 0.000000000000000000, 1.000000000000000000, 0.000000000000000000 ) ) ;
#9669 = CARTESIAN_POINT ( 'NONE',  ( -5.656854249492381470, -29.56249999999999645, 5.656854249492379694 ) ) ;
#9670 =( LENGTH_UNIT ( ) NAMED_UNIT ( * ) SI_UNIT ( .MILLI., .METRE. ) );
#9671 = EDGE_CURVE ( 'NONE', #88738, #14520, #5301, .T. ) ;
#9672 = B_SPLINE_CURVE_WITH_KNOTS ( 'NONE', 3,
 ( #55015, #89004, #38866, #71732, #47986, #39402 ),
 .UNSPECIFIED., .F., .F.,
 ( 4, 2, 4 ),
 ( 0.01390592816464533005, 0.01784842065628997748, 0.02179091314793462145 ),
 .UNSPECIFIED. ) ;
#9673 = AXIS2_PLACEMENT_3D ( 'NONE', #32115, #39678, #64997 ) ;
#9674 = TOROIDAL_SURFACE ( 'NONE', #28680, 6.999999999999999112, 0.5000000000000000000 ) ;
#9675 = CONICAL_SURFACE ( 'NONE', #16548, 5.000000000000000000, 0.9599310885968913576 ) ;
#9676 = CARTESIAN_POINT ( 'NONE',  ( 15.42181578661909747, 44.08896874612430139, -5.093856415474347976 ) ) ;
#9677 = VERTEX_POINT ( 'NONE', #19535 ) ;
#9678 = CARTESIAN_POINT ( 'NONE',  ( 85.58339654611728520, -25.25876667343988657, 173.5966304797753423 ) ) ;
#9679 = CARTESIAN_POINT ( 'NONE',  ( -38.17791925832861466, 27.65688341279261664, 11.10440149930134091 ) ) ;
#9680 = CARTESIAN_POINT ( 'NONE',  ( -4.912113277822308000, -8.720202683089764761, 6.401595221162452276 ) ) ;
#9681 = ORIENTED_EDGE ( 'NONE', *, *, #74405, .F. ) ;
#9682 = CARTESIAN_POINT ( 'NONE',  ( -8.000000000000000000, -32.93750000409677625, -9.797174393178825657E-16 ) ) ;
#9683 = VECTOR ( 'NONE', #83251, 1000.000000000000000 ) ;
#9684 = FACE_OUTER_BOUND ( 'NONE', #102675, .T. ) ;
#9685 = DIRECTION ( 'NONE',  ( -1.000000000000000000, -1.224606353822377258E-16, -0.000000000000000000 ) ) ;
#9686 = CARTESIAN_POINT ( 'NONE',  ( 0.000000000000000000, -30.00000000000000000, 0.000000000000000000 ) ) ;
#9687 = CARTESIAN_POINT ( 'NONE',  ( -11.78124729767428924, -3.000000000000002665, -94.38183245065363280 ) ) ;
#9688 = VECTOR ( 'NONE', #79237, 1000.000000000000000 ) ;
#9689 = CARTESIAN_POINT ( 'NONE',  ( -18.64887156299073823, -25.34552484672397910, -38.50094829128359208 ) ) ;
#9690 = CARTESIAN_POINT ( 'NONE',  ( -11.46837915170103983, -1.524771657339345721, 20.53918122967341375 ) ) ;
#9691 = ADVANCED_FACE ( 'NONE', ( #52372 ), #21575, .T. ) ;
#9692 = CARTESIAN_POINT ( 'NONE',  ( 46.76626013676900584, -60.00000000000000711, 64.25575086454696816 ) ) ;
#9693 = AXIS2_PLACEMENT_3D ( 'NONE', #97083, #47988, #73323 ) ;
#9694 = DIRECTION ( 'NONE',  ( 0.000000000000000000, -1.000000000000000000, 0.000000000000000000 ) ) ;
#9695 = CARTESIAN_POINT ( 'NONE',  ( 5.358783066250208726, -12.92270511644005460, 32.09298117868684841 ) ) ;
#9697 = CARTESIAN_POINT ( 'NONE',  ( -13.32385011686026566, 24.28998873518373358, -2.970456920810112145 ) ) ;
#9696 = CARTESIAN_POINT ( 'NONE',  ( -14.21687706511438876, -22.25485696289420190, 35.82459387298590059 ) ) ;
#9698 = FACE_OUTER_BOUND ( 'NONE', #15311, .T. ) ;
#9699 = CARTESIAN_POINT ( 'NONE',  ( -5.082755093536326818, -9.218750002048382797, 5.082755093536325042 ) ) ;
#9700 = CARTESIAN_POINT ( 'NONE',  ( 0.3351242481862675704, -69.52513411664634191, 12.72773023341044940 ) ) ;
#9701 = CARTESIAN_POINT ( 'NONE',  ( -1.305263714129178521, 8.377797850839289850, -7.792447862505335721 ) ) ;
#9702 = ORIENTED_EDGE ( 'NONE', *, *, #9406, .F. ) ;
#9703 = DIRECTION ( 'NONE',  ( 0.000000000000000000, -1.155626614413199331E-16, 1.000000000000000000 ) ) ;
#9704 = AXIS2_PLACEMENT_3D ( 'NONE', #12770, #54821, #62413 ) ;
#9705 = CARTESIAN_POINT ( 'NONE',  ( -18.92590207683343806, 49.07586612980275476, 62.10725160223359609 ) ) ;
#9706 = CARTESIAN_POINT ( 'NONE',  ( -15.92336767484350801, -2.186116430727330417, 14.84188263806296426 ) ) ;
#9707 =( GEOMETRIC_REPRESENTATION_CONTEXT ( 3 ) GLOBAL_UNCERTAINTY_ASSIGNED_CONTEXT ( ( #68580 ) ) GLOBAL_UNIT_ASSIGNED_CONTEXT ( ( #104340, #8832, #16946 ) ) REPRESENTATION_CONTEXT ( 'NONE', 'WORKASPACE' ) );
#9708 = CARTESIAN_POINT ( 'NONE',  ( -41.43869626312952903, 465.5146466453550715, 16.04577920756167231 ) ) ;
#9710 = CARTESIAN_POINT ( 'NONE',  ( 53.22521075176659622, -34.58939553375807918, -27.04733313792341676 ) ) ;
#9709 = CARTESIAN_POINT ( 'NONE',  ( 4.151327550446272774, 54.24139430477373480, 6.759075926815422797 ) ) ;
#9711 = ORIENTED_EDGE ( 'NONE', *, *, #98224, .T. ) ;
#9712 = CARTESIAN_POINT ( 'NONE',  ( 14.29190075645646907, 21.26710225494832329, -5.626279437268317807 ) ) ;
#9713 = ORIENTED_EDGE ( 'NONE', *, *, #19686, .F. ) ;
#9714 = DIRECTION ( 'NONE',  ( -1.000000000000000000, -1.224606353822377258E-16, -0.000000000000000000 ) ) ;
#9715 = CARTESIAN_POINT ( 'NONE',  ( 0.000000000000000000, 0.000000000000000000, 0.000000000000000000 ) ) ;
#9716 = CARTESIAN_POINT ( 'NONE',  ( -16.11469797371095325, 41.97267161074977793, -84.98552174202809795 ) ) ;
#9717 = CARTESIAN_POINT ( 'NONE',  ( -102.8043655696301641, -60.00000000000000000, 97.43818821035735311 ) ) ;
#9718 = CARTESIAN_POINT ( 'NONE',  ( -33.00000000000000000, 450.0000000000002274, 13.20242257375370976 ) ) ;
#9719 = DIRECTION ( 'NONE',  ( -1.000000000000000000, 0.000000000000000000, 0.000000000000000000 ) ) ;
#9720 = CARTESIAN_POINT ( 'NONE',  ( 35.66932529116966322, 438.9565575286536045, 4.011496722538590909 ) ) ;
#9721 = CARTESIAN_POINT ( 'NONE',  ( 41.33517203638527349, 460.1869644147471945, 2.191757750721595066 ) ) ;
#9723 = CARTESIAN_POINT ( 'NONE',  ( 29.99999999999916156, 487.3993633549791298, 6.447931125014418896 ) ) ;
#9722 = CARTESIAN_POINT ( 'NONE',  ( -33.52854060314342632, 435.4521953938931347, 9.505701922647736168 ) ) ;
#9724 = CARTESIAN_POINT ( 'NONE',  ( -85.11569458792331488, -25.46023517225657784, 167.9907940485576887 ) ) ;
#9725 = ORIENTED_EDGE ( 'NONE', *, *, #63645, .F. ) ;
#9726 = SURFACE_SIDE_STYLE ('',( #18948 ) ) ;
#9727 = VERTEX_POINT ( 'NONE', #40312 ) ;
#9728 = VERTEX_POINT ( 'NONE', #74790 ) ;
#9729 = CARTESIAN_POINT ( 'NONE',  ( -20.37278541768183615, 303.8378246129572631, -10.00297115033342266 ) ) ;
#9730 = EDGE_CURVE ( 'NONE', #60518, #97465, #90081, .T. ) ;
#9731 = CARTESIAN_POINT ( 'NONE',  ( 0.000000000000000000, 0.000000000000000000, -0.7408754770741831086 ) ) ;
#9732 = VERTEX_POINT ( 'NONE', #16571 ) ;
#9733 = CARTESIAN_POINT ( 'NONE',  ( -73.19784523472750948, -56.33007067409605639, -24.31537338432895012 ) ) ;
#9734 = EDGE_CURVE ( 'NONE', #88628, #75560, #11553, .T. ) ;
#9735 = LINE ( 'NONE', #90143, #7753 ) ;
#9736 = CARTESIAN_POINT ( 'NONE',  ( -7.744168461338430731, -61.53745938284842509, 2.019395720771554270 ) ) ;
#9737 = DIRECTION ( 'NONE',  ( 0.000000000000000000, -1.000000000000000000, 0.000000000000000000 ) ) ;
#9738 = SURFACE_STYLE_USAGE ( .BOTH. , #75553 ) ;
#9739 = DIRECTION ( 'NONE',  ( 0.000000000000000000, 0.000000000000000000, -1.000000000000000000 ) ) ;
#9740 = CARTESIAN_POINT ( 'NONE',  ( 104.0150978814680940, -30.00000000000001421, 120.6686366764556766 ) ) ;
#9741 = EDGE_CURVE ( 'NONE', #102808, #52615, #80130, .T. ) ;
#9742 = CARTESIAN_POINT ( 'NONE',  ( -79.57248154261856143, -14.21045842199419873, 190.0114072710836979 ) ) ;
#9743 = CARTESIAN_POINT ( 'NONE',  ( -58.95728471227350553, -25.60210830145040717, 63.31610968965730990 ) ) ;
#9744 = VERTEX_POINT ( 'NONE', #105572 ) ;
#9745 = CARTESIAN_POINT ( 'NONE',  ( -1.128238012697766912, 300.0000000000000000, 9.936150108905552614 ) ) ;
#9746 = CARTESIAN_POINT ( 'NONE',  ( 63.92811455585417946, -60.00000000001919176, -37.02723835566183652 ) ) ;
#9747 = CIRCLE ( 'NONE', #83837, 6.500000000000000888 ) ;
#9748 = ORIENTED_EDGE ( 'NONE', *, *, #100472, .F. ) ;
#9749 = CARTESIAN_POINT ( 'NONE',  ( 5.068871021964256762, -39.47244754689903345, 30.45846616484312008 ) ) ;
#9750 = MECHANICAL_DESIGN_GEOMETRIC_PRESENTATION_REPRESENTATION (  '', ( #102791 ), #99289 ) ;
#9751 = CARTESIAN_POINT ( 'NONE',  ( -101.0703404440478153, -37.82018982836708432, 188.0744957792581715 ) ) ;
#9753 = CIRCLE ( 'NONE', #92371, 5.000000000000011546 ) ;
#9752 = CARTESIAN_POINT ( 'NONE',  ( 6.162888688655347558, 7.505553499465140277, 0.000000000000000000 ) ) ;
#9754 = DIRECTION ( 'NONE',  ( -1.000000000000000000, -1.224606353822377258E-16, -0.000000000000000000 ) ) ;
#9755 = DIRECTION ( 'NONE',  ( -1.000000000000000000, -1.224606353822377258E-16, -0.000000000000000000 ) ) ;
#9756 = ORIENTED_EDGE ( 'NONE', *, *, #62642, .F. ) ;
#9757 = LINE ( 'NONE', #82602, #21852 ) ;
#9759 = VECTOR ( 'NONE', #42929, 1000.000000000000000 ) ;
#9758 = CARTESIAN_POINT ( 'NONE',  ( -36.70586056242206041, -60.00000000000001421, 48.05235279427500927 ) ) ;
#9760 = CARTESIAN_POINT ( 'NONE',  ( 31.08349330513380337, -4.000000000000000000, 4.898587196589415787E-16 ) ) ;
#9761 = CARTESIAN_POINT ( 'NONE',  ( -2.977408999572650039, -20.56250000204838457, -7.188101187500001821 ) ) ;
#9762 = ADVANCED_FACE ( 'NONE', ( #16032 ), #98014, .T. ) ;
#9763 = CARTESIAN_POINT ( 'NONE',  ( -5.000000000000000000, 6.123233995736766282E-16, 0.000000000000000000 ) ) ;
#9764 = PRESENTATION_LAYER_ASSIGNMENT (  '', '', ( #73435 ) ) ;
#9765 = FACE_OUTER_BOUND ( 'NONE', #93105, .T. ) ;
#9766 = CARTESIAN_POINT ( 'NONE',  ( -1.800054524762938479, 21.43447476329978585, -6.769169511956039997 ) ) ;
#9767 = DIRECTION ( 'NONE',  ( -1.000000000000000000, -1.224606353822377258E-16, -0.000000000000000000 ) ) ;
#9768 = CARTESIAN_POINT ( 'NONE',  ( 24.93816302196866275, 307.4233949143036284, 10.52291764336465008 ) ) ;
#9769 = CARTESIAN_POINT ( 'NONE',  ( 6.101956569544443987, -7.474254432360360134, 13.82088739650973963 ) ) ;
#9770 = CARTESIAN_POINT ( 'NONE',  ( -23.86089617542280550, 27.29447341560883089, 33.04113357524851580 ) ) ;
#9771 = LINE ( 'NONE', #90714, #34532 ) ;
#9772 = CARTESIAN_POINT ( 'NONE',  ( -31.81784266628647018, -42.96403268502453443, 34.45923875972478356 ) ) ;
#9773 = CARTESIAN_POINT ( 'NONE',  ( -2.520370815125025477, -49.57822929787493393, 103.1554032654396735 ) ) ;
#9774 = CARTESIAN_POINT ( 'NONE',  ( 43.84264430761513154, -36.07170451123901955, 41.44757837376981513 ) ) ;
#9775 = SURFACE_STYLE_FILL_AREA ( #17904 ) ;
#9776 = VERTEX_POINT ( 'NONE', #24687 ) ;
#9777 = CARTESIAN_POINT ( 'NONE',  ( -6.928203230275510549, 85.26930929695539874, -4.000000000000000000 ) ) ;
#9778 = CARTESIAN_POINT ( 'NONE',  ( -81.35954770826289462, -38.84021855358666642, 195.0925015028629730 ) ) ;
#9779 = ORIENTED_EDGE ( 'NONE', *, *, #10884, .T. ) ;
#9781 = DIRECTION ( 'NONE',  ( -1.000000000000000000, 0.000000000000000000, 0.000000000000000000 ) ) ;
#9780 = CARTESIAN_POINT ( 'NONE',  ( 42.10086803841213765, 435.6552064019005570, 19.95582312411065828 ) ) ;
#9782 = CARTESIAN_POINT ( 'NONE',  ( 37.33349330513379982, -4.000000000000000000, 4.898587196589415787E-16 ) ) ;
#9783 = DIRECTION ( 'NONE',  ( 0.000000000000000000, 0.000000000000000000, 1.000000000000000000 ) ) ;
#9784 = CARTESIAN_POINT ( 'NONE',  ( -7.040774328009895555, 41.35742559143615438, -58.68913211047704692 ) ) ;
#9785 = CARTESIAN_POINT ( 'NONE',  ( 9.907647895771711788, 15.45478884909084094, -1.400734872026643929 ) ) ;
#9786 = CARTESIAN_POINT ( 'NONE',  ( -12.50000000000000000, 0.000000000000000000, 0.000000000000000000 ) ) ;
#9787 = CARTESIAN_POINT ( 'NONE',  ( 5.000000000000000000, -31.04498766150742384, -0.1867737091359144008 ) ) ;
#9788 =( NAMED_UNIT ( * ) SI_UNIT ( $, .STERADIAN. ) SOLID_ANGLE_UNIT ( ) );
#9789 = VECTOR ( 'NONE', #31553, 1000.000000000000000 ) ;
#9790 = CARTESIAN_POINT ( 'NONE',  ( 108.7801334214385776, -60.00000000000002842, 134.4245170770223297 ) ) ;
#9791 = FACE_OUTER_BOUND ( 'NONE', #41223, .T. ) ;
#9792 = CIRCLE ( 'NONE', #70090, 11.18527996897366528 ) ;
#9793 = CARTESIAN_POINT ( 'NONE',  ( 22.25669491856071858, 5.000000000000002665, 0.000000000000000000 ) ) ;
#9794 = VERTEX_POINT ( 'NONE', #89926 ) ;
#9795 = ADVANCED_FACE ( 'NONE', ( #8996 ), #64599, .T. ) ;
#9796 = CARTESIAN_POINT ( 'NONE',  ( -97.45253354081053487, -29.99999999999991118, 190.9130999118634691 ) ) ;
#9797 = ORIENTED_EDGE ( 'NONE', *, *, #79066, .F. ) ;
#9798 = CARTESIAN_POINT ( 'NONE',  ( 0.000000000000000000, 0.000000000000000000, 0.000000000000000000 ) ) ;
#9799 = CARTESIAN_POINT ( 'NONE',  ( 31.69432218924449174, 348.2033222337485086, 20.16708524006936187 ) ) ;
#9800 = CARTESIAN_POINT ( 'NONE',  ( 20.19615384615384457, 1.411358822780289120E-15, 0.000000000000000000 ) ) ;
#9801 = CARTESIAN_POINT ( 'NONE',  ( -2.977408999572654480, -20.00000000204838813, 7.188101187499999156 ) ) ;
#9802 = PRESENTATION_STYLE_ASSIGNMENT (( #11936 ) ) ;
#9803 = EDGE_CURVE ( 'NONE', #80882, #19372, #81808, .T. ) ;
#9804 = EDGE_CURVE ( 'NONE', #83020, #21929, #45726, .T. ) ;
#9805 = DIRECTION ( 'NONE',  ( 0.000000000000000000, -0.000000000000000000, 1.000000000000000000 ) ) ;
#9806 =( GEOMETRIC_REPRESENTATION_CONTEXT ( 3 ) GLOBAL_UNCERTAINTY_ASSIGNED_CONTEXT ( ( #94448 ) ) GLOBAL_UNIT_ASSIGNED_CONTEXT ( ( #6802, #48310, #80682 ) ) REPRESENTATION_CONTEXT ( 'NONE', 'WORKASPACE' ) );
#9808 = ORIENTED_EDGE ( 'NONE', *, *, #98751, .T. ) ;
#9807 = CARTESIAN_POINT ( 'NONE',  ( -40.38558023182025636, 460.4657127107437873, 1.744790644328846119 ) ) ;
#9809 = CARTESIAN_POINT ( 'NONE',  ( 81.96495203190069390, -42.96965882988520491, 165.6653473756363724 ) ) ;
#9810 = DIRECTION ( 'NONE',  ( 0.000000000000000000, -1.000000000000000000, 0.000000000000000000 ) ) ;
#9811 = CONICAL_SURFACE ( 'NONE', #87298, 3.309500000000001663, 0.9599310885968770357 ) ;
#9812 = PLANE ( 'NONE',  #86768 ) ;
#9813 = EDGE_LOOP ( 'NONE', ( #75618, #60759, #76375 ) ) ;
#9814 = CARTESIAN_POINT ( 'NONE',  ( 42.79777464980544011, 484.2777864412636859, -1.379167304946101513 ) ) ;
#9815 = CARTESIAN_POINT ( 'NONE',  ( -48.02835407290515946, 14.94086294439721030, 16.85535821593516559 ) ) ;
#9816 = CARTESIAN_POINT ( 'NONE',  ( 6.289692432696784685, 1.244853941008388061E-13, 6.828989928337166226 ) ) ;
#9817 = CARTESIAN_POINT ( 'NONE',  ( 30.00000000002700773, 486.5488479674867790, 4.838494452995623085 ) ) ;
#9818 = CARTESIAN_POINT ( 'NONE',  ( 10.91073407590456057, 45.93358294599330094, 13.06300009034433351 ) ) ;
#9819 = CARTESIAN_POINT ( 'NONE',  ( -7.499999902153906106, -3.000145757760796617, -20.99858933621342061 ) ) ;
#9820 = EDGE_CURVE ( 'NONE', #103023, #101842, #104205, .T. ) ;
#9821 = EDGE_LOOP ( 'NONE', ( #2000, #92540, #24125 ) ) ;
#9822 = CIRCLE ( 'NONE', #87384, 6.500000000000000888 ) ;
#9823 = AXIS2_PLACEMENT_3D ( 'NONE', #69723, #102615, #45978 ) ;
#9824 = CARTESIAN_POINT ( 'NONE',  ( 0.000000000000000000, 0.000000000000000000, -10.00000000000000000 ) ) ;
#9825 = CARTESIAN_POINT ( 'NONE',  ( -1.000000000000000000, -59.33879011272768622, 7.480853745783086595 ) ) ;
#9827 = EDGE_CURVE ( 'NONE', #14924, #25868, #33647, .T. ) ;
#9826 = CARTESIAN_POINT ( 'NONE',  ( 87.08998920831058399, -28.00350159148703710, 187.1668149538881494 ) ) ;
#9828 = DIRECTION ( 'NONE',  ( -1.000000000000000000, -1.224606353822377258E-16, -0.000000000000000000 ) ) ;
#9829 = CARTESIAN_POINT ( 'NONE',  ( -1.320432766682874540E-15, -31.53125000204838457, 7.188101187500000044 ) ) ;
#9830 = AXIS2_PLACEMENT_3D ( 'NONE', #105109, #23148, #31251 ) ;
#9831 = CARTESIAN_POINT ( 'NONE',  ( -41.99669677994153005, 488.0206791017693604, 9.049833624058100767 ) ) ;
#9832 = AXIS2_PLACEMENT_3D ( 'NONE', #60340, #50087, #35007 ) ;
#9833 = CARTESIAN_POINT ( 'NONE',  ( 3.250000000000015987, -5.629165124598843661, 1.734723475976807094E-15 ) ) ;
#9834 = EDGE_CURVE ( 'NONE', #63571, #97678, #30184, .T. ) ;
#9835 = CARTESIAN_POINT ( 'NONE',  ( 42.21835935850999988, 436.4384481632506549, 19.62208033733222123 ) ) ;
#9836 = ORIENTED_EDGE ( 'NONE', *, *, #44877, .F. ) ;
#9837 = CARTESIAN_POINT ( 'NONE',  ( -35.75416653242249510, 438.1735696696629248, 3.975240391341059887 ) ) ;
#9839 =( NAMED_UNIT ( * ) SI_UNIT ( $, .STERADIAN. ) SOLID_ANGLE_UNIT ( ) );
#9838 =( BOUNDED_SURFACE ( )  B_SPLINE_SURFACE ( 3, 2, ( 
 ( #71997, #80077, #22945 ),
 ( #95749, #46658, #48233 ),
 ( #7245, #87668, #40155 ),
 ( #13747, #55781, #46144 ) ),
 .UNSPECIFIED., .F., .F., .F. ) 
 B_SPLINE_SURFACE_WITH_KNOTS ( ( 4, 4 ),
 ( 3, 3 ),
 ( -8.673617379884035472E-19, 0.001949576957920114064 ),
 ( 0.000000000000000000, 1.000000000000000000 ),
 .UNSPECIFIED. ) 
 GEOMETRIC_REPRESENTATION_ITEM ( )  RATIONAL_B_SPLINE_SURFACE ( (
 ( 1.000000000000000000, 0.7964405967476593240, 1.000000000000000000),
 ( 1.000000000000000000, 0.8057025330220216608, 1.000000000000000000),
 ( 1.000000000000000000, 0.8148370924185578401, 1.000000000000000000),
 ( 1.000000000000000000, 0.8238944711860017867, 1.000000000000000000) ) ) 
 REPRESENTATION_ITEM ( '' )  SURFACE ( )  );
#9840 = CARTESIAN_POINT ( 'NONE',  ( -9.999342726568489326, 7.500940813882568392, -5.000000000000000888 ) ) ;
#9841 = MECHANICAL_DESIGN_GEOMETRIC_PRESENTATION_REPRESENTATION (  '', ( #8150 ), #104628 ) ;
#9842 = CARTESIAN_POINT ( 'NONE',  ( 21.84999999999999787, -3.309499999999999886, 0.000000000000000000 ) ) ;
#9843 = ORIENTED_EDGE ( 'NONE', *, *, #16347, .T. ) ;
#9844 =( LENGTH_UNIT ( ) NAMED_UNIT ( * ) SI_UNIT ( .MILLI., .METRE. ) );
#9845 = CARTESIAN_POINT ( 'NONE',  ( -7.500000000000004441, 42.83333333333329307, -71.71180648257555390 ) ) ;
#9846 = ORIENTED_EDGE ( 'NONE', *, *, #29456, .T. ) ;
#9847 = DIRECTION ( 'NONE',  ( -1.000000000000000000, -0.000000000000000000, -0.000000000000000000 ) ) ;
#9848 = SURFACE_STYLE_USAGE ( .BOTH. , #83737 ) ;
#9849 = CIRCLE ( 'NONE', #75302, 15.00000000000000000 ) ;
#9850 = CARTESIAN_POINT ( 'NONE',  ( 19.29515645702225868, 3.851859888774471706E-31, 5.000000000000001776 ) ) ;
#9851 = DIRECTION ( 'NONE',  ( -0.000000000000000000, 0.000000000000000000, 1.000000000000000000 ) ) ;
#9852 = CARTESIAN_POINT ( 'NONE',  ( -76.28990388871434902, -60.00000000000000711, 188.1246153785924093 ) ) ;
#9853 = CARTESIAN_POINT ( 'NONE',  ( 0.000000000000000000, 0.000000000000000000, 0.000000000000000000 ) ) ;
#9854 = CARTESIAN_POINT ( 'NONE',  ( 0.000000000000000000, 0.000000000000000000, 0.000000000000000000 ) ) ;
#9855 = DIRECTION ( 'NONE',  ( 1.224646799147349509E-16, 0.000000000000000000, -1.000000000000000000 ) ) ;
#9856 = AXIS2_PLACEMENT_3D ( 'NONE', #105801, #99838, #82050 ) ;
#9857 = CARTESIAN_POINT ( 'NONE',  ( -83.48188574608597889, -57.36243674763982625, 189.6665432021039521 ) ) ;
#9858 = VERTEX_POINT ( 'NONE', #97469 ) ;
#9859 =( NAMED_UNIT ( * ) SI_UNIT ( $, .STERADIAN. ) SOLID_ANGLE_UNIT ( ) );
#9860 = VECTOR ( 'NONE', #38116, 1000.000000000000000 ) ;
#9861 = VERTEX_POINT ( 'NONE', #23626 ) ;
#9862 = CARTESIAN_POINT ( 'NONE',  ( 16.02749411895483078, 4.188372957633037963, -2.551519145317325155 ) ) ;
#9863 = EDGE_CURVE ( 'NONE', #78368, #105843, #50149, .T. ) ;
#9864 = DIRECTION ( 'NONE',  ( 1.000000000000000000, 0.000000000000000000, -0.000000000000000000 ) ) ;
#9865 = CARTESIAN_POINT ( 'NONE',  ( -85.75146761789847005, -52.73616787743888068, -6.162650518953375567 ) ) ;
#9866 =( LENGTH_UNIT ( ) NAMED_UNIT ( * ) SI_UNIT ( .MILLI., .METRE. ) );
#9867 = CARTESIAN_POINT ( 'NONE',  ( -30.00000000000000000, 461.8665070935974768, 11.40527499426167424 ) ) ;
#9868 = DIRECTION ( 'NONE',  ( 0.000000000000000000, 1.000000000000000000, 0.000000000000000000 ) ) ;
#9869 = CARTESIAN_POINT ( 'NONE',  ( 30.11650669486618881, 1.474610560812782335E-15, 0.000000000000000000 ) ) ;
#9870 = CARTESIAN_POINT ( 'NONE',  ( 11.85444436799972934, 42.00000000000000000, 90.56128410203886858 ) ) ;
#9871 = EDGE_CURVE ( 'NONE', #58651, #76997, #66179, .T. ) ;
#9873 = PRESENTATION_LAYER_ASSIGNMENT (  '', '', ( #101220 ) ) ;
#9872 = DIRECTION ( 'NONE',  ( -1.000000000000000000, -1.224606353822377258E-16, -0.000000000000000000 ) ) ;
#9874 = CARTESIAN_POINT ( 'NONE',  ( 70.37902863207267501, -59.99999999999998579, 160.1157867729151576 ) ) ;
#9875 = DIRECTION ( 'NONE',  ( 0.000000000000000000, 0.000000000000000000, 1.000000000000000000 ) ) ;
#9876 = ADVANCED_FACE ( 'NONE', ( #96957 ), #23774, .F. ) ;
#9877 = CARTESIAN_POINT ( 'NONE',  ( 24.89419722466787022, -30.00000000000004974, -38.80375014483585261 ) ) ;
#9878 = CARTESIAN_POINT ( 'NONE',  ( -75.11045228325910728, -39.49349330803696034, 121.1541899256156256 ) ) ;
#9879 = VERTEX_POINT ( 'NONE', #100140 ) ;
#9880 = CARTESIAN_POINT ( 'NONE',  ( 65.47680943546976096, -59.99999999999998579, 130.5870305019238913 ) ) ;
#9881 = CARTESIAN_POINT ( 'NONE',  ( -2.958006552684906865, 40.83778438954344381, 65.00031278382145672 ) ) ;
#9882 = CARTESIAN_POINT ( 'NONE',  ( 2.852950387436009816, -60.00000000016757440, 42.00000030345589153 ) ) ;
#9883 = ORIENTED_EDGE ( 'NONE', *, *, #25905, .T. ) ;
#9884 = CARTESIAN_POINT ( 'NONE',  ( 12.50000000000000355, 41.59226156894002457, -76.70843802411151557 ) ) ;
#9885 = EDGE_CURVE ( 'NONE', #32589, #45380, #101738, .T. ) ;
#9886 = CARTESIAN_POINT ( 'NONE',  ( 98.31310517497099966, 1.030564683017419500E-14, 0.000000000000000000 ) ) ;
#9887 = ORIENTED_EDGE ( 'NONE', *, *, #36515, .F. ) ;
#9889 = CARTESIAN_POINT ( 'NONE',  ( -6.999999999999999112, 0.000000000000000000, 0.000000000000000000 ) ) ;
#9888 = AXIS2_PLACEMENT_3D ( 'NONE', #19563, #95525, #29246 ) ;
#9890 = CARTESIAN_POINT ( 'NONE',  ( 7.007095409419857340E-15, 44.50000000000000711, -57.21727615095610275 ) ) ;
#9891 = EDGE_CURVE ( 'NONE', #91113, #3260, #69829, .T. ) ;
#9892 = DIRECTION ( 'NONE',  ( 0.000000000000000000, 0.000000000000000000, -1.000000000000000000 ) ) ;
#9893 = CARTESIAN_POINT ( 'NONE',  ( -10.85130948263470785, 43.18006360272092792, 15.27593722711275070 ) ) ;
#9894 = CARTESIAN_POINT ( 'NONE',  ( 2.977408999572651815, -14.93750000204838457, 7.188101187500000933 ) ) ;
#9895 = ADVANCED_FACE ( 'NONE', ( #83425 ), #76930, .F. ) ;
#9896 = CARTESIAN_POINT ( 'NONE',  ( -49.24354615586529604, 13.35554545791851666, 15.29900703100092407 ) ) ;
#9897 = CARTESIAN_POINT ( 'NONE',  ( 19.00223544648544660, -4.285714285714296246, -16.66764709352487017 ) ) ;
#9898 = CARTESIAN_POINT ( 'NONE',  ( 3.505888691173186356, -49.11846080224859179, 103.6125332151819833 ) ) ;
#9899 = CARTESIAN_POINT ( 'NONE',  ( 9.601913782316092494, 10.04478976116411815, -12.77952306666690241 ) ) ;
#9900 = DIRECTION ( 'NONE',  ( 0.000000000000000000, 1.000000000000000000, 0.000000000000000000 ) ) ;
#9901 = CARTESIAN_POINT ( 'NONE',  ( -12.13034742782427955, 48.00000000000000000, -93.82352941176471006 ) ) ;
#9902 = ORIENTED_EDGE ( 'NONE', *, *, #78433, .T. ) ;
#9903 = CARTESIAN_POINT ( 'NONE',  ( -7.319239792064268890, 40.56016599439953296, -70.61402026096378393 ) ) ;
#9904 =( GEOMETRIC_REPRESENTATION_CONTEXT ( 3 ) GLOBAL_UNCERTAINTY_ASSIGNED_CONTEXT ( ( #9498 ) ) GLOBAL_UNIT_ASSIGNED_CONTEXT ( ( #37526, #63373, #12135 ) ) REPRESENTATION_CONTEXT ( 'NONE', 'WORKASPACE' ) );
#9905 = PRESENTATION_LAYER_ASSIGNMENT (  '', '', ( #16861 ) ) ;
#9906 = CARTESIAN_POINT ( 'NONE',  ( 32.48674833035018850, -49.90044203452471550, 36.01891768520543735 ) ) ;
#9907 = CARTESIAN_POINT ( 'NONE',  ( -5.124946335852966328, 51.37806724455837326, -8.531152949374570582 ) ) ;
#9908 = ORIENTED_EDGE ( 'NONE', *, *, #104404, .F. ) ;
#9909 = CARTESIAN_POINT ( 'NONE',  ( -0.07780686506603742836, 18.87382441218277407, 49.24999999999999289 ) ) ;
#9910 = EDGE_LOOP ( 'NONE', ( #79667, #99820, #3535, #46627, #21099 ) ) ;
#9911 = AXIS2_PLACEMENT_3D ( 'NONE', #15832, #81602, #40635 ) ;
#9913 = CARTESIAN_POINT ( 'NONE',  ( -0.7814574642159710649, 43.98401667755953781, -16.51064847437958605 ) ) ;
#9912 = CARTESIAN_POINT ( 'NONE',  ( 11.08349330513380160, 1.593028355512270567E-15, 0.000000000000000000 ) ) ;
#9914 = STYLED_ITEM ( 'NONE', ( #81206 ), #58495 ) ;
#9915 = CARTESIAN_POINT ( 'NONE',  ( 9.757377548409222196E-14, 52.17923068443732149, -7.749999999998994582 ) ) ;
#9916 = CARTESIAN_POINT ( 'NONE',  ( -33.00000000000000000, 435.0774731480752848, 11.67986145722080948 ) ) ;
#9917 = CIRCLE ( 'NONE', #78740, 4.000000000000007105 ) ;
#9918 = CARTESIAN_POINT ( 'NONE',  ( -5.500000000000007994, 42.00000000000000000, -68.91429205818155879 ) ) ;
#9919 = CARTESIAN_POINT ( 'NONE',  ( 0.000000000000000000, 0.000000000000000000, 0.000000000000000000 ) ) ;
#9920 = CARTESIAN_POINT ( 'NONE',  ( 0.9433870083987758726, 17.83644259124481479, -49.67632658074430196 ) ) ;
#9921 = ORIENTED_EDGE ( 'NONE', *, *, #72350, .F. ) ;
#9922 = CARTESIAN_POINT ( 'NONE',  ( 92.53276982938558604, -59.99999999999997868, -10.97258584023427375 ) ) ;
#9923 = CARTESIAN_POINT ( 'NONE',  ( -9.507180395705038478, 46.21450860196618038, 13.17662286211865386 ) ) ;
#9924 = B_SPLINE_CURVE_WITH_KNOTS ( 'NONE', 3,
 ( #7635, #39512, #97713, #56173, #22810, #73971, #56721, #65365, #33025, #98257, #23332, #90709, #105291, #80998, #15744, #48627, #38977, #71850, #81513, #104756 ),
 .UNSPECIFIED., .F., .F.,
 ( 4, 2, 2, 2, 2, 2, 2, 2, 2, 4 ),
 ( 0.006900400531842612595, 0.007152251793637217671, 0.007404103055431822747, 0.007907805579021032899, 0.008411508102610243051, 0.008915210626199449734, 0.009418913149788658151, 0.009922615673377864834, 0.01042631819696707152, 0.01093002072055627993 ),
 .UNSPECIFIED. ) ;
#9925 =( NAMED_UNIT ( * ) SI_UNIT ( $, .STERADIAN. ) SOLID_ANGLE_UNIT ( ) );
#9926 = PRESENTATION_LAYER_ASSIGNMENT (  '', '', ( #78829 ) ) ;
#9927 = CARTESIAN_POINT ( 'NONE',  ( 43.58349330513380693, -4.000000000000000888, 4.898587196589416773E-16 ) ) ;
#9928 = ORIENTED_EDGE ( 'NONE', *, *, #5617, .T. ) ;
#9929 = AXIS2_PLACEMENT_3D ( 'NONE', #67041, #78827, #11971 ) ;
#9930 = CARTESIAN_POINT ( 'NONE',  ( 21.36650669486618881, 1.474610560812782335E-15, 0.000000000000000000 ) ) ;
#9931 = VERTEX_POINT ( 'NONE', #11114 ) ;
#9932 = EDGE_LOOP ( 'NONE', ( #48593, #750, #40747, #50229 ) ) ;
#9933 = FACE_OUTER_BOUND ( 'NONE', #13728, .T. ) ;
#9934 = CARTESIAN_POINT ( 'NONE',  ( -6.158268339717665185E-14, -15.58845726811991739, -11.79422863405993382 ) ) ;
#9935 = DIRECTION ( 'NONE',  ( -1.000000000000000000, -1.224606353822377258E-16, -0.000000000000000000 ) ) ;
#9936 = DIRECTION ( 'NONE',  ( 0.000000000000000000, -1.000000000000000000, 0.000000000000000000 ) ) ;
#9937 = CARTESIAN_POINT ( 'NONE',  ( 84.30433287656845209, -52.73991272358569660, -14.69517893486082727 ) ) ;
#9938 = CARTESIAN_POINT ( 'NONE',  ( -39.10808401951415902, 311.3452410718041961, 1.932008273133060783 ) ) ;
#9939 = CARTESIAN_POINT ( 'NONE',  ( -16.97161852214282618, 303.5650176660444117, -10.06095684947478830 ) ) ;
#9940 = CARTESIAN_POINT ( 'NONE',  ( 12.50000000000000000, 29.87326214413186776, -47.66873073394299354 ) ) ;
#9941 = VERTEX_POINT ( 'NONE', #52644 ) ;
#9943 = EDGE_CURVE ( 'NONE', #6938, #12797, #16725, .T. ) ;
#9942 = DIRECTION ( 'NONE',  ( 1.000000000000000000, 0.000000000000000000, -1.734723475976807094E-16 ) ) ;
#9944 = ORIENTED_EDGE ( 'NONE', *, *, #69013, .F. ) ;
#9945 = VECTOR ( 'NONE', #17899, 1000.000000000000000 ) ;
#9946 = CARTESIAN_POINT ( 'NONE',  ( 44.83349330513380693, -7.703719777548943412E-31, 4.000000000000001776 ) ) ;
#9947 = FILL_AREA_STYLE_COLOUR ( '', #36993 ) ;
#9948 = VECTOR ( 'NONE', #92149, 1000.000000000000227 ) ;
#9950 = EDGE_LOOP ( 'NONE', ( #91534, #46239, #50910, #99790 ) ) ;
#9949 = DIRECTION ( 'NONE',  ( 0.000000000000000000, 0.000000000000000000, -1.000000000000000000 ) ) ;
#9951 = CARTESIAN_POINT ( 'NONE',  ( 75.68650039582325917, -32.54705830725040983, 118.5082925635865081 ) ) ;
#9952 = ORIENTED_EDGE ( 'NONE', *, *, #78245, .T. ) ;
#9953 = CARTESIAN_POINT ( 'NONE',  ( 17.50000000000002842, 49.00315172309048961, 64.05179859717361524 ) ) ;
#9955 = CARTESIAN_POINT ( 'NONE',  ( 8.099999999999999645, -7.505553499465142053, -3.129864801432410934E-16 ) ) ;
#9954 = MECHANICAL_DESIGN_GEOMETRIC_PRESENTATION_REPRESENTATION (  '', ( #47809 ), #46081 ) ;
#9956 = CARTESIAN_POINT ( 'NONE',  ( -2.977408999572654480, -27.12500000204838457, 7.188101187499999156 ) ) ;
#9957 = CARTESIAN_POINT ( 'NONE',  ( -88.38279035983548226, -57.66943555457145720, -24.13713039724196818 ) ) ;
#9958 = ORIENTED_EDGE ( 'NONE', *, *, #70282, .T. ) ;
#9959 = B_SPLINE_CURVE_WITH_KNOTS ( 'NONE', 3,
 ( #49610, #57164, #66331, #99214, #32400, #90076, #98681, #24835, #65272, #106779, #14576, #32930, #88498, #98162 ),
 .UNSPECIFIED., .F., .F.,
 ( 4, 2, 2, 2, 2, 2, 4 ),
 ( 2.023315308605685309E-16, 0.001829618653527544016, 0.002744427980291228204, 0.003659237307054911958, 0.005488855960582240436, 0.006403665287345909445, 0.007318474614109578454 ),
 .UNSPECIFIED. ) ;
#9960 =( NAMED_UNIT ( * ) SI_UNIT ( $, .STERADIAN. ) SOLID_ANGLE_UNIT ( ) );
#9961 = DIRECTION ( 'NONE',  ( -1.000000000000000000, 0.000000000000000000, -0.000000000000000000 ) ) ;
#9962 = AXIS2_PLACEMENT_3D ( 'NONE', #12630, #68781, #62806 ) ;
#9963 = CARTESIAN_POINT ( 'NONE',  ( 101.5505671214599914, -37.84846131813309000, 186.3044032585196135 ) ) ;
#9964 = AXIS2_PLACEMENT_3D ( 'NONE', #41363, #82889, #1955 ) ;
#9965 = CARTESIAN_POINT ( 'NONE',  ( -37.56673239365971284, 27.88554838446211548, -10.95617127780556466 ) ) ;
#9966 = LINE ( 'NONE', #74687, #82556 ) ;
#9967 = CARTESIAN_POINT ( 'NONE',  ( -8.000000000000001776, -22.34375000409677625, 3.313708498984758943 ) ) ;
#9968 = LINE ( 'NONE', #17016, #24478 ) ;
#9969 = CARTESIAN_POINT ( 'NONE',  ( 40.11650669486618881, -3.999999999999998224, 0.000000000000000000 ) ) ;
#9970 = FILL_AREA_STYLE_COLOUR ( '', #106677 ) ;
#9971 = EDGE_CURVE ( 'NONE', #81556, #80103, #3585, .T. ) ;
#9972 = CONICAL_SURFACE ( 'NONE', #51312, 4.000000000000001776, 0.9599310885968808105 ) ;
#9973 = CARTESIAN_POINT ( 'NONE',  ( -36.87655955837857391, 438.2068510013161813, 3.933030107424692279 ) ) ;
#9974 = CARTESIAN_POINT ( 'NONE',  ( 32.15166163075728178, 486.0589784586659903, 5.199393881400817818 ) ) ;
#9975 = CARTESIAN_POINT ( 'NONE',  ( 73.88291765283140933, 518.1183258647171215, 182.3141634307102095 ) ) ;
#9976 = CARTESIAN_POINT ( 'NONE',  ( -3.316968746323984085, 15.92795519102023860, -9.435590127033053776 ) ) ;
#9977 = ORIENTED_EDGE ( 'NONE', *, *, #97217, .F. ) ;
#9978 = DIRECTION ( 'NONE',  ( 1.000000000000000000, -0.000000000000000000, -0.000000000000000000 ) ) ;
#9979 = CARTESIAN_POINT ( 'NONE',  ( 6.400000000000000355, 6.613092715395708453E-16, 5.400000000000001243 ) ) ;
#9980 = CARTESIAN_POINT ( 'NONE',  ( 0.07750125733394593042, 7.746009256456432901, 51.75000000000002842 ) ) ;
#9981 = CARTESIAN_POINT ( 'NONE',  ( -87.91521282718065322, -29.99999999999999289, 186.5625098616759487 ) ) ;
#9982 = VERTEX_POINT ( 'NONE', #4114 ) ;
#9983 = CIRCLE ( 'NONE', #96158, 4.000000000000007105 ) ;
#9984 = CARTESIAN_POINT ( 'NONE',  ( 38.78101150684803144, 25.16816242078845534, -12.51454816041207785 ) ) ;
#9985 = AXIS2_PLACEMENT_3D ( 'NONE', #60606, #43863, #84330 ) ;
#9986 = CARTESIAN_POINT ( 'NONE',  ( 70.41623196469389256, -57.68248939742788650, 157.4130776120266546 ) ) ;
#9987 = COLOUR_RGB ( '', 0.40784314, 0.44705882, 0.49803922) ;
#9989 = DIRECTION ( 'NONE',  ( -1.000000000000000000, -0.000000000000000000, -0.000000000000000000 ) ) ;
#9988 = CARTESIAN_POINT ( 'NONE',  ( -14.98982670280977203, 2.030473042281319529, -0.4147640935789676520 ) ) ;
#9990 = ORIENTED_EDGE ( 'NONE', *, *, #69469, .F. ) ;
#9991 = CARTESIAN_POINT ( 'NONE',  ( 45.16523152280084474, -34.40758779083247987, -36.86626960789413232 ) ) ;
#9992 = CARTESIAN_POINT ( 'NONE',  ( -39.83572194810943756, 489.3931820501592824, 11.44122026684815907 ) ) ;
#9993 = CARTESIAN_POINT ( 'NONE',  ( -44.15351406616127861, -60.00000000000000711, 58.95332731642092483 ) ) ;
#9994 = VECTOR ( 'NONE', #44058, 1000.000000000000000 ) ;
#9995 = CARTESIAN_POINT ( 'NONE',  ( -31.36710069068199402, 439.6781111632997181, 23.41206205511423732 ) ) ;
#9996 = FACE_OUTER_BOUND ( 'NONE', #97474, .T. ) ;
#9997 = B_SPLINE_CURVE_WITH_KNOTS ( 'NONE', 3,
 ( #95614, #54064, #61132, #54592, #70809, #6053, #46528, #53563, #69751, #69235, #3954, #94023, #13080, #71328, #53035, #61686, #102104, #62216, #95100, #20184, #21235, #85956, #12029, #44959, #77841, #78888, #105816, #72905, #81002, #82067, #23336, #64319, #71853, #48100 ),
 .UNSPECIFIED., .F., .F.,
 ( 4, 2, 2, 2, 2, 2, 2, 2, 2, 2, 2, 2, 2, 2, 2, 2, 4 ),
 ( 0.000000000000000000, 0.0007951492273476395067, 0.001590298454695279013, 0.002385447682042918845, 0.003180596909390558027, 0.003975746136738197642, 0.004770895364085837691, 0.005566044591433476005, 0.006361193818781115186, 0.007156343046128753500, 0.007951492273476390080, 0.008746641500824029261, 0.009541790728171666708, 0.01033693995551930589, 0.01113208918286694334, 0.01192723841021458078, 0.01272238763756221823 ),
 .UNSPECIFIED. ) ;
#9998 = CARTESIAN_POINT ( 'NONE',  ( -86.31883211543134848, -39.17431195792791243, 187.7266355625923495 ) ) ;
#9999 = ORIENTED_EDGE ( 'NONE', *, *, #30789, .F. ) ;
#10000 = CARTESIAN_POINT ( 'NONE',  ( 30.55657801806797735, 16.37492758275030980, 39.95287151819740501 ) ) ;
#10001 = CARTESIAN_POINT ( 'NONE',  ( -4.101533912778845270, -53.40245796095344843, 32.78225363056029806 ) ) ;
#10002 =( LENGTH_UNIT ( ) NAMED_UNIT ( * ) SI_UNIT ( .MILLI., .METRE. ) );
#10003 = CARTESIAN_POINT ( 'NONE',  ( 32.22503847990217452, 485.9064490506207790, 4.829857536092636572 ) ) ;
#10005 = CARTESIAN_POINT ( 'NONE',  ( 4.190163371923140367, -67.97891175596915048, 13.63061500497633816 ) ) ;
#10004 = CARTESIAN_POINT ( 'NONE',  ( -40.13939232030954685, 319.6057995888056666, 7.960803243963931131 ) ) ;
#10006 = EDGE_LOOP ( 'NONE', ( #83353, #104840, #41816, #98617, #86006 ) ) ;
#10007 = CARTESIAN_POINT ( 'NONE',  ( -33.77601377298719143, 321.0243391643527389, -5.815655461559389394 ) ) ;
#10008 = CARTESIAN_POINT ( 'NONE',  ( -8.056626385452181793, -4.999999999999978684, -15.81257860883812327 ) ) ;
#10009 = CARTESIAN_POINT ( 'NONE',  ( -30.80805190526311321, 8.074044156869284450, -41.40902236837665384 ) ) ;
#10010 = CARTESIAN_POINT ( 'NONE',  ( 17.51469545665185024, 50.00000000000001421, 63.29293518440665167 ) ) ;
#10011 = CARTESIAN_POINT ( 'NONE',  ( 65.52222222222222570, 3.309500000000014541, 0.000000000000000000 ) ) ;
#10012 = ADVANCED_FACE ( 'NONE', ( #69909, #63429 ), #69386, .T. ) ;
#10013 =( NAMED_UNIT ( * ) PLANE_ANGLE_UNIT ( ) SI_UNIT ( $, .RADIAN. ) );
#10014 = PRESENTATION_STYLE_ASSIGNMENT (( #817 ) ) ;
#10015 = AXIS2_PLACEMENT_3D ( 'NONE', #28407, #1543, #37031 ) ;
#10016 = CARTESIAN_POINT ( 'NONE',  ( 106.6793784964389289, -14.21045842199433729, 163.7934217252150972 ) ) ;
#10017 = CARTESIAN_POINT ( 'NONE',  ( -81.98242152828360929, -32.56195222614032758, 150.9971016278573188 ) ) ;
#10018 = ORIENTED_EDGE ( 'NONE', *, *, #10109, .T. ) ;
#10019 = FACE_OUTER_BOUND ( 'NONE', #53870, .T. ) ;
#10020 = CARTESIAN_POINT ( 'NONE',  ( 4.656749229489900443, 251.3176040812644203, -3.785628640239131038 ) ) ;
#10021 = CARTESIAN_POINT ( 'NONE',  ( -0.8750000000009734435, -70.58759490697451611, 13.02737050516266315 ) ) ;
#10022 = CARTESIAN_POINT ( 'NONE',  ( 7.000000000000000000, 0.000000000000000000, -13.00000000000000000 ) ) ;
#10024 = CONICAL_SURFACE ( 'NONE', #104717, 3.309500000000007880, 0.9599310885968770357 ) ;
#10023 = CARTESIAN_POINT ( 'NONE',  ( 37.68814790064792675, 414.9506305060368163, 6.370022659008212074 ) ) ;
#10025 = DIRECTION ( 'NONE',  ( -1.000000000000000000, -1.224606353822377258E-16, -0.000000000000000000 ) ) ;
#10026 = ORIENTED_EDGE ( 'NONE', *, *, #33603, .F. ) ;
#10027 = CARTESIAN_POINT ( 'NONE',  ( -23.17317412221422046, 304.6499743691934441, 10.11024954114910024 ) ) ;
#10028 = EDGE_CURVE ( 'NONE', #78219, #90250, #102553, .T. ) ;
#10029 = ORIENTED_EDGE ( 'NONE', *, *, #59904, .T. ) ;
#10030 = CARTESIAN_POINT ( 'NONE',  ( 51.01037695545453232, 450.0000000000002274, 18.20242257375371153 ) ) ;
#10031 = EDGE_CURVE ( 'NONE', #26535, #58364, #51490, .T. ) ;
#10032 = DIRECTION ( 'NONE',  ( -1.000000000000000000, -1.224606353822377258E-16, -0.000000000000000000 ) ) ;
#10033 = CARTESIAN_POINT ( 'NONE',  ( 32.73605680485899683, 486.1418706179427431, 5.972480793486623973 ) ) ;
#10034 = CARTESIAN_POINT ( 'NONE',  ( -5.388845162059435978, 41.63012960719941447, -58.67906650638375510 ) ) ;
#10035 = DIRECTION ( 'NONE',  ( 0.000000000000000000, 0.000000000000000000, 1.000000000000000000 ) ) ;
#10036 = CARTESIAN_POINT ( 'NONE',  ( 96.28888888888889142, 1.023464760207051730E-14, 0.000000000000000000 ) ) ;
#10037 = ORIENTED_EDGE ( 'NONE', *, *, #60908, .T. ) ;
#10038 = CARTESIAN_POINT ( 'NONE',  ( 107.4330949502293464, -60.00000000000000000, 196.5277503695512564 ) ) ;
#10040 = CARTESIAN_POINT ( 'NONE',  ( 21.68997527405830184, -53.39465657004741672, 33.52469154556025188 ) ) ;
#10039 = CARTESIAN_POINT ( 'NONE',  ( -81.96434049221993234, -29.99999999999993250, 194.6677479149438454 ) ) ;
#10042 = CARTESIAN_POINT ( 'NONE',  ( 43.30868969682389036, 1.340359594676612611E-15, 0.000000000000000000 ) ) ;
#10041 = PRODUCT_DEFINITION_CONTEXT ( 'detailed design', #84455, 'design' ) ;
#10043 = DIRECTION ( 'NONE',  ( 0.000000000000000000, -0.9459915920726907901, 0.3241911592375332218 ) ) ;
#10044 = AXIS2_PLACEMENT_3D ( 'NONE', #29349, #39539, #70308 ) ;
#10045 = CARTESIAN_POINT ( 'NONE',  ( -41.95185451917502206, -60.25535463032460370, 45.28364850313863599 ) ) ;
#10046 = CARTESIAN_POINT ( 'NONE',  ( -30.95568101992225252, 18.64284798593066483, 22.77427805267372563 ) ) ;
#10047 = UNCERTAINTY_MEASURE_WITH_UNIT (LENGTH_MEASURE( 1.000000000000000082E-05 ), #87876, 'distance_accuracy_value', 'NONE');
#10048 = EDGE_LOOP ( 'NONE', ( #28503, #4995, #42626, #845 ) ) ;
#10049 =( NAMED_UNIT ( * ) SI_UNIT ( $, .STERADIAN. ) SOLID_ANGLE_UNIT ( ) );
#10050 = CARTESIAN_POINT ( 'NONE',  ( 33.00496812083888898, 465.6658704666191966, 15.15901827093884258 ) ) ;
#10051 = CARTESIAN_POINT ( 'NONE',  ( 30.35537264529554946, 338.7115663565144246, 18.05293407820170515 ) ) ;
#10052 = CARTESIAN_POINT ( 'NONE',  ( 62.33904886068935980, 6.975173280561618775E-15, 0.000000000000000000 ) ) ;
#10053 = DIRECTION ( 'NONE',  ( -1.000000000000000000, -1.224606353822377258E-16, -0.000000000000000000 ) ) ;
#10054 = ORIENTED_EDGE ( 'NONE', *, *, #40089, .T. ) ;
#10055 = CARTESIAN_POINT ( 'NONE',  ( -16.18722300313207896, 37.20509570188509940, -21.93860808728204859 ) ) ;
#10056 = AXIS2_PLACEMENT_3D ( 'NONE', #17819, #51212, #34022 ) ;
#10057 = ORIENTED_EDGE ( 'NONE', *, *, #82323, .T. ) ;
#10058 = CARTESIAN_POINT ( 'NONE',  ( 81.06325062923930602, -30.00000000000000000, 2.799235988874741565 ) ) ;
#10059 = CARTESIAN_POINT ( 'NONE',  ( 46.77684132781884330, 13.57955522726353692, 15.57752954476143437 ) ) ;
#10060 = CARTESIAN_POINT ( 'NONE',  ( 0.000000000000000000, 0.000000000000000000, 0.000000000000000000 ) ) ;
#10061 = CARTESIAN_POINT ( 'NONE',  ( 41.08349330513380693, -7.703719777548943412E-31, 4.000000000000001776 ) ) ;
#10062 = CARTESIAN_POINT ( 'NONE',  ( 80.82096024282435565, -30.00000000000000000, 17.00536050008537003 ) ) ;
#10063 = CARTESIAN_POINT ( 'NONE',  ( -24.31638901882701020, 305.3158659931349916, 10.26002132804774192 ) ) ;
#10064 = ORIENTED_EDGE ( 'NONE', *, *, #5026, .F. ) ;
#10065 = EDGE_LOOP ( 'NONE', ( #82426, #9264, #53820, #37049 ) ) ;
#10066 = ORIENTED_EDGE ( 'NONE', *, *, #46407, .T. ) ;
#10067 = CIRCLE ( 'NONE', #60059, 4.000000000000000888 ) ;
#10068 = CARTESIAN_POINT ( 'NONE',  ( -47.14545574308343845, 12.03700443135205056, -16.50078943917375796 ) ) ;
#10069 = CARTESIAN_POINT ( 'NONE',  ( -36.58584895476980847, 25.86851599530958268, -12.99742464195551150 ) ) ;
#10070 = AXIS2_PLACEMENT_3D ( 'NONE', #10676, #101308, #43592 ) ;
#10071 = CARTESIAN_POINT ( 'NONE',  ( 33.99969272045851199, 439.9157840834117223, 24.30689657658924574 ) ) ;
#10073 = CONICAL_SURFACE ( 'NONE', #77453, 3.309500000000007880, 0.9599310885968770357 ) ;
#10072 = CARTESIAN_POINT ( 'NONE',  ( -32.18022093138533535, 410.2521187074748354, 25.67972843377013703 ) ) ;
#10074 = FILL_AREA_STYLE_COLOUR ( '', #13939 ) ;
#10075 = VERTEX_POINT ( 'NONE', #87162 ) ;
#10077 = EDGE_CURVE ( 'NONE', #78587, #68971, #9523, .T. ) ;
#10076 = CARTESIAN_POINT ( 'NONE',  ( -2.617478844990396514, 50.00000000000001421, -94.73972676610910071 ) ) ;
#10078 = ORIENTED_EDGE ( 'NONE', *, *, #89855, .F. ) ;
#10079 = CARTESIAN_POINT ( 'NONE',  ( 0.000000000000000000, 0.000000000000000000, 5.000000000000000888 ) ) ;
#10080 = CARTESIAN_POINT ( 'NONE',  ( 77.53117718845349771, -38.51705233716531751, 186.5868546221014412 ) ) ;
#10081 = DIRECTION ( 'NONE',  ( 0.000000000000000000, 0.000000000000000000, -1.000000000000000000 ) ) ;
#10082 = CARTESIAN_POINT ( 'NONE',  ( 26.54313204476279253, 306.2751507266256681, 10.71856527558073857 ) ) ;
#10083 = MECHANICAL_DESIGN_GEOMETRIC_PRESENTATION_REPRESENTATION (  '', ( #101322 ), #94482 ) ;
#10084 = CARTESIAN_POINT ( 'NONE',  ( 21.08349330513380337, 4.000000000000002665, 0.000000000000000000 ) ) ;
#10085 = EDGE_LOOP ( 'NONE', ( #25788, #34366 ) ) ;
#10086 = CARTESIAN_POINT ( 'NONE',  ( 95.42421628608209971, 5.000000000000020428, 0.000000000000000000 ) ) ;
#10087 = CARTESIAN_POINT ( 'NONE',  ( 40.36332270526656174, 321.1565039326854389, 8.346576249228172983 ) ) ;
#10088 = EDGE_CURVE ( 'NONE', #101318, #75872, #45118, .T. ) ;
#10089 = CARTESIAN_POINT ( 'NONE',  ( -4.551587301587297851, -48.79941684889506348, 104.4018401814738013 ) ) ;
#10090 = CARTESIAN_POINT ( 'NONE',  ( 15.39795322966678981, 3.054092008340477449, -2.852131183220913080 ) ) ;
#10091 = VERTEX_POINT ( 'NONE', #102810 ) ;
#10092 = DIRECTION ( 'NONE',  ( -1.000000000000000000, -0.000000000000000000, -0.000000000000000000 ) ) ;
#10093 = CARTESIAN_POINT ( 'NONE',  ( 4.678819457397413117, 143.9212778189090898, 0.000000000000000000 ) ) ;
#10094 = DIRECTION ( 'NONE',  ( -1.000000000000000000, -1.224606353822377258E-16, -0.000000000000000000 ) ) ;
#10095 = CARTESIAN_POINT ( 'NONE',  ( 32.33349330513379982, -4.000000000000000888, 4.898587196589416773E-16 ) ) ;
#10096 = FACE_OUTER_BOUND ( 'NONE', #64238, .T. ) ;
#10097 = AXIS2_PLACEMENT_3D ( 'NONE', #28330, #68229, #75780 ) ;
#10098 = LINE ( 'NONE', #100171, #39846 ) ;
#10099 = CARTESIAN_POINT ( 'NONE',  ( 84.89364056863026065, -50.19228796424612682, 188.9982818557025723 ) ) ;
#10100 = VECTOR ( 'NONE', #53201, 1000.000000000000000 ) ;
#10101 = SURFACE_STYLE_USAGE ( .BOTH. , #100699 ) ;
#10102 = ADVANCED_FACE ( 'NONE', ( #71482, #78515 ), #37042, .T. ) ;
#10103 = CARTESIAN_POINT ( 'NONE',  ( -8.745545711797721111, 132.0170111787107317, 5.000000000000635936 ) ) ;
#10104 = VERTEX_POINT ( 'NONE', #94188 ) ;
#10105 = CARTESIAN_POINT ( 'NONE',  ( -8.559508646656370345, -1.200000000000000030E-05, 2.781152949374564365 ) ) ;
#10106 = CARTESIAN_POINT ( 'NONE',  ( 0.000000000000000000, 0.000000000000000000, -4.000000000000000000 ) ) ;
#10107 = CARTESIAN_POINT ( 'NONE',  ( 16.18602784294493802, 35.07682394434411322, -21.93920426711484950 ) ) ;
#10108 = SURFACE_STYLE_FILL_AREA ( #25821 ) ;
#10109 = EDGE_CURVE ( 'NONE', #65330, #31480, #17632, .T. ) ;
#10110 = CARTESIAN_POINT ( 'NONE',  ( -86.92488039023091062, -30.00000000000000711, 70.05807166599328184 ) ) ;
#10111 = CIRCLE ( 'NONE', #63573, 5.000000000000010658 ) ;
#10112 = CARTESIAN_POINT ( 'NONE',  ( 8.099999999999999645, 3.752776749732562589, -6.500000000000000888 ) ) ;
#10113 = CARTESIAN_POINT ( 'NONE',  ( 1.224646799147353454E-15, -6.505213034913025026E-15, 10.00000000000000178 ) ) ;
#10114 = CARTESIAN_POINT ( 'NONE',  ( -7.169303301815157958, 4.521054846639327884, -7.349897473155612815 ) ) ;
#10116 = DIRECTION ( 'NONE',  ( 0.000000000000000000, 1.000000000000000000, 0.000000000000000000 ) ) ;
#10115 = CARTESIAN_POINT ( 'NONE',  ( -10.00005432054558341, 245.9998641986207701, 0.2621623937322782871 ) ) ;
#10117 = CARTESIAN_POINT ( 'NONE',  ( 1.637502573363885733E-19, 51.26930509877138320, -10.24999999999999822 ) ) ;
#10118 = DIRECTION ( 'NONE',  ( -0.000000000000000000, -0.000000000000000000, 1.000000000000000000 ) ) ;
#10119 = CARTESIAN_POINT ( 'NONE',  ( -35.64643974835908580, 491.6938676210187396, 12.49042095397502372 ) ) ;
#10120 = CARTESIAN_POINT ( 'NONE',  ( 4.905194654929173836, -82.97605604980155647, 3.459476078998853676 ) ) ;
#10121 = DIRECTION ( 'NONE',  ( 0.000000000000000000, -1.000000000000000000, 0.000000000000000000 ) ) ;
#10122 = CARTESIAN_POINT ( 'NONE',  ( 43.48294143132324763, 479.1558696509461015, 6.034796630239570803 ) ) ;
#10123 = CARTESIAN_POINT ( 'NONE',  ( 56.17098950358883513, -28.68981958306524049, -26.22444997023189828 ) ) ;
#10124 = AXIS2_PLACEMENT_3D ( 'NONE', #48179, #23417, #66494 ) ;
#10125 = EDGE_CURVE ( 'NONE', #73679, #69327, #61839, .T. ) ;
#10126 = CARTESIAN_POINT ( 'NONE',  ( -25.43960792238905100, -22.08944486031660759, 28.86612087644610725 ) ) ;
#10127 = EDGE_LOOP ( 'NONE', ( #22857, #190, #38734, #60532, #97023, #67420, #58974, #68190, #91879, #15491 ) ) ;
#10128 = CARTESIAN_POINT ( 'NONE',  ( 16.36650669486618881, 4.898587196589411843E-16, -4.000000000000000888 ) ) ;
#10129 = CARTESIAN_POINT ( 'NONE',  ( -9.989435848181784650, 108.9738029252842466, -0.5278651953176012324 ) ) ;
#10130 = CARTESIAN_POINT ( 'NONE',  ( -10.28624191511820207, 45.38549880562041494, 15.40779740156164124 ) ) ;
#10131 = CARTESIAN_POINT ( 'NONE',  ( -65.27364549594882703, -29.77031089310590772, -22.95100066570442010 ) ) ;
#10132 = LINE ( 'NONE', #58146, #11219 ) ;
#10133 = EDGE_LOOP ( 'NONE', ( #997, #9347, #82640, #56830, #44651 ) ) ;
#10134 = CARTESIAN_POINT ( 'NONE',  ( -35.61562608342421044, 436.8850424094961227, 4.737375314588414987 ) ) ;
#10135 = ORIENTED_EDGE ( 'NONE', *, *, #39007, .F. ) ;
#10136 = SURFACE_STYLE_FILL_AREA ( #44654 ) ;
#10137 = CARTESIAN_POINT ( 'NONE',  ( 16.01537386455376932, 3.832633078742941457, 1.292357405299655815 ) ) ;
#10138 = CARTESIAN_POINT ( 'NONE',  ( -97.47674776263787066, -60.00000000000000000, 196.6139650356533934 ) ) ;
#10139 = ORIENTED_EDGE ( 'NONE', *, *, #77742, .T. ) ;
#10140 = SURFACE_SIDE_STYLE ('',( #76463 ) ) ;
#10141 = DIRECTION ( 'NONE',  ( 1.871721906610600077E-16, 0.000000000000000000, -1.000000000000000000 ) ) ;
#10142 = CARTESIAN_POINT ( 'NONE',  ( 102.4337014127728054, -60.18830211168408084, 193.6666088890698632 ) ) ;
#10144 = CARTESIAN_POINT ( 'NONE',  ( -6.928203230275509661, -9.735207327464285854, 3.999999999999999112 ) ) ;
#10143 = CARTESIAN_POINT ( 'NONE',  ( -6.750000000000018652, 11.69134295108991317, -13.00000000000000000 ) ) ;
#10145 = VERTEX_POINT ( 'NONE', #13243 ) ;
#10146 = ORIENTED_EDGE ( 'NONE', *, *, #797, .F. ) ;
#10147 = EDGE_CURVE ( 'NONE', #89487, #9727, #77997, .T. ) ;
#10148 = ORIENTED_EDGE ( 'NONE', *, *, #77919, .T. ) ;
#10149 = CARTESIAN_POINT ( 'NONE',  ( 31.69611817388674879, 348.2576632951648890, 20.17743617868276473 ) ) ;
#10150 = EDGE_CURVE ( 'NONE', #55214, #85106, #96321, .T. ) ;
#10151 = CARTESIAN_POINT ( 'NONE',  ( 31.08349330513380693, 1.593028355512270962E-15, 0.000000000000000000 ) ) ;
#10152 = CARTESIAN_POINT ( 'NONE',  ( 9.381644744338347053, 53.45431541546333420, 3.726433245770410796 ) ) ;
#10153 = VERTEX_POINT ( 'NONE', #70444 ) ;
#10154 = CARTESIAN_POINT ( 'NONE',  ( 83.28888888888889142, 4.172000000000019249, 0.000000000000000000 ) ) ;
#10155 = FACE_OUTER_BOUND ( 'NONE', #89397, .T. ) ;
#10156 = DIRECTION ( 'NONE',  ( 1.000000000000000000, -0.000000000000000000, -0.000000000000000000 ) ) ;
#10157 = CARTESIAN_POINT ( 'NONE',  ( -42.46252528007325111, -57.68686955033432895, 59.97785686028149854 ) ) ;
#10158 = CARTESIAN_POINT ( 'NONE',  ( 6.928203230275509661, -65.26479267253573369, 4.000000000000002665 ) ) ;
#10159 = CARTESIAN_POINT ( 'NONE',  ( -32.11411341898570981, 317.7919323371296514, -6.873671351699469412 ) ) ;
#10160 = CARTESIAN_POINT ( 'NONE',  ( -6.943035977205679110, 41.50417750172036335, -58.81491712266881677 ) ) ;
#10161 = EDGE_CURVE ( 'NONE', #61495, #7932, #103340, .T. ) ;
#10162 = CARTESIAN_POINT ( 'NONE',  ( -89.98348853342757536, -29.99999999999992184, -2.848863062743723695 ) ) ;
#10163 = CARTESIAN_POINT ( 'NONE',  ( -7.943779790039141808, 51.78215888541748768, 3.880567839249599693 ) ) ;
#10164 = CARTESIAN_POINT ( 'NONE',  ( -49.92868248732877134, -22.20187048435544241, 44.97503486679070761 ) ) ;
#10165 = DIRECTION ( 'NONE',  ( 0.000000000000000000, 1.000000000000000000, 0.000000000000000000 ) ) ;
#10166 = ORIENTED_EDGE ( 'NONE', *, *, #73204, .F. ) ;
#10167 = CARTESIAN_POINT ( 'NONE',  ( 12.50000000000000000, 14.91295971516869301, -32.73279170529961846 ) ) ;
#10168 = CARTESIAN_POINT ( 'NONE',  ( -7.742691193564556151, 302.4167829614867742, -10.02995440365129021 ) ) ;
#10169 = CARTESIAN_POINT ( 'NONE',  ( 15.75700568575396865, -1.458561159084935221, 14.93088058109044169 ) ) ;
#10170 = ORIENTED_EDGE ( 'NONE', *, *, #30121, .F. ) ;
#10171 = CARTESIAN_POINT ( 'NONE',  ( 75.66773936237699161, -38.35839768494054880, 175.7330108619280793 ) ) ;
#10172 = CARTESIAN_POINT ( 'NONE',  ( 48.15057074821019256, 16.50253122541073125, 14.35535821593427386 ) ) ;
#10173 = CARTESIAN_POINT ( 'NONE',  ( 5.799999999999999822, 9.237604307034018802, 0.000000000000000000 ) ) ;
#10174 = CARTESIAN_POINT ( 'NONE',  ( -16.30160124920373477, 294.5672738068976741, 9.876520238985763811 ) ) ;
#10175 = CARTESIAN_POINT ( 'NONE',  ( -79.13121736037271603, 42.00000000000000000, 45.60838156032633606 ) ) ;
#10176 = CARTESIAN_POINT ( 'NONE',  ( 91.68272017985721334, -30.00000000000000711, 190.7589576344717557 ) ) ;
#10177 =( BOUNDED_SURFACE ( )  B_SPLINE_SURFACE ( 3, 2, ( 
 ( #3356, #70211, #103633 ),
 ( #95547, #62145, #21174 ),
 ( #45939, #102037, #78818 ),
 ( #85334, #29785, #4950 ),
 ( #21691, #54524, #46466 ),
 ( #93964, #19587, #11419 ),
 ( #77240, #20114, #7050 ),
 ( #80402, #64769, #72326 ),
 ( #87994, #97126, #46981 ),
 ( #23811, #63189, #79879 ),
 ( #57185, #48031, #96612 ),
 ( #80939, #15148, #22748 ),
 ( #105230, #7569, #32426 ),
 ( #56656, #39967, #56110 ),
 ( #64256, #40486, #73365 ),
 ( #89581, #72838, #49089 ),
 ( #71261, #105749, #106264 ),
 ( #15674, #104155, #88523 ),
 ( #14597, #63728, #23266 ),
 ( #65296, #5985, #98187 ),
 ( #16207, #6515, #39449 ),
 ( #31885, #30301, #48564 ),
 ( #55585, #38396, #14072 ),
 ( #89045, #24342, #22214 ),
 ( #47510, #97644, #81455 ),
 ( #90101, #31375, #96082 ),
 ( #81991, #55064, #38914 ),
 ( #71781, #104690, #30842 ),
 ( #27002, #59883, #8644 ),
 ( #18913, #91706, #73904 ),
 ( #34561, #42077, #50169 ),
 ( #42607, #9163, #49634 ),
 ( #66351, #67435, #25404 ),
 ( #84141, #74960, #10238 ),
 ( #17823, #99236, #26472 ),
 ( #43152, #2131, #76035 ),
 ( #50674, #25953, #99784 ),
 ( #35085, #67955, #58813 ),
 ( #9697, #51758, #1599 ),
 ( #83072, #100838, #41548 ),
 ( #92756, #100310, #82540 ),
 ( #33478, #34027, #83589 ),
 ( #74434, #1052, #513 ),
 ( #8109, #58264, #59343 ),
 ( #66900, #75505, #91188 ),
 ( #41023, #17295, #49063 ),
 ( #51215, #32955, #65825 ),
 ( #92207, #98704, #24859 ),
 ( #18364, #57709, #90636 ),
 ( #16744, #102447, #36694 ),
 ( #84672, #85755, #77108 ),
 ( #61475, #86288, #19454 ),
 ( #37211, #93298, #78683 ),
 ( #52827, #94368, #94906 ),
 ( #12886, #43673, #62529 ),
 ( #11828, #21555, #85199 ),
 ( #53369, #76561, #44758 ),
 ( #60420, #52289, #69557 ),
 ( #68499, #4817, #101908 ),
 ( #45284, #21046, #28592 ),
 ( #2672, #4283, #20531 ),
 ( #78164, #45807, #12360 ),
 ( #29657, #3224, #69034 ),
 ( #70080, #10756, #35624 ),
 ( #101390, #19982, #102982 ),
 ( #77646, #27541, #29143 ),
 ( #53881, #62013, #11284 ),
 ( #60939, #103505, #86813 ),
 ( #95415, #37753, #44217 ),
 ( #36166, #93829, #3762 ),
 ( #70615, #28066, #40356 ),
 ( #15010, #14467, #105105 ),
 ( #80809, #46338, #6923 ),
 ( #30168, #87337, #31245 ),
 ( #63599, #31758, #13414 ),
 ( #39845, #104558, #79753 ),
 ( #64134, #48439, #22081 ),
 ( #95956, #54936, #89454 ),
 ( #15546, #97003, #105619 ),
 ( #87864, #54391, #23142 ),
 ( #88393, #72201, #38785 ),
 ( #23675, #55982, #5859 ),
 ( #72717, #71652, #13947 ),
 ( #47382, #56524, #88917 ),
 ( #65164, #96486, #55461 ),
 ( #22629, #79226, #73234 ) ),
 .UNSPECIFIED., .F., .F., .T. ) 
 B_SPLINE_SURFACE_WITH_KNOTS ( ( 4, 2, 2, 2, 2, 2, 2, 2, 2, 2, 2, 2, 2, 2, 2, 2, 2, 2, 2, 2, 2, 2, 2, 2, 2, 2, 2, 2, 2, 2, 2, 2, 2, 2, 2, 2, 2, 2, 2, 2, 2, 2, 4 ),
 ( 3, 3 ),
 ( 0.02634172422113034359, 0.02840705912624018337, 0.03047239403135001967, 0.03253772893645985598, 0.03357039638901477413, 0.03460306384156969228, 0.03666839874667952859, 0.03873373365178936489, 0.04079906855689920120, 0.04183173600945411935, 0.04286440346200903750, 0.04389707091456395566, 0.04492973836711887381, 0.04699507327222871012, 0.04906040817733854642, 0.05112574308244838273, 0.05215841053500330088, 0.05319107798755821903, 0.05525641289266805534, 0.05628908034522297349, 0.05732174779777789164, 0.05938708270288772795, 0.06145241760799756425, 0.06351775251310740056, 0.06455041996566232565, 0.06558308741821723686, 0.06661575487077214808, 0.06764842232332707317, 0.06971375722843690947, 0.07074642468099182069, 0.07177909213354674578, 0.07384442703865658209, 0.07487709449121149330, 0.07590976194376641839, 0.07797509684887625470, 0.08004043175398609100, 0.08210576665909592731, 0.08417110156420576361, 0.08623643646931559992, 0.08830177137442543622, 0.08933443882698036131, 0.09036710627953527253, 0.09243244118464510883 ),
 ( 0.000000000000000000, 1.000000000000000000 ),
 .UNSPECIFIED. ) 
 GEOMETRIC_REPRESENTATION_ITEM ( )  RATIONAL_B_SPLINE_SURFACE ( (
 ( 1.000000000000000000, 0.7574005004452331047, 1.000000000000000000),
 ( 1.000000000000000000, 0.7678086279399819469, 1.000000000000000000),
 ( 1.000000000000000000, 0.7789244113962565663, 1.000000000000000000),
 ( 1.000000000000000000, 0.8016316046185457678, 1.000000000000000000),
 ( 1.000000000000000000, 0.8132948587418985520, 1.000000000000000000),
 ( 1.000000000000000000, 0.8357926363597657504, 1.000000000000000000),
 ( 1.000000000000000000, 0.8466816614498698934, 1.000000000000000000),
 ( 1.000000000000000000, 0.8621003063894946417, 1.000000000000000000),
 ( 1.000000000000000000, 0.8670881561880485755, 1.000000000000000000),
 ( 1.000000000000000000, 0.8766998973978601395, 1.000000000000000000),
 ( 1.000000000000000000, 0.8813097246197982848, 1.000000000000000000),
 ( 1.000000000000000000, 0.8943093724793236277, 1.000000000000000000),
 ( 1.000000000000000000, 0.9019441283705564860, 1.000000000000000000),
 ( 1.000000000000000000, 0.9147276970316240430, 1.000000000000000000),
 ( 1.000000000000000000, 0.9198874818270340592, 1.000000000000000000),
 ( 1.000000000000000000, 0.9267810911149524378, 1.000000000000000000),
 ( 1.000000000000000000, 0.9285972973398308739, 1.000000000000000000),
 ( 1.000000000000000000, 0.9286317451279045843, 1.000000000000000000),
 ( 1.000000000000000000, 0.9281858723822534740, 1.000000000000000000),
 ( 1.000000000000000000, 0.9264403244317799269, 1.000000000000000000),
 ( 1.000000000000000000, 0.9251417076504168113, 1.000000000000000000),
 ( 1.000000000000000000, 0.9217459610402344294, 1.000000000000000000),
 ( 1.000000000000000000, 0.9196487206541981152, 1.000000000000000000),
 ( 1.000000000000000000, 0.9146973172701069466, 1.000000000000000000),
 ( 1.000000000000000000, 0.9118257467883083001, 1.000000000000000000),
 ( 1.000000000000000000, 0.9023115364206620859, 1.000000000000000000),
 ( 1.000000000000000000, 0.8947616380145678727, 1.000000000000000000),
 ( 1.000000000000000000, 0.8778037105062616030, 1.000000000000000000),
 ( 1.000000000000000000, 0.8683411594436707404, 1.000000000000000000),
 ( 1.000000000000000000, 0.8486622380153294731, 1.000000000000000000),
 ( 1.000000000000000000, 0.8383870565666979857, 1.000000000000000000),
 ( 1.000000000000000000, 0.8228778961941588532, 1.000000000000000000),
 ( 1.000000000000000000, 0.8176744109529193727, 1.000000000000000000),
 ( 1.000000000000000000, 0.8074431182712563659, 1.000000000000000000),
 ( 1.000000000000000000, 0.8024440009126241335, 1.000000000000000000),
 ( 1.000000000000000000, 0.7879812762414096783, 1.000000000000000000),
 ( 1.000000000000000000, 0.7790450003668998313, 1.000000000000000000),
 ( 1.000000000000000000, 0.7675477608643064276, 1.000000000000000000),
 ( 1.000000000000000000, 0.7640348910737623234, 1.000000000000000000),
 ( 1.000000000000000000, 0.7578134264054862124, 1.000000000000000000),
 ( 1.000000000000000000, 0.7551270526901607827, 1.000000000000000000),
 ( 1.000000000000000000, 0.7486526966700658425, 1.000000000000000000),
 ( 1.000000000000000000, 0.7463801361677054880, 1.000000000000000000),
 ( 1.000000000000000000, 0.7463127164022264060, 1.000000000000000000),
 ( 1.000000000000000000, 0.7486000928341679517, 1.000000000000000000),
 ( 1.000000000000000000, 0.7571961929099836341, 1.000000000000000000),
 ( 1.000000000000000000, 0.7634567568201346965, 1.000000000000000000),
 ( 1.000000000000000000, 0.7750654466030536538, 1.000000000000000000),
 ( 1.000000000000000000, 0.7793053813432258004, 1.000000000000000000),
 ( 1.000000000000000000, 0.7882146539232089966, 1.000000000000000000),
 ( 1.000000000000000000, 0.7929022008513715303, 1.000000000000000000),
 ( 1.000000000000000000, 0.8025966256814718314, 1.000000000000000000),
 ( 1.000000000000000000, 0.8076036615378768824, 1.000000000000000000),
 ( 1.000000000000000000, 0.8178083114314877999, 1.000000000000000000),
 ( 1.000000000000000000, 0.8230260163010280072, 1.000000000000000000),
 ( 1.000000000000000000, 0.8386284071981864319, 1.000000000000000000),
 ( 1.000000000000000000, 0.8489266526250032197, 1.000000000000000000),
 ( 1.000000000000000000, 0.8636680828574543334, 1.000000000000000000),
 ( 1.000000000000000000, 0.8684659181649216908, 1.000000000000000000),
 ( 1.000000000000000000, 0.8777487523221890742, 1.000000000000000000),
 ( 1.000000000000000000, 0.8822506950759456679, 1.000000000000000000),
 ( 1.000000000000000000, 0.8950015522441460147, 1.000000000000000000),
 ( 1.000000000000000000, 0.9025191533021075241, 1.000000000000000000),
 ( 1.000000000000000000, 0.9119467452851578448, 1.000000000000000000),
 ( 1.000000000000000000, 0.9147804332722992982, 1.000000000000000000),
 ( 1.000000000000000000, 0.9197485997668242153, 1.000000000000000000),
 ( 1.000000000000000000, 0.9218702435470463863, 1.000000000000000000),
 ( 1.000000000000000000, 0.9269502648627369057, 1.000000000000000000),
 ( 1.000000000000000000, 0.9286883261994179906, 1.000000000000000000),
 ( 1.000000000000000000, 0.9285486022662473582, 1.000000000000000000),
 ( 1.000000000000000000, 0.9266646312235611305, 1.000000000000000000),
 ( 1.000000000000000000, 0.9196578271540671867, 1.000000000000000000),
 ( 1.000000000000000000, 0.9144563017674409711, 1.000000000000000000),
 ( 1.000000000000000000, 0.9016091177945602109, 1.000000000000000000),
 ( 1.000000000000000000, 0.8939535693208001677, 1.000000000000000000),
 ( 1.000000000000000000, 0.8766021895685242038, 1.000000000000000000),
 ( 1.000000000000000000, 0.8668555216837416921, 1.000000000000000000),
 ( 1.000000000000000000, 0.8462716989656902111, 1.000000000000000000),
 ( 1.000000000000000000, 0.8353730651404011054, 1.000000000000000000),
 ( 1.000000000000000000, 0.8184904932442989001, 1.000000000000000000),
 ( 1.000000000000000000, 0.8127516586172595092, 1.000000000000000000),
 ( 1.000000000000000000, 0.8012917549111018278, 1.000000000000000000),
 ( 1.000000000000000000, 0.7955843342310977562, 1.000000000000000000),
 ( 1.000000000000000000, 0.7786720583377687577, 1.000000000000000000),
 ( 1.000000000000000000, 0.7676722966783382507, 1.000000000000000000),
 ( 1.000000000000000000, 0.7574005004457203816, 1.000000000000000000) ) ) 
 REPRESENTATION_ITEM ( '' )  SURFACE ( )  );
#10178 = B_SPLINE_CURVE_WITH_KNOTS ( 'NONE', 3,
 ( #73829, #82992, #17739, #106723, #50599, #34486, #8563, #432, #75425, #1518, #41464, #41996, #49552, #59263, #50086, #98629, #74354, #99159, #82459, #33401, #9087, #43072, #57105, #66272, #25317, #84055, #74876, #33944, #67353, #40935 ),
 .UNSPECIFIED., .F., .F.,
 ( 4, 2, 2, 2, 2, 2, 2, 2, 2, 2, 2, 2, 2, 2, 4 ),
 ( 0.008103130636685088387, 0.008563624816068822476, 0.009024118995452558301, 0.009945107354220028215, 0.01086609571298749813, 0.01178708407175496631, 0.01270807243052244143, 0.01316856660990617899, 0.01362906078928991654, 0.01408955496867365237, 0.01431980205836551334, 0.01455004914805737085, 0.01478029623774923182, 0.01501054332744109106, 0.01547103750682481647 ),
 .UNSPECIFIED. ) ;
#10179 = B_SPLINE_SURFACE_WITH_KNOTS ( 'NONE', 1, 3, ( 
 ( #27332, #60730, #37539, #69871, #35407, #68275, #70405, #61802 ),
 ( #103303, #19773, #94696, #101171, #69351, #52602, #85531, #11610 ) ),
 .UNSPECIFIED., .F., .F., .F.,
 ( 2, 2 ),
 ( 4, 2, 2, 4 ),
 ( 0.000000000000000000, 1.000000000000000000 ),
 ( 0.000000000000000000, 0.04450745600790868145, 0.06676118401186306728, 0.08901491201581737678 ),
 .UNSPECIFIED. ) ;
#10180 = CARTESIAN_POINT ( 'NONE',  ( 0.1691555275570714445, 46.21383923812596350, -16.25000000000000000 ) ) ;
#10181 = DIRECTION ( 'NONE',  ( 0.5735764363510490460, 0.8191520442889896891, 0.000000000000000000 ) ) ;
#10182 = AXIS2_PLACEMENT_3D ( 'NONE', #28573, #21033, #86799 ) ;
#10183 = ORIENTED_EDGE ( 'NONE', *, *, #85721, .T. ) ;
#10184 = ORIENTED_EDGE ( 'NONE', *, *, #78866, .F. ) ;
#10185 = CARTESIAN_POINT ( 'NONE',  ( 51.13096205315856224, -25.65380906861201993, 47.91585540195683990 ) ) ;
#10186 = CARTESIAN_POINT ( 'NONE',  ( -44.14412608174431085, 435.2201606271638639, 14.45841244836588757 ) ) ;
#10187 = CARTESIAN_POINT ( 'NONE',  ( -7.500000000000007105, 42.00000000000000711, -58.69229087761262065 ) ) ;
#10188 = ORIENTED_EDGE ( 'NONE', *, *, #41546, .T. ) ;
#10190 = EDGE_CURVE ( 'NONE', #74794, #83609, #26288, .T. ) ;
#10189 = CARTESIAN_POINT ( 'NONE',  ( -91.21237190957077701, -38.40264986056752861, -11.26304677710397328 ) ) ;
#10191 = ORIENTED_EDGE ( 'NONE', *, *, #23188, .F. ) ;
#10192 = CARTESIAN_POINT ( 'NONE',  ( 14.95236164054155559, 4.204970931318847249, 5.179833178257711168 ) ) ;
#10193 = CARTESIAN_POINT ( 'NONE',  ( 108.2638565580548971, -38.35770216212828387, 192.2389173063952228 ) ) ;
#10194 = CARTESIAN_POINT ( 'NONE',  ( 13.42487756469949467, 22.38025266455044715, 3.525519932714368032 ) ) ;
#10195 = CARTESIAN_POINT ( 'NONE',  ( 86.75328224081307837, -60.14641367048189835, 26.71604830143463616 ) ) ;
#10196 = CARTESIAN_POINT ( 'NONE',  ( 34.99229983299962754, 435.2421343821194455, 7.288263853914603629 ) ) ;
#10197 = CARTESIAN_POINT ( 'NONE',  ( -9.739726766683153514, -3.000000000000002665, -82.38252115640719353 ) ) ;
#10198 = CARTESIAN_POINT ( 'NONE',  ( 2.789712857210963737, -9.223132490777652848, -12.21941282805324391 ) ) ;
#10199 = EDGE_CURVE ( 'NONE', #91282, #104078, #79057, .T. ) ;
#10200 = CYLINDRICAL_SURFACE ( 'NONE', #44365, 7.000000000000000000 ) ;
#10201 = DIRECTION ( 'NONE',  ( -1.000000000000000000, -0.000000000000000000, -0.000000000000000000 ) ) ;
#10202 = ORIENTED_EDGE ( 'NONE', *, *, #48668, .F. ) ;
#10203 = CARTESIAN_POINT ( 'NONE',  ( 62.81177132629515825, -25.58257438566387876, 72.96335641850546949 ) ) ;
#10204 = EDGE_CURVE ( 'NONE', #16577, #99841, #31427, .T. ) ;
#10205 = CARTESIAN_POINT ( 'NONE',  ( -13.00000000000003730, -85.00000000000000000, 4.000000000000001776 ) ) ;
#10206 = CYLINDRICAL_SURFACE ( 'NONE', #531, 10.00000000000000178 ) ;
#10207 = B_SPLINE_CURVE_WITH_KNOTS ( 'NONE', 3,
 ( #22776, #66383, #76064, #84175, #25985, #99814, #34059, #17857, #3258, #26508 ),
 .UNSPECIFIED., .F., .F.,
 ( 4, 2, 2, 2, 4 ),
 ( 0.000000000000000000, 0.5000000000000000000, 0.7500000000000000000, 0.8750000000000000000, 1.000000000000000000 ),
 .UNSPECIFIED. ) ;
#10208 = ORIENTED_EDGE ( 'NONE', *, *, #69262, .T. ) ;
#10209 = CARTESIAN_POINT ( 'NONE',  ( 4.551587301587293410, -48.79941684889506348, 104.4018401814738013 ) ) ;
#10210 = CARTESIAN_POINT ( 'NONE',  ( -42.78144316814210413, 391.1871488574614659, 19.62185425083864843 ) ) ;
#10211 = CARTESIAN_POINT ( 'NONE',  ( -32.80551872593252227, 486.0171861992462254, 5.671217483526080017 ) ) ;
#10212 = CARTESIAN_POINT ( 'NONE',  ( 58.92761780597729881, 4.000000000000015099, 4.898587196589422689E-16 ) ) ;
#10213 = CARTESIAN_POINT ( 'NONE',  ( -5.656854249492379694, -26.93749999999999645, -5.656854249492380582 ) ) ;
#10214 = CARTESIAN_POINT ( 'NONE',  ( 34.49754285437400370, -23.83101018980520180, 33.28975017431508121 ) ) ;
#10215 = VECTOR ( 'NONE', #22991, 1000.000000000000000 ) ;
#10216 = AXIS2_PLACEMENT_3D ( 'NONE', #103129, #45432, #78307 ) ;
#10217 = CIRCLE ( 'NONE', #68844, 3.400000000000000355 ) ;
#10218 = DIRECTION ( 'NONE',  ( 0.000000000000000000, -1.000000000000000000, 0.000000000000000000 ) ) ;
#10219 = ORIENTED_EDGE ( 'NONE', *, *, #46903, .T. ) ;
#10220 = CARTESIAN_POINT ( 'NONE',  ( 85.12060041149554479, -28.84484196787844468, 173.9512315299091938 ) ) ;
#10221 = DIRECTION ( 'NONE',  ( 0.000000000000000000, -1.000000000000000000, 0.000000000000000000 ) ) ;
#10222 = DIRECTION ( 'NONE',  ( -1.000000000000000000, -1.224606353822377258E-16, -0.000000000000000000 ) ) ;
#10223 = ORIENTED_EDGE ( 'NONE', *, *, #68061, .F. ) ;
#10224 = FACE_OUTER_BOUND ( 'NONE', #18021, .T. ) ;
#10225 =( LENGTH_UNIT ( ) NAMED_UNIT ( * ) SI_UNIT ( .MILLI., .METRE. ) );
#10226 = CYLINDRICAL_SURFACE ( 'NONE', #83079, 8.000000000000000000 ) ;
#10227 = CARTESIAN_POINT ( 'NONE',  ( 32.19136361712703120, 464.6890450778107606, 10.76797718186793773 ) ) ;
#10228 = CARTESIAN_POINT ( 'NONE',  ( -18.66309977023624356, -25.35065258291380985, -38.50078107122106985 ) ) ;
#10229 = ADVANCED_FACE ( 'NONE', ( #79582 ), #36521, .T. ) ;
#10230 = CIRCLE ( 'NONE', #68859, 4.172000000000001485 ) ;
#10231 = CARTESIAN_POINT ( 'NONE',  ( 50.68031002952036346, -60.00000000000001421, 73.51902701646098137 ) ) ;
#10232 =( GEOMETRIC_REPRESENTATION_CONTEXT ( 3 ) GLOBAL_UNCERTAINTY_ASSIGNED_CONTEXT ( ( #3831 ) ) GLOBAL_UNIT_ASSIGNED_CONTEXT ( ( #29524, #6243, #22487 ) ) REPRESENTATION_CONTEXT ( 'NONE', 'WORKASPACE' ) );
#10233 = CARTESIAN_POINT ( 'NONE',  ( 32.12416968186654032, -33.82503823335301263, 41.92710291939467027 ) ) ;
#10234 = CARTESIAN_POINT ( 'NONE',  ( 7.986711519608433285, 108.9736190362343535, -0.5300249774147602899 ) ) ;
#10235 = CARTESIAN_POINT ( 'NONE',  ( 21.71774177896430302, -17.82916512352614546, 31.46925418864567092 ) ) ;
#10236 = EDGE_CURVE ( 'NONE', #85207, #72809, #19437, .T. ) ;
#10239 = AXIS2_PLACEMENT_3D ( 'NONE', #11959, #54004, #44891 ) ;
#10238 = CARTESIAN_POINT ( 'NONE',  ( -14.42049321383198723, 21.45136809881161000, -5.352595841921786501 ) ) ;
#10237 = CARTESIAN_POINT ( 'NONE',  ( -2.499999999999996891, -8.000000000000000000, -17.89626171146327493 ) ) ;
#10240 = EDGE_CURVE ( 'NONE', #66410, #5108, #60720, .T. ) ;
#10241 = DIRECTION ( 'NONE',  ( 0.000000000000000000, -1.000000000000000000, 0.000000000000000000 ) ) ;
#10242 = CARTESIAN_POINT ( 'NONE',  ( 20.97754405179121662, 294.8763868968453608, 9.942224931492262385 ) ) ;
#10243 = EDGE_CURVE ( 'NONE', #91205, #12476, #89981, .T. ) ;
#10244 = FACE_OUTER_BOUND ( 'NONE', #86560, .T. ) ;
#10245 = CARTESIAN_POINT ( 'NONE',  ( 0.000000000000000000, -4.000000000000003553, 27.00000000000000000 ) ) ;
#10246 = CIRCLE ( 'NONE', #42992, 5.000000000000001776 ) ;
#10247 = EDGE_LOOP ( 'NONE', ( #19828, #43654, #31346, #8831 ) ) ;
#10248 = CARTESIAN_POINT ( 'NONE',  ( -13.50000000000000178, 0.000000000000000000, 0.000000000000000000 ) ) ;
#10249 = CARTESIAN_POINT ( 'NONE',  ( -1.007969207232617206E-15, -0.7818963812180719231, 7.999999999999996447 ) ) ;
#10250 = CARTESIAN_POINT ( 'NONE',  ( 98.31310517497099966, 5.000000000000021316, 0.000000000000000000 ) ) ;
#10252 = CARTESIAN_POINT ( 'NONE',  ( 37.34004865435771592, -21.77016028096032230, -27.75726658366467703 ) ) ;
#10251 = FILL_AREA_STYLE ('',( #60954 ) ) ;
#10253 = VERTEX_POINT ( 'NONE', #82227 ) ;
#10254 = AXIS2_PLACEMENT_3D ( 'NONE', #65429, #9295, #98323 ) ;
#10255 = CARTESIAN_POINT ( 'NONE',  ( 28.32636678626138504, 36.29712012945766020, 9.122391396881491588 ) ) ;
#10256 = FACE_OUTER_BOUND ( 'NONE', #64104, .T. ) ;
#10257 = ORIENTED_EDGE ( 'NONE', *, *, #101306, .F. ) ;
#10258 = CARTESIAN_POINT ( 'NONE',  ( 11.89131030317610183, 1.482358050883964840E-15, 0.000000000000000000 ) ) ;
#10259 = CARTESIAN_POINT ( 'NONE',  ( -6.542885568110277106, 41.77240995323538897, -59.03854211387476880 ) ) ;
#10260 = FACE_OUTER_BOUND ( 'NONE', #31615, .T. ) ;
#10261 = CARTESIAN_POINT ( 'NONE',  ( -101.9681297424606896, -60.00000000000000000, 92.55871325212498846 ) ) ;
#10262 = DIRECTION ( 'NONE',  ( 0.000000000000000000, 0.000000000000000000, -1.000000000000000000 ) ) ;
#10263 = CARTESIAN_POINT ( 'NONE',  ( -8.673617379884035472E-16, 15.58845726811991561, -1.205771365940065953 ) ) ;
#10264 = CARTESIAN_POINT ( 'NONE',  ( 24.80105969489321893, 306.0237540681346218, -9.745911707960095427 ) ) ;
#10265 = CARTESIAN_POINT ( 'NONE',  ( 39.69617136735197249, 460.2157148251832837, 2.207451131566625868 ) ) ;
#10267 = CARTESIAN_POINT ( 'NONE',  ( -7.000000000000000000, 8.572527594031471218E-16, -8.125150395352576993 ) ) ;
#10266 = CARTESIAN_POINT ( 'NONE',  ( -8.737863884121843228, -3.000000000000002665, -79.96381019768948306 ) ) ;
#10268 = CIRCLE ( 'NONE', #91218, 5.000000000000001776 ) ;
#10269 = CARTESIAN_POINT ( 'NONE',  ( -84.97744388938244242, -25.49483301205029662, 166.4590254830890785 ) ) ;
#10270 = EDGE_LOOP ( 'NONE', ( #35833, #22155, #59950, #93774, #67723, #32356 ) ) ;
#10271 = DIRECTION ( 'NONE',  ( 0.000000000000000000, 0.000000000000000000, -1.000000000000000000 ) ) ;
#10272 = ORIENTED_EDGE ( 'NONE', *, *, #8471, .F. ) ;
#10273 = ORIENTED_EDGE ( 'NONE', *, *, #57720, .F. ) ;
#10274 = LINE ( 'NONE', #77145, #4464 ) ;
#10275 = CARTESIAN_POINT ( 'NONE',  ( 26.36650669486618881, -3.851859888774471706E-31, 4.000000000000000888 ) ) ;
#10276 = ADVANCED_FACE ( 'NONE', ( #105966 ), #90869, .F. ) ;
#10277 = DIRECTION ( 'NONE',  ( 0.000000000000000000, 0.000000000000000000, 1.000000000000000000 ) ) ;
#10278 = ORIENTED_EDGE ( 'NONE', *, *, #3616, .F. ) ;
#10279 = CARTESIAN_POINT ( 'NONE',  ( -89.99999999999997158, -52.00000000000000000, 198.0238439516549818 ) ) ;
#10280 = CARTESIAN_POINT ( 'NONE',  ( 0.000000000000000000, 0.000000000000000000, -3.852324522925831385 ) ) ;
#10281 = CARTESIAN_POINT ( 'NONE',  ( -3.972557191600006643, 17.31504860060557505, 5.763927351470794491 ) ) ;
#10282 = CARTESIAN_POINT ( 'NONE',  ( -2.324561895696642773E-13, 53.39766064372246746, 10.25000000000230038 ) ) ;
#10283 = DIRECTION ( 'NONE',  ( -1.000000000000000000, 0.000000000000000000, 0.000000000000000000 ) ) ;
#10284 = AXIS2_PLACEMENT_3D ( 'NONE', #30033, #62923, #3621 ) ;
#10285 = ADVANCED_FACE ( 'NONE', ( #72026 ), #7270, .T. ) ;
#10286 = CARTESIAN_POINT ( 'NONE',  ( 93.38347165230982228, -30.00000000000000711, 56.44843285056885662 ) ) ;
#10287 = CARTESIAN_POINT ( 'NONE',  ( -75.88739805180117060, -29.99999999999992895, 164.4352692622292409 ) ) ;
#10288 = CARTESIAN_POINT ( 'NONE',  ( -58.57938139866309513, -60.33867871034321695, 78.30623259849073747 ) ) ;
#10289 = ORIENTED_EDGE ( 'NONE', *, *, #78304, .T. ) ;
#10290 = CARTESIAN_POINT ( 'NONE',  ( 7.000182694785905824, 17.00031971603035430, -0.2646331733798831243 ) ) ;
#10291 = EDGE_LOOP ( 'NONE', ( #13772, #57943, #22523 ) ) ;
#10292 = CARTESIAN_POINT ( 'NONE',  ( -103.4779138909778027, -45.26536958372710018, 182.5772158687078388 ) ) ;
#10293 = CARTESIAN_POINT ( 'NONE',  ( 5.082755093536325930, -10.34375000204838457, -5.082755093536325042 ) ) ;
#10294 = CARTESIAN_POINT ( 'NONE',  ( -29.68315524077005207, 13.47185074185902209, -42.10535821593474282 ) ) ;
#10295 =( NAMED_UNIT ( * ) SI_UNIT ( $, .STERADIAN. ) SOLID_ANGLE_UNIT ( ) );
#10296 = VERTEX_POINT ( 'NONE', #74132 ) ;
#10297 = CARTESIAN_POINT ( 'NONE',  ( 7.225703553013920200, -4.999999999999999112, -73.19314196553180807 ) ) ;
#10298 = CARTESIAN_POINT ( 'NONE',  ( -74.19888714062773261, -60.00000000000002842, 174.2398114387819419 ) ) ;
#10299 = CARTESIAN_POINT ( 'NONE',  ( -3.454253436624930451, -0.8414180287960395521, 103.7259032015043232 ) ) ;
#10300 = CARTESIAN_POINT ( 'NONE',  ( -5.082755093536326818, -20.09375000204838457, 5.082755093536325042 ) ) ;
#10301 = CARTESIAN_POINT ( 'NONE',  ( -0.6462866794873234344, 37.14682203640808211, -27.41685252655225113 ) ) ;
#10302 = CARTESIAN_POINT ( 'NONE',  ( 0.000000000000000000, -1.200000000000000030E-05, -17.50000000000000000 ) ) ;
#10303 = CARTESIAN_POINT ( 'NONE',  ( 7.540179673759326739, -0.000000000000000000, 15.29468310207052362 ) ) ;
#10304 = CARTESIAN_POINT ( 'NONE',  ( 23.21751746555220564, -1.200000000000000030E-05, -33.20617127781077471 ) ) ;
#10305 = CARTESIAN_POINT ( 'NONE',  ( 5.061945117287558915, -8.365139857377744903, 13.66775534171251394 ) ) ;
#10306 = DIRECTION ( 'NONE',  ( 0.000000000000000000, 0.000000000000000000, 1.000000000000000000 ) ) ;
#10307 = SURFACE_STYLE_USAGE ( .BOTH. , #51830 ) ;
#10308 = UNCERTAINTY_MEASURE_WITH_UNIT (LENGTH_MEASURE( 1.000000000000000082E-05 ), #12986, 'distance_accuracy_value', 'NONE');
#10309 = CARTESIAN_POINT ( 'NONE',  ( -29.95449917297849396, -42.96243585709494539, 33.73512318794586662 ) ) ;
#10310 = AXIS2_PLACEMENT_3D ( 'NONE', #52551, #42877, #10503 ) ;
#10311 = CARTESIAN_POINT ( 'NONE',  ( 42.72751150375061258, -29.15843491787571296, 38.64392542651763307 ) ) ;
#10312 = CARTESIAN_POINT ( 'NONE',  ( 5.656854249492380582, -13.81249999999999112, -5.656854249492379694 ) ) ;
#10313 = CARTESIAN_POINT ( 'NONE',  ( -0.3377801289881405822, 46.20008771969307304, 16.28498333803777598 ) ) ;
#10314 = AXIS2_PLACEMENT_3D ( 'NONE', #82414, #100189, #42480 ) ;
#10316 = ADVANCED_FACE ( 'NONE', ( #33179 ), #21134, .T. ) ;
#10315 = CARTESIAN_POINT ( 'NONE',  ( -94.17984850184487300, -38.49173615782690661, 201.2012723578915256 ) ) ;
#10317 = ORIENTED_EDGE ( 'NONE', *, *, #56340, .T. ) ;
#10319 = CARTESIAN_POINT ( 'NONE',  ( 32.35336999986095208, 300.6590557721156642, 11.25190399080426751 ) ) ;
#10318 = LINE ( 'NONE', #60503, #79737 ) ;
#10320 = CARTESIAN_POINT ( 'NONE',  ( 76.76980298920247492, -59.99999999999994316, 146.8786135127453178 ) ) ;
#10321 = CARTESIAN_POINT ( 'NONE',  ( 17.61650669486618881, 0.000000000000000000, 4.000000000000000888 ) ) ;
#10322 = CARTESIAN_POINT ( 'NONE',  ( -7.237253929247286166, 41.05631633789147372, -58.62830998736340149 ) ) ;
#10323 = CARTESIAN_POINT ( 'NONE',  ( 17.81438722625302518, -5.000000000000000888, 6.123233995736769241E-16 ) ) ;
#10324 = CARTESIAN_POINT ( 'NONE',  ( -12.50000000000000000, -3.000000000000003109, -14.34180675897363599 ) ) ;
#10325 = DIRECTION ( 'NONE',  ( 0.000000000000000000, -1.000000000000000000, 0.000000000000000000 ) ) ;
#10326 = DIRECTION ( 'NONE',  ( -1.000000000000000000, -1.224606353822377258E-16, -0.000000000000000000 ) ) ;
#10327 = CONICAL_SURFACE ( 'NONE', #103356, 5.000000000000010658, 0.9599310885968697082 ) ;
#10328 = CARTESIAN_POINT ( 'NONE',  ( 106.8925583917160083, -59.99999999999999289, 121.9434126937530891 ) ) ;
#10329 = CARTESIAN_POINT ( 'NONE',  ( 5.819846122303831137, -4.937269551422888370, 4.448398286272754909 ) ) ;
#10330 = CARTESIAN_POINT ( 'NONE',  ( 13.58349330513380515, 4.000000000000002665, 0.000000000000000000 ) ) ;
#10331 = VERTEX_POINT ( 'NONE', #56344 ) ;
#10332 = ADVANCED_FACE ( 'NONE', ( #66586 ), #25640, .T. ) ;
#10333 = DIRECTION ( 'NONE',  ( 0.000000000000000000, 1.000000000000000000, 0.000000000000000000 ) ) ;
#10334 = VERTEX_POINT ( 'NONE', #60122 ) ;
#10335 = CIRCLE ( 'NONE', #49905, 7.000000000000000000 ) ;
#10336 = CARTESIAN_POINT ( 'NONE',  ( 26.18069599319563068, 36.97239296640589146, -9.652207212211994403 ) ) ;
#10337 = DIRECTION ( 'NONE',  ( -0.5735764363510459374, -0.8191520442889919096, 0.000000000000000000 ) ) ;
#10338 = CARTESIAN_POINT ( 'NONE',  ( 25.35866071869866190, 306.3477625189083255, 10.50099866488358202 ) ) ;
#10339 = CARTESIAN_POINT ( 'NONE',  ( 34.83349330513379982, 1.593028355512270567E-15, 0.000000000000000000 ) ) ;
#10340 = CARTESIAN_POINT ( 'NONE',  ( 7.188101187500001821, -17.93750000204838457, -2.977408999572650483 ) ) ;
#10341 = FACE_OUTER_BOUND ( 'NONE', #83340, .T. ) ;
#10342 = AXIS2_PLACEMENT_3D ( 'NONE', #42676, #75575, #101454 ) ;
#10343 = UNCERTAINTY_MEASURE_WITH_UNIT (LENGTH_MEASURE( 1.000000000000000082E-05 ), #104, 'distance_accuracy_value', 'NONE');
#10344 = CARTESIAN_POINT ( 'NONE',  ( -5.656854249492379694, -12.12500000409676915, -5.656854249492380582 ) ) ;
#10346 = VERTEX_POINT ( 'NONE', #101617 ) ;
#10345 = CARTESIAN_POINT ( 'NONE',  ( -38.85520731754901647, 460.5778612837317496, 2.285564115289548059 ) ) ;
#10347 = CARTESIAN_POINT ( 'NONE',  ( 80.03137391603202389, -56.86261681419952652, 169.5251337316609579 ) ) ;
#10348 = VECTOR ( 'NONE', #71420, 1000.000000000000341 ) ;
#10349 = CARTESIAN_POINT ( 'NONE',  ( -45.99999999999999289, 462.9157814553173012, 7.768519869190400939 ) ) ;
#10350 = DIRECTION ( 'NONE',  ( -0.000000000000000000, -0.000000000000000000, 1.000000000000000000 ) ) ;
#10351 = ORIENTED_EDGE ( 'NONE', *, *, #99851, .T. ) ;
#10352 = CARTESIAN_POINT ( 'NONE',  ( -18.75715577600996298, 302.6227400944664510, -10.04868916684661073 ) ) ;
#10353 = CARTESIAN_POINT ( 'NONE',  ( 40.02592568779148507, 3.851859888774471706E-31, 5.000000000000001776 ) ) ;
#10354 = LINE ( 'NONE', #9286, #70925 ) ;
#10355 = SURFACE_SIDE_STYLE ('',( #99902 ) ) ;
#10356 = LINE ( 'NONE', #633, #41174 ) ;
#10357 = DIRECTION ( 'NONE',  ( -0.5735764363510494901, -0.8191520442889894671, 0.000000000000000000 ) ) ;
#10358 = EDGE_CURVE ( 'NONE', #101925, #28968, #97934, .T. ) ;
#10359 = ORIENTED_EDGE ( 'NONE', *, *, #36291, .F. ) ;
#10360 = DIRECTION ( 'NONE',  ( 0.000000000000000000, -1.000000000000000000, 0.000000000000000000 ) ) ;
#10361 = CIRCLE ( 'NONE', #48236, 12.16579798332631945 ) ;
#10362 = CARTESIAN_POINT ( 'NONE',  ( -1.000000000000000000, -64.69605072851580019, 10.12418081636205436 ) ) ;
#10363 = CARTESIAN_POINT ( 'NONE',  ( 87.48442578725276064, -35.36902786773393359, 189.1140711639433221 ) ) ;
#10364 = ADVANCED_FACE ( 'NONE', ( #10987 ), #18054, .F. ) ;
#10365 = DIRECTION ( 'NONE',  ( -1.000000000000000000, -1.224606353822377258E-16, -0.000000000000000000 ) ) ;
#10366 = CARTESIAN_POINT ( 'NONE',  ( 7.188101187499999156, -28.25000000204838813, 2.977408999572654924 ) ) ;
#10367 = DIRECTION ( 'NONE',  ( 0.000000000000000000, -0.000000000000000000, 1.000000000000000000 ) ) ;
#10368 = CARTESIAN_POINT ( 'NONE',  ( 7.808540133805411010, 51.84039965102822833, 3.793121522970396065 ) ) ;
#10369 = CARTESIAN_POINT ( 'NONE',  ( 0.000000000000000000, 0.000000000000000000, 13.27631144943088515 ) ) ;
#10370 = ORIENTED_EDGE ( 'NONE', *, *, #39415, .F. ) ;
#10371 = EDGE_CURVE ( 'NONE', #3543, #32331, #16172, .T. ) ;
#10372 = CARTESIAN_POINT ( 'NONE',  ( 1.010771448917421544, 43.89380339074816817, 16.74650787413497355 ) ) ;
#10373 = CARTESIAN_POINT ( 'NONE',  ( -10.43542583693973036, 6.878147458890449428, 0.000000000000000000 ) ) ;
#10374 = LINE ( 'NONE', #43289, #63585 ) ;
#10375 = MECHANICAL_DESIGN_GEOMETRIC_PRESENTATION_REPRESENTATION (  '', ( #56877 ), #6991 ) ;
#10376 = ORIENTED_EDGE ( 'NONE', *, *, #74414, .T. ) ;
#10377 = CARTESIAN_POINT ( 'NONE',  ( -7.370387608271186330, 52.18044071326720967, -2.386534409371826371 ) ) ;
#10378 = DIRECTION ( 'NONE',  ( 1.000000000000000000, 0.000000000000000000, 0.000000000000000000 ) ) ;
#10379 = ORIENTED_EDGE ( 'NONE', *, *, #55082, .F. ) ;
#10380 = VECTOR ( 'NONE', #49909, 1000.000000000000000 ) ;
#10381 = CARTESIAN_POINT ( 'NONE',  ( 32.13614325032531127, 435.4396166566540956, 16.27706860089754670 ) ) ;
#10382 = CARTESIAN_POINT ( 'NONE',  ( -0.07775081836201770680, 7.746009256456749092, -51.74999999999986500 ) ) ;
#10383 = CARTESIAN_POINT ( 'NONE',  ( 9.999945253488242258, 101.0001368662946675, -0.2662901834230885223 ) ) ;
#10384 = DIRECTION ( 'NONE',  ( -1.000000000000000000, -1.224606353822377258E-16, -0.000000000000000000 ) ) ;
#10385 = CARTESIAN_POINT ( 'NONE',  ( -86.49296547713275629, -59.99999999999998579, 200.7931037995327870 ) ) ;
#10386 = CARTESIAN_POINT ( 'NONE',  ( 10.28624191511809371, 43.99263840937192782, -12.90779740156171407 ) ) ;
#10387 = DIRECTION ( 'NONE',  ( 0.000000000000000000, -0.5000000000000004441, 0.8660254037844383745 ) ) ;
#10388 = CARTESIAN_POINT ( 'NONE',  ( 33.09999999999999432, 1.533819458162526451E-15, 0.000000000000000000 ) ) ;
#10389 = B_SPLINE_CURVE_WITH_KNOTS ( 'NONE', 3,
 ( #9277, #43259, #77219, #3331, #42184, #75615, #59457, #35192, #43783, #35734, #92325, #92859, #19027, #20637, #103096, #53477, #96061, #4388, #85867, #55044, #12992, #104135, #30279, #86399, #53981, #95524, #21151, #71238, #22193, #46958 ),
 .UNSPECIFIED., .F., .F.,
 ( 4, 2, 2, 2, 2, 2, 2, 2, 2, 2, 2, 2, 2, 2, 4 ),
 ( 0.008103130636685064100, 0.008563624816068786047, 0.009024118995452509728, 0.009945107354219958826, 0.01086609571298740792, 0.01178708407175485702, 0.01270807243052230612, 0.01316856660990603500, 0.01362906078928976215, 0.01408955496867348930, 0.01431980205836536416, 0.01455004914805723901, 0.01478029623774911386, 0.01501054332744098871, 0.01547103750682472800 ),
 .UNSPECIFIED. ) ;
#10390 = CARTESIAN_POINT ( 'NONE',  ( -83.81516214089008088, -53.77059041807098083, 188.4648016043023517 ) ) ;
#10391 = CARTESIAN_POINT ( 'NONE',  ( -5.290067270632214047, 53.47475093287474124, -8.531152949374821048 ) ) ;
#10392 = AXIS2_PLACEMENT_3D ( 'NONE', #92441, #74660, #34255 ) ;
#10393 = CIRCLE ( 'NONE', #68946, 5.000000000000002665 ) ;
#10394 = ORIENTED_EDGE ( 'NONE', *, *, #13164, .F. ) ;
#10395 = CARTESIAN_POINT ( 'NONE',  ( -18.99999999999999289, -4.000000000000000000, 25.00000000000000000 ) ) ;
#10396 = ADVANCED_FACE ( 'NONE', ( #9933 ), #71038, .F. ) ;
#10397 = CARTESIAN_POINT ( 'NONE',  ( 3.350247031700767320, -1.071204144247449586, 104.4269854689273558 ) ) ;
#10398 = CARTESIAN_POINT ( 'NONE',  ( -82.81177915581980642, -37.82586872126953637, 1.744547249875558093 ) ) ;
#10400 = B_SPLINE_CURVE_WITH_KNOTS ( 'NONE', 3,
 ( #96735, #105867, #14726, #97771, #47096, #55703, #80526, #72960, #72445, #105349 ),
 .UNSPECIFIED., .F., .F.,
 ( 4, 2, 2, 2, 4 ),
 ( 0.000000000000000000, 0.001993803085173303461, 0.003987606170346606922, 0.005981409255519910817, 0.007975212340693213844 ),
 .UNSPECIFIED. ) ;
#10399 = CIRCLE ( 'NONE', #19083, 24.55262289886175964 ) ;
#10401 = CARTESIAN_POINT ( 'NONE',  ( -3.964214964211822068, -12.08915882607856318, -10.21564873357087500 ) ) ;
#10402 = CARTESIAN_POINT ( 'NONE',  ( -34.06332199976886699, 330.0526646846329299, -3.810096259360388427 ) ) ;
#10403 = CARTESIAN_POINT ( 'NONE',  ( -30.00000000000000000, 461.8887775513397855, 11.55279652844097171 ) ) ;
#10404 = CARTESIAN_POINT ( 'NONE',  ( -11.38238776550285003, -10.91738000822960686, 10.29643454240246214 ) ) ;
#10405 = CARTESIAN_POINT ( 'NONE',  ( -6.362732954939748886, -11.89495883945591004, 10.82964177580678644 ) ) ;
#10406 = SURFACE_STYLE_USAGE ( .BOTH. , #43844 ) ;
#10407 = EDGE_CURVE ( 'NONE', #17539, #101821, #28646, .T. ) ;
#10408 = CARTESIAN_POINT ( 'NONE',  ( -43.40712426123182155, 434.3590067275359274, 15.37327885490237911 ) ) ;
#10409 = CARTESIAN_POINT ( 'NONE',  ( 67.93272126786412457, -60.00000000000005684, 143.1824220594335770 ) ) ;
#10410 =( NAMED_UNIT ( * ) SI_UNIT ( $, .STERADIAN. ) SOLID_ANGLE_UNIT ( ) );
#10411 = CARTESIAN_POINT ( 'NONE',  ( -94.85933876937251341, -60.00000000000005684, 26.66572952598730595 ) ) ;
#10412 = CARTESIAN_POINT ( 'NONE',  ( -70.22133738824466320, -49.91278461913130116, 108.8011977758523301 ) ) ;
#10413 = ORIENTED_EDGE ( 'NONE', *, *, #1587, .F. ) ;
#10414 = CARTESIAN_POINT ( 'NONE',  ( 67.93272126786412457, -60.00000000000005684, 143.1824220594335770 ) ) ;
#10415 = CARTESIAN_POINT ( 'NONE',  ( 51.81797853811001886, 40.83872170108235622, 39.69809105071564659 ) ) ;
#10416 = CARTESIAN_POINT ( 'NONE',  ( 11.32007523880735178, -59.99999999999015898, 42.02588058645514479 ) ) ;
#10417 = EDGE_LOOP ( 'NONE', ( #101801, #83671, #59680, #103603 ) ) ;
#10418 = CARTESIAN_POINT ( 'NONE',  ( 14.91270732344407257, 41.98564553269472555, -86.62216337287246404 ) ) ;
#10419 = B_SPLINE_CURVE_WITH_KNOTS ( 'NONE', 3,
 ( #105437, #47185, #80085, #6192, #39128, #104917, #31576, #63935, #6735, #96823, #22953, #39658, #80612, #43360, #76245, #9913, #25622, #98910, #16967, #35293, #2353, #18032 ),
 .UNSPECIFIED., .F., .F.,
 ( 4, 2, 2, 2, 2, 2, 2, 2, 2, 2, 4 ),
 ( 0.007315589541698120334, 0.007567575265297590316, 0.007819560988897061166, 0.008323532436096002865, 0.008827503883294946299, 0.009331475330493889733, 0.009835446777692833167, 0.01033941822489177487, 0.01084338967209071830, 0.01109537539569019002, 0.01134736111928966174 ),
 .UNSPECIFIED. ) ;
#10420 = CARTESIAN_POINT ( 'NONE',  ( 7.188101187500000044, -27.03125000204838813, 0.000000000000000000 ) ) ;
#10421 = AXIS2_PLACEMENT_3D ( 'NONE', #70526, #14921, #55378 ) ;
#10422 = CARTESIAN_POINT ( 'NONE',  ( -5.858824175751780494, -6.214209391276424022, -1.318356988357135107 ) ) ;
#10423 = ORIENTED_EDGE ( 'NONE', *, *, #106259, .F. ) ;
#10424 = VERTEX_POINT ( 'NONE', #51456 ) ;
#10425 = CARTESIAN_POINT ( 'NONE',  ( 1.735558044533036748, 41.99999999999999289, -69.74083754112251654 ) ) ;
#10426 = CARTESIAN_POINT ( 'NONE',  ( -11.54058046252955627, 43.31680132832994445, 14.28235035768446082 ) ) ;
#10427 = CARTESIAN_POINT ( 'NONE',  ( -1.320432766682874540E-15, -13.53125000204838457, 7.188101187500000044 ) ) ;
#10428 = CARTESIAN_POINT ( 'NONE',  ( -48.98918515124638162, 13.11539385479550113, 16.41516879933075046 ) ) ;
#10429 = DIRECTION ( 'NONE',  ( 1.000000000000000000, 1.224606353822377258E-16, 0.000000000000000000 ) ) ;
#10430 = CARTESIAN_POINT ( 'NONE',  ( 14.29190075645222358, 19.61368180395867356, -4.501023549814667568 ) ) ;
#10431 = CARTESIAN_POINT ( 'NONE',  ( -1.570796324980112679, 50.00000000000000000, -97.00000000000000000 ) ) ;
#10432 = CARTESIAN_POINT ( 'NONE',  ( -12.44829945131329474, -3.980163019925683443, -13.20820160251541431 ) ) ;
#10433 = FACE_OUTER_BOUND ( 'NONE', #104847, .T. ) ;
#10434 = EDGE_CURVE ( 'NONE', #92260, #74342, #93463, .T. ) ;
#10435 = ORIENTED_EDGE ( 'NONE', *, *, #47720, .T. ) ;
#10436 = CARTESIAN_POINT ( 'NONE',  ( 4.399054598113323777, -1.887557197752986804, 102.7269706464928021 ) ) ;
#10438 = CARTESIAN_POINT ( 'NONE',  ( 31.09166453561272547, -29.07463850443421904, 31.63965989746132834 ) ) ;
#10437 = CARTESIAN_POINT ( 'NONE',  ( -3.801077171203096405, -48.88909605940818182, 104.1059035333590401 ) ) ;
#10439 = VECTOR ( 'NONE', #36823, 1000.000000000000000 ) ;
#10440 = CARTESIAN_POINT ( 'NONE',  ( 20.16952962162183738, -4.285714285713005722, -15.50035291838722884 ) ) ;
#10441 = ORIENTED_EDGE ( 'NONE', *, *, #1960, .F. ) ;
#10442 = EDGE_CURVE ( 'NONE', #104224, #6978, #102063, .T. ) ;
#10443 = AXIS2_PLACEMENT_3D ( 'NONE', #65125, #40846, #24175 ) ;
#10444 = ORIENTED_EDGE ( 'NONE', *, *, #2754, .T. ) ;
#10446 = CARTESIAN_POINT ( 'NONE',  ( -6.145999768515837403, -5.000000000000000000, 7.996316163935361487 ) ) ;
#10445 = CARTESIAN_POINT ( 'NONE',  ( -26.94610874357095298, 34.81329346479147802, -7.564552669781196670 ) ) ;
#10447 = CARTESIAN_POINT ( 'NONE',  ( 97.73333333333333428, 1.023464760207051730E-14, 0.000000000000000000 ) ) ;
#10448 = CARTESIAN_POINT ( 'NONE',  ( -43.67509741642822974, 485.0313177283814525, 1.734658348000118755 ) ) ;
#10449 =( LENGTH_UNIT ( ) NAMED_UNIT ( * ) SI_UNIT ( .MILLI., .METRE. ) );
#10450 = FACE_OUTER_BOUND ( 'NONE', #79671, .T. ) ;
#10451 = ORIENTED_EDGE ( 'NONE', *, *, #49462, .F. ) ;
#10452 = CARTESIAN_POINT ( 'NONE',  ( 87.58642902445230050, -60.00000000000000000, -22.04675162796464960 ) ) ;
#10453 = DIRECTION ( 'NONE',  ( -0.000000000000000000, -0.000000000000000000, -1.000000000000000000 ) ) ;
#10454 = CARTESIAN_POINT ( 'NONE',  ( 62.59428447264396311, 6.856755485862130937E-15, 0.000000000000000000 ) ) ;
#10455 = CARTESIAN_POINT ( 'NONE',  ( -46.97290287162347511, 17.76084728355517584, -16.28892042402491924 ) ) ;
#10456 = EDGE_LOOP ( 'NONE', ( #57486, #62517, #89486, #11686 ) ) ;
#10457 =( GEOMETRIC_REPRESENTATION_CONTEXT ( 3 ) GLOBAL_UNCERTAINTY_ASSIGNED_CONTEXT ( ( #66742 ) ) GLOBAL_UNIT_ASSIGNED_CONTEXT ( ( #64712, #2079, #11767 ) ) REPRESENTATION_CONTEXT ( 'NONE', 'WORKASPACE' ) );
#10458 = CARTESIAN_POINT ( 'NONE',  ( -101.0993648165865295, -30.00000000001622524, 198.6624016725467357 ) ) ;
#10459 = EDGE_LOOP ( 'NONE', ( #31431, #72869, #82775, #99577, #6333, #16627 ) ) ;
#10460 = ORIENTED_EDGE ( 'NONE', *, *, #87246, .T. ) ;
#10461 = CIRCLE ( 'NONE', #27772, 4.172000000000001485 ) ;
#10462 = CARTESIAN_POINT ( 'NONE',  ( 7.743982712349854580, 81.53786985239264595, 2.020119794285907044 ) ) ;
#10463 = CARTESIAN_POINT ( 'NONE',  ( 43.84452598814514346, 485.1288417159794903, -0.7004174638389097929 ) ) ;
#10464 = CARTESIAN_POINT ( 'NONE',  ( 0.01372220897661637073, 5.309964801958114933, -3.802871176606130277 ) ) ;
#10465 = SURFACE_STYLE_USAGE ( .BOTH. , #19151 ) ;
#10466 = CARTESIAN_POINT ( 'NONE',  ( 85.67655332170797067, -52.75487301146129937, -9.150629182708584608 ) ) ;
#10467 = CARTESIAN_POINT ( 'NONE',  ( -40.93720775505873632, 312.8591800994336722, -5.708390564187923566 ) ) ;
#10468 = LINE ( 'NONE', #51462, #52512 ) ;
#10469 = CARTESIAN_POINT ( 'NONE',  ( -18.26456092131584796, 45.00000000000001421, 62.42260643610311632 ) ) ;
#10470 = EDGE_LOOP ( 'NONE', ( #10273, #103939, #41356, #50716, #496, #83495, #36220, #25383, #17679 ) ) ;
#10471 = CARTESIAN_POINT ( 'NONE',  ( -6.499999999999998224, 2.723853875608233555, -6.224027332483752950 ) ) ;
#10472 = ORIENTED_EDGE ( 'NONE', *, *, #38723, .T. ) ;
#10473 = CARTESIAN_POINT ( 'NONE',  ( 48.15129163819126035, 9.495040186444088093, -16.85535821593549954 ) ) ;
#10474 = CARTESIAN_POINT ( 'NONE',  ( 19.00000000000000711, 5.000000000000000888, 25.00000000000000000 ) ) ;
#10476 = ORIENTED_EDGE ( 'NONE', *, *, #38880, .F. ) ;
#10475 = CARTESIAN_POINT ( 'NONE',  ( 5.420470438621123321, 41.88321586334136981, -59.04137885805280916 ) ) ;
#10477 = CARTESIAN_POINT ( 'NONE',  ( 75.77493148631056386, -42.96215371644679237, 126.5390892215617100 ) ) ;
#10478 = ORIENTED_EDGE ( 'NONE', *, *, #26063, .F. ) ;
#10479 = AXIS2_PLACEMENT_3D ( 'NONE', #90611, #82516, #16720 ) ;
#10480 = CARTESIAN_POINT ( 'NONE',  ( 5.312125216579068443, -51.48437205207593337, 39.95393515823275266 ) ) ;
#10481 = LINE ( 'NONE', #99040, #43870 ) ;
#10482 = CARTESIAN_POINT ( 'NONE',  ( -5.082755093536326818, -24.21875000204838813, 5.082755093536325042 ) ) ;
#10483 =( BOUNDED_SURFACE ( )  B_SPLINE_SURFACE ( 2, 3, ( 
 ( #6132, #71943, #6668, #46085, #70883, #30448, #55212, #22890 ),
 ( #96236, #103255, #78966, #29401, #104846, #13156, #61756, #96758 ),
 ( #62283, #4558, #71399, #69824, #87610, #88137, #55729, #95173 ) ),
 .UNSPECIFIED., .F., .F., .F. ) 
 B_SPLINE_SURFACE_WITH_KNOTS ( ( 3, 3 ),
 ( 4, 2, 2, 4 ),
 ( 0.000000000000000000, 1.000000000000000000 ),
 ( -0.05863181436295197141, -0.05487404235502676975, -0.04584008019048942117, -0.04405802166693190830 ),
 .UNSPECIFIED. ) 
 GEOMETRIC_REPRESENTATION_ITEM ( )  RATIONAL_B_SPLINE_SURFACE ( (
 ( 1.000000000000000000, 1.000000000000000000, 1.000000000000000000, 1.000000000000000000, 1.000000000000000000, 1.000000000000000000, 1.000000000000000000, 1.000000000000000000),
 ( 1.857142857142858317, 1.857142857142858317, 1.857142857142858317, 1.857142857142858317, 1.857142857142858317, 1.857142857142858317, 1.857142857142858317, 1.857142857142858317),
 ( 1.000000000000000000, 1.000000000000000000, 1.000000000000000000, 1.000000000000000000, 1.000000000000000000, 1.000000000000000000, 1.000000000000000000, 1.000000000000000000) ) ) 
 REPRESENTATION_ITEM ( '' )  SURFACE ( )  );
#10484 = PRESENTATION_LAYER_ASSIGNMENT (  '', '', ( #44922 ) ) ;
#10485 = CARTESIAN_POINT ( 'NONE',  ( -94.14808112328414325, -57.65316219711669987, -13.38331396264917394 ) ) ;
#10486 = EDGE_CURVE ( 'NONE', #84262, #58211, #60755, .T. ) ;
#10487 = ORIENTED_EDGE ( 'NONE', *, *, #55753, .F. ) ;
#10488 = CIRCLE ( 'NONE', #103501, 7.000000000000000000 ) ;
#10489 = FILL_AREA_STYLE ('',( #2397 ) ) ;
#10490 = CARTESIAN_POINT ( 'NONE',  ( 6.281175601187043434, -7.505553499465149159, -1.184821369511938456E-16 ) ) ;
#10492 = CARTESIAN_POINT ( 'NONE',  ( 103.9750665207554476, -52.71699900044285414, 186.8198939251532238 ) ) ;
#10491 = AXIS2_PLACEMENT_3D ( 'NONE', #73821, #56564, #40394 ) ;
#10493 = CARTESIAN_POINT ( 'NONE',  ( 6.429306121731439561, 51.32037123737740103, -7.802259468956040500 ) ) ;
#10494 = EDGE_CURVE ( 'NONE', #76235, #29175, #94607, .T. ) ;
#10495 = AXIS2_PLACEMENT_3D ( 'NONE', #11938, #36797, #29761 ) ;
#10496 = CARTESIAN_POINT ( 'NONE',  ( 40.02592568779148507, 1.482358050883964840E-15, 0.000000000000000000 ) ) ;
#10497 = CARTESIAN_POINT ( 'NONE',  ( -5.656854249492379694, -15.12500000409677092, -5.656854249492380582 ) ) ;
#10498 = DIRECTION ( 'NONE',  ( -1.000000000000000000, -1.224606353822377258E-16, -0.000000000000000000 ) ) ;
#10499 = CARTESIAN_POINT ( 'NONE',  ( 0.000000000000000000, 0.5000000000000000000, 14.78272384904389192 ) ) ;
#10500 = EDGE_CURVE ( 'NONE', #52941, #9249, #78393, .T. ) ;
#10501 = DIRECTION ( 'NONE',  ( 0.000000000000000000, 0.000000000000000000, 1.000000000000000000 ) ) ;
#10502 = CARTESIAN_POINT ( 'NONE',  ( -37.62251730745835943, 437.3427388312646258, 4.535622330043169725 ) ) ;
#10503 = DIRECTION ( 'NONE',  ( -1.000000000000000000, 0.000000000000000000, 0.000000000000000000 ) ) ;
#10504 = DIRECTION ( 'NONE',  ( 1.000000000000000000, 0.000000000000000000, 0.000000000000000000 ) ) ;
#10505 = DIRECTION ( 'NONE',  ( -0.000000000000000000, -0.000000000000000000, -1.000000000000000000 ) ) ;
#10506 = ORIENTED_EDGE ( 'NONE', *, *, #52543, .T. ) ;
#10507 = CARTESIAN_POINT ( 'NONE',  ( 0.6250000000000004441, -8.299410119600883817, -7.298562697733114391 ) ) ;
#10508 = ADVANCED_FACE ( 'NONE', ( #62757 ), #78922, .F. ) ;
#10509 = CARTESIAN_POINT ( 'NONE',  ( 1.235549969621061006, 10.15115531407437999, 50.72583874370463519 ) ) ;
#10510 = CARTESIAN_POINT ( 'NONE',  ( -84.97248593416721008, -29.99999999999999645, 170.0635220576484699 ) ) ;
#10511 = ORIENTED_EDGE ( 'NONE', *, *, #78576, .F. ) ;
#10512 = CARTESIAN_POINT ( 'NONE',  ( 37.88767513972955214, 25.36992872674205657, -13.42525127874668023 ) ) ;
#10513 = CARTESIAN_POINT ( 'NONE',  ( 72.74531393631698961, -57.65900400693993788, 179.1409299794756862 ) ) ;
#10514 = CONICAL_SURFACE ( 'NONE', #36372, 33.82893434829263413, 1.221730476396026610 ) ;
#10516 = DIRECTION ( 'NONE',  ( -1.000000000000000000, -1.224606353822377258E-16, -0.000000000000000000 ) ) ;
#10515 = CARTESIAN_POINT ( 'NONE',  ( -14.46174234134181624, 2.926873011486890164, -3.961839331262607899 ) ) ;
#10517 = CARTESIAN_POINT ( 'NONE',  ( 64.43482812103761148, -37.84152687303451756, -32.99898107021154914 ) ) ;
#10518 = CIRCLE ( 'NONE', #93221, 4.172000000000001485 ) ;
#10519 = CARTESIAN_POINT ( 'NONE',  ( -43.59756234217329052, 434.3244621007144133, 14.55946156040312545 ) ) ;
#10520 = CARTESIAN_POINT ( 'NONE',  ( -30.87182542889072323, -60.00000000000001421, 43.47827688693090664 ) ) ;
#10521 = DIRECTION ( 'NONE',  ( -1.000000000000000000, -1.224606353822377258E-16, -0.000000000000000000 ) ) ;
#10522 = CARTESIAN_POINT ( 'NONE',  ( -51.78317192862404994, 48.00000000000000000, 39.73656039225668479 ) ) ;
#10523 = CARTESIAN_POINT ( 'NONE',  ( -86.12452592232807547, -50.16182726635322098, 190.9343274795246828 ) ) ;
#10524 = ORIENTED_EDGE ( 'NONE', *, *, #68209, .F. ) ;
#10525 = CARTESIAN_POINT ( 'NONE',  ( 30.90725857724351044, 14.69157187025844813, 40.57373053090514503 ) ) ;
#10526 = CARTESIAN_POINT ( 'NONE',  ( -2.033835829640177284, -49.92092604325223704, 32.20724000701986256 ) ) ;
#10527 = CYLINDRICAL_SURFACE ( 'NONE', #39462, 4.000000000000000000 ) ;
#10528 = CARTESIAN_POINT ( 'NONE',  ( -42.57785836761692622, 484.8814997681452610, 8.276214290995149270 ) ) ;
#10530 = SURFACE_STYLE_USAGE ( .BOTH. , #101145 ) ;
#10529 = CARTESIAN_POINT ( 'NONE',  ( -21.97639485782973878, 294.9974105476200066, 1.968212750500118124 ) ) ;
#10531 = ORIENTED_EDGE ( 'NONE', *, *, #16337, .T. ) ;
#10532 = ADVANCED_FACE ( 'NONE', ( #5047 ), #69370, .T. ) ;
#10533 = CIRCLE ( 'NONE', #77769, 4.000000000000007105 ) ;
#10534 = CARTESIAN_POINT ( 'NONE',  ( -1.836601268058450879E-15, 1.005902684993158047, -14.99698745252234566 ) ) ;
#10535 = CARTESIAN_POINT ( 'NONE',  ( 1.011751391879055717, 27.47325995063050641, 40.25199818947412211 ) ) ;
#10536 = CARTESIAN_POINT ( 'NONE',  ( -30.92868852183901396, 8.704894651777072667, -40.98784967800754941 ) ) ;
#10537 = CARTESIAN_POINT ( 'NONE',  ( 17.78133731104211535, 50.00000000000002132, 62.21716898123242601 ) ) ;
#10538 = CARTESIAN_POINT ( 'NONE',  ( 35.57955382936916067, 363.3973965622570859, 2.919629247011395368 ) ) ;
#10539 = EDGE_CURVE ( 'NONE', #74088, #38824, #36675, .T. ) ;
#10540 = CARTESIAN_POINT ( 'NONE',  ( 34.84618260875170392, 489.9833681528626812, 11.97975507378813731 ) ) ;
#10541 = CARTESIAN_POINT ( 'NONE',  ( -14.29190075645216851, 12.99999999999999289, 0.000000000000000000 ) ) ;
#10542 = CARTESIAN_POINT ( 'NONE',  ( 106.1195120942077494, -59.99999999999999289, 102.8136370513695397 ) ) ;
#10543 = CARTESIAN_POINT ( 'NONE',  ( -81.76550668722990167, -29.09399621363404975, 145.4573940219550821 ) ) ;
#10544 = ORIENTED_EDGE ( 'NONE', *, *, #84423, .F. ) ;
#10545 = CARTESIAN_POINT ( 'NONE',  ( 16.08349330513380337, 4.000000000000002665, 0.000000000000000000 ) ) ;
#10546 = DIRECTION ( 'NONE',  ( 0.000000000000000000, -1.000000000000000000, 0.000000000000000000 ) ) ;
#10547 = CARTESIAN_POINT ( 'NONE',  ( -6.106896958092910666, -4.373166921188805567, -16.80698729315730944 ) ) ;
#10548 = CARTESIAN_POINT ( 'NONE',  ( 37.67371248340228362, 380.0629637908955374, 5.300177988891823233 ) ) ;
#10549 = DIRECTION ( 'NONE',  ( -1.000000000000000000, -1.224606353822377258E-16, -0.000000000000000000 ) ) ;
#10550 = ORIENTED_EDGE ( 'NONE', *, *, #61861, .F. ) ;
#10551 = CIRCLE ( 'NONE', #77784, 4.172000000000001485 ) ;
#10552 = DIRECTION ( 'NONE',  ( -0.000000000000000000, -1.000000000000000000, -0.000000000000000000 ) ) ;
#10553 = VERTEX_POINT ( 'NONE', #19679 ) ;
#10554 = PRESENTATION_STYLE_ASSIGNMENT (( #35954 ) ) ;
#10555 = VECTOR ( 'NONE', #63961, 1000.000000000000000 ) ;
#10556 = CARTESIAN_POINT ( 'NONE',  ( -6.750000000000018652, 11.69134295108991317, -13.00000000000000000 ) ) ;
#10557 = CARTESIAN_POINT ( 'NONE',  ( 6.403347876734715172, 41.95607664916837365, -69.22843809692237471 ) ) ;
#10558 = CARTESIAN_POINT ( 'NONE',  ( -60.66923414622394262, 50.00000000000000000, 17.93278245653412384 ) ) ;
#10559 = CARTESIAN_POINT ( 'NONE',  ( 4.999999999999960032, -13.81090860391464048, 13.12305563960480548 ) ) ;
#10560 = EDGE_CURVE ( 'NONE', #1581, #35102, #77981, .T. ) ;
#10561 = CIRCLE ( 'NONE', #36418, 3.309500000000001663 ) ;
#10562 = PRESENTATION_STYLE_ASSIGNMENT (( #27876 ) ) ;
#10563 = ORIENTED_EDGE ( 'NONE', *, *, #26243, .T. ) ;
#10564 = CARTESIAN_POINT ( 'NONE',  ( 94.67064643570367366, -59.99999999999998579, 46.77569099326773028 ) ) ;
#10566 = CARTESIAN_POINT ( 'NONE',  ( 19.10045511374297078, -42.95404717622270141, 31.48189410863279392 ) ) ;
#10565 = CARTESIAN_POINT ( 'NONE',  ( -93.93757927471676794, -14.21045842199439946, 198.1409199811383246 ) ) ;
#10567 = FACE_OUTER_BOUND ( 'NONE', #43000, .T. ) ;
#10568 = CARTESIAN_POINT ( 'NONE',  ( 0.000000000000000000, 0.000000000000000000, 0.000000000000000000 ) ) ;
#10569 = CARTESIAN_POINT ( 'NONE',  ( -39.87592166654171422, -32.60641129436071850, 37.08344799359745991 ) ) ;
#10570 = VECTOR ( 'NONE', #93807, 1000.000000000000000 ) ;
#10571 = CARTESIAN_POINT ( 'NONE',  ( -35.39685905337628213, 18.64284798593103787, 14.96610495029052323 ) ) ;
#10572 = UNCERTAINTY_MEASURE_WITH_UNIT (LENGTH_MEASURE( 1.000000000000000082E-05 ), #64046, 'distance_accuracy_value', 'NONE');
#10573 = ORIENTED_EDGE ( 'NONE', *, *, #45932, .F. ) ;
#10574 = CARTESIAN_POINT ( 'NONE',  ( 0.000000000000000000, 0.000000000000000000, 0.000000000000000000 ) ) ;
#10575 = CARTESIAN_POINT ( 'NONE',  ( 7.808293529262138932, 53.96887308738315880, 3.792886552870250672 ) ) ;
#10576 = CARTESIAN_POINT ( 'NONE',  ( -6.499999999999999112, 3.752776749732556816, -6.064240316920397333 ) ) ;
#10577 = DIRECTION ( 'NONE',  ( -1.000000000000000000, -0.000000000000000000, -0.000000000000000000 ) ) ;
#10578 = EDGE_CURVE ( 'NONE', #46770, #93333, #22130, .T. ) ;
#10579 = CARTESIAN_POINT ( 'NONE',  ( 6.692588830498425345, 3.932766476276031486, 6.892929031562513131 ) ) ;
#10580 = CARTESIAN_POINT ( 'NONE',  ( -32.18945282278795617, 486.1438615785898492, 5.458730664921381148 ) ) ;
#10581 = ORIENTED_EDGE ( 'NONE', *, *, #99200, .T. ) ;
#10582 = VERTEX_POINT ( 'NONE', #89680 ) ;
#10583 = CARTESIAN_POINT ( 'NONE',  ( 97.79383724715447102, -30.00000000000014921, 190.7107357665381642 ) ) ;
#10584 = CARTESIAN_POINT ( 'NONE',  ( 31.91296609491446645, 40.84410790408901448, -63.71736666452449072 ) ) ;
#10585 = CARTESIAN_POINT ( 'NONE',  ( -4.660674839411966808, -83.68217514695594161, -3.778981567323765223 ) ) ;
#10586 = CARTESIAN_POINT ( 'NONE',  ( 81.97066485211418296, -30.00000000000000000, 33.64756664518507279 ) ) ;
#10587 = CARTESIAN_POINT ( 'NONE',  ( -25.78371382301346415, 306.9235641000283863, 10.63880919120126478 ) ) ;
#10588 = EDGE_LOOP ( 'NONE', ( #20571, #101809, #97698, #46960, #13358, #103817 ) ) ;
#10589 = ORIENTED_EDGE ( 'NONE', *, *, #80650, .F. ) ;
#10590 = ORIENTED_EDGE ( 'NONE', *, *, #19298, .F. ) ;
#10591 = CARTESIAN_POINT ( 'NONE',  ( -13.00000000000003730, -65.00000000000000000, 0.000000000000000000 ) ) ;
#10592 = DIRECTION ( 'NONE',  ( -1.000000000000000000, -1.224606353822377258E-16, -0.000000000000000000 ) ) ;
#10593 = CARTESIAN_POINT ( 'NONE',  ( -36.47299678459301475, 26.07223862938034387, -11.57805873600646329 ) ) ;
#10594 = CIRCLE ( 'NONE', #93293, 61.00000000000000000 ) ;
#10595 = CARTESIAN_POINT ( 'NONE',  ( 4.905018583967753365, -12.02359985679681742, -3.459768807258289502 ) ) ;
#10596 = CARTESIAN_POINT ( 'NONE',  ( -30.95268495340540937, 348.5034653024914064, 18.99969819225128020 ) ) ;
#10597 = CARTESIAN_POINT ( 'NONE',  ( -30.00000000000000000, 450.0000000000002274, 25.20242257375371864 ) ) ;
#10598 = ORIENTED_EDGE ( 'NONE', *, *, #100053, .F. ) ;
#10599 = CARTESIAN_POINT ( 'NONE',  ( 6.043427762771891310, 50.00000000000000000, -95.48543666094653304 ) ) ;
#10600 = VECTOR ( 'NONE', #78051, 1000.000000000000000 ) ;
#10601 = ORIENTED_EDGE ( 'NONE', *, *, #8758, .F. ) ;
#10602 = CARTESIAN_POINT ( 'NONE',  ( 4.699999999999999289, -5.629165124598853431, -3.249999999999994671 ) ) ;
#10603 = CARTESIAN_POINT ( 'NONE',  ( 77.52093042597508088, -38.51585880812307749, 186.5480975061236109 ) ) ;
#10604 = CARTESIAN_POINT ( 'NONE',  ( -33.00000000000000000, 485.0303364503728289, 0.9535057477320436625 ) ) ;
#10605 = CARTESIAN_POINT ( 'NONE',  ( 25.59799303312738061, 305.1324663277200102, 10.44726884554200375 ) ) ;
#10606 = CARTESIAN_POINT ( 'NONE',  ( 17.61650669486618881, 1.474610560812782335E-15, 0.000000000000000000 ) ) ;
#10607 = ORIENTED_EDGE ( 'NONE', *, *, #36911, .F. ) ;
#10608 = CARTESIAN_POINT ( 'NONE',  ( 29.33080127677424187, 13.52978328598926971, -39.65469037846457212 ) ) ;
#10609 = CARTESIAN_POINT ( 'NONE',  ( 17.81928184698852746, 45.39461501854594161, -4.975624619099646928 ) ) ;
#10610 = CARTESIAN_POINT ( 'NONE',  ( 21.19348424345033521, 294.8901562694577478, 1.945151701991110205 ) ) ;
#10611 = DIRECTION ( 'NONE',  ( 1.000000000000000000, 0.000000000000000000, -0.000000000000000000 ) ) ;
#10612 = ADVANCED_FACE ( 'NONE', ( #72423 ), #7668, .T. ) ;
#10613 = ORIENTED_EDGE ( 'NONE', *, *, #22675, .F. ) ;
#10614 = DIRECTION ( 'NONE',  ( 0.000000000000000000, 0.8660254037844375974, -0.5000000000000019984 ) ) ;
#10615 = DIRECTION ( 'NONE',  ( -1.000000000000000000, -1.224606353822377258E-16, -0.000000000000000000 ) ) ;
#10616 = CARTESIAN_POINT ( 'NONE',  ( 11.36650669486618881, 1.474610560812782335E-15, 0.000000000000000000 ) ) ;
#10617 = CARTESIAN_POINT ( 'NONE',  ( 19.00000000000001066, -4.000000000000000000, -2.500000000000000000 ) ) ;
#10618 = CARTESIAN_POINT ( 'NONE',  ( 34.64166250171380312, 490.4813561613898401, 11.60003975507685325 ) ) ;
#10619 = EDGE_CURVE ( 'NONE', #50381, #54238, #47604, .T. ) ;
#10620 = DIRECTION ( 'NONE',  ( 1.000000000000000000, 0.000000000000000000, 0.000000000000000000 ) ) ;
#10621 = EDGE_CURVE ( 'NONE', #40315, #54371, #72936, .T. ) ;
#10622 = CARTESIAN_POINT ( 'NONE',  ( 26.69900261086841198, 5.000000000000002665, 0.000000000000000000 ) ) ;
#10623 = CARTESIAN_POINT ( 'NONE',  ( 86.37697157886478294, -28.18731561469257940, 184.2989669348581288 ) ) ;
#10624 = CARTESIAN_POINT ( 'NONE',  ( 17.51195277503147452, 36.87917477456677062, -22.05183216906725363 ) ) ;
#10625 = CARTESIAN_POINT ( 'NONE',  ( -8.813577900860385839, 133.4610148809287864, -1.734723475955139846E-15 ) ) ;
#10626 = ORIENTED_EDGE ( 'NONE', *, *, #36730, .T. ) ;
#10627 = CARTESIAN_POINT ( 'NONE',  ( -7.500000000000005329, 4.330127018922183879, -7.564335161054492218 ) ) ;
#10628 = CYLINDRICAL_SURFACE ( 'NONE', #53890, 1.250000000000000000 ) ;
#10629 = FACE_OUTER_BOUND ( 'NONE', #97010, .T. ) ;
#10630 = EDGE_CURVE ( 'NONE', #66517, #43629, #76277, .T. ) ;
#10631 = CARTESIAN_POINT ( 'NONE',  ( -86.45571998004572833, -29.99999999999999645, 67.09524892540846963 ) ) ;
#10632 = FACE_OUTER_BOUND ( 'NONE', #53528, .T. ) ;
#10633 = DIRECTION ( 'NONE',  ( -0.5735764363510461594, 0.8191520442889916875, 1.003171929053524870E-16 ) ) ;
#10635 =( NAMED_UNIT ( * ) SI_UNIT ( $, .STERADIAN. ) SOLID_ANGLE_UNIT ( ) );
#10634 = CARTESIAN_POINT ( 'NONE',  ( 37.50059943756144776, 490.7879993827856993, 12.38039871356534505 ) ) ;
#10636 = AXIS2_PLACEMENT_3D ( 'NONE', #91440, #9416, #82800 ) ;
#10637 = LINE ( 'NONE', #84011, #2287 ) ;
#10638 = CARTESIAN_POINT ( 'NONE',  ( -11.42066797802348077, -21.20489296322393002, 27.45196823644660000 ) ) ;
#10639 = CARTESIAN_POINT ( 'NONE',  ( 14.91270732344407257, 41.98564553269472555, -86.62216337287246404 ) ) ;
#10640 = CARTESIAN_POINT ( 'NONE',  ( -43.03987588564135081, 486.0760633267553317, 5.817066388976053659 ) ) ;
#10641 = LINE ( 'NONE', #3099, #49404 ) ;
#10642 = CARTESIAN_POINT ( 'NONE',  ( 55.98375673512529715, -28.65874727311520687, -26.28204123211169829 ) ) ;
#10643 = CARTESIAN_POINT ( 'NONE',  ( -24.76425723927362554, -36.00077592485400402, 31.10340529209751637 ) ) ;
#10644 = VERTEX_POINT ( 'NONE', #23370 ) ;
#10645 = CARTESIAN_POINT ( 'NONE',  ( 6.692588830498428898, -7.935834885954430540, 0.04058884017440032160 ) ) ;
#10646 = CARTESIAN_POINT ( 'NONE',  ( -9.380894568449075877, 107.0113063311094237, -3.467341429141166831 ) ) ;
#10647 = CARTESIAN_POINT ( 'NONE',  ( -16.70090518186424333, -35.99505156839033759, 30.12198634049419965 ) ) ;
#10648 = CARTESIAN_POINT ( 'NONE',  ( -63.90368348448107128, -29.66094596946048512, -23.51237261270683021 ) ) ;
#10650 = CARTESIAN_POINT ( 'NONE',  ( 4.387778976649723378E-15, 29.08768991669519721, -35.82893434829263413 ) ) ;
#10649 = CARTESIAN_POINT ( 'NONE',  ( -1.100802702663628896, 27.96907460577615012, 38.88676574253319274 ) ) ;
#10651 = VERTEX_POINT ( 'NONE', #98290 ) ;
#10652 = CARTESIAN_POINT ( 'NONE',  ( -35.51073831230387157, 436.6043880790006710, 4.950196615276987622 ) ) ;
#10653 = VERTEX_POINT ( 'NONE', #80499 ) ;
#10654 = CARTESIAN_POINT ( 'NONE',  ( 0.000000000000000000, 0.9999999999999970024, 0.000000000000000000 ) ) ;
#10655 = AXIS2_PLACEMENT_3D ( 'NONE', #75717, #59017, #66033 ) ;
#10656 = EDGE_CURVE ( 'NONE', #25416, #81100, #18317, .T. ) ;
#10657 = CONICAL_SURFACE ( 'NONE', #64058, 4.000000000000001776, 0.9599310885968808105 ) ;
#10658 = CARTESIAN_POINT ( 'NONE',  ( 15.05785784214677037, 3.824195276769946972, 4.604276673498408634 ) ) ;
#10659 = DIRECTION ( 'NONE',  ( -1.000000000000000000, -1.224606353822377258E-16, -0.000000000000000000 ) ) ;
#10660 = ORIENTED_EDGE ( 'NONE', *, *, #8530, .T. ) ;
#10661 = SURFACE_SIDE_STYLE ('',( #34986 ) ) ;
#10662 = CARTESIAN_POINT ( 'NONE',  ( 0.000000000000000000, 50.00000000000000000, -97.00000000000000000 ) ) ;
#10663 = CARTESIAN_POINT ( 'NONE',  ( 100.3691303487159416, -52.75941910667004464, 193.9373745264102240 ) ) ;
#10665 = CARTESIAN_POINT ( 'NONE',  ( -7.002990960197235104, -8.947331816165435825, 3.868040364119522234 ) ) ;
#10664 = CARTESIAN_POINT ( 'NONE',  ( 2.806318047554528849, 294.8278478787091785, -9.615287951362873287 ) ) ;
#10666 = ORIENTED_EDGE ( 'NONE', *, *, #24537, .T. ) ;
#10667 = ORIENTED_EDGE ( 'NONE', *, *, #80082, .F. ) ;
#10668 = ORIENTED_EDGE ( 'NONE', *, *, #91480, .F. ) ;
#10669 = CARTESIAN_POINT ( 'NONE',  ( 24.88870436626125837, 307.3804518054343475, 10.51319220944573729 ) ) ;
#10670 = EDGE_CURVE ( 'NONE', #3869, #70831, #100369, .T. ) ;
#10671 = CARTESIAN_POINT ( 'NONE',  ( 4.699999999999999289, 3.752776749732553263, -6.499999999999999112 ) ) ;
#10672 = CARTESIAN_POINT ( 'NONE',  ( 15.56661972382058501, 46.04807679453924152, 6.063442319127587687 ) ) ;
#10673 = ORIENTED_EDGE ( 'NONE', *, *, #79542, .T. ) ;
#10674 = B_SPLINE_CURVE_WITH_KNOTS ( 'NONE', 3,
 ( #74249, #100653, #325, #84486, #67766, #26813, #66701, #82882, #83407, #92034, #51029, #33289 ),
 .UNSPECIFIED., .F., .F.,
 ( 4, 2, 2, 2, 2, 4 ),
 ( 1.829968831002800917E-16, 0.002066773779721026074, 0.004133547559441869135, 0.005166934449302291316, 0.006200321339162713496, 0.008267095118883622043 ),
 .UNSPECIFIED. ) ;
#10675 = CARTESIAN_POINT ( 'NONE',  ( -42.57704743493907529, 486.1612337113410831, 7.852296464539637810 ) ) ;
#10676 = CARTESIAN_POINT ( 'NONE',  ( 0.000000000000000000, 0.000000000000000000, -10.00000000000000000 ) ) ;
#10677 = DIRECTION ( 'NONE',  ( 0.000000000000000000, -1.000000000000000000, 0.000000000000000000 ) ) ;
#10678 = CARTESIAN_POINT ( 'NONE',  ( -102.2519545932779010, -60.00000000013668000, 80.19353485699372186 ) ) ;
#10679 = CARTESIAN_POINT ( 'NONE',  ( 7.344361273354517827, -67.44560530588525182, -3.175733139645580128 ) ) ;
#10680 = CARTESIAN_POINT ( 'NONE',  ( -34.94338628507543376, 342.5355909536760350, -0.9693026116843473927 ) ) ;
#10681 = DIRECTION ( 'NONE',  ( -0.5735764363510497121, 0.8191520442889892450, 1.003171929053521665E-16 ) ) ;
#10682 = CARTESIAN_POINT ( 'NONE',  ( -86.47621369144106040, -14.21045842199425735, -14.66750133381012589 ) ) ;
#10683 =( NAMED_UNIT ( * ) PLANE_ANGLE_UNIT ( ) SI_UNIT ( $, .RADIAN. ) );
#10684 = CARTESIAN_POINT ( 'NONE',  ( -50.93686057180333648, -53.37436350439492116, 57.23435777560519000 ) ) ;
#10685 = VERTEX_POINT ( 'NONE', #88613 ) ;
#10686 = DIRECTION ( 'NONE',  ( 0.000000000000000000, -1.000000000000000000, 0.000000000000000000 ) ) ;
#10687 = ORIENTED_EDGE ( 'NONE', *, *, #68314, .T. ) ;
#10688 = LINE ( 'NONE', #3151, #78753 ) ;
#10689 = EDGE_CURVE ( 'NONE', #160, #77143, #4560, .T. ) ;
#10690 = CARTESIAN_POINT ( 'NONE',  ( -9.549008551970846526, 295.0805096965098642, -10.04182235106918952 ) ) ;
#10691 = EDGE_CURVE ( 'NONE', #69383, #14419, #4526, .T. ) ;
#10692 = FACE_BOUND ( 'NONE', #75750, .T. ) ;
#10693 = VERTEX_POINT ( 'NONE', #64862 ) ;
#10694 = CARTESIAN_POINT ( 'NONE',  ( 4.814352310392297163, 248.2032140589641642, -3.583053941560760958 ) ) ;
#10695 = CARTESIAN_POINT ( 'NONE',  ( 96.06728777640114458, -38.48540547217477581, 201.2030628861659807 ) ) ;
#10696 = CARTESIAN_POINT ( 'NONE',  ( 9.349999999999997868, 1.533819458162526451E-15, 0.000000000000000000 ) ) ;
#10697 = CARTESIAN_POINT ( 'NONE',  ( 3.707709148205156957, -48.90047616793709295, 104.5934084724877948 ) ) ;
#10698 = AXIS2_PLACEMENT_3D ( 'NONE', #11410, #13003, #44335 ) ;
#10699 = LINE ( 'NONE', #83011, #28978 ) ;
#10700 = CARTESIAN_POINT ( 'NONE',  ( 55.65414010180120385, 42.00000000000000000, -72.41885610122511707 ) ) ;
#10701 = CARTESIAN_POINT ( 'NONE',  ( 86.13034586361173695, -29.99999999999999645, 179.4755604668315812 ) ) ;
#10702 = CIRCLE ( 'NONE', #96807, 2.000000000000001776 ) ;
#10703 = CARTESIAN_POINT ( 'NONE',  ( 85.31310517497098544, 1.030564683017419500E-14, 0.000000000000000000 ) ) ;
#10704 = VERTEX_POINT ( 'NONE', #56208 ) ;
#10705 = EDGE_LOOP ( 'NONE', ( #24940, #73315, #57812, #55537, #103982, #31203 ) ) ;
#10706 = CARTESIAN_POINT ( 'NONE',  ( 51.90082211129554679, -18.71876729291939512, 46.78542853416100655 ) ) ;
#10707 = CARTESIAN_POINT ( 'NONE',  ( 6.970005868343639222, 41.38563980255786845, -58.64823803489037601 ) ) ;
#10708 = PRESENTATION_LAYER_ASSIGNMENT (  '', '', ( #57200 ) ) ;
#10709 = CARTESIAN_POINT ( 'NONE',  ( -7.500000000000007105, 40.00000000000000000, -58.09827136975972905 ) ) ;
#10710 = AXIS2_PLACEMENT_3D ( 'NONE', #89848, #96366, #76307 ) ;
#10711 = ORIENTED_EDGE ( 'NONE', *, *, #44818, .T. ) ;
#10712 = CARTESIAN_POINT ( 'NONE',  ( -91.25706933832147172, -38.36172668882709758, -1.507939045793343702 ) ) ;
#10713 = VERTEX_POINT ( 'NONE', #79975 ) ;
#10714 = DIRECTION ( 'NONE',  ( -1.000000000000000000, 0.000000000000000000, 0.000000000000000000 ) ) ;
#10715 = CARTESIAN_POINT ( 'NONE',  ( 106.8950883828628946, -38.36540791790844196, 195.0233813272650139 ) ) ;
#10716 = CARTESIAN_POINT ( 'NONE',  ( 13.60307364985986744, 22.67980367822178067, -2.541457539100715923 ) ) ;
#10717 = CARTESIAN_POINT ( 'NONE',  ( 85.13574873232160201, -45.28282078271436717, 36.04402567606572916 ) ) ;
#10718 = CARTESIAN_POINT ( 'NONE',  ( -4.651132217449170270, -5.000000000000000000, -15.66661053588738106 ) ) ;
#10719 = CARTESIAN_POINT ( 'NONE',  ( -25.13271562044587526, 306.2273044284306707, -9.700012334803982839 ) ) ;
#10720 = CARTESIAN_POINT ( 'NONE',  ( 3.684569285724539789, -8.676863831076616407, -12.27927943165980551 ) ) ;
#10721 = APPLICATION_CONTEXT ( 'automotive_design' ) ;
#10722 = CARTESIAN_POINT ( 'NONE',  ( -24.42503034277509499, 25.46443454461794076, -31.59611462731667331 ) ) ;
#10723 = CARTESIAN_POINT ( 'NONE',  ( -43.00000000000000000, 464.8825480873695710, 15.07585856869432206 ) ) ;
#10724 = CARTESIAN_POINT ( 'NONE',  ( 3.225607053687307602, 115.6489559503065152, 5.000000000000000000 ) ) ;
#10725 = EDGE_LOOP ( 'NONE', ( #38492, #67256, #14380, #73212, #92357, #83629, #98527 ) ) ;
#10726 = CYLINDRICAL_SURFACE ( 'NONE', #49876, 7.000000000000000000 ) ;
#10727 = DIRECTION ( 'NONE',  ( -0.000000000000000000, -0.000000000000000000, 1.000000000000000000 ) ) ;
#10728 = AXIS2_PLACEMENT_3D ( 'NONE', #14983, #57033, #47878 ) ;
#10729 = CARTESIAN_POINT ( 'NONE',  ( -44.48436518344863799, 465.3427600001859332, 9.644189083065656476 ) ) ;
#10730 = VERTEX_POINT ( 'NONE', #89146 ) ;
#10731 = CARTESIAN_POINT ( 'NONE',  ( 27.33349330513380693, -3.851859888774471706E-31, 4.000000000000001776 ) ) ;
#10732 = CARTESIAN_POINT ( 'NONE',  ( -27.91514439139539405, 308.8047814446088069, 11.33986536342479390 ) ) ;
#10733 = CARTESIAN_POINT ( 'NONE',  ( -12.11400133237649968, -4.683782139512427278, -76.82602898264141800 ) ) ;
#10734 = CYLINDRICAL_SURFACE ( 'NONE', #12806, 4.000000000000000000 ) ;
#10735 = CARTESIAN_POINT ( 'NONE',  ( -8.000000000000001776, -28.15625000000000000, 3.313708498984758943 ) ) ;
#10736 = COLOUR_RGB ( '', 0.72549020, 0.75294118, 0.79215686) ;
#10737 = SURFACE_SIDE_STYLE ('',( #51735 ) ) ;
#10738 = LINE ( 'NONE', #2652, #3593 ) ;
#10739 = VECTOR ( 'NONE', #87692, 1000.000000000000000 ) ;
#10740 = ORIENTED_EDGE ( 'NONE', *, *, #96302, .T. ) ;
#10741 = CARTESIAN_POINT ( 'NONE',  ( 85.31399179591240056, -28.76387208470135093, 175.9376541799884421 ) ) ;
#10742 = CARTESIAN_POINT ( 'NONE',  ( 34.35000000000000142, -3.309499999999999886, 4.475777889183790779E-16 ) ) ;
#10743 = FACE_OUTER_BOUND ( 'NONE', #37690, .T. ) ;
#10744 = ORIENTED_EDGE ( 'NONE', *, *, #1253, .T. ) ;
#10745 = CARTESIAN_POINT ( 'NONE',  ( -89.59862634610074394, -60.15398014766234525, 51.74679006964829142 ) ) ;
#10746 = PRESENTATION_STYLE_ASSIGNMENT (( #86803 ) ) ;
#10747 = CARTESIAN_POINT ( 'NONE',  ( 32.62207953394533178, 6.123233995736772199E-16, -5.000000000000001776 ) ) ;
#10748 = CARTESIAN_POINT ( 'NONE',  ( 18.91736802153303998, 304.6924624432400606, 8.903130582026813400 ) ) ;
#10749 = ADVANCED_FACE ( 'NONE', ( #40059 ), #23532, .T. ) ;
#10750 = CARTESIAN_POINT ( 'NONE',  ( -23.21907688075229714, -27.03733090009978213, -38.42007954425987037 ) ) ;
#10751 = EDGE_CURVE ( 'NONE', #1743, #15047, #42744, .T. ) ;
#10752 = CARTESIAN_POINT ( 'NONE',  ( 41.55847581142891300, -60.00000000000000000, 54.44581446459392282 ) ) ;
#10753 = CARTESIAN_POINT ( 'NONE',  ( 26.92113802654871435, -30.35670355970656686, 39.03432911242002490 ) ) ;
#10754 = DIRECTION ( 'NONE',  ( 0.000000000000000000, -1.000000000000000000, 0.000000000000000000 ) ) ;
#10756 = CARTESIAN_POINT ( 'NONE',  ( -11.00368196113950781, 16.88294327153011309, 9.222626775518351749 ) ) ;
#10755 = CARTESIAN_POINT ( 'NONE',  ( -37.01124464218769106, -36.50269617998545613, 46.22989763715360567 ) ) ;
#10757 = CARTESIAN_POINT ( 'NONE',  ( 0.6398555294277069594, 296.1023409384113734, -10.00028515034549592 ) ) ;
#10758 = CARTESIAN_POINT ( 'NONE',  ( 5.082755093536324154, -10.34375000204838457, 5.082755093536326818 ) ) ;
#10759 = PLANE ( 'NONE',  #87132 ) ;
#10760 = ADVANCED_FACE ( 'NONE', ( #615 ), #87257, .T. ) ;
#10761 = CARTESIAN_POINT ( 'NONE',  ( 103.5111111111111057, 1.023464760207051730E-14, 0.000000000000000000 ) ) ;
#10762 = CIRCLE ( 'NONE', #40269, 5.000000000000011546 ) ;
#10763 = VERTEX_POINT ( 'NONE', #18466 ) ;
#10764 = CARTESIAN_POINT ( 'NONE',  ( 5.979512004945818582, -4.053280633787088583, -0.5609245978742307681 ) ) ;
#10765 = CARTESIAN_POINT ( 'NONE',  ( -17.49999999999998579, 51.30660076971290096, 62.83706383106828497 ) ) ;
#10766 = DIRECTION ( 'NONE',  ( -1.000000000000000000, -1.224606353822377258E-16, -0.000000000000000000 ) ) ;
#10767 = CARTESIAN_POINT ( 'NONE',  ( 37.20098947014512447, 438.1443347308020293, 4.012567541587164222 ) ) ;
#10769 = CARTESIAN_POINT ( 'NONE',  ( 12.77004905764128928, -47.40885985275529180, -34.44498021351899553 ) ) ;
#10768 = CARTESIAN_POINT ( 'NONE',  ( 9.176855344543007220, 250.5296042697742109, -3.973472207155925862 ) ) ;
#10770 = VERTEX_POINT ( 'NONE', #58365 ) ;
#10771 = CARTESIAN_POINT ( 'NONE',  ( -44.32938218976925526, 463.8543910928598848, 7.949978264524292904 ) ) ;
#10772 = CARTESIAN_POINT ( 'NONE',  ( 1.000000000000000444, -69.90918681875037066, 12.94764124286841067 ) ) ;
#10773 = ORIENTED_EDGE ( 'NONE', *, *, #57096, .F. ) ;
#10774 = FACE_OUTER_BOUND ( 'NONE', #91153, .T. ) ;
#10775 = EDGE_CURVE ( 'NONE', #37699, #33537, #27104, .T. ) ;
#10776 = CARTESIAN_POINT ( 'NONE',  ( -6.338673264423879239, 41.81695718870634693, -59.02782128990620691 ) ) ;
#10777 = CARTESIAN_POINT ( 'NONE',  ( 27.33349330513380337, -4.000000000000000888, 4.898587196589416773E-16 ) ) ;
#10778 = CARTESIAN_POINT ( 'NONE',  ( -93.65395957099387658, -59.99999999999999289, 38.40458741383176289 ) ) ;
#10779 = CARTESIAN_POINT ( 'NONE',  ( -46.00000000000000000, 450.0000000000002274, 1.202422573753698876 ) ) ;
#10780 = CARTESIAN_POINT ( 'NONE',  ( 5.276765049035075705, -6.073111908730308706, -7.634085501268430107 ) ) ;
#10781 = CARTESIAN_POINT ( 'NONE',  ( 35.76482652855951017, 405.2378813769876729, 6.148826621638260548 ) ) ;
#10782 = CARTESIAN_POINT ( 'NONE',  ( 40.11988102503458009, 460.2461986766708719, 2.235918385956437326 ) ) ;
#10784 = SURFACE_STYLE_USAGE ( .BOTH. , #36195 ) ;
#10783 = CARTESIAN_POINT ( 'NONE',  ( 1.308996937480704670, -3.000000000000002665, -95.00000000000000000 ) ) ;
#10785 = CARTESIAN_POINT ( 'NONE',  ( -83.05624746893637678, -42.97990360462496540, 175.6772798865610525 ) ) ;
#10786 = ORIENTED_EDGE ( 'NONE', *, *, #7708, .T. ) ;
#10787 = FACE_OUTER_BOUND ( 'NONE', #46882, .T. ) ;
#10788 = ORIENTED_EDGE ( 'NONE', *, *, #22711, .F. ) ;
#10789 = ORIENTED_EDGE ( 'NONE', *, *, #59454, .T. ) ;
#10790 = CARTESIAN_POINT ( 'NONE',  ( -18.99999999999999289, -5.000000000000000000, -1.500000000000001332 ) ) ;
#10792 =( BOUNDED_SURFACE ( )  B_SPLINE_SURFACE ( 3, 2, ( 
 ( #39531, #71341, #89130 ),
 ( #104236, #105829, #81529 ),
 ( #104777, #7654, #40571 ),
 ( #73453, #63806, #32513 ) ),
 .UNSPECIFIED., .F., .F., .T. ) 
 B_SPLINE_SURFACE_WITH_KNOTS ( ( 4, 4 ),
 ( 3, 3 ),
 ( 6.559423143537301826E-18, 0.0001614739849780087732 ),
 ( 0.000000000000000000, 1.000000000000000000 ),
 .UNSPECIFIED. ) 
 GEOMETRIC_REPRESENTATION_ITEM ( )  RATIONAL_B_SPLINE_SURFACE ( (
 ( 1.000000000000000000, 0.9028401456532985092, 1.000000000000000000),
 ( 1.000000000000000000, 0.9031964952773765543, 1.000000000000000000),
 ( 1.000000000000000000, 0.9035643897146851122, 1.000000000000000000),
 ( 1.000000000000000000, 0.9039444415359824125, 1.000000000000000000) ) ) 
 REPRESENTATION_ITEM ( '' )  SURFACE ( )  );
#10791 = CARTESIAN_POINT ( 'NONE',  ( 7.255520619061520016, -4.332661967062336750, 16.69105336089074854 ) ) ;
#10793 = ADVANCED_FACE ( 'NONE', ( #26056 ), #106155, .T. ) ;
#10794 = CARTESIAN_POINT ( 'NONE',  ( 13.50000000000000533, -7.794228634059982674, -11.79422863405993382 ) ) ;
#10795 = EDGE_LOOP ( 'NONE', ( #45224, #52671, #34948, #41171, #93834 ) ) ;
#10796 = STYLED_ITEM ( 'NONE', ( #37067 ), #75546 ) ;
#10797 = DIRECTION ( 'NONE',  ( -1.000000000000000000, 0.000000000000000000, 0.000000000000000000 ) ) ;
#10798 = CARTESIAN_POINT ( 'NONE',  ( -111.7589076751911392, -57.67119524614439285, 141.4413276519820784 ) ) ;
#10799 = CARTESIAN_POINT ( 'NONE',  ( 7.619135598915497631, -13.17305367784679859, 2.449260492474792272 ) ) ;
#10800 = CARTESIAN_POINT ( 'NONE',  ( 12.33349330513380337, 4.000000000000003553, 0.000000000000000000 ) ) ;
#10801 =( GEOMETRIC_REPRESENTATION_CONTEXT ( 3 ) GLOBAL_UNCERTAINTY_ASSIGNED_CONTEXT ( ( #51332 ) ) GLOBAL_UNIT_ASSIGNED_CONTEXT ( ( #68050, #84771, #76664 ) ) REPRESENTATION_CONTEXT ( 'NONE', 'WORKASPACE' ) );
#10802 = CARTESIAN_POINT ( 'NONE',  ( 100.0424503805845831, 1.016364837396684119E-14, 0.000000000000000000 ) ) ;
#10803 = FILL_AREA_STYLE_COLOUR ( '', #35603 ) ;
#10804 = DIRECTION ( 'NONE',  ( 0.5735764363510468256, 0.8191520442889913545, 0.000000000000000000 ) ) ;
#10805 = CARTESIAN_POINT ( 'NONE',  ( 108.9225596800844897, -59.99999999999995737, 119.6931403564588123 ) ) ;
#10806 = CARTESIAN_POINT ( 'NONE',  ( -77.40171858393368609, -14.21045842199445630, 153.6868182409262431 ) ) ;
#10807 = CARTESIAN_POINT ( 'NONE',  ( -57.84207542031359139, -46.44074207334602278, 69.91486170460251515 ) ) ;
#10808 = ORIENTED_EDGE ( 'NONE', *, *, #11698, .F. ) ;
#10809 = CARTESIAN_POINT ( 'NONE',  ( 5.835236874069059887, 14.05646090491896594, 3.867049007331976540 ) ) ;
#10810 = EDGE_LOOP ( 'NONE', ( #82918, #81804, #5505, #33018 ) ) ;
#10811 = CARTESIAN_POINT ( 'NONE',  ( -103.1567554067950141, -45.26542592305720802, 184.6143969872866819 ) ) ;
#10812 = EDGE_CURVE ( 'NONE', #90027, #93494, #76135, .T. ) ;
#10813 = CARTESIAN_POINT ( 'NONE',  ( 14.81716630709848737, 41.99561238121396656, -87.50450243860541377 ) ) ;
#10814 = ORIENTED_EDGE ( 'NONE', *, *, #103889, .T. ) ;
#10815 = DIRECTION ( 'NONE',  ( 1.000000000000000000, 1.224606353822377258E-16, 0.000000000000000000 ) ) ;
#10816 = CARTESIAN_POINT ( 'NONE',  ( -54.47032963692922891, -60.00000000000001421, 83.72682086598487672 ) ) ;
#10817 = CARTESIAN_POINT ( 'NONE',  ( 36.32858960327170905, 26.02883040073359666, -12.39689931504920395 ) ) ;
#10818 = CARTESIAN_POINT ( 'NONE',  ( -1.320432766682874540E-15, -12.40625000204838635, 7.188101187500000044 ) ) ;
#10819 = CARTESIAN_POINT ( 'NONE',  ( -0.7827516548123796269, 37.11091899138959604, -27.51176826853287594 ) ) ;
#10820 = PRESENTATION_STYLE_ASSIGNMENT (( #2201 ) ) ;
#10821 = CARTESIAN_POINT ( 'NONE',  ( 16.14659623658357290, 0.000000000000000000, -5.483224646668203306 ) ) ;
#10822 = CARTESIAN_POINT ( 'NONE',  ( -11.16469478931291448, -4.978653580250081312, -12.57749972225050072 ) ) ;
#10823 = CARTESIAN_POINT ( 'NONE',  ( 0.000000000000000000, -46.00000000000000000, 112.0000000000000000 ) ) ;
#10824 = EDGE_CURVE ( 'NONE', #78207, #89572, #35618, .T. ) ;
#10825 = CARTESIAN_POINT ( 'NONE',  ( 5.722593143194981913, -7.814937950054605231, 13.77127656069876771 ) ) ;
#10826 = CARTESIAN_POINT ( 'NONE',  ( -15.39075092899651942, 46.20845424323130146, -5.262406961020227314 ) ) ;
#10827 = CARTESIAN_POINT ( 'NONE',  ( 13.88435755492751511, 42.00000000000000000, -90.88030988993200765 ) ) ;
#10828 = CARTESIAN_POINT ( 'NONE',  ( -29.96432046203353394, -56.86175435685562718, 36.18131803398338064 ) ) ;
#10829 = CARTESIAN_POINT ( 'NONE',  ( 43.12828152119622160, -42.98012150843932488, 42.46846544478599839 ) ) ;
#10830 = CARTESIAN_POINT ( 'NONE',  ( 68.45015997180047407, 6.975173280561618775E-15, 0.000000000000000000 ) ) ;
#10831 = EDGE_CURVE ( 'NONE', #71976, #83228, #94128, .T. ) ;
#10832 = CARTESIAN_POINT ( 'NONE',  ( -5.834906339164276368, 14.05456999085811631, 3.867544450381312338 ) ) ;
#10833 = CARTESIAN_POINT ( 'NONE',  ( -90.57426512392396489, -38.51016351068651744, 200.7127688951560174 ) ) ;
#10834 = ORIENTED_EDGE ( 'NONE', *, *, #15481, .T. ) ;
#10836 = CARTESIAN_POINT ( 'NONE',  ( 83.86866073052654258, 5.000000000000020428, 0.000000000000000000 ) ) ;
#10835 = CARTESIAN_POINT ( 'NONE',  ( -16.14595037822608248, 20.23371447308014481, 4.922994507609256054 ) ) ;
#10837 = CARTESIAN_POINT ( 'NONE',  ( 2.087952376091057438, -59.99999999999998579, 33.88964995960238014 ) ) ;
#10839 = EDGE_CURVE ( 'NONE', #3581, #84046, #65845, .T. ) ;
#10838 = CARTESIAN_POINT ( 'NONE',  ( -48.80467726777875015, 9.660151405757225973, -14.61811727277458495 ) ) ;
#10840 = CARTESIAN_POINT ( 'NONE',  ( -7.341136682164572491, 41.28570584283517064, -59.23704219074569721 ) ) ;
#10841 = CARTESIAN_POINT ( 'NONE',  ( 6.731385056190076099, 41.26098032358547840, -70.78618130126719166 ) ) ;
#10842 = FACE_OUTER_BOUND ( 'NONE', #103040, .T. ) ;
#10844 = CARTESIAN_POINT ( 'NONE',  ( -20.45609435626379380, 304.8998821832971657, 8.947188782534524876 ) ) ;
#10843 = PRESENTATION_LAYER_ASSIGNMENT (  '', '', ( #57337 ) ) ;
#10845 = CARTESIAN_POINT ( 'NONE',  ( 31.35596682365711274, 438.0939828603570732, 22.55458131664589061 ) ) ;
#10846 = CARTESIAN_POINT ( 'NONE',  ( 106.6141358215111268, -59.99999999999999289, 197.5847826952339688 ) ) ;
#10848 = CARTESIAN_POINT ( 'NONE',  ( 6.333820801334183237, -4.275724398228409662, 5.594228103108734196 ) ) ;
#10847 = AXIS2_PLACEMENT_3D ( 'NONE', #58286, #35113, #9719 ) ;
#10849 = EDGE_CURVE ( 'NONE', #79592, #74189, #1709, .T. ) ;
#10850 = AXIS2_PLACEMENT_3D ( 'NONE', #42365, #106564, #32715 ) ;
#10851 = FACE_OUTER_BOUND ( 'NONE', #20186, .T. ) ;
#10852 = ORIENTED_EDGE ( 'NONE', *, *, #18048, .T. ) ;
#10853 = CARTESIAN_POINT ( 'NONE',  ( 36.31162387720077334, 438.2523736922215676, 3.875403351156465614 ) ) ;
#10854 = CARTESIAN_POINT ( 'NONE',  ( -81.48499160583682510, -29.99999999999999289, -3.293153312921696330 ) ) ;
#10855 = VERTEX_POINT ( 'NONE', #98807 ) ;
#10857 = CARTESIAN_POINT ( 'NONE',  ( -1.715570313355245569, -4.332661967060489339, -17.83376356531591256 ) ) ;
#10856 = CARTESIAN_POINT ( 'NONE',  ( -74.02947286502273982, -38.32606267584065307, 160.4867843101843903 ) ) ;
#10858 = CARTESIAN_POINT ( 'NONE',  ( 42.51410301897681165, 462.6487061729961283, 3.764838390842401239 ) ) ;
#10859 = CARTESIAN_POINT ( 'NONE',  ( 6.907083959255991168, 41.55068448857264229, -58.85924345847777062 ) ) ;
#10860 = PRESENTATION_LAYER_ASSIGNMENT (  '', '', ( #79771 ) ) ;
#10861 = CARTESIAN_POINT ( 'NONE',  ( 7.188101187500001821, -19.43750000204838457, -2.977408999572650483 ) ) ;
#10862 = CARTESIAN_POINT ( 'NONE',  ( -10.48543666094732352, -5.000000000000002665, -78.95657223722187723 ) ) ;
#10863 = CARTESIAN_POINT ( 'NONE',  ( 89.64643850830432825, -5.000000000000000888, 6.123233995736779101E-16 ) ) ;
#10865 = ORIENTED_EDGE ( 'NONE', *, *, #16070, .F. ) ;
#10864 = DIRECTION ( 'NONE',  ( 0.000000000000000000, 1.000000000000000000, -0.000000000000000000 ) ) ;
#10866 = CARTESIAN_POINT ( 'NONE',  ( 83.92759608957032924, -29.05489278753509552, 161.8030344486882086 ) ) ;
#10867 = CARTESIAN_POINT ( 'NONE',  ( 0.000000000000000000, -5.629165124598848990, -3.250000000000003553 ) ) ;
#10868 = CARTESIAN_POINT ( 'NONE',  ( 36.36650669486618881, 1.474610560812782335E-15, 0.000000000000000000 ) ) ;
#10869 = EDGE_LOOP ( 'NONE', ( #89444, #59402, #32070, #30606, #40797, #85016 ) ) ;
#10870 = FACE_OUTER_BOUND ( 'NONE', #51454, .T. ) ;
#10871 = PRESENTATION_LAYER_ASSIGNMENT (  '', '', ( #21319 ) ) ;
#10872 = CARTESIAN_POINT ( 'NONE',  ( -0.3577666611213474179, 18.74973685375030641, -49.30079757914840854 ) ) ;
#10873 = DIRECTION ( 'NONE',  ( -0.5735764363510512664, 0.8191520442889881348, 1.003171929053520309E-16 ) ) ;
#10874 = LINE ( 'NONE', #84792, #53755 ) ;
#10875 = FILL_AREA_STYLE ('',( #50805 ) ) ;
#10876 = CARTESIAN_POINT ( 'NONE',  ( 16.96276686007057322, 43.64335858091297382, 4.157797401561411199 ) ) ;
#10877 =( LENGTH_UNIT ( ) NAMED_UNIT ( * ) SI_UNIT ( .MILLI., .METRE. ) );
#10878 = ADVANCED_FACE ( 'NONE', ( #84772 ), #34663, .T. ) ;
#10879 = ORIENTED_EDGE ( 'NONE', *, *, #52609, .T. ) ;
#10880 = COLOUR_RGB ( '', 0.72549020, 0.75294118, 0.79215686) ;
#10881 =( NAMED_UNIT ( * ) SI_UNIT ( $, .STERADIAN. ) SOLID_ANGLE_UNIT ( ) );
#10882 = AXIS2_PLACEMENT_3D ( 'NONE', #16051, #17137, #81301 ) ;
#10883 = FACE_BOUND ( 'NONE', #25900, .T. ) ;
#10884 = EDGE_CURVE ( 'NONE', #58075, #71976, #50363, .T. ) ;
#10885 = CARTESIAN_POINT ( 'NONE',  ( 23.07257312861869281, 18.64284798592816017, 30.73399254005308734 ) ) ;
#10886 = CARTESIAN_POINT ( 'NONE',  ( 87.22190787708925086, -35.38180814089842841, 188.6303834557791390 ) ) ;
#10887 = CARTESIAN_POINT ( 'NONE',  ( 5.082755093536325930, -27.96875000204838457, -5.082755093536325042 ) ) ;
#10888 = CARTESIAN_POINT ( 'NONE',  ( -42.99999999999852207, 487.9285348210879647, 8.903916466045032507 ) ) ;
#10889 = DIRECTION ( 'NONE',  ( 0.000000000000000000, -1.000000000000000000, 0.000000000000000000 ) ) ;
#10890 = SURFACE_STYLE_FILL_AREA ( #100452 ) ;
#10891 = ORIENTED_EDGE ( 'NONE', *, *, #96365, .T. ) ;
#10892 = CARTESIAN_POINT ( 'NONE',  ( 38.47428897412579119, 485.7788508071993760, -4.770630528148342542 ) ) ;
#10893 = DIRECTION ( 'NONE',  ( -1.096832036894112098E-16, 0.000000000000000000, -1.000000000000000000 ) ) ;
#10894 = CARTESIAN_POINT ( 'NONE',  ( -9.999806008771985333, 7.500277120289516652, 0.000000000000000000 ) ) ;
#10895 = CYLINDRICAL_SURFACE ( 'NONE', #94624, 5.000000000000002665 ) ;
#10896 = EDGE_CURVE ( 'NONE', #97744, #80543, #37319, .T. ) ;
#10897 = ORIENTED_EDGE ( 'NONE', *, *, #39854, .F. ) ;
#10898 = CARTESIAN_POINT ( 'NONE',  ( 0.000000000000000000, 0.000000000000000000, -3.432199999999999918 ) ) ;
#10899 = CARTESIAN_POINT ( 'NONE',  ( -33.95909125837312104, 464.3583096732938316, 17.59538848557463453 ) ) ;
#10900 = DIRECTION ( 'NONE',  ( -0.5735764363510494901, -0.8191520442889894671, 0.000000000000000000 ) ) ;
#10901 = ADVANCED_FACE ( 'NONE', ( #62118 ), #82072, .T. ) ;
#10902 = CARTESIAN_POINT ( 'NONE',  ( -1.107233591667432293, 12.11777053784344282, -49.90351304355277762 ) ) ;
#10903 = CARTESIAN_POINT ( 'NONE',  ( 41.85000000000000142, 3.309500000000003439, 4.052968581778167743E-16 ) ) ;
#10904 = DIRECTION ( 'NONE',  ( 0.000000000000000000, 1.000000000000000000, 0.000000000000000000 ) ) ;
#10905 = CARTESIAN_POINT ( 'NONE',  ( -106.1836608158888424, -60.00000000000001421, 198.0778789678093972 ) ) ;
#10906 = CARTESIAN_POINT ( 'NONE',  ( 19.50000000000171596, 49.99999999999931788, 59.64162155654628350 ) ) ;
#10907 = MECHANICAL_DESIGN_GEOMETRIC_PRESENTATION_REPRESENTATION (  '', ( #57422 ), #76369 ) ;
#10908 = CARTESIAN_POINT ( 'NONE',  ( 0.000000000000000000, 0.000000000000000000, 0.000000000000000000 ) ) ;
#10909 = CARTESIAN_POINT ( 'NONE',  ( -43.17545047952408765, 487.6211760455623221, 8.487215481670535411 ) ) ;
#10910 = DIRECTION ( 'NONE',  ( 0.000000000000000000, -1.000000000000000000, 0.000000000000000000 ) ) ;
#10911 = CARTESIAN_POINT ( 'NONE',  ( -85.34260332515654568, -32.20242061357984653, 180.0776980316103391 ) ) ;
#10912 = CIRCLE ( 'NONE', #97089, 4.000000000000007105 ) ;
#10913 = DIRECTION ( 'NONE',  ( 0.000000000000000000, 1.000000000000000000, -0.000000000000000000 ) ) ;
#10914 = MECHANICAL_DESIGN_GEOMETRIC_PRESENTATION_REPRESENTATION (  '', ( #69550 ), #88487 ) ;
#10915 = VERTEX_POINT ( 'NONE', #54495 ) ;
#10916 = CARTESIAN_POINT ( 'NONE',  ( -9.721734870800478490, 46.20860777233757233, -13.03934063175032954 ) ) ;
#10917 = EDGE_CURVE ( 'NONE', #58545, #61408, #55506, .T. ) ;
#10918 = CARTESIAN_POINT ( 'NONE',  ( 3.405129523702669303, -1.148734789118030619, 104.5473292671427856 ) ) ;
#10919 = CARTESIAN_POINT ( 'NONE',  ( -83.85874690879670368, -45.26861737670255792, 5.011569712850605818 ) ) ;
#10920 = CARTESIAN_POINT ( 'NONE',  ( -5.109687690909018087, -13.89725820713649895, -5.663713107265619939 ) ) ;
#10921 = CARTESIAN_POINT ( 'NONE',  ( -15.53402121140690184, 43.94041489164831660, 5.989367130121264537 ) ) ;
#10922 = FACE_OUTER_BOUND ( 'NONE', #64720, .T. ) ;
#10923 = CARTESIAN_POINT ( 'NONE',  ( 15.75384615384615294, 4.172000000000003261, 0.000000000000000000 ) ) ;
#10924 = CARTESIAN_POINT ( 'NONE',  ( 90.56128410203886858, 42.00000000000000000, 11.85444436786826472 ) ) ;
#10925 = CARTESIAN_POINT ( 'NONE',  ( 71.69540001792421435, -59.99999999999999289, 172.8810247122642352 ) ) ;
#10926 =( LENGTH_UNIT ( ) NAMED_UNIT ( * ) SI_UNIT ( .MILLI., .METRE. ) );
#10927 = CARTESIAN_POINT ( 'NONE',  ( -86.74711523299461646, -14.21045842199446518, 20.03206905870895227 ) ) ;
#10928 = CARTESIAN_POINT ( 'NONE',  ( -71.96658176269305329, -25.59195321872661211, 100.0548059226765787 ) ) ;
#10929 = EDGE_LOOP ( 'NONE', ( #35569, #97882, #65461 ) ) ;
#10930 = CARTESIAN_POINT ( 'NONE',  ( 104.4175052224803864, -30.00000000000007105, 196.2185630211469629 ) ) ;
#10931 = CARTESIAN_POINT ( 'NONE',  ( -64.56213072485851967, 40.83885790042619846, -8.095562774589749822 ) ) ;
#10932 = CARTESIAN_POINT ( 'NONE',  ( 83.42010501496858410, -57.67103833101577948, -28.15582197385028707 ) ) ;
#10933 = EDGE_LOOP ( 'NONE', ( #81504, #42124, #47860, #26954 ) ) ;
#10934 = CARTESIAN_POINT ( 'NONE',  ( 9.322265351940091094, -11.89100710989636411, 9.148759095228598426 ) ) ;
#10935 = CARTESIAN_POINT ( 'NONE',  ( 7.188101187500000044, -25.53125000204838813, 0.000000000000000000 ) ) ;
#10936 = CARTESIAN_POINT ( 'NONE',  ( -0.1699168734760051480, 28.20319722039545596, -38.25876859947282327 ) ) ;
#10937 = VERTEX_POINT ( 'NONE', #36790 ) ;
#10938 = CARTESIAN_POINT ( 'NONE',  ( 0.000000000000000000, 0.000000000000000000, -8.028130060628445364 ) ) ;
#10939 = EDGE_LOOP ( 'NONE', ( #40120, #69321, #18396, #3461, #35198, #12468 ) ) ;
#10940 = CARTESIAN_POINT ( 'NONE',  ( -1.966965783804975887, 41.99999999999999289, -67.70628254661242806 ) ) ;
#10941 = MECHANICAL_DESIGN_GEOMETRIC_PRESENTATION_REPRESENTATION (  '', ( #76401 ), #103965 ) ;
#10942 = CARTESIAN_POINT ( 'NONE',  ( 48.02835407290414338, 14.94086294439859408, -16.85535821593631667 ) ) ;
#10943 = CARTESIAN_POINT ( 'NONE',  ( -37.96692578069663426, -60.00000000000488853, 53.22380867697400220 ) ) ;
#10944 = FACE_OUTER_BOUND ( 'NONE', #20673, .T. ) ;
#10945 = CARTESIAN_POINT ( 'NONE',  ( 5.082755093536324154, -14.84375000204838457, 5.082755093536326818 ) ) ;
#10946 = DIRECTION ( 'NONE',  ( -1.000000000000000000, -1.224606353822377258E-16, -0.000000000000000000 ) ) ;
#10947 = AXIS2_PLACEMENT_3D ( 'NONE', #77343, #94609, #45521 ) ;
#10948 = DIRECTION ( 'NONE',  ( -1.000000000000000000, 0.000000000000000000, 0.000000000000000000 ) ) ;
#10949 = CARTESIAN_POINT ( 'NONE',  ( 11.99999999999999467, 50.00000000000000000, -83.42920367501479006 ) ) ;
#10950 = ADVANCED_FACE ( 'NONE', ( #102548 ), #61392, .F. ) ;
#10951 = FACE_OUTER_BOUND ( 'NONE', #70335, .T. ) ;
#10952 = FILL_AREA_STYLE_COLOUR ( '', #6534 ) ;
#10953 = UNCERTAINTY_MEASURE_WITH_UNIT (LENGTH_MEASURE( 1.000000000000000082E-05 ), #79380, 'distance_accuracy_value', 'NONE');
#10954 =( GEOMETRIC_REPRESENTATION_CONTEXT ( 3 ) GLOBAL_UNCERTAINTY_ASSIGNED_CONTEXT ( ( #59673 ) ) GLOBAL_UNIT_ASSIGNED_CONTEXT ( ( #87462, #68634, #46975 ) ) REPRESENTATION_CONTEXT ( 'NONE', 'WORKASPACE' ) );
#10955 = CIRCLE ( 'NONE', #93598, 74.46152422706630603 ) ;
#10956 = ORIENTED_EDGE ( 'NONE', *, *, #41015, .T. ) ;
#10957 = CARTESIAN_POINT ( 'NONE',  ( 5.688569873206805738, -2.951204850235011445, 103.9352763293503585 ) ) ;
#10958 =( GEOMETRIC_REPRESENTATION_CONTEXT ( 3 ) GLOBAL_UNCERTAINTY_ASSIGNED_CONTEXT ( ( #10343 ) ) GLOBAL_UNIT_ASSIGNED_CONTEXT ( ( #104, #49751, #49210 ) ) REPRESENTATION_CONTEXT ( 'NONE', 'WORKASPACE' ) );
#10960 = CARTESIAN_POINT ( 'NONE',  ( 31.76254636305852941, -36.01904366976002336, 33.16591156249626948 ) ) ;
#10959 = CARTESIAN_POINT ( 'NONE',  ( 4.048442073968021582, 51.85559909576627291, -7.633306776926700898 ) ) ;
#10961 = CARTESIAN_POINT ( 'NONE',  ( -3.301606509414613644, -4.285714285714286476, 25.22241582816893413 ) ) ;
#10962 = ORIENTED_EDGE ( 'NONE', *, *, #16553, .F. ) ;
#10963 = EDGE_CURVE ( 'NONE', #82194, #102006, #14863, .T. ) ;
#10964 = CARTESIAN_POINT ( 'NONE',  ( -9.739726766683149961, 47.99999999999999289, -87.61747884359279226 ) ) ;
#10965 = ORIENTED_EDGE ( 'NONE', *, *, #7852, .F. ) ;
#10967 =( NAMED_UNIT ( * ) PLANE_ANGLE_UNIT ( ) SI_UNIT ( $, .RADIAN. ) );
#10966 = CARTESIAN_POINT ( 'NONE',  ( 32.70432414512695374, 489.1110749878063757, 10.33859015772799950 ) ) ;
#10968 = B_SPLINE_CURVE_WITH_KNOTS ( 'NONE', 3,
 ( #9729, #18952, #2715, #76067, #35661, #100877, #59385, #95325, #34597, #46244 ),
 .UNSPECIFIED., .F., .F.,
 ( 4, 2, 2, 2, 4 ),
 ( -5.999999999415129831E-08, 0.002545901231907733622, 0.005091862463815460815, 0.01018378492763092474, 0.02036762985526185607 ),
 .UNSPECIFIED. ) ;
#10969 = LINE ( 'NONE', #86507, #45734 ) ;
#10970 = CARTESIAN_POINT ( 'NONE',  ( 7.999999999999998224, -23.28125000409677270, 3.313708498984766049 ) ) ;
#10971 = CARTESIAN_POINT ( 'NONE',  ( 91.95555555555554861, 1.023464760207051730E-14, 0.000000000000000000 ) ) ;
#10972 = EDGE_CURVE ( 'NONE', #47749, #49640, #37322, .T. ) ;
#10973 = FACE_OUTER_BOUND ( 'NONE', #42430, .T. ) ;
#10974 = SURFACE_STYLE_USAGE ( .BOTH. , #53056 ) ;
#10975 = ORIENTED_EDGE ( 'NONE', *, *, #35133, .F. ) ;
#10976 = CARTESIAN_POINT ( 'NONE',  ( 92.35555844375753054, -59.99999999999999289, 0.7610974540291322032 ) ) ;
#10977 = B_SPLINE_CURVE_WITH_KNOTS ( 'NONE', 3,
 ( #8246, #71385, #104285, #105878 ),
 .UNSPECIFIED., .F., .F.,
 ( 4, 4 ),
 ( 0.000000000000000000, 0.005000000000000029594 ),
 .UNSPECIFIED. ) ;
#10979 = EDGE_CURVE ( 'NONE', #93333, #46770, #69685, .T. ) ;
#10978 = SURFACE_STYLE_FILL_AREA ( #84890 ) ;
#10980 = CARTESIAN_POINT ( 'NONE',  ( -35.44355846852403857, 438.5242933846664641, 4.909140697160467859 ) ) ;
#10981 = CARTESIAN_POINT ( 'NONE',  ( -6.855072974175857148, 40.29457745454482875, -71.16068772830431044 ) ) ;
#10982 = CARTESIAN_POINT ( 'NONE',  ( -46.81266956378431843, 18.41561415511115740, -15.90959751601133831 ) ) ;
#10983 = ORIENTED_EDGE ( 'NONE', *, *, #17302, .T. ) ;
#10984 = AXIS2_PLACEMENT_3D ( 'NONE', #40024, #6574, #23326 ) ;
#10985 = CARTESIAN_POINT ( 'NONE',  ( -98.51253199265957505, -29.99999999997342570, 199.5684000351004954 ) ) ;
#10986 = EDGE_LOOP ( 'NONE', ( #93852, #63174, #60912, #102809 ) ) ;
#10987 = FACE_OUTER_BOUND ( 'NONE', #35433, .T. ) ;
#10988 = CARTESIAN_POINT ( 'NONE',  ( 6.445370176741509916, -4.584736124522773792, -5.738941594273985203 ) ) ;
#10989 = CARTESIAN_POINT ( 'NONE',  ( 33.00000000000000000, 485.0303364503728289, 0.9535057477322557151 ) ) ;
#10990 = DIRECTION ( 'NONE',  ( 0.000000000000000000, 0.000000000000000000, 1.000000000000000000 ) ) ;
#10991 = CARTESIAN_POINT ( 'NONE',  ( 84.79553490237442759, -52.74953656108841216, -13.56258598970848972 ) ) ;
#10992 = CARTESIAN_POINT ( 'NONE',  ( -37.96433707770334109, 307.9427360707604180, 1.079370785649505837 ) ) ;
#10993 = CARTESIAN_POINT ( 'NONE',  ( 7.188101187500000044, -34.53125000204838813, 0.000000000000000000 ) ) ;
#10994 = CYLINDRICAL_SURFACE ( 'NONE', #1925, 5.000000000000002665 ) ;
#10995 = DIRECTION ( 'NONE',  ( -1.000000000000000000, -0.000000000000000000, -0.000000000000000000 ) ) ;
#10996 = ORIENTED_EDGE ( 'NONE', *, *, #1876, .F. ) ;
#10997 = DIRECTION ( 'NONE',  ( -1.000000000000000000, -0.000000000000000000, -0.000000000000000000 ) ) ;
#10998 = ORIENTED_EDGE ( 'NONE', *, *, #43431, .F. ) ;
#10999 = CARTESIAN_POINT ( 'NONE',  ( 49.09793955338178506, 7.820164633611708993, -16.25544133048972739 ) ) ;
#11000 = CARTESIAN_POINT ( 'NONE',  ( -44.53215874387177564, 465.2814620064186215, 9.437388644039931052 ) ) ;
#11001 = AXIS2_PLACEMENT_3D ( 'NONE', #45568, #6139, #13700 ) ;
#11003 = ORIENTED_EDGE ( 'NONE', *, *, #75155, .F. ) ;
#11002 = DIRECTION ( 'NONE',  ( -0.000000000000000000, -1.000000000000000000, -0.000000000000000000 ) ) ;
#11004 = CARTESIAN_POINT ( 'NONE',  ( 74.87613309056551714, -53.37519123465959581, 130.5581752795035300 ) ) ;
#11005 = ORIENTED_EDGE ( 'NONE', *, *, #67729, .F. ) ;
#11006 = CARTESIAN_POINT ( 'NONE',  ( 1.339715621834636883, -50.03010211448981437, 40.96304831423880444 ) ) ;
#11007 = LINE ( 'NONE', #68756, #54162 ) ;
#11008 = AXIS2_PLACEMENT_3D ( 'NONE', #99832, #85255, #69087 ) ;
#11009 = CARTESIAN_POINT ( 'NONE',  ( -7.188101187500002709, -24.31250000204838813, 2.977408999572647819 ) ) ;
#11010 = CARTESIAN_POINT ( 'NONE',  ( -72.09688937032439071, -57.67332965070641393, 173.0313604384042776 ) ) ;
#11011 = ADVANCED_FACE ( 'NONE', ( #5960 ), #23448, .T. ) ;
#11012 = ORIENTED_EDGE ( 'NONE', *, *, #25006, .F. ) ;
#11013 = CARTESIAN_POINT ( 'NONE',  ( -34.46463798447544491, 42.67666558786937969, -63.11895629106728478 ) ) ;
#11014 = CARTESIAN_POINT ( 'NONE',  ( 103.9524479304479883, -45.28272538064109654, 177.1755535782787661 ) ) ;
#11015 = EDGE_CURVE ( 'NONE', #37220, #45973, #9614, .T. ) ;
#11016 = CARTESIAN_POINT ( 'NONE',  ( -36.94654418156419950, 28.08625268104305661, -11.10888460376342124 ) ) ;
#11018 = CARTESIAN_POINT ( 'NONE',  ( -43.00000000000000000, 500.0000000000002274, 0.000000000000000000 ) ) ;
#11017 = B_SPLINE_CURVE_WITH_KNOTS ( 'NONE', 3,
 ( #49645, #75518, #99795, #58825, #100323, #82553, #41561, #9172, #34038, #34574, #9709, #42085, #82003, #24352, #8122, #91717, #74444, #42619, #57196, #26484, #523, #17838, #33486, #99246 ),
 .UNSPECIFIED., .F., .F.,
 ( 4, 2, 2, 2, 2, 2, 2, 2, 2, 2, 2, 4 ),
 ( 0.007071253621610506558, 0.007323632620172739610, 0.007576011618734973529, 0.008080769615859441368, 0.008333148614421678757, 0.008585527612983914411, 0.009090285610108389189, 0.009595043607232863966, 0.01009980160435733701, 0.01060455960148180832, 0.01085693860004404571, 0.01110931759860628310 ),
 .UNSPECIFIED. ) ;
#11019 = CARTESIAN_POINT ( 'NONE',  ( -5.656854249492379694, -18.12500000409676915, -5.656854249492380582 ) ) ;
#11020 = CARTESIAN_POINT ( 'NONE',  ( -51.39591267744368253, -29.90029742506343169, 48.99010193482668996 ) ) ;
#11021 = DIRECTION ( 'NONE',  ( 1.427673741351707591E-16, -0.5626279437277410533, 0.8267102254942136907 ) ) ;
#11022 = SURFACE_STYLE_USAGE ( .BOTH. , #51492 ) ;
#11023 = DIRECTION ( 'NONE',  ( 0.000000000000000000, 0.000000000000000000, -1.000000000000000000 ) ) ;
#11025 = VECTOR ( 'NONE', #9562, 1000.000000000000000 ) ;
#11024 = DIRECTION ( 'NONE',  ( 1.000000000000000000, 0.000000000000000000, 0.000000000000000000 ) ) ;
#11026 = CARTESIAN_POINT ( 'NONE',  ( 32.89395609997539083, 463.7240567052265305, 7.148062722715214257 ) ) ;
#11027 = EDGE_LOOP ( 'NONE', ( #5057, #40923, #103190, #63088 ) ) ;
#11028 = CARTESIAN_POINT ( 'NONE',  ( -5.420469775605654128, 41.88321586335170821, -59.04137891894603030 ) ) ;
#11029 = CARTESIAN_POINT ( 'NONE',  ( 11.82318485997968160, -4.853296004839451783, -12.56016920883609167 ) ) ;
#11030 = CARTESIAN_POINT ( 'NONE',  ( 0.5302602878479981685, 13.43200846721745023, 49.36160310769543713 ) ) ;
#11031 = CIRCLE ( 'NONE', #23086, 3.309500000000001663 ) ;
#11032 = CARTESIAN_POINT ( 'NONE',  ( -85.52168577127288529, -30.00000000000000711, 175.0049642106293390 ) ) ;
#11033 = EDGE_CURVE ( 'NONE', #35979, #12685, #14779, .T. ) ;
#11034 = CIRCLE ( 'NONE', #41992, 4.172000000000001485 ) ;
#11035 = ORIENTED_EDGE ( 'NONE', *, *, #2241, .T. ) ;
#11036 = CARTESIAN_POINT ( 'NONE',  ( -11.39884040742384919, -4.333298119783878910, 13.82668420665306819 ) ) ;
#11037 = CARTESIAN_POINT ( 'NONE',  ( 82.19213530885137686, -57.52430221361731810, 200.6401692809732538 ) ) ;
#11039 = CARTESIAN_POINT ( 'NONE',  ( 43.87333262551332069, 435.3945242957474306, 16.14343998350848253 ) ) ;
#11038 = FACE_OUTER_BOUND ( 'NONE', #97615, .T. ) ;
#11040 = CARTESIAN_POINT ( 'NONE',  ( 56.66881868820166090, -36.84070694962797177, -34.92016498303262750 ) ) ;
#11041 = CARTESIAN_POINT ( 'NONE',  ( -16.13469797932748051, 21.10829079391486474, -3.392296823503756276 ) ) ;
#11042 =( NAMED_UNIT ( * ) SI_UNIT ( $, .STERADIAN. ) SOLID_ANGLE_UNIT ( ) );
#11043 = CARTESIAN_POINT ( 'NONE',  ( -42.91031540250999399, -60.00000000000000711, 56.70723876392563056 ) ) ;
#11044 = CARTESIAN_POINT ( 'NONE',  ( 56.06936961865346802, 48.00000000000000000, -33.41736086621895652 ) ) ;
#11045 = CARTESIAN_POINT ( 'NONE',  ( -86.39907952452841755, -17.11962503844113215, 182.3896902915995497 ) ) ;
#11046 = EDGE_LOOP ( 'NONE', ( #96340, #59294, #10673, #73708, #61062 ) ) ;
#11047 = CARTESIAN_POINT ( 'NONE',  ( 30.00306714711529921, 17.76853250946123097, 39.63934773235497744 ) ) ;
#11048 = CARTESIAN_POINT ( 'NONE',  ( -5.086419386595018466, -42.95753334118048627, 31.03917363720831091 ) ) ;
#11049 =( NAMED_UNIT ( * ) PLANE_ANGLE_UNIT ( ) SI_UNIT ( $, .RADIAN. ) );
#11050 = PRODUCT_DEFINITION_SHAPE ( 'NONE', 'NONE',  #25882 ) ;
#11052 = DIRECTION ( 'NONE',  ( 0.000000000000000000, 1.000000000000000000, 0.000000000000000000 ) ) ;
#11051 = CARTESIAN_POINT ( 'NONE',  ( -41.20682028735892999, 328.7367104015643804, 10.18925674989210250 ) ) ;
#11053 = ORIENTED_EDGE ( 'NONE', *, *, #11537, .F. ) ;
#11054 = CARTESIAN_POINT ( 'NONE',  ( 28.12328997684540610, 24.73290587908618932, -14.06164498842270838 ) ) ;
#11055 = LINE ( 'NONE', #12653, #47788 ) ;
#11056 = CARTESIAN_POINT ( 'NONE',  ( 0.7847287007732014485, 27.38973784147641055, 40.48658148275971769 ) ) ;
#11057 = CARTESIAN_POINT ( 'NONE',  ( -30.75880901179656846, 7.960713337733316131, -41.50491223544449326 ) ) ;
#11058 = CARTESIAN_POINT ( 'NONE',  ( 26.54372762322449475, 296.0128866330822461, -9.750039548960653946 ) ) ;
#11059 = CARTESIAN_POINT ( 'NONE',  ( 28.21644434148578640, 308.7733337496239301, -9.112255642778066544 ) ) ;
#11060 = CARTESIAN_POINT ( 'NONE',  ( 11.31153846153846132, 1.411358822780289120E-15, 0.000000000000000000 ) ) ;
#11061 = CARTESIAN_POINT ( 'NONE',  ( 91.50784380495012726, -29.99999999999993960, 42.72614900145088512 ) ) ;
#11062 = CARTESIAN_POINT ( 'NONE',  ( -79.70987173175713281, -49.90920779543258590, 156.1999154600009092 ) ) ;
#11063 = ORIENTED_EDGE ( 'NONE', *, *, #7117, .F. ) ;
#11064 = CARTESIAN_POINT ( 'NONE',  ( -1.841875822471433519E-14, -3.000000000000002665, -70.00227127314062159 ) ) ;
#11065 = DIRECTION ( 'NONE',  ( 0.000000000000000000, 1.000000000000000000, 0.000000000000000000 ) ) ;
#11066 = CARTESIAN_POINT ( 'NONE',  ( 34.00423421181317707, -57.69387838581924655, 48.14221580456336369 ) ) ;
#11067 = CIRCLE ( 'NONE', #71365, 4.172000000000009479 ) ;
#11068 = LINE ( 'NONE', #43991, #40795 ) ;
#11069 = CARTESIAN_POINT ( 'NONE',  ( 34.91905476978136136, 321.9141106910175836, -5.351601672289109324 ) ) ;
#11070 = ORIENTED_EDGE ( 'NONE', *, *, #106748, .F. ) ;
#11071 = CIRCLE ( 'NONE', #71369, 4.000000000000001776 ) ;
#11072 = DIRECTION ( 'NONE',  ( 0.000000000000000000, 0.000000000000000000, 1.000000000000000000 ) ) ;
#11073 = FACE_OUTER_BOUND ( 'NONE', #69947, .T. ) ;
#11074 = CARTESIAN_POINT ( 'NONE',  ( -7.188101187500001821, -30.50000000204838813, -2.977408999572651371 ) ) ;
#11075 = ORIENTED_EDGE ( 'NONE', *, *, #24444, .F. ) ;
#11076 = CARTESIAN_POINT ( 'NONE',  ( -14.11595029532502643, 2.410436752314748521, -5.024000119269296682 ) ) ;
#11077 = CARTESIAN_POINT ( 'NONE',  ( 2.455962139888425710, 15.75268258782372754, 9.700350089084274430 ) ) ;
#11078 = CARTESIAN_POINT ( 'NONE',  ( 5.041270396327364622, 41.82074884801023984, -70.25592674792672199 ) ) ;
#11079 = EDGE_CURVE ( 'NONE', #82451, #9067, #32061, .T. ) ;
#11080 = CARTESIAN_POINT ( 'NONE',  ( -56.06936961859863544, 49.99999999999999289, -33.41736086620520751 ) ) ;
#11081 = LINE ( 'NONE', #95225, #100697 ) ;
#11082 = EDGE_CURVE ( 'NONE', #57762, #21618, #105764, .T. ) ;
#11083 = ORIENTED_EDGE ( 'NONE', *, *, #22608, .T. ) ;
#11084 = CARTESIAN_POINT ( 'NONE',  ( -71.80342408229677176, -30.00000000000000000, -19.71767938363507966 ) ) ;
#11086 = CARTESIAN_POINT ( 'NONE',  ( 23.90148031990576882, -46.43417030711851368, 32.71422033971168730 ) ) ;
#11085 = CARTESIAN_POINT ( 'NONE',  ( -106.7759996721837297, -60.00000000000014211, 200.9056163170290858 ) ) ;
#11087 = CARTESIAN_POINT ( 'NONE',  ( 121.1901574356003550, 4.501353321498349658, -60.59507871780015620 ) ) ;
#11088 = EDGE_CURVE ( 'NONE', #32538, #48149, #16570, .T. ) ;
#11089 = CARTESIAN_POINT ( 'NONE',  ( -34.39935170888136895, -56.83658484021449908, 38.30124131949656174 ) ) ;
#11090 = UNCERTAINTY_MEASURE_WITH_UNIT (LENGTH_MEASURE( 1.000000000000000082E-05 ), #10002, 'distance_accuracy_value', 'NONE');
#11091 = EDGE_LOOP ( 'NONE', ( #53599, #100785, #14060, #30145, #103936 ) ) ;
#11092 = CARTESIAN_POINT ( 'NONE',  ( -12.64023069600375138, -4.285714285714295357, 21.88880945939638423 ) ) ;
#11093 = DIRECTION ( 'NONE',  ( -1.000000000000000000, -1.224606353822377258E-16, -0.000000000000000000 ) ) ;
#11094 = CARTESIAN_POINT ( 'NONE',  ( -13.64640293162734785, -56.64148551553003585, 30.13230102324352799 ) ) ;
#11095 = DIRECTION ( 'NONE',  ( 0.000000000000000000, 0.000000000000000000, -1.000000000000000000 ) ) ;
#11096 = CARTESIAN_POINT ( 'NONE',  ( 7.896571385775229324, -61.21002000654245734, 1.305932416347441505 ) ) ;
#11097 = CARTESIAN_POINT ( 'NONE',  ( 12.35731595739100186, -3.034588722688706941, 20.66425384906944274 ) ) ;
#11098 = ORIENTED_EDGE ( 'NONE', *, *, #20142, .T. ) ;
#11099 = CARTESIAN_POINT ( 'NONE',  ( 0.000000000000000000, 35.00000000000000000, 0.000000000000000000 ) ) ;
#11100 = ORIENTED_EDGE ( 'NONE', *, *, #38488, .F. ) ;
#11101 = CARTESIAN_POINT ( 'NONE',  ( 98.18183449922635475, -29.99999999999996447, 190.3207026146189946 ) ) ;
#11102 = CARTESIAN_POINT ( 'NONE',  ( 80.00000000000000000, -60.00000000000000000, -23.09707704303352926 ) ) ;
#11103 = AXIS2_PLACEMENT_3D ( 'NONE', #14874, #7842, #22491 ) ;
#11105 = ADVANCED_FACE ( 'NONE', ( #96056 ), #26925, .T. ) ;
#11104 = CARTESIAN_POINT ( 'NONE',  ( -4.472135954999579610, -85.00000000000000000, -4.000000000000001776 ) ) ;
#11106 = CARTESIAN_POINT ( 'NONE',  ( 80.76909324667138890, -30.00000000000000000, 10.58948054053466770 ) ) ;
#11107 =( BOUNDED_SURFACE ( )  B_SPLINE_SURFACE ( 3, 2, ( 
 ( #18104, #18648, #59085 ),
 ( #26749, #10515, #92495 ),
 ( #34302, #75787, #42890 ),
 ( #83875, #59626, #1339 ),
 ( #2423, #42354, #67178 ),
 ( #43957, #54013, #2952 ),
 ( #75241, #9988, #51505 ),
 ( #43429, #35367, #68235 ),
 ( #101129, #19201, #27289 ),
 ( #60172, #35911, #86957 ),
 ( #62156, #95049, #13024 ),
 ( #105758, #23282, #56120 ),
 ( #55076, #79888, #39460 ),
 ( #31901, #7060, #72339 ),
 ( #54536, #5487, #15157 ),
 ( #39978, #87480, #64780 ) ),
 .UNSPECIFIED., .F., .F., .F. ) 
 B_SPLINE_SURFACE_WITH_KNOTS ( ( 4, 2, 2, 2, 2, 2, 2, 4 ),
 ( 3, 3 ),
 ( 0.01025942932839742083, 0.01330785678259500601, 0.01483207050969379860, 0.01635628423679259119, 0.01788049796389138205, 0.01940471169099017290, 0.02092892541808896723, 0.02245313914518775808 ),
 ( 0.3005395333822533654, 1.000000000000000000 ),
 .UNSPECIFIED. ) 
 GEOMETRIC_REPRESENTATION_ITEM ( )  RATIONAL_B_SPLINE_SURFACE ( (
 ( 0.8980036390037944294, 0.8303112408401904787, 1.000000000000000000),
 ( 0.9116818979159437841, 0.8530674133114374280, 1.000000000000000000),
 ( 0.9228127777807579868, 0.8715855758632119477, 1.000000000000000000),
 ( 0.9345546761373868527, 0.8911202743843785745, 1.000000000000000000),
 ( 0.9375544117806571265, 0.8961108585007369065, 1.000000000000000000),
 ( 0.9415935919673855681, 0.9028307401437135615, 1.000000000000000000),
 ( 0.9426280110961577918, 0.9045516770153640973, 1.000000000000000000),
 ( 0.9426141662316074310, 0.9045286436653173778, 1.000000000000000000),
 ( 0.9415455155258669606, 0.9027507565871785156, 1.000000000000000000),
 ( 0.9374309181787365830, 0.8959054053270217866, 1.000000000000000000),
 ( 0.9344062863247678541, 0.8908734020162928369, 1.000000000000000000),
 ( 0.9266839229609493689, 0.8780259019271841048, 1.000000000000000000),
 ( 0.9219922915685003773, 0.8702205537594245310, 1.000000000000000000),
 ( 0.9110602365930542401, 0.8520331711338884340, 1.000000000000000000),
 ( 0.9047689875046434071, 0.8415665795716911202, 1.000000000000000000),
 ( 0.8980036390032253291, 0.8303112408392433474, 1.000000000000000000) ) ) 
 REPRESENTATION_ITEM ( '' )  SURFACE ( )  );
#11108 = AXIS2_PLACEMENT_3D ( 'NONE', #81696, #74152, #7822 ) ;
#11109 = VERTEX_POINT ( 'NONE', #10209 ) ;
#11110 = AXIS2_PLACEMENT_3D ( 'NONE', #51494, #43943, #100576 ) ;
#11111 = CONICAL_SURFACE ( 'NONE', #71401, 4.000000000000001776, 0.9599310885968808105 ) ;
#11112 = EDGE_LOOP ( 'NONE', ( #3157, #33153, #38161, #13120 ) ) ;
#11113 = ORIENTED_EDGE ( 'NONE', *, *, #21094, .F. ) ;
#11114 = CARTESIAN_POINT ( 'NONE',  ( 14.27307692307692299, -4.171999999999999709, 5.616230220889763424E-16 ) ) ;
#11115 = DIRECTION ( 'NONE',  ( -0.000000000000000000, 1.000000000000000000, -0.000000000000000000 ) ) ;
#11116 = CARTESIAN_POINT ( 'NONE',  ( 42.51481257291533922, 437.0237169648399345, 20.73861080916342203 ) ) ;
#11117 = CARTESIAN_POINT ( 'NONE',  ( 47.40949999999999420, 4.898587196589412829E-16, -4.000000000000000000 ) ) ;
#11118 = CARTESIAN_POINT ( 'NONE',  ( 5.612461429774295851, 54.11923096040738557, 6.070761239882453530 ) ) ;
#11119 = DIRECTION ( 'NONE',  ( 1.000000000000000000, 0.000000000000000000, 0.000000000000000000 ) ) ;
#11120 = VERTEX_POINT ( 'NONE', #51190 ) ;
#11121 = CARTESIAN_POINT ( 'NONE',  ( 9.739726766105679445, 49.99999999999999289, -82.38252115500968387 ) ) ;
#11122 = EDGE_LOOP ( 'NONE', ( #42829, #88538, #19052 ) ) ;
#11123 = CARTESIAN_POINT ( 'NONE',  ( -5.727189096784631062, -61.42130124751258791, -1.806430436190351374 ) ) ;
#11124 = CARTESIAN_POINT ( 'NONE',  ( 71.10593052259025626, -38.32839063090802512, 140.6717657492907279 ) ) ;
#11125 = CARTESIAN_POINT ( 'NONE',  ( 0.000000000000000000, 0.000000000000000000, -12.97459999999999525 ) ) ;
#11126 = CARTESIAN_POINT ( 'NONE',  ( 29.60571183216354996, 297.6835046505696596, 2.558988572085852731 ) ) ;
#11127 = CARTESIAN_POINT ( 'NONE',  ( -5.909259836070535066, 246.1372279575791993, -1.072443315311452539 ) ) ;
#11128 = VERTEX_POINT ( 'NONE', #90609 ) ;
#11129 = CARTESIAN_POINT ( 'NONE',  ( 29.08094203968477487, 13.68582110885885861, -39.75724343093586555 ) ) ;
#11130 = FACE_OUTER_BOUND ( 'NONE', #77142, .T. ) ;
#11131 = CARTESIAN_POINT ( 'NONE',  ( 40.93668190287354491, 325.7203899766267341, 9.467451731427237505 ) ) ;
#11132 = CARTESIAN_POINT ( 'NONE',  ( 9.797174393178825657E-16, -30.00000000000000000, -8.000000000000000000 ) ) ;
#11133 = ADVANCED_FACE ( 'NONE', ( #67407 ), #34165, .F. ) ;
#11134 = ORIENTED_EDGE ( 'NONE', *, *, #59096, .F. ) ;
#11135 = CARTESIAN_POINT ( 'NONE',  ( 7.986468734911285949, -88.97313679723080782, 0.5341897780976099241 ) ) ;
#11136 = DIRECTION ( 'NONE',  ( -1.000000000000000000, -1.224606353822377258E-16, -0.000000000000000000 ) ) ;
#11137 = SURFACE_STYLE_FILL_AREA ( #365 ) ;
#11138 = CARTESIAN_POINT ( 'NONE',  ( 42.61140200160141944, 465.9030374194820752, 13.21253569360416869 ) ) ;
#11139 = CARTESIAN_POINT ( 'NONE',  ( 0.000000000000000000, 0.000000000000000000, 0.000000000000000000 ) ) ;
#11140 = EDGE_CURVE ( 'NONE', #58193, #98966, #59313, .T. ) ;
#11141 = EDGE_CURVE ( 'NONE', #60788, #38588, #51709, .T. ) ;
#11142 = CARTESIAN_POINT ( 'NONE',  ( -5.000000000000000000, 0.000000000000000000, -5.710657142857142432 ) ) ;
#11143 = CIRCLE ( 'NONE', #76585, 5.000000000000011546 ) ;
#11144 = MECHANICAL_DESIGN_GEOMETRIC_PRESENTATION_REPRESENTATION (  '', ( #88623 ), #57639 ) ;
#11145 = DIRECTION ( 'NONE',  ( 1.000000000000000000, 0.000000000000000000, 0.000000000000000000 ) ) ;
#11146 = AXIS2_PLACEMENT_3D ( 'NONE', #85368, #68112, #101010 ) ;
#11147 = CARTESIAN_POINT ( 'NONE',  ( 85.38455353301951334, -46.55565056629794896, 188.3801272255345793 ) ) ;
#11148 = LINE ( 'NONE', #44077, #46336 ) ;
#11149 = CARTESIAN_POINT ( 'NONE',  ( -8.147102310899050792, 111.6559345260857441, -1.270355265678086219E-12 ) ) ;
#11150 = ORIENTED_EDGE ( 'NONE', *, *, #56410, .T. ) ;
#11151 = VECTOR ( 'NONE', #93345, 1000.000000000000000 ) ;
#11152 = CARTESIAN_POINT ( 'NONE',  ( 44.35000000000000142, 3.309500000000003439, 0.000000000000000000 ) ) ;
#11153 = CARTESIAN_POINT ( 'NONE',  ( 0.000000000000000000, 0.000000000000000000, 5.000000000000002665 ) ) ;
#11154 = DIRECTION ( 'NONE',  ( 0.000000000000000000, 0.000000000000000000, -1.000000000000000000 ) ) ;
#11155 = CARTESIAN_POINT ( 'NONE',  ( 4.999999999999999112, -14.11572642558175694, 9.475261081874535307 ) ) ;
#11156 = VECTOR ( 'NONE', #40605, 1000.000000000000000 ) ;
#11157 = CARTESIAN_POINT ( 'NONE',  ( -86.43767908690688273, -29.99999999999999645, 66.98128119464180941 ) ) ;
#11158 = ADVANCED_FACE ( 'NONE', ( #45778 ), #37729, .T. ) ;
#11159 = DIRECTION ( 'NONE',  ( 1.000000000000000000, -0.000000000000000000, -0.000000000000000000 ) ) ;
#11160 = CARTESIAN_POINT ( 'NONE',  ( 34.42460263732258596, -57.69442024241028832, 48.56685808796169823 ) ) ;
#11162 = DIRECTION ( 'NONE',  ( 0.000000000000000000, 0.000000000000000000, -1.000000000000000000 ) ) ;
#11161 = CARTESIAN_POINT ( 'NONE',  ( -9.918579450955581578, 246.2069608703131109, 1.297207292923867827 ) ) ;
#11163 = EDGE_CURVE ( 'NONE', #89992, #26896, #106089, .T. ) ;
#11164 = CARTESIAN_POINT ( 'NONE',  ( 33.00000000000000000, 450.0000000000002274, 13.20242257375370976 ) ) ;
#11165 = CARTESIAN_POINT ( 'NONE',  ( -44.65110393089528884, -36.78960268062586181, 42.54015205027794622 ) ) ;
#11166 = CARTESIAN_POINT ( 'NONE',  ( 39.95753117817223909, 490.6049172992408671, 11.69497456421692227 ) ) ;
#11167 = CARTESIAN_POINT ( 'NONE',  ( -42.87890743753310119, 485.5827513095709946, 6.686224016762015943 ) ) ;
#11168 = LINE ( 'NONE', #58688, #11532 ) ;
#11169 = B_SPLINE_CURVE_WITH_KNOTS ( 'NONE', 3,
 ( #73665, #106568, #24627, #84440, #20282, #102206, #77404, #11587, #45054, #35386, #2437, #36980, #35927, #92513, #60189, #53133, #68253, #70380 ),
 .UNSPECIFIED., .F., .F.,
 ( 4, 2, 2, 2, 2, 2, 2, 2, 4 ),
 ( 0.002770935648931494456, 0.003276907721204434191, 0.003782879793477374360, 0.004794823938023257300, 0.005047809974159726300, 0.005300796010296196167, 0.005806768082569134168, 0.006312740154842072168, 0.006818712227115010169 ),
 .UNSPECIFIED. ) ;
#11170 = EDGE_CURVE ( 'NONE', #68599, #10651, #102651, .T. ) ;
#11171 = CARTESIAN_POINT ( 'NONE',  ( 21.71031025268755243, -19.05264385521112658, -33.48785545119387308 ) ) ;
#11172 = CARTESIAN_POINT ( 'NONE',  ( -26.85002416475204257, -42.96004896817819230, 32.78313945162506116 ) ) ;
#11173 = ORIENTED_EDGE ( 'NONE', *, *, #47995, .F. ) ;
#11174 = CARTESIAN_POINT ( 'NONE',  ( 6.924369423635565290, 9.133630944394992568, -1.059067681833820940 ) ) ;
#11175 = CARTESIAN_POINT ( 'NONE',  ( -20.86068844919981302, -22.07412597659780218, 28.15033270248965991 ) ) ;
#11177 = CARTESIAN_POINT ( 'NONE',  ( 1.196618058419959393E-20, 36.30024107553216339, -29.75000000000000355 ) ) ;
#11176 = CARTESIAN_POINT ( 'NONE',  ( 0.000000000000000000, 0.000000000000000000, 0.000000000000000000 ) ) ;
#11178 = EDGE_CURVE ( 'NONE', #1155, #105753, #74285, .T. ) ;
#11179 = VERTEX_POINT ( 'NONE', #10731 ) ;
#11180 = FILL_AREA_STYLE ('',( #52181 ) ) ;
#11181 = EDGE_LOOP ( 'NONE', ( #98615, #59425, #55927, #64364, #85027, #17665 ) ) ;
#11182 = CARTESIAN_POINT ( 'NONE',  ( -4.045830998955862512, 50.00000000000000711, -97.52795967580351544 ) ) ;
#11183 = FACE_OUTER_BOUND ( 'NONE', #8695, .T. ) ;
#11184 = CARTESIAN_POINT ( 'NONE',  ( -8.000000000000000000, -23.93750000409677270, -9.797174393178825657E-16 ) ) ;
#11185 = ORIENTED_EDGE ( 'NONE', *, *, #101178, .T. ) ;
#11186 = DIRECTION ( 'NONE',  ( -1.000000000000000000, -0.000000000000000000, -0.000000000000000000 ) ) ;
#11187 = CARTESIAN_POINT ( 'NONE',  ( 9.610124387788696154, 50.00000000000001421, -92.36062461489224518 ) ) ;
#11188 = CARTESIAN_POINT ( 'NONE',  ( 102.2803054478323190, -45.28266389599684771, 188.3718694929765718 ) ) ;
#11190 = CARTESIAN_POINT ( 'NONE',  ( -48.02835407290516656, 11.61227450977240494, 14.35535821593516559 ) ) ;
#11189 = DIRECTION ( 'NONE',  ( -0.000000000000000000, -0.000000000000000000, 1.000000000000000000 ) ) ;
#11191 = ORIENTED_EDGE ( 'NONE', *, *, #76380, .T. ) ;
#11192 = VECTOR ( 'NONE', #28463, 1000.000000000000000 ) ;
#11193 = EDGE_LOOP ( 'NONE', ( #69742, #60668, #92130, #31934, #3059 ) ) ;
#11194 = ORIENTED_EDGE ( 'NONE', *, *, #31479, .T. ) ;
#11195 = CARTESIAN_POINT ( 'NONE',  ( 25.07810932049445540, 307.4824937442463693, 9.536528439053487460 ) ) ;
#11196 = CYLINDRICAL_SURFACE ( 'NONE', #87093, 5.000000000000002665 ) ;
#11197 = CARTESIAN_POINT ( 'NONE',  ( 11.36650669486618881, 1.474610560812782335E-15, 0.000000000000000000 ) ) ;
#11198 = ORIENTED_EDGE ( 'NONE', *, *, #103751, .T. ) ;
#11199 = EDGE_CURVE ( 'NONE', #77225, #3027, #40656, .T. ) ;
#11200 = AXIS2_PLACEMENT_3D ( 'NONE', #77743, #11383, #102541 ) ;
#11201 = CARTESIAN_POINT ( 'NONE',  ( 0.000000000000000000, -1.550510257216834331, 120.5000000000000000 ) ) ;
#11202 = CARTESIAN_POINT ( 'NONE',  ( -6.965116046117188375, 41.61856606226407962, -70.00485699691061825 ) ) ;
#11203 = DIRECTION ( 'NONE',  ( 0.000000000000000000, -1.000000000000000000, 0.000000000000000000 ) ) ;
#11204 = CARTESIAN_POINT ( 'NONE',  ( -94.29220476078621971, -59.99999999999877076, -14.61292367681898341 ) ) ;
#11205 = CARTESIAN_POINT ( 'NONE',  ( 7.801777176595948937, -68.58827985812635575, -1.786991866639918936 ) ) ;
#11206 = CARTESIAN_POINT ( 'NONE',  ( -35.56416567029047116, 496.2909070316903239, -10.19064917708978335 ) ) ;
#11207 = CARTESIAN_POINT ( 'NONE',  ( -5.658903634044489372, 41.71506109579434707, -58.75004022056472053 ) ) ;
#11208 = CARTESIAN_POINT ( 'NONE',  ( -94.69971540129887444, -59.99999999999987921, 1.030331952319396782 ) ) ;
#11209 = EDGE_CURVE ( 'NONE', #24250, #95368, #100949, .T. ) ;
#11210 =( LENGTH_UNIT ( ) NAMED_UNIT ( * ) SI_UNIT ( .MILLI., .METRE. ) );
#11211 = CARTESIAN_POINT ( 'NONE',  ( -48.92667392005618154, -18.75201781075177010, 42.51917512051642944 ) ) ;
#11212 = ORIENTED_EDGE ( 'NONE', *, *, #67044, .F. ) ;
#11213 = FACE_OUTER_BOUND ( 'NONE', #70731, .T. ) ;
#11214 = AXIS2_PLACEMENT_3D ( 'NONE', #24240, #97541, #64669 ) ;
#11215 = ORIENTED_EDGE ( 'NONE', *, *, #73725, .F. ) ;
#11216 = AXIS2_PLACEMENT_3D ( 'NONE', #49970, #59683, #82879 ) ;
#11217 = DIRECTION ( 'NONE',  ( 0.000000000000000000, 1.000000000000000000, 0.000000000000000000 ) ) ;
#11218 = VECTOR ( 'NONE', #21081, 999.9999999999998863 ) ;
#11219 = VECTOR ( 'NONE', #93721, 1000.000000000000000 ) ;
#11220 = CARTESIAN_POINT ( 'NONE',  ( 9.165151389911679658, 85.00000000000000000, 4.000000000000000000 ) ) ;
#11221 = EDGE_CURVE ( 'NONE', #33725, #9363, #13121, .T. ) ;
#11222 = DIRECTION ( 'NONE',  ( 0.5735764363510468256, 0.8191520442889913545, 0.000000000000000000 ) ) ;
#11223 = EDGE_LOOP ( 'NONE', ( #46397, #60619, #63223, #45237 ) ) ;
#11224 = CARTESIAN_POINT ( 'NONE',  ( 4.595881407952560060, 248.9337456679867842, -3.857520671226082776 ) ) ;
#11225 = CIRCLE ( 'NONE', #95642, 5.000000000000010658 ) ;
#11226 = CARTESIAN_POINT ( 'NONE',  ( 87.28426567074583886, -30.00000000000508393, -18.21208458236663219 ) ) ;
#11228 = EDGE_CURVE ( 'NONE', #22409, #98784, #28447, .T. ) ;
#11227 = CARTESIAN_POINT ( 'NONE',  ( 48.26750065955900482, 16.22349350713542293, 14.37287707152939120 ) ) ;
#11229 = CARTESIAN_POINT ( 'NONE',  ( 3.405129524021479615, -48.85126521005803824, 104.5473292663389202 ) ) ;
#11231 = ADVANCED_FACE ( 'NONE', ( #96465 ), #88371, .T. ) ;
#11230 = CARTESIAN_POINT ( 'NONE',  ( -4.784091155926208039, -14.50372271115726086, -7.881159729540446079 ) ) ;
#11232 = CARTESIAN_POINT ( 'NONE',  ( 33.52312678243841759, 18.64316884716171785, -19.32152200345659665 ) ) ;
#11233 = CARTESIAN_POINT ( 'NONE',  ( 87.80209714494544926, -29.99999999999999289, 186.2705117335520697 ) ) ;
#11234 = CARTESIAN_POINT ( 'NONE',  ( -11.42607455529675065, 43.22995051892015539, -14.67755458576255201 ) ) ;
#11235 = CARTESIAN_POINT ( 'NONE',  ( -1.100561925788291262, 36.97067097995192597, 27.88635067314485028 ) ) ;
#11236 = EDGE_LOOP ( 'NONE', ( #68989, #14025, #34449, #60476 ) ) ;
#11237 = VERTEX_POINT ( 'NONE', #103998 ) ;
#11238 = CARTESIAN_POINT ( 'NONE',  ( 54.92320801914589623, -25.62319343846946040, 54.64829759656625896 ) ) ;
#11239 = CARTESIAN_POINT ( 'NONE',  ( 6.870855349944958057, 41.24230146623948912, -58.43742520720547162 ) ) ;
#11240 = CARTESIAN_POINT ( 'NONE',  ( -7.500000000000008882, 42.00000000000000711, -71.41947339646975479 ) ) ;
#11241 = EDGE_LOOP ( 'NONE', ( #101914, #102107, #95583, #77592 ) ) ;
#11242 = CARTESIAN_POINT ( 'NONE',  ( -84.96323215186174593, -38.35906192739592058, -22.88021158659245913 ) ) ;
#11243 = ORIENTED_EDGE ( 'NONE', *, *, #79449, .T. ) ;
#11244 = CARTESIAN_POINT ( 'NONE',  ( 108.5962463409214109, -38.35700097774115847, 191.3600774737103336 ) ) ;
#11245 = CARTESIAN_POINT ( 'NONE',  ( 11.77969503333905799, 19.16028191506968525, 7.890828749183966373 ) ) ;
#11246 = CARTESIAN_POINT ( 'NONE',  ( 84.98339600688585449, -52.71227180090472331, 17.49894070180983618 ) ) ;
#11247 = CARTESIAN_POINT ( 'NONE',  ( 42.67612106404315142, 370.2343072762694760, 17.77331514814132163 ) ) ;
#11248 = CARTESIAN_POINT ( 'NONE',  ( -26.03786948766120091, 306.7736357239633662, -9.576938274587746491 ) ) ;
#11249 = CARTESIAN_POINT ( 'NONE',  ( 5.109687690906336677, -13.89725820713331572, -5.663713107265837543 ) ) ;
#11250 = CARTESIAN_POINT ( 'NONE',  ( -24.17891642670491947, 25.18055287771648665, -32.75954025174772966 ) ) ;
#11251 = AXIS2_PLACEMENT_3D ( 'NONE', #21693, #45422, #102582 ) ;
#11252 = CARTESIAN_POINT ( 'NONE',  ( -43.81012751977135622, 434.3196218770653445, 12.85389645199988706 ) ) ;
#11253 = CARTESIAN_POINT ( 'NONE',  ( 2.955800887862049198, 98.65828318553602116, 5.000000000000000000 ) ) ;
#11254 = ORIENTED_EDGE ( 'NONE', *, *, #31122, .T. ) ;
#11255 = FACE_OUTER_BOUND ( 'NONE', #60077, .T. ) ;
#11256 = CARTESIAN_POINT ( 'NONE',  ( 7.414909996474294829, 40.55825027170075003, -70.34917702029655118 ) ) ;
#11257 = DIRECTION ( 'NONE',  ( -0.000000000000000000, -1.000000000000000000, -0.000000000000000000 ) ) ;
#11258 = EDGE_LOOP ( 'NONE', ( #59528, #64672, #5808, #93860, #4341 ) ) ;
#11259 = CARTESIAN_POINT ( 'NONE',  ( 0.7145311798163208605, 4.618802153517005848, 7.999999999999996447 ) ) ;
#11260 = CARTESIAN_POINT ( 'NONE',  ( -30.12911869256660324, 316.8191984638645522, 13.35676862894592176 ) ) ;
#11261 = CARTESIAN_POINT ( 'NONE',  ( -32.84237740334653921, 485.2251842821277137, 5.746442123024029236 ) ) ;
#11262 = DIRECTION ( 'NONE',  ( 0.8191520442889975717, 1.003171929053531773E-16, -0.5735764363510378328 ) ) ;
#11263 = CARTESIAN_POINT ( 'NONE',  ( -8.000000000000000000, -19.24999999999999289, -9.797174393178825657E-16 ) ) ;
#11264 = CARTESIAN_POINT ( 'NONE',  ( 8.208016662565434274, -13.37663391665104662, 31.98074858385048458 ) ) ;
#11265 = ADVANCED_FACE ( 'NONE', ( #7417 ), #104375, .F. ) ;
#11266 = CARTESIAN_POINT ( 'NONE',  ( 23.85217781305834350, 47.99999999999999289, 60.68504519422547361 ) ) ;
#11267 = ORIENTED_EDGE ( 'NONE', *, *, #55871, .F. ) ;
#11268 = CARTESIAN_POINT ( 'NONE',  ( 86.37194580826782442, -18.00985568670380843, 173.0435977549529696 ) ) ;
#11269 = CARTESIAN_POINT ( 'NONE',  ( 10.11650669486618881, 4.898587196589413815E-16, -4.000000000000000888 ) ) ;
#11270 = CARTESIAN_POINT ( 'NONE',  ( -16.48376536647094781, 45.65789762114239636, 6.657797401561870387 ) ) ;
#11271 = ORIENTED_EDGE ( 'NONE', *, *, #4403, .T. ) ;
#11272 = CARTESIAN_POINT ( 'NONE',  ( -88.73957585412472326, -45.26530870161231945, 62.97202553129596936 ) ) ;
#11273 = CARTESIAN_POINT ( 'NONE',  ( 26.36650669486618881, 1.474610560812782335E-15, 0.000000000000000000 ) ) ;
#11274 = CARTESIAN_POINT ( 'NONE',  ( 11.90609530896518464, -5.000000000000002665, -79.26133957282229403 ) ) ;
#11275 = CARTESIAN_POINT ( 'NONE',  ( 14.67571981732077191, -3.000000000000002665, -81.61772031543902983 ) ) ;
#11276 = CARTESIAN_POINT ( 'NONE',  ( -27.77384242259211433, -28.75021021836514734, -38.27450564851195480 ) ) ;
#11277 = EDGE_CURVE ( 'NONE', #61408, #7512, #63318, .T. ) ;
#11278 = AXIS2_PLACEMENT_3D ( 'NONE', #2099, #101352, #100804 ) ;
#11279 = SURFACE_STYLE_FILL_AREA ( #78678 ) ;
#11280 = CARTESIAN_POINT ( 'NONE',  ( 36.39487064310255704, -59.99999999999998579, 47.74500844687908341 ) ) ;
#11281 = CARTESIAN_POINT ( 'NONE',  ( 35.59999999999999432, 3.309500000000003439, 4.052968581778167743E-16 ) ) ;
#11282 = CARTESIAN_POINT ( 'NONE',  ( 19.19339060673821251, -16.77195851612492206, 31.49183225866399738 ) ) ;
#11284 = CARTESIAN_POINT ( 'NONE',  ( -11.59363613587280817, 15.60194627659213751, 9.659792498495315627 ) ) ;
#11283 = CARTESIAN_POINT ( 'NONE',  ( -43.25681043230515144, -38.30618596757071970, 54.80884264012910734 ) ) ;
#11285 = EDGE_CURVE ( 'NONE', #35576, #70143, #105081, .T. ) ;
#11286 = CARTESIAN_POINT ( 'NONE',  ( 4.926264938193783749, 301.1864079208653493, -10.01402411462960806 ) ) ;
#11287 = CARTESIAN_POINT ( 'NONE',  ( -7.188101187500000044, -9.406250002048384573, -8.802885111219163269E-16 ) ) ;
#11288 = AXIS2_PLACEMENT_3D ( 'NONE', #74113, #35294, #18033 ) ;
#11289 = CONICAL_SURFACE ( 'NONE', #85388, 4.000000000000007105, 0.9599310885968835860 ) ;
#11290 = CARTESIAN_POINT ( 'NONE',  ( 6.333820801330769967, 6.982605850970919903, -0.9057718968924614034 ) ) ;
#11291 =( GEOMETRIC_REPRESENTATION_CONTEXT ( 3 ) GLOBAL_UNCERTAINTY_ASSIGNED_CONTEXT ( ( #5156 ) ) GLOBAL_UNIT_ASSIGNED_CONTEXT ( ( #88552, #21719, #5506 ) ) REPRESENTATION_CONTEXT ( 'NONE', 'WORKASPACE' ) );
#11292 = EDGE_CURVE ( 'NONE', #53736, #36077, #20090, .T. ) ;
#11293 = CARTESIAN_POINT ( 'NONE',  ( -3.269135563215229023, 294.8518027752268722, -10.00000000024436275 ) ) ;
#11294 = PRODUCT ( '10. Furnel', '10. Furnel', '', ( #49230 ) ) ;
#11295 = SURFACE_STYLE_FILL_AREA ( #101397 ) ;
#11296 = AXIS2_PLACEMENT_3D ( 'NONE', #72505, #41203, #97842 ) ;
#11297 = ORIENTED_EDGE ( 'NONE', *, *, #106064, .T. ) ;
#11298 = CARTESIAN_POINT ( 'NONE',  ( -32.99999999999992184, 465.3568906370357467, 17.69306951624802338 ) ) ;
#11299 = CARTESIAN_POINT ( 'NONE',  ( 16.84999999999999787, 1.533819458162526451E-15, 0.000000000000000000 ) ) ;
#11300 = VECTOR ( 'NONE', #24988, 1000.000000000000000 ) ;
#11301 = CARTESIAN_POINT ( 'NONE',  ( 5.382057749264594904, -62.00173201596057027, -2.659775980967110431 ) ) ;
#11303 = CARTESIAN_POINT ( 'NONE',  ( -15.77836386018752890, -34.58954351035645658, -32.12809626525399409 ) ) ;
#11302 = DIRECTION ( 'NONE',  ( -1.000000000000000000, -1.224606353822377258E-16, -0.000000000000000000 ) ) ;
#11304 = EDGE_LOOP ( 'NONE', ( #64549, #79262, #86103, #12533, #72452 ) ) ;
#11305 = DIRECTION ( 'NONE',  ( 1.000000000000000000, 0.000000000000000000, -1.224646799147353207E-16 ) ) ;
#11306 = ORIENTED_EDGE ( 'NONE', *, *, #37328, .F. ) ;
#11307 = DIRECTION ( 'NONE',  ( 0.000000000000000000, 0.000000000000000000, -1.000000000000000000 ) ) ;
#11308 = DIRECTION ( 'NONE',  ( -1.000000000000000000, -1.224606353822377258E-16, -0.000000000000000000 ) ) ;
#11309 = DIRECTION ( 'NONE',  ( 0.000000000000000000, 1.000000000000000000, 0.000000000000000000 ) ) ;
#11310 = PRODUCT_RELATED_PRODUCT_CATEGORY ( 'part', '', ( #94105 ) ) ;
#11311 = CARTESIAN_POINT ( 'NONE',  ( -91.97475618974988265, -60.00000000000000711, 6.756679468872493821 ) ) ;
#11312 = DIRECTION ( 'NONE',  ( -0.000000000000000000, -1.000000000000000000, -0.000000000000000000 ) ) ;
#11313 = CARTESIAN_POINT ( 'NONE',  ( 7.149999999999997691, 41.65000000000000568, -59.82695526683420439 ) ) ;
#11314 =( NAMED_UNIT ( * ) PLANE_ANGLE_UNIT ( ) SI_UNIT ( $, .RADIAN. ) );
#11316 = FACE_OUTER_BOUND ( 'NONE', #82783, .T. ) ;
#11315 = CARTESIAN_POINT ( 'NONE',  ( 2.617478844990903664, -3.000000000000002665, -94.73972676610405586 ) ) ;
#11317 = B_SPLINE_CURVE_WITH_KNOTS ( 'NONE', 3,
 ( #96908, #74733, #74205, #73130, #24110, #99002, #106034, #283, #33251, #66123, #73674, #15443, #55876, #80702, #58022, #97412, #57482, #88811, #24635, #106577, #81752, #98482, #32181, #32729, #90949, #23572, #17057, #40781, #82304, #65596, #49936, #90407, #82841, #16510 ),
 .UNSPECIFIED., .F., .F.,
 ( 4, 2, 2, 2, 2, 2, 2, 2, 2, 2, 2, 2, 2, 2, 2, 2, 4 ),
 ( 0.01272238763756221476, 0.01351613129786393384, 0.01430987495816565119, 0.01510361861846737028, 0.01589736227876908936, 0.01669110593907080844, 0.01748484959937252753, 0.01827859325967424314, 0.01907233691997596223, 0.01986608058027768131, 0.02065982424057940040, 0.02145356790088111948, 0.02224731156118283509, 0.02304105522148455765, 0.02383479888178627326, 0.02462854254208799235, 0.02542228620238971143 ),
 .UNSPECIFIED. ) ;
#11318 = CARTESIAN_POINT ( 'NONE',  ( -80.31716401001155248, -60.40697784079697641, 178.0905699403173514 ) ) ;
#11319 = ORIENTED_EDGE ( 'NONE', *, *, #44034, .T. ) ;
#11320 = DIRECTION ( 'NONE',  ( 1.000000000000000000, 0.000000000000000000, 0.000000000000000000 ) ) ;
#11321 = ORIENTED_EDGE ( 'NONE', *, *, #4535, .T. ) ;
#11322 = AXIS2_PLACEMENT_3D ( 'NONE', #47909, #30716, #72721 ) ;
#11323 = EDGE_LOOP ( 'NONE', ( #89265, #15557, #1959, #25535 ) ) ;
#11324 = CARTESIAN_POINT ( 'NONE',  ( 4.684274960302871098E-15, 26.07813853931757464, 38.25000000000000000 ) ) ;
#11325 = CARTESIAN_POINT ( 'NONE',  ( 3.510455435514055811, -4.999999999999999112, 17.23741894013592102 ) ) ;
#11326 = ORIENTED_EDGE ( 'NONE', *, *, #85921, .T. ) ;
#11327 = SURFACE_STYLE_FILL_AREA ( #12398 ) ;
#11328 = CARTESIAN_POINT ( 'NONE',  ( -55.77313467663169888, -57.67115539668835567, -38.70230501811910528 ) ) ;
#11329 = CARTESIAN_POINT ( 'NONE',  ( -32.78741055188834963, 485.3331003366709524, 5.977022408746728743 ) ) ;
#11330 = EDGE_CURVE ( 'NONE', #78717, #62030, #39819, .T. ) ;
#11331 = DIRECTION ( 'NONE',  ( 1.000000000000000000, 1.224606353822377258E-16, 0.000000000000000000 ) ) ;
#11332 = FACE_OUTER_BOUND ( 'NONE', #75251, .T. ) ;
#11333 = CARTESIAN_POINT ( 'NONE',  ( -97.24366422982762970, -45.35372475475530507, 193.9806419842749676 ) ) ;
#11334 = CARTESIAN_POINT ( 'NONE',  ( 92.59918368926680898, -29.99999999999998224, 50.96418643717338881 ) ) ;
#11335 = EDGE_CURVE ( 'NONE', #63169, #55214, #73361, .T. ) ;
#11336 = CARTESIAN_POINT ( 'NONE',  ( -93.93757927471676794, -14.21045842199439946, 198.1409199811383246 ) ) ;
#11337 = CARTESIAN_POINT ( 'NONE',  ( -61.73170311023775270, -18.64112613040916244, 66.86421780239220425 ) ) ;
#11338 = VERTEX_POINT ( 'NONE', #87306 ) ;
#11339 = ORIENTED_EDGE ( 'NONE', *, *, #4417, .T. ) ;
#11340 = CARTESIAN_POINT ( 'NONE',  ( -100.7907627686642655, -37.81985441028579942, 188.8871514420389701 ) ) ;
#11341 = CARTESIAN_POINT ( 'NONE',  ( -30.00000000000000000, 0.000000000000000000, 0.000000000000000000 ) ) ;
#11342 =( LENGTH_UNIT ( ) NAMED_UNIT ( * ) SI_UNIT ( .MILLI., .METRE. ) );
#11343 =( LENGTH_UNIT ( ) NAMED_UNIT ( * ) SI_UNIT ( .MILLI., .METRE. ) );
#11344 = ORIENTED_EDGE ( 'NONE', *, *, #22997, .F. ) ;
#11345 = CARTESIAN_POINT ( 'NONE',  ( 19.49348534677603340, 49.99933769095211744, 60.04655563041394117 ) ) ;
#11346 = AXIS2_PLACEMENT_3D ( 'NONE', #6521, #47516, #38402 ) ;
#11347 = CARTESIAN_POINT ( 'NONE',  ( 0.000000000000000000, 1.000000000000000888, 0.000000000000000000 ) ) ;
#11348 = CARTESIAN_POINT ( 'NONE',  ( -3.369683342533076331, -0.9132179776671506266, 104.1613013819149387 ) ) ;
#11349 = CARTESIAN_POINT ( 'NONE',  ( 4.401442555609581635E-16, -13.15625000204838280, -7.188101187500000044 ) ) ;
#11350 = DIRECTION ( 'NONE',  ( -1.000000000000000000, -1.224606353822377258E-16, -0.000000000000000000 ) ) ;
#11352 = ADVANCED_FACE ( 'NONE', ( #38247, #105592 ), #22600, .T. ) ;
#11351 = CARTESIAN_POINT ( 'NONE',  ( 43.03185303983483578, 485.3613526602390493, 6.073233449168488285 ) ) ;
#11353 = CARTESIAN_POINT ( 'NONE',  ( 7.986539162393897939, -81.02672828942547767, -0.5321833565149911571 ) ) ;
#11354 = CARTESIAN_POINT ( 'NONE',  ( 83.13703396460537931, -45.33804159704407510, -14.25699536724285110 ) ) ;
#11355 = CARTESIAN_POINT ( 'NONE',  ( -6.746558653882650525, 3.895127454922563182, -6.526045885145563830 ) ) ;
#11356 = EDGE_CURVE ( 'NONE', #102954, #104748, #55958, .T. ) ;
#11357 = CARTESIAN_POINT ( 'NONE',  ( -9.523678393152335886, 43.48341758817304026, -15.16113424488535344 ) ) ;
#11358 = CARTESIAN_POINT ( 'NONE',  ( -16.02938566285134669, 45.83159863292935654, -6.508120059605710495 ) ) ;
#11359 = CIRCLE ( 'NONE', #28667, 4.000000000000001776 ) ;
#11360 = CARTESIAN_POINT ( 'NONE',  ( -5.367391215540106231, 43.24496486319789312, -60.11082976391323029 ) ) ;
#11361 = UNCERTAINTY_MEASURE_WITH_UNIT (LENGTH_MEASURE( 1.000000000000000082E-05 ), #68845, 'distance_accuracy_value', 'NONE');
#11362 = CARTESIAN_POINT ( 'NONE',  ( -32.12776895466944183, -42.96425948997189437, 34.59058220734644351 ) ) ;
#11363 = UNCERTAINTY_MEASURE_WITH_UNIT (LENGTH_MEASURE( 1.000000000000000082E-05 ), #41082, 'distance_accuracy_value', 'NONE');
#11364 = CARTESIAN_POINT ( 'NONE',  ( 45.55829705881837555, -42.98293676978153144, 45.30720637935260697 ) ) ;
#11365 = CIRCLE ( 'NONE', #90371, 12.00000000000000711 ) ;
#11366 = CARTESIAN_POINT ( 'NONE',  ( -7.343637806710344051, 87.44363121900617841, 3.177475076494672201 ) ) ;
#11367 = CARTESIAN_POINT ( 'NONE',  ( -86.18829832611947950, -38.63105478832063966, 199.1571653378964584 ) ) ;
#11368 = AXIS2_PLACEMENT_3D ( 'NONE', #46690, #74138, #90334 ) ;
#11369 = VERTEX_POINT ( 'NONE', #14982 ) ;
#11371 = CARTESIAN_POINT ( 'NONE',  ( -28.34317069729203098, 36.34622212941757624, 8.615775889579945002 ) ) ;
#11370 = CARTESIAN_POINT ( 'NONE',  ( 40.92692307692308162, -4.171999999999999709, 5.616230220889763424E-16 ) ) ;
#11372 = CARTESIAN_POINT ( 'NONE',  ( 83.88447113947664491, -60.00000000000000000, 191.6821499555289847 ) ) ;
#11373 = CARTESIAN_POINT ( 'NONE',  ( -19.21241590914347341, 49.78725338447024740, 61.53583624396806329 ) ) ;
#11374 = CARTESIAN_POINT ( 'NONE',  ( -7.384656406523468775, 41.09429650711703630, -59.07190356531275910 ) ) ;
#11375 = AXIS2_PLACEMENT_3D ( 'NONE', #64849, #30926, #14683 ) ;
#11376 = CIRCLE ( 'NONE', #78531, 4.172000000000001485 ) ;
#11377 = CARTESIAN_POINT ( 'NONE',  ( 6.812289211616648466, 40.56151012360425767, -71.12586855819816378 ) ) ;
#11378 = FACE_OUTER_BOUND ( 'NONE', #19277, .T. ) ;
#11379 = CARTESIAN_POINT ( 'NONE',  ( 42.48722704179519383, 465.9004001135055546, 13.75636562493388126 ) ) ;
#11380 = CARTESIAN_POINT ( 'NONE',  ( 33.51588970236548448, 434.0196042276504045, 13.78171046059029869 ) ) ;
#11381 = CARTESIAN_POINT ( 'NONE',  ( 112.1264442912419241, -59.99999999999999289, 177.3897674384393781 ) ) ;
#11382 = AXIS2_PLACEMENT_3D ( 'NONE', #41168, #22889, #16899 ) ;
#11383 = DIRECTION ( 'NONE',  ( -1.000000000000000000, -1.224606353822377258E-16, -0.000000000000000000 ) ) ;
#11384 = ORIENTED_EDGE ( 'NONE', *, *, #38114, .F. ) ;
#11385 = SURFACE_SIDE_STYLE ('',( #27100 ) ) ;
#11386 = CARTESIAN_POINT ( 'NONE',  ( -95.32476753328225527, -30.00000000000000000, 119.8948401030209965 ) ) ;
#11387 = ORIENTED_EDGE ( 'NONE', *, *, #21653, .F. ) ;
#11389 = CARTESIAN_POINT ( 'NONE',  ( -9.125156274357966169, -53.47050611676294096, 31.09081505442903648 ) ) ;
#11388 = CARTESIAN_POINT ( 'NONE',  ( -76.19933201318396243, -38.38804777193976037, 180.0097251488151358 ) ) ;
#11390 = DIRECTION ( 'NONE',  ( -0.000000000000000000, -1.000000000000000000, -0.000000000000000000 ) ) ;
#11391 = CARTESIAN_POINT ( 'NONE',  ( 69.92761780597730592, -1.232595164407830946E-29, 4.000000000000007105 ) ) ;
#11392 = AXIS2_PLACEMENT_3D ( 'NONE', #53860, #85726, #93268 ) ;
#11393 = DIRECTION ( 'NONE',  ( -1.000000000000000000, -0.000000000000000000, -0.000000000000000000 ) ) ;
#11394 = CARTESIAN_POINT ( 'NONE',  ( -7.188101187500000044, -12.78125000204838635, -8.802885111219163269E-16 ) ) ;
#11395 = CARTESIAN_POINT ( 'NONE',  ( 10.48543666094595217, -5.000000000000002665, -91.04342776276725147 ) ) ;
#11396 = ADVANCED_FACE ( 'NONE', ( #30146 ), #37236, .F. ) ;
#11397 = UNCERTAINTY_MEASURE_WITH_UNIT (LENGTH_MEASURE( 1.000000000000000082E-05 ), #40329, 'distance_accuracy_value', 'NONE');
#11398 = DIRECTION ( 'NONE',  ( 0.000000000000000000, -1.000000000000000000, 0.000000000000000000 ) ) ;
#11400 = VERTEX_POINT ( 'NONE', #60143 ) ;
#11399 = SURFACE_STYLE_FILL_AREA ( #104136 ) ;
#11401 = CARTESIAN_POINT ( 'NONE',  ( 84.26967318104641436, -32.46622938755235310, 170.8684416685377698 ) ) ;
#11403 = AXIS2_PLACEMENT_3D ( 'NONE', #4071, #10549, #43468 ) ;
#11402 = CARTESIAN_POINT ( 'NONE',  ( -4.440267933150495061, -1.157000248813045085, 104.3849335853022779 ) ) ;
#11404 = B_SPLINE_CURVE_WITH_KNOTS ( 'NONE', 3,
 ( #38123, #103357, #46180, #87707, #5707, #29504, #71496, #104396, #95269, #21398, #62901, #30545, #96338, #55307, #39688, #16449, #49877, #32129, #8884, #49336, #25104, #73070, #56894, #65008, #40725, #15390, #82782, #82242, #6769, #89295, #105467, #41789, #41259, #90344, #74146, #8357, #56359, #48276, #230, #73612, #15925, #33194, #89821, #17000, #72564, #81177, #74672, #66066, #24054, #24580, #7288, #55819, #98943, #105979, #48802, #40194, #31607, #57963 ),
 .UNSPECIFIED., .F., .F.,
 ( 4, 2, 2, 2, 2, 2, 2, 2, 2, 2, 2, 2, 2, 2, 2, 2, 2, 2, 2, 2, 2, 2, 2, 2, 2, 2, 2, 2, 4 ),
 ( 0.3785283831463345794, 0.3800322516953381635, 0.3815361202443417477, 0.3845438573423488049, 0.3875515944403558621, 0.3905593315383629749, 0.3965748057343771449, 0.4025902799303912594, 0.4146212283224195994, 0.4266521767144478838, 0.4386831251064762238, 0.4507140734985045638, 0.4747759702825611328, 0.4868069186745894728, 0.4988378670666178127, 0.5048533412626319272, 0.5108688154586461527, 0.5168842896546603782, 0.5228997638506744927, 0.5259075009486815500, 0.5289152380466886072, 0.5349307122427028327, 0.5379384493407098899, 0.5409461864387169472, 0.5469616606347311727, 0.5529771348307452872, 0.5589926090267594017, 0.5650080832227735161, 0.5710235574187877416 ),
 .UNSPECIFIED. ) ;
#11405 = DIRECTION ( 'NONE',  ( -1.000000000000000000, 0.000000000000000000, 0.000000000000000000 ) ) ;
#11406 = ORIENTED_EDGE ( 'NONE', *, *, #52022, .F. ) ;
#11407 = CARTESIAN_POINT ( 'NONE',  ( -13.48373700555449162, 302.5481773704228772, -10.06453227936397354 ) ) ;
#11408 = CARTESIAN_POINT ( 'NONE',  ( 17.37570930947881465, 34.80728798345248975, 21.96198386118272339 ) ) ;
#11409 = DIRECTION ( 'NONE',  ( 0.5735764363510557073, -0.8191520442889850262, 1.003171929053516612E-16 ) ) ;
#11410 = CARTESIAN_POINT ( 'NONE',  ( -89.99999999999997158, 500000.0000000000582, 196.0238439516549818 ) ) ;
#11411 = CARTESIAN_POINT ( 'NONE',  ( -5.477578620271503773, 253.1650143901609908, -2.459398706554668745 ) ) ;
#11412 = CARTESIAN_POINT ( 'NONE',  ( 0.3591563125534498746, 18.74881295153323535, 49.30117588463760825 ) ) ;
#11413 = EDGE_CURVE ( 'NONE', #95368, #85900, #75066, .T. ) ;
#11414 = VERTEX_POINT ( 'NONE', #2924 ) ;
#11415 = CARTESIAN_POINT ( 'NONE',  ( -80.63290903287661138, -30.00000000000000711, -12.77866334089981670 ) ) ;
#11416 = CARTESIAN_POINT ( 'NONE',  ( 38.38499389482827695, 18.64284798592676395, 1.874612472324977519 ) ) ;
#11417 = CARTESIAN_POINT ( 'NONE',  ( 86.62891540500523035, -16.99681948805599774, 185.2243898127639739 ) ) ;
#11419 = CARTESIAN_POINT ( 'NONE',  ( -14.22864388059377916, 6.541366219244691749, -7.652784845931969393 ) ) ;
#11418 = DIRECTION ( 'NONE',  ( -1.000000000000000000, -1.224606353822377258E-16, -0.000000000000000000 ) ) ;
#11420 = CARTESIAN_POINT ( 'NONE',  ( -7.188101187500002709, -25.81250000204838457, 2.977408999572648707 ) ) ;
#11421 = DIRECTION ( 'NONE',  ( -1.000000000000000000, -1.224606353822377258E-16, -0.000000000000000000 ) ) ;
#11422 = DIRECTION ( 'NONE',  ( -1.000000000000000000, 0.000000000000000000, 0.000000000000000000 ) ) ;
#11423 = ADVANCED_FACE ( 'NONE', ( #59592 ), #1851, .F. ) ;
#11424 = CARTESIAN_POINT ( 'NONE',  ( 42.53724782439362428, 437.0052025638185569, 20.70619558814934180 ) ) ;
#11425 = VECTOR ( 'NONE', #40324, 1000.000000000000000 ) ;
#11426 = CONTEXT_DEPENDENT_SHAPE_REPRESENTATION ( #70742, #63213 ) ;
#11427 = ORIENTED_EDGE ( 'NONE', *, *, #100379, .T. ) ;
#11428 = CARTESIAN_POINT ( 'NONE',  ( 98.31310517497099966, -2.002967142162725287E-29, 5.000000000000011546 ) ) ;
#11429 = CARTESIAN_POINT ( 'NONE',  ( -10.00791540606109820, 7.488695628611232280, 0.000000000000000000 ) ) ;
#11430 =( BOUNDED_SURFACE ( )  B_SPLINE_SURFACE ( 3, 2, ( 
 ( #49994, #90461, #24169 ),
 ( #66182, #89411, #91010 ),
 ( #74267, #98540, #82902 ),
 ( #25227, #341, #33310 ),
 ( #81284, #55930, #17118 ),
 ( #56483, #98017, #8999 ),
 ( #40841, #872, #16573 ),
 ( #73733, #48916, #6878 ),
 ( #32784, #106635, #66722 ),
 ( #41905, #65121, #88872 ),
 ( #74792, #39799, #15505 ),
 ( #14961, #24691, #47856 ) ),
 .UNSPECIFIED., .F., .F., .F. ) 
 B_SPLINE_SURFACE_WITH_KNOTS ( ( 4, 2, 2, 2, 2, 4 ),
 ( 3, 3 ),
 ( 0.001868552850199507254, 0.003758858514504430717, 0.005649164178809354397, 0.006594317010961816238, 0.007539469843114278078, 0.009429775507419201758 ),
 ( 0.000000000000000000, 1.000000000000000000 ),
 .UNSPECIFIED. ) 
 GEOMETRIC_REPRESENTATION_ITEM ( )  RATIONAL_B_SPLINE_SURFACE ( (
 ( 1.000000000000000000, 0.7560596356352350389, 1.000000000000000000),
 ( 1.000000000000000000, 0.7673542365376597729, 1.000000000000000000),
 ( 1.000000000000000000, 0.7800062459456665875, 1.000000000000000000),
 ( 1.000000000000000000, 0.8052793511181970398, 1.000000000000000000),
 ( 1.000000000000000000, 0.8179389361350274390, 1.000000000000000000),
 ( 1.000000000000000000, 0.8361751068035501167, 1.000000000000000000),
 ( 1.000000000000000000, 0.8421576244855180082, 1.000000000000000000),
 ( 1.000000000000000000, 0.8536052415463137866, 1.000000000000000000),
 ( 1.000000000000000000, 0.8590641661814891750, 1.000000000000000000),
 ( 1.000000000000000000, 0.8745109084890774209, 1.000000000000000000),
 ( 1.000000000000000000, 0.8835763275885871737, 1.000000000000000000),
 ( 1.000000000000000000, 0.8909749942927646105, 1.000000000000000000) ) ) 
 REPRESENTATION_ITEM ( '' )  SURFACE ( )  );
#11431 = EDGE_CURVE ( 'NONE', #15319, #3854, #11007, .T. ) ;
#11432 = CIRCLE ( 'NONE', #61200, 65.00000000000000000 ) ;
#11433 = EDGE_LOOP ( 'NONE', ( #46708, #5771, #41924, #60246 ) ) ;
#11434 = CARTESIAN_POINT ( 'NONE',  ( -7.308237722677127124, 52.16199744752358214, -2.719250781937797345 ) ) ;
#11435 =( NAMED_UNIT ( * ) SI_UNIT ( $, .STERADIAN. ) SOLID_ANGLE_UNIT ( ) );
#11436 = AXIS2_PLACEMENT_3D ( 'NONE', #61500, #94391, #11309 ) ;
#11437 = VERTEX_POINT ( 'NONE', #27256 ) ;
#11438 = CARTESIAN_POINT ( 'NONE',  ( -0.6261581091747900896, 8.128258333189501528, -51.58587807493976385 ) ) ;
#11439 = CARTESIAN_POINT ( 'NONE',  ( 9.797537890442933772, 101.5344220233380810, 2.014215961808881072 ) ) ;
#11440 = UNCERTAINTY_MEASURE_WITH_UNIT (LENGTH_MEASURE( 1.000000000000000082E-05 ), #73649, 'distance_accuracy_value', 'NONE');
#11441 = CARTESIAN_POINT ( 'NONE',  ( -98.88275070081830620, -60.00000000000000711, 202.1696466176894660 ) ) ;
#11442 = VECTOR ( 'NONE', #95255, 1000.000000000000114 ) ;
#11443 = AXIS2_PLACEMENT_3D ( 'NONE', #16616, #49509, #389 ) ;
#11444 = SURFACE_STYLE_FILL_AREA ( #77266 ) ;
#11445 = CONICAL_SURFACE ( 'NONE', #1109, 4.000000000000000000, 0.9599310885968912466 ) ;
#11446 = CONICAL_SURFACE ( 'NONE', #97604, 4.000000000000001776, 0.9599310885968774798 ) ;
#11447 = CARTESIAN_POINT ( 'NONE',  ( 6.326416241096633364, 1.324101276589543907, 6.831531844319973068 ) ) ;
#11448 = DIRECTION ( 'NONE',  ( 0.000000000000000000, 0.000000000000000000, 1.000000000000000000 ) ) ;
#11449 = DIRECTION ( 'NONE',  ( 1.000000000000000000, -0.000000000000000000, 1.224646799147353207E-16 ) ) ;
#11450 = CARTESIAN_POINT ( 'NONE',  ( -82.85955728807176968, -60.89795309201070950, 190.2906973079219881 ) ) ;
#11451 = ADVANCED_FACE ( 'NONE', ( #76283 ), #86934, .F. ) ;
#11452 = CARTESIAN_POINT ( 'NONE',  ( -4.185364993345132234, 53.85950711538551872, -7.946775408610140090 ) ) ;
#11453 = ORIENTED_EDGE ( 'NONE', *, *, #69806, .F. ) ;
#11454 = CARTESIAN_POINT ( 'NONE',  ( -9.182151393623367852, 45.78138532639618319, -14.82507784383112792 ) ) ;
#11455 = CARTESIAN_POINT ( 'NONE',  ( 3.534854069000094690, -1.070477528868737371, 104.4405781011824956 ) ) ;
#11456 = CARTESIAN_POINT ( 'NONE',  ( -86.60779780715820664, -60.14586139666025133, 0.8348040731936827719 ) ) ;
#11457 = CARTESIAN_POINT ( 'NONE',  ( -5.290067270634260410, 52.08006895350597176, -6.031152949369843697 ) ) ;
#11458 = CARTESIAN_POINT ( 'NONE',  ( -4.557876263184661880, 143.2026128489522989, -5.000000000000000000 ) ) ;
#11459 = CARTESIAN_POINT ( 'NONE',  ( 8.986743721229322190, 136.5670193726028856, -6.141763964344532733E-13 ) ) ;
#11460 = CARTESIAN_POINT ( 'NONE',  ( 27.26440085636200550, 36.55135662950691966, -10.05698433968642469 ) ) ;
#11461 = FILL_AREA_STYLE ('',( #31544 ) ) ;
#11462 = CARTESIAN_POINT ( 'NONE',  ( 69.35339668739648289, -14.21045842199427511, 113.5888189438209537 ) ) ;
#11463 = CARTESIAN_POINT ( 'NONE',  ( -0.000000000000000000, 58.72416816948006613, -16.91618513671782509 ) ) ;
#11464 = CARTESIAN_POINT ( 'NONE',  ( -94.21206122632280255, -59.99999999999995737, 9.571777650087724965 ) ) ;
#11465 = CARTESIAN_POINT ( 'NONE',  ( -68.52812349397821379, -39.48763755164299027, 97.13502983046556949 ) ) ;
#11466 = ORIENTED_EDGE ( 'NONE', *, *, #32565, .F. ) ;
#11467 = CARTESIAN_POINT ( 'NONE',  ( 101.7112553140276390, -14.21045842199441367, 195.4619641463733615 ) ) ;
#11468 = CARTESIAN_POINT ( 'NONE',  ( 32.79512188131152328, -59.99999999999019451, 47.57302644083591048 ) ) ;
#11469 = EDGE_LOOP ( 'NONE', ( #13968, #31699 ) ) ;
#11470 = CARTESIAN_POINT ( 'NONE',  ( 13.99719405338373512, -57.99973887820377172, 27.38482409491458114 ) ) ;
#11471 = CARTESIAN_POINT ( 'NONE',  ( -7.188101187500000044, -23.28125000204838457, -8.802885111219163269E-16 ) ) ;
#11472 = DIRECTION ( 'NONE',  ( -1.000000000000000000, -1.224606353822377258E-16, -0.000000000000000000 ) ) ;
#11473 = ORIENTED_EDGE ( 'NONE', *, *, #14774, .T. ) ;
#11474 = AXIS2_PLACEMENT_3D ( 'NONE', #46127, #79015, #79538 ) ;
#11475 = CARTESIAN_POINT ( 'NONE',  ( -16.07917213302809856, 5.118112109469922899, -4.258304778695157999 ) ) ;
#11476 = ORIENTED_EDGE ( 'NONE', *, *, #53800, .T. ) ;
#11477 = CARTESIAN_POINT ( 'NONE',  ( 6.821717117272701358, 41.99999999999999289, -69.36621149908677353 ) ) ;
#11478 = CARTESIAN_POINT ( 'NONE',  ( 47.50459250088609053, 17.89957706894796985, -14.46754909258835298 ) ) ;
#11479 = CARTESIAN_POINT ( 'NONE',  ( -91.84069786539126312, -59.99999999999998579, 13.61882742409930458 ) ) ;
#11480 = CARTESIAN_POINT ( 'NONE',  ( -10.28624191511820207, 43.25714326066858462, 15.40779740156164124 ) ) ;
#11481 = CARTESIAN_POINT ( 'NONE',  ( 7.188101187500001821, -29.93750000204839523, -2.977408999572650483 ) ) ;
#11482 = CARTESIAN_POINT ( 'NONE',  ( -48.55172137731392468, 13.85052760073561373, 16.74335408647196033 ) ) ;
#11483 = VECTOR ( 'NONE', #82476, 1000.000000000000000 ) ;
#11484 = ADVANCED_FACE ( 'NONE', ( #49478 ), #95537, .T. ) ;
#11485 = CARTESIAN_POINT ( 'NONE',  ( 20.05453516056601515, -4.285714285714294469, -15.38541618194246752 ) ) ;
#11486 = CARTESIAN_POINT ( 'NONE',  ( 1.469576158976823356E-15, 50.00000000000000000, -73.00000000000001421 ) ) ;
#11487 = ADVANCED_FACE ( 'NONE', ( #43924 ), #76820, .T. ) ;
#11488 = CARTESIAN_POINT ( 'NONE',  ( -12.48795976855787870, -3.509606880211245006, -13.74293554157829078 ) ) ;
#11489 = CARTESIAN_POINT ( 'NONE',  ( 41.92198544132045868, 435.4206365487824542, 7.395723383306480159 ) ) ;
#11490 = EDGE_LOOP ( 'NONE', ( #41850, #99313, #52370, #96284, #2775 ) ) ;
#11491 = CARTESIAN_POINT ( 'NONE',  ( -7.500000000000006217, 40.00000000000064659, -68.91429205785792078 ) ) ;
#11493 = CARTESIAN_POINT ( 'NONE',  ( 32.37148614391195167, -36.02175558211217066, 33.41981937705683947 ) ) ;
#11492 = CARTESIAN_POINT ( 'NONE',  ( 43.21901510197806573, 436.3299561109158731, 19.40633274081966420 ) ) ;
#11494 = CARTESIAN_POINT ( 'NONE',  ( 25.22241582816893413, -4.285714285714286476, -3.301606509414618973 ) ) ;
#11495 = EDGE_CURVE ( 'NONE', #64080, #95206, #76813, .T. ) ;
#11496 = ORIENTED_EDGE ( 'NONE', *, *, #61844, .F. ) ;
#11497 = CARTESIAN_POINT ( 'NONE',  ( 0.000000000000000000, -4.000000000000003553, 112.0000000000000000 ) ) ;
#11498 = B_SPLINE_CURVE_WITH_KNOTS ( 'NONE', 3,
 ( #9901, #42809, #82737, #98386, #187, #99979, #25610, #57384, #75703, #33152, #90297, #1801, #91376, #42269, #74630, #92413, #58469, #34759 ),
 .UNSPECIFIED., .F., .F.,
 ( 4, 2, 2, 2, 2, 2, 2, 2, 4 ),
 ( 0.000000000000000000, 0.1250000000000000555, 0.2500000000000001110, 0.3750000000000000555, 0.5000000000000000000, 0.6249999999999998890, 0.7499999999999998890, 0.8749999999999998890, 1.000000000000000000 ),
 .UNSPECIFIED. ) ;
#11500 = CARTESIAN_POINT ( 'NONE',  ( -35.56416567323501710, 480.2820146177156175, -4.363888856302766683 ) ) ;
#11499 = CARTESIAN_POINT ( 'NONE',  ( -26.12422881270600783, 34.87013364854426101, -9.598205162888435282 ) ) ;
#11501 = DIRECTION ( 'NONE',  ( 1.000000000000000000, 1.224606353822377258E-16, 0.000000000000000000 ) ) ;
#11502 = CARTESIAN_POINT ( 'NONE',  ( -33.26763304901776763, 435.2198496106717585, 10.58492093550778179 ) ) ;
#11503 = CARTESIAN_POINT ( 'NONE',  ( -7.500000000000005329, -3.000000000000000000, -52.94236561372732552 ) ) ;
#11504 = DIRECTION ( 'NONE',  ( 0.5166563581655553294, 0.4014477553984801550, -0.7562446080816890293 ) ) ;
#11505 = DIRECTION ( 'NONE',  ( 0.000000000000000000, -1.000000000000000000, 0.000000000000000000 ) ) ;
#11506 = ORIENTED_EDGE ( 'NONE', *, *, #98674, .T. ) ;
#11507 = CARTESIAN_POINT ( 'NONE',  ( 91.87144242711445941, -60.00000000000000711, 10.36148848589531646 ) ) ;
#11508 = AXIS2_PLACEMENT_3D ( 'NONE', #29886, #79463, #62771 ) ;
#11509 =( NAMED_UNIT ( * ) SI_UNIT ( $, .STERADIAN. ) SOLID_ANGLE_UNIT ( ) );
#11510 = CARTESIAN_POINT ( 'NONE',  ( 9.833493305133801599, 4.898587196589405926E-16, -4.000000000000001776 ) ) ;
#11511 = CARTESIAN_POINT ( 'NONE',  ( -6.731385053086962778, 41.26098029351368979, -70.78618130022729815 ) ) ;
#11512 = CARTESIAN_POINT ( 'NONE',  ( 0.000000000000000000, -100.0000000000000000, 0.000000000000000000 ) ) ;
#11513 = ORIENTED_EDGE ( 'NONE', *, *, #40084, .T. ) ;
#11514 = CARTESIAN_POINT ( 'NONE',  ( -106.1473986865280352, -29.99999999999119282, 193.5445986010597608 ) ) ;
#11515 = ORIENTED_EDGE ( 'NONE', *, *, #31994, .F. ) ;
#11516 = CARTESIAN_POINT ( 'NONE',  ( 0.000000000000000000, 67.00000000000002842, -7.025805963803935406 ) ) ;
#11517 = CARTESIAN_POINT ( 'NONE',  ( 1.101454001169991148, -14.95253250404446632, -12.16137996778338781 ) ) ;
#11518 = DIRECTION ( 'NONE',  ( 1.734723475976806108E-16, -1.000000000000000000, 0.000000000000000000 ) ) ;
#11519 = CARTESIAN_POINT ( 'NONE',  ( 14.87170168469208953, 23.06219547135946968, 1.058210525649228906 ) ) ;
#11521 = CARTESIAN_POINT ( 'NONE',  ( 82.37929189246122519, -37.80917422459863531, -12.96937234471123190 ) ) ;
#11520 = AXIS2_PLACEMENT_3D ( 'NONE', #52718, #77001, #26378 ) ;
#11522 = CARTESIAN_POINT ( 'NONE',  ( -27.82417241905227101, 305.6171509223005387, -9.386799076929978725 ) ) ;
#11523 = CARTESIAN_POINT ( 'NONE',  ( 8.431345355002174176E-24, 304.8518027762757470, -9.000000000000005329 ) ) ;
#11524 = DIRECTION ( 'NONE',  ( -1.000000000000000000, -0.000000000000000000, -0.000000000000000000 ) ) ;
#11525 = CARTESIAN_POINT ( 'NONE',  ( 0.000000000000000000, 4.898587196589412829E-16, -4.000000000000000000 ) ) ;
#11526 = ORIENTED_EDGE ( 'NONE', *, *, #76027, .T. ) ;
#11527 = CARTESIAN_POINT ( 'NONE',  ( -6.499999999999999112, -2.727365451014163167, -5.874157743772093987 ) ) ;
#11528 = VERTEX_POINT ( 'NONE', #35877 ) ;
#11529 = EDGE_CURVE ( 'NONE', #74683, #11535, #11365, .T. ) ;
#11530 = CARTESIAN_POINT ( 'NONE',  ( 48.15068916914983532, 11.33291430652588971, -14.35535821593549954 ) ) ;
#11531 = CIRCLE ( 'NONE', #6363, 5.000000000000000000 ) ;
#11532 = VECTOR ( 'NONE', #93174, 1000.000000000000000 ) ;
#11533 = AXIS2_PLACEMENT_3D ( 'NONE', #46897, #79803, #38831 ) ;
#11535 = VERTEX_POINT ( 'NONE', #27794 ) ;
#11534 = CARTESIAN_POINT ( 'NONE',  ( -30.00000000000000000, 0.000000000000000000, 0.000000000000000000 ) ) ;
#11536 = CARTESIAN_POINT ( 'NONE',  ( 75.97406738546011695, -29.07565650354853659, 117.1859408371087881 ) ) ;
#11537 = EDGE_CURVE ( 'NONE', #88345, #97345, #51629, .T. ) ;
#11538 = ORIENTED_EDGE ( 'NONE', *, *, #14486, .F. ) ;
#11539 = CARTESIAN_POINT ( 'NONE',  ( 3.816044156919698782, -48.93725730783727812, 40.64983015004354172 ) ) ;
#11540 = CIRCLE ( 'NONE', #61545, 12.00000000000001066 ) ;
#11541 = CARTESIAN_POINT ( 'NONE',  ( 2.977408999572650927, -21.87500000204838813, -7.188101187500000933 ) ) ;
#11542 = CARTESIAN_POINT ( 'NONE',  ( -90.87004379432312362, -57.61277171722555579, 204.1615020926832358 ) ) ;
#11543 = EDGE_CURVE ( 'NONE', #89196, #106610, #24610, .T. ) ;
#11544 = ORIENTED_EDGE ( 'NONE', *, *, #61853, .F. ) ;
#11545 =( NAMED_UNIT ( * ) SI_UNIT ( $, .STERADIAN. ) SOLID_ANGLE_UNIT ( ) );
#11546 = DIRECTION ( 'NONE',  ( -1.000000000000000000, -1.224606353822377258E-16, -0.000000000000000000 ) ) ;
#11547 = CARTESIAN_POINT ( 'NONE',  ( 103.9399051704855736, -45.28278063994613234, 168.0512949665413771 ) ) ;
#11548 = CARTESIAN_POINT ( 'NONE',  ( -9.253500431420428995, 83.70228450082292682, 3.792688295761951434 ) ) ;
#11549 = CARTESIAN_POINT ( 'NONE',  ( 48.02835407290504577, 16.78162100668611956, -14.35535821593549954 ) ) ;
#11550 = CARTESIAN_POINT ( 'NONE',  ( -8.000000000000000000, -19.43750000409677270, -9.797174393178825657E-16 ) ) ;
#11551 = DIRECTION ( 'NONE',  ( -1.000000000000000000, -0.000000000000000000, -0.000000000000000000 ) ) ;
#11552 = CARTESIAN_POINT ( 'NONE',  ( 9.843481099141470736, 246.4079544384660494, -1.779148000612204017 ) ) ;
#11553 = B_SPLINE_CURVE_WITH_KNOTS ( 'NONE', 3,
 ( #73729, #91005, #40839, #25224, #57537, #81806, #7398, #98538 ),
 .UNSPECIFIED., .F., .F.,
 ( 4, 2, 2, 4 ),
 ( 0.02285338878549945940, 0.02519297481083175236, 0.02636276782349789710, 0.02753256083616404531 ),
 .UNSPECIFIED. ) ;
#11554 = CARTESIAN_POINT ( 'NONE',  ( 29.08076923076923137, 1.411358822780289120E-15, 0.000000000000000000 ) ) ;
#11555 = PRESENTATION_LAYER_ASSIGNMENT (  '', '', ( #32302 ) ) ;
#11556 = CARTESIAN_POINT ( 'NONE',  ( 32.17608548772838617, 486.0066403424745545, 5.076835838892871600 ) ) ;
#11557 = DIRECTION ( 'NONE',  ( -1.000000000000000000, -4.493451613012042306E-20, 9.836563810905641458E-22 ) ) ;
#11558 = CARTESIAN_POINT ( 'NONE',  ( 13.69330508143927538, 1.340359594676612611E-15, 0.000000000000000000 ) ) ;
#11559 = ORIENTED_EDGE ( 'NONE', *, *, #5735, .F. ) ;
#11560 = CARTESIAN_POINT ( 'NONE',  ( -0.7777777777777786783, -54.00000000000000000, 40.97837836547555668 ) ) ;
#11561 = DIRECTION ( 'NONE',  ( 0.5735764363510491570, -0.8191520442889895781, 1.003171929053522035E-16 ) ) ;
#11562 = CARTESIAN_POINT ( 'NONE',  ( -7.500000000000005329, -3.000000000000000888, -52.94236561372726868 ) ) ;
#11563 = CARTESIAN_POINT ( 'NONE',  ( 45.32577667521739784, -27.72066794804566570, -35.73301877889856826 ) ) ;
#11564 = CARTESIAN_POINT ( 'NONE',  ( -85.41469452698387954, -30.00000000000000355, 174.1069072483980165 ) ) ;
#11565 = EDGE_CURVE ( 'NONE', #96013, #1084, #71646, .T. ) ;
#11566 = B_SPLINE_CURVE_WITH_KNOTS ( 'NONE', 3,
 ( #22633, #14474, #64142, #97008 ),
 .UNSPECIFIED., .F., .F.,
 ( 4, 4 ),
 ( 3.469446951953614189E-18, 0.0001993833013644588040 ),
 .UNSPECIFIED. ) ;
#11567 = ORIENTED_EDGE ( 'NONE', *, *, #101646, .T. ) ;
#11568 = CARTESIAN_POINT ( 'NONE',  ( 33.94783393359906398, 484.1261039197348737, 1.321740980885009353 ) ) ;
#11569 = CARTESIAN_POINT ( 'NONE',  ( 77.44455754849047935, -57.51855352125810583, 195.7701994778959431 ) ) ;
#11570 = CARTESIAN_POINT ( 'NONE',  ( 5.799999999999999822, 0.000000000000000000, 8.000000000000000000 ) ) ;
#11571 = EDGE_CURVE ( 'NONE', #47451, #9744, #10481, .T. ) ;
#11572 = AXIS2_PLACEMENT_3D ( 'NONE', #76629, #68570, #101455 ) ;
#11573 = CARTESIAN_POINT ( 'NONE',  ( 32.25685646263797679, -30.38137028985621413, -38.05272615982493534 ) ) ;
#11574 = CARTESIAN_POINT ( 'NONE',  ( 7.500000000000007105, -4.999999999999999112, -68.91429205785460965 ) ) ;
#11575 = FACE_OUTER_BOUND ( 'NONE', #19486, .T. ) ;
#11576 = CARTESIAN_POINT ( 'NONE',  ( -72.00682906772283332, -60.00000000000000000, 154.3286074057541555 ) ) ;
#11577 = STYLED_ITEM ( 'NONE', ( #67036 ), #7067 ) ;
#11578 = CARTESIAN_POINT ( 'NONE',  ( 29.08076923076923137, -4.171999999999999709, 0.000000000000000000 ) ) ;
#11579 =( NAMED_UNIT ( * ) PLANE_ANGLE_UNIT ( ) SI_UNIT ( $, .RADIAN. ) );
#11580 = CONICAL_SURFACE ( 'NONE', #85683, 4.000000000000001776, 0.9599310885968808105 ) ;
#11581 = CARTESIAN_POINT ( 'NONE',  ( -86.54352349054052240, -24.44773404303954578, 184.2160000694978237 ) ) ;
#11582 = ORIENTED_EDGE ( 'NONE', *, *, #75895, .T. ) ;
#11583 = CARTESIAN_POINT ( 'NONE',  ( -41.70256300459694643, 461.0340457114390347, 3.032228049028243611 ) ) ;
#11584 = CARTESIAN_POINT ( 'NONE',  ( -0.9846993451217399551, -18.58623111607190026, 26.98735514561435522 ) ) ;
#11585 = CARTESIAN_POINT ( 'NONE',  ( -5.484632972945890472, 41.99999999999999289, -59.73832710422585990 ) ) ;
#11586 = DIRECTION ( 'NONE',  ( -1.000000000000000000, -1.224606353822377258E-16, -0.000000000000000000 ) ) ;
#11587 = CARTESIAN_POINT ( 'NONE',  ( -7.308109670146557768, 54.29019187464274410, 2.720881023164113177 ) ) ;
#11588 = EDGE_LOOP ( 'NONE', ( #84877, #67715, #48142, #58819, #57644, #80225 ) ) ;
#11589 = CARTESIAN_POINT ( 'NONE',  ( -35.99330346212021681, 343.8006504399280061, -0.4438237030743195644 ) ) ;
#11590 = CARTESIAN_POINT ( 'NONE',  ( 46.00000000000000000, 450.0000000000002274, 13.20242257375370976 ) ) ;
#11591 = DIRECTION ( 'NONE',  ( -1.000000000000000000, -1.224606353822377258E-16, -0.000000000000000000 ) ) ;
#11592 = AXIS2_PLACEMENT_3D ( 'NONE', #1776, #9872, #42785 ) ;
#11593 = VERTEX_POINT ( 'NONE', #55912 ) ;
#11594 = CARTESIAN_POINT ( 'NONE',  ( 24.55741454880129027, 303.7856203223532816, -9.798360968772033885 ) ) ;
#11595 = CARTESIAN_POINT ( 'NONE',  ( 44.43774958859658142, 337.2802145563449017, 0.2445019049555710311 ) ) ;
#11596 = DIRECTION ( 'NONE',  ( 0.000000000000000000, 0.000000000000000000, -1.000000000000000000 ) ) ;
#11597 = CARTESIAN_POINT ( 'NONE',  ( 8.875907993205162327, 53.84819675155885932, -1.561518095665555883 ) ) ;
#11598 = CARTESIAN_POINT ( 'NONE',  ( 89.52590460267296635, -30.00000000000006395, 22.04891038916446888 ) ) ;
#11599 = CARTESIAN_POINT ( 'NONE',  ( -79.56974465040984512, -53.38012466183634075, 159.7390108954374455 ) ) ;
#11600 = ORIENTED_EDGE ( 'NONE', *, *, #7935, .F. ) ;
#11601 = DIRECTION ( 'NONE',  ( -1.000000000000000000, -1.224606353822377258E-16, -0.000000000000000000 ) ) ;
#11602 = CARTESIAN_POINT ( 'NONE',  ( 4.658465013329196047, 251.3236387967309327, 3.783534922165387115 ) ) ;
#11603 = AXIS2_PLACEMENT_3D ( 'NONE', #105719, #47480, #80378 ) ;
#11604 = PRESENTATION_STYLE_ASSIGNMENT (( #45071 ) ) ;
#11605 = CIRCLE ( 'NONE', #71903, 0.5000000000000004441 ) ;
#11606 = DIRECTION ( 'NONE',  ( 0.000000000000000000, 1.000000000000000000, 5.787437586309764365E-15 ) ) ;
#11607 = CARTESIAN_POINT ( 'NONE',  ( 41.10432692360283369, 313.4425910679791514, -5.561186666570553605 ) ) ;
#11608 = CARTESIAN_POINT ( 'NONE',  ( 43.72316710615049118, 464.1667603278397110, 8.066774506831963620 ) ) ;
#11609 = ORIENTED_EDGE ( 'NONE', *, *, #861, .F. ) ;
#11610 = CARTESIAN_POINT ( 'NONE',  ( -19.70764564238367100, 304.7954121406193053, 9.925013215726757210 ) ) ;
#11611 = CARTESIAN_POINT ( 'NONE',  ( 31.03678703375047476, 438.6650838204854495, 21.86890379897699788 ) ) ;
#11612 = CARTESIAN_POINT ( 'NONE',  ( -2.977408999572654480, -24.12500000204838457, 7.188101187499999156 ) ) ;
#11613 = ORIENTED_EDGE ( 'NONE', *, *, #19066, .T. ) ;
#11614 =( NAMED_UNIT ( * ) PLANE_ANGLE_UNIT ( ) SI_UNIT ( $, .RADIAN. ) );
#11615 = CONICAL_SURFACE ( 'NONE', #35774, 5.000000000000001776, 0.9599310885968803664 ) ;
#11616 = CARTESIAN_POINT ( 'NONE',  ( 3.082707893549380351, 15.00000000000000000, 9.999999999999998224 ) ) ;
#11617 = CARTESIAN_POINT ( 'NONE',  ( 5.622685207874442703, 41.99823429251897977, -69.46126848786613550 ) ) ;
#11618 = ADVANCED_FACE ( 'NONE', ( #24150 ), #80742, .T. ) ;
#11619 = CARTESIAN_POINT ( 'NONE',  ( 53.52139369741866659, 50.00000000000000000, 33.73130704865685914 ) ) ;
#11620 = DIRECTION ( 'NONE',  ( -1.000000000000000000, -1.224606353822377258E-16, -0.000000000000000000 ) ) ;
#11621 = STYLED_ITEM ( 'NONE', ( #77251 ), #43674 ) ;
#11622 = CARTESIAN_POINT ( 'NONE',  ( -9.999999999999982236, 7.499999999999973355, 0.000000000000000000 ) ) ;
#11623 = ORIENTED_EDGE ( 'NONE', *, *, #29375, .T. ) ;
#11624 = CARTESIAN_POINT ( 'NONE',  ( 89.42130242191619516, -60.00000000000001421, -19.83448431725998518 ) ) ;
#11626 = CARTESIAN_POINT ( 'NONE',  ( 23.57173127243913413, -35.99637045962803228, 30.88673654114889544 ) ) ;
#11625 = CARTESIAN_POINT ( 'NONE',  ( -60.31416392689769879, -59.99999999999997158, 109.8312514449790456 ) ) ;
#11627 = CARTESIAN_POINT ( 'NONE',  ( 3.200388772515927248E-15, 60.33964880548970200, -13.06657876680918662 ) ) ;
#11628 = EDGE_CURVE ( 'NONE', #80282, #9641, #8453, .T. ) ;
#11629 = CARTESIAN_POINT ( 'NONE',  ( -36.95781401624343943, -60.28554291635620643, 40.61646249653143315 ) ) ;
#11630 = ORIENTED_EDGE ( 'NONE', *, *, #68656, .T. ) ;
#11631 = CARTESIAN_POINT ( 'NONE',  ( 34.28937322550587652, 463.1540285681008413, 5.961485652431926852 ) ) ;
#11632 = DIRECTION ( 'NONE',  ( -1.000000000000000000, -0.000000000000000000, -0.000000000000000000 ) ) ;
#11633 = CARTESIAN_POINT ( 'NONE',  ( -13.80732344291479663, -57.17861966895164016, 24.67475631203899411 ) ) ;
#11634 = CARTESIAN_POINT ( 'NONE',  ( -1.015626162675523636, 51.43337680269377898, -9.747245237717404365 ) ) ;
#11635 = CARTESIAN_POINT ( 'NONE',  ( 6.928203230275507885, -64.73473843067414180, 4.000000000000002665 ) ) ;
#11636 = CARTESIAN_POINT ( 'NONE',  ( 0.000000000000000000, 4.898587196589412829E-16, -4.000000000000000000 ) ) ;
#11638 = ORIENTED_EDGE ( 'NONE', *, *, #17136, .F. ) ;
#11637 = AXIS2_PLACEMENT_3D ( 'NONE', #29590, #61405, #62991 ) ;
#11639 = CARTESIAN_POINT ( 'NONE',  ( 89.64643850830432825, 1.030564683017419500E-14, 0.000000000000000000 ) ) ;
#11640 = CARTESIAN_POINT ( 'NONE',  ( 43.71217423904096222, 435.6632154632235938, 9.092528312217307729 ) ) ;
#11641 = ORIENTED_EDGE ( 'NONE', *, *, #9213, .F. ) ;
#11642 = CARTESIAN_POINT ( 'NONE',  ( 91.28451791618600453, -29.99999999999999289, 190.6136022142257502 ) ) ;
#11643 = CARTESIAN_POINT ( 'NONE',  ( 42.26632963665326770, 39.52651209077802008, -49.94030005733648636 ) ) ;
#11644 = CARTESIAN_POINT ( 'NONE',  ( 0.3498606326581470416, 15.11603512203462962, 10.00000000000000000 ) ) ;
#11645 = CIRCLE ( 'NONE', #6480, 3.309500000000007880 ) ;
#11646 = CARTESIAN_POINT ( 'NONE',  ( 80.98167351161701788, -29.99999999999999645, 4.326988430357994631 ) ) ;
#11647 =( NAMED_UNIT ( * ) SI_UNIT ( $, .STERADIAN. ) SOLID_ANGLE_UNIT ( ) );
#11648 = ORIENTED_EDGE ( 'NONE', *, *, #85692, .F. ) ;
#11649 = EDGE_CURVE ( 'NONE', #6102, #22089, #48998, .T. ) ;
#11650 = ORIENTED_EDGE ( 'NONE', *, *, #13081, .F. ) ;
#11651 = ORIENTED_EDGE ( 'NONE', *, *, #73377, .T. ) ;
#11652 = CARTESIAN_POINT ( 'NONE',  ( -32.84088564781242781, 464.9638558180852215, 11.24476942535882706 ) ) ;
#11653 = CARTESIAN_POINT ( 'NONE',  ( 49.55398133112713310, 40.83861519483421176, -42.37453886910446244 ) ) ;
#11654 = DIRECTION ( 'NONE',  ( 0.000000000000000000, -1.000000000000000000, 0.000000000000000000 ) ) ;
#11655 = CARTESIAN_POINT ( 'NONE',  ( 5.910690929868577470, -13.86495906093194463, -1.065041252563911467 ) ) ;
#11656 = CARTESIAN_POINT ( 'NONE',  ( -31.35426068356128582, 438.7453971934658625, 22.94710527597258931 ) ) ;
#11657 = CARTESIAN_POINT ( 'NONE',  ( -6.928203230275507885, -85.00000000000000000, -4.000000000000001776 ) ) ;
#11658 = CARTESIAN_POINT ( 'NONE',  ( 39.08667504521157099, 48.00000000000000000, -56.76470588235297043 ) ) ;
#11659 = AXIS2_PLACEMENT_3D ( 'NONE', #980, #100779, #8581 ) ;
#11660 = ORIENTED_EDGE ( 'NONE', *, *, #51143, .F. ) ;
#11661 = CARTESIAN_POINT ( 'NONE',  ( 11.99999999999999467, 50.00000000000000000, -86.57079632498522415 ) ) ;
#11662 = ORIENTED_EDGE ( 'NONE', *, *, #61984, .T. ) ;
#11663 = FACE_OUTER_BOUND ( 'NONE', #106147, .T. ) ;
#11664 = CARTESIAN_POINT ( 'NONE',  ( 22.02269777243552795, 303.1965344776037341, 10.01107272578568441 ) ) ;
#11665 = DIRECTION ( 'NONE',  ( -0.000000000000000000, 1.000000000000000000, -0.000000000000000000 ) ) ;
#11666 = STYLED_ITEM ( 'NONE', ( #76420 ), #67270 ) ;
#11667 = ORIENTED_EDGE ( 'NONE', *, *, #54336, .T. ) ;
#11668 = CARTESIAN_POINT ( 'NONE',  ( 28.43271360265383052, 12.18326821505114310, -40.99299228862982147 ) ) ;
#11669 = CARTESIAN_POINT ( 'NONE',  ( 5.000000000000000000, -14.21727251090713828, 9.320362779989000757 ) ) ;
#11670 = CARTESIAN_POINT ( 'NONE',  ( 26.18186645338464302, 296.0319025976779699, 2.191702204871421422 ) ) ;
#11671 = CARTESIAN_POINT ( 'NONE',  ( -9.635469362647075542, 51.40912437293231818, 2.123716195014139885 ) ) ;
#11672 = EDGE_CURVE ( 'NONE', #19372, #62030, #95782, .T. ) ;
#11673 = ORIENTED_EDGE ( 'NONE', *, *, #99441, .T. ) ;
#11674 = DIRECTION ( 'NONE',  ( -1.000000000000000000, -0.000000000000000000, -0.000000000000000000 ) ) ;
#11675 = LINE ( 'NONE', #68345, #24374 ) ;
#11676 = CARTESIAN_POINT ( 'NONE',  ( 23.86650669486618881, 4.898587196589413815E-16, -4.000000000000000888 ) ) ;
#11677 = AXIS2_PLACEMENT_3D ( 'NONE', #90014, #106175, #32337 ) ;
#11679 = CARTESIAN_POINT ( 'NONE',  ( 19.03532703341449306, 294.6737986316037450, 9.899163670852404451 ) ) ;
#11678 =( GEOMETRIC_REPRESENTATION_CONTEXT ( 3 ) GLOBAL_UNCERTAINTY_ASSIGNED_CONTEXT ( ( #95573 ) ) GLOBAL_UNIT_ASSIGNED_CONTEXT ( ( #60464, #45329, #85244 ) ) REPRESENTATION_CONTEXT ( 'NONE', 'WORKASPACE' ) );
#11680 = CARTESIAN_POINT ( 'NONE',  ( 42.88690168185203788, 465.8389250139256319, 12.02233836084533181 ) ) ;
#11681 = AXIS2_PLACEMENT_3D ( 'NONE', #30076, #79660, #86194 ) ;
#11682 = CARTESIAN_POINT ( 'NONE',  ( 9.981531048852463783, 15.23280014800325688, 0.7018335428337066917 ) ) ;
#11683 = CARTESIAN_POINT ( 'NONE',  ( 85.68274303767356059, -57.45247238031033987, 192.8335385098638994 ) ) ;
#11684 = CARTESIAN_POINT ( 'NONE',  ( -5.293208566653007097, 18.42467780193287297, -37.80131242301784766 ) ) ;
#11685 = CARTESIAN_POINT ( 'NONE',  ( -9.061657589588678618, 137.7585088366314210, 4.999999999999998224 ) ) ;
#11686 = ORIENTED_EDGE ( 'NONE', *, *, #96581, .T. ) ;
#11687 = CARTESIAN_POINT ( 'NONE',  ( -7.233900571379007438, -15.80755961705004609, -35.01922747709534889 ) ) ;
#11688 = FACE_OUTER_BOUND ( 'NONE', #83713, .T. ) ;
#11689 = CARTESIAN_POINT ( 'NONE',  ( 13.38090213880806978, -54.00000000000000711, 31.11721482942554928 ) ) ;
#11690 = CARTESIAN_POINT ( 'NONE',  ( 34.24294763429116983, 434.2296471008492631, 10.63362831703380174 ) ) ;
#11691 = CARTESIAN_POINT ( 'NONE',  ( -94.80346114260228774, -30.00000000000000711, 116.7752331319604906 ) ) ;
#11692 = ADVANCED_FACE ( 'NONE', ( #15485 ), #14941, .T. ) ;
#11693 = AXIS2_PLACEMENT_3D ( 'NONE', #68508, #10766, #101399 ) ;
#11694 = CARTESIAN_POINT ( 'NONE',  ( -1.049032378834029666, -6.899894373156710614, -0.3607371497494648582 ) ) ;
#11695 = CARTESIAN_POINT ( 'NONE',  ( 1.463027203524020825, -57.67120326094947558, 41.61038173843766685 ) ) ;
#11697 = SURFACE_STYLE_USAGE ( .BOTH. , #45165 ) ;
#11696 = CARTESIAN_POINT ( 'NONE',  ( 36.50553548277586913, 490.9914377858967782, 12.47054410074822783 ) ) ;
#11698 = EDGE_CURVE ( 'NONE', #82092, #14056, #76073, .T. ) ;
#11699 = AXIS2_PLACEMENT_3D ( 'NONE', #98900, #24535, #59006 ) ;
#11700 = CARTESIAN_POINT ( 'NONE',  ( 0.000000000000000000, 0.000000000000000000, 0.000000000000000000 ) ) ;
#11701 = CARTESIAN_POINT ( 'NONE',  ( -80.00000000000000000, 500000.0000000000582, -21.09707704303352926 ) ) ;
#11702 = CARTESIAN_POINT ( 'NONE',  ( 4.999999999999995559, -46.00000000000000000, 40.07669683062201926 ) ) ;
#11703 = CARTESIAN_POINT ( 'NONE',  ( 53.78349330513380266, 6.975173280561618775E-15, 0.000000000000000000 ) ) ;
#11704 = CARTESIAN_POINT ( 'NONE',  ( 32.85093540130672807, -22.62736283781948288, -31.69982964332332998 ) ) ;
#11705 = AXIS2_PLACEMENT_3D ( 'NONE', #36644, #28020, #60369 ) ;
#11706 = CARTESIAN_POINT ( 'NONE',  ( -26.62684460577862566, -53.39439586559441153, 34.52290616355812602 ) ) ;
#11707 = EDGE_CURVE ( 'NONE', #41900, #73170, #44007, .T. ) ;
#11708 = EDGE_LOOP ( 'NONE', ( #31154, #14243, #48133, #97883, #6739 ) ) ;
#11709 = CARTESIAN_POINT ( 'NONE',  ( 5.744562646538026840, 12.72967408581656201, 3.999999999999999112 ) ) ;
#11710 = CARTESIAN_POINT ( 'NONE',  ( -20.49954036836691174, -53.40101138645616885, 33.37275672667104232 ) ) ;
#11712 = CARTESIAN_POINT ( 'NONE',  ( -37.03219520467648351, 439.7234317543791917, 24.13053059517222820 ) ) ;
#11711 = CARTESIAN_POINT ( 'NONE',  ( -0.7857478027959594602, 28.10741379899660686, 38.51436396715669730 ) ) ;
#11713 = EDGE_LOOP ( 'NONE', ( #69465, #76513, #12368, #32632 ) ) ;
#11714 = VECTOR ( 'NONE', #91454, 1000.000000000000227 ) ;
#11715 = CARTESIAN_POINT ( 'NONE',  ( 56.96666666666666856, 6.915964383211875250E-15, 0.000000000000000000 ) ) ;
#11716 = ORIENTED_EDGE ( 'NONE', *, *, #81985, .F. ) ;
#11717 = VECTOR ( 'NONE', #50502, 1000.000000000000000 ) ;
#11718 = CARTESIAN_POINT ( 'NONE',  ( 16.03930365250129952, 4.449877915870326106, 3.144092084176011159 ) ) ;
#11719 = CARTESIAN_POINT ( 'NONE',  ( -43.41290683822509067, 487.0833545439620593, 7.569976829064872348 ) ) ;
#11720 = ORIENTED_EDGE ( 'NONE', *, *, #82812, .T. ) ;
#11721 = DIRECTION ( 'NONE',  ( -1.224646799147353454E-16, 0.000000000000000000, -1.000000000000000000 ) ) ;
#11722 = DIRECTION ( 'NONE',  ( -1.000000000000000000, -1.224606353822377258E-16, -0.000000000000000000 ) ) ;
#11723 = CARTESIAN_POINT ( 'NONE',  ( 100.3444285902703683, -37.84519586678835879, 189.9254009749505485 ) ) ;
#11724 = CARTESIAN_POINT ( 'NONE',  ( -6.944371705245973025, -9.461003085754503772, -3.972324460300561633 ) ) ;
#11725 = CONICAL_SURFACE ( 'NONE', #32410, 3.309500000000001663, 0.9599310885968770357 ) ;
#11726 = ORIENTED_EDGE ( 'NONE', *, *, #50059, .T. ) ;
#11727 = ORIENTED_EDGE ( 'NONE', *, *, #69410, .F. ) ;
#11728 = ORIENTED_EDGE ( 'NONE', *, *, #31588, .F. ) ;
#11730 =( BOUNDED_SURFACE ( )  B_SPLINE_SURFACE ( 3, 2, ( 
 ( #28347, #11583, #44510 ),
 ( #77935, #4043, #18117 ),
 ( #2965, #19215, #67192 ),
 ( #77399, #102200, #68793 ) ),
 .UNSPECIFIED., .F., .F., .T. ) 
 B_SPLINE_SURFACE_WITH_KNOTS ( ( 4, 4 ),
 ( 3, 3 ),
 ( 2.688821387764050996E-17, 0.001313222278771114223 ),
 ( 0.000000000000000000, 1.000000000000000000 ),
 .UNSPECIFIED. ) 
 GEOMETRIC_REPRESENTATION_ITEM ( )  RATIONAL_B_SPLINE_SURFACE ( (
 ( 1.000000000000000000, 0.8270258197359517949, 1.000000000000000000),
 ( 1.000000000000000000, 0.8180084242886423995, 1.000000000000000000),
 ( 1.000000000000000000, 0.8088315090908753113, 1.000000000000000000),
 ( 1.000000000000000000, 0.7996726260853282975, 1.000000000000000000) ) ) 
 REPRESENTATION_ITEM ( '' )  SURFACE ( )  );
#11729 = CARTESIAN_POINT ( 'NONE',  ( 27.89340747318720659, 311.6758220793392979, 11.81716561949889766 ) ) ;
#11731 = DIRECTION ( 'NONE',  ( 0.000000000000000000, -1.000000000000000000, 0.000000000000000000 ) ) ;
#11732 = DIRECTION ( 'NONE',  ( -1.000000000000000000, -1.224606353822377258E-16, -0.000000000000000000 ) ) ;
#11733 = ORIENTED_EDGE ( 'NONE', *, *, #17815, .F. ) ;
#11734 = EDGE_CURVE ( 'NONE', #94312, #93124, #81966, .T. ) ;
#11735 = CARTESIAN_POINT ( 'NONE',  ( 11.08349330513380160, 1.593028355512270567E-15, 0.000000000000000000 ) ) ;
#11736 = CARTESIAN_POINT ( 'NONE',  ( -6.221959883623910059, 4.750744965685583132, -5.000000000000037303 ) ) ;
#11737 = CARTESIAN_POINT ( 'NONE',  ( -28.06723731321121562, -60.00000000007723600, -43.53660501072154432 ) ) ;
#11738 = CARTESIAN_POINT ( 'NONE',  ( 18.71538461538461462, 1.411358822780289120E-15, 0.000000000000000000 ) ) ;
#11739 = CIRCLE ( 'NONE', #37609, 4.172000000000001485 ) ;
#11740 = CARTESIAN_POINT ( 'NONE',  ( 14.20386879384134637, -60.00000000000001421, 39.75101514688974902 ) ) ;
#11741 = CARTESIAN_POINT ( 'NONE',  ( 6.394337469123803075, 3.776351736504755863, -6.540833074877203224 ) ) ;
#11742 = AXIS2_PLACEMENT_3D ( 'NONE', #43593, #39106, #10677 ) ;
#11743 = CARTESIAN_POINT ( 'NONE',  ( -6.736688764309785249, 41.36687430129245513, -58.48851226247030155 ) ) ;
#11744 =( GEOMETRIC_REPRESENTATION_CONTEXT ( 3 ) GLOBAL_UNCERTAINTY_ASSIGNED_CONTEXT ( ( #96986 ) ) GLOBAL_UNIT_ASSIGNED_CONTEXT ( ( #12661, #45065, #29436 ) ) REPRESENTATION_CONTEXT ( 'NONE', 'WORKASPACE' ) );
#11746 = CARTESIAN_POINT ( 'NONE',  ( 4.005264604613198109, -29.02925082544549795, 28.72090773042863887 ) ) ;
#11745 = CARTESIAN_POINT ( 'NONE',  ( -104.4271118349969498, -14.21045842199436926, 141.4138186051453090 ) ) ;
#11747 = EDGE_CURVE ( 'NONE', #44445, #84797, #64746, .T. ) ;
#11748 = AXIS2_PLACEMENT_3D ( 'NONE', #37184, #13385, #38756 ) ;
#11749 = ADVANCED_FACE ( 'NONE', ( #49972 ), #39782, .F. ) ;
#11750 = CARTESIAN_POINT ( 'NONE',  ( -49.24971250091634545, -22.20977592223509234, 44.01979842293178535 ) ) ;
#11751 = VERTEX_POINT ( 'NONE', #81268 ) ;
#11752 = DIRECTION ( 'NONE',  ( 0.5735764363510491570, -0.8191520442889895781, 1.003171929053522035E-16 ) ) ;
#11753 = ORIENTED_EDGE ( 'NONE', *, *, #61575, .T. ) ;
#11754 = CARTESIAN_POINT ( 'NONE',  ( 35.61553451506884471, 436.8848301207117402, 4.737533046128437952 ) ) ;
#11755 = AXIS2_PLACEMENT_3D ( 'NONE', #47618, #80519, #46574 ) ;
#11756 = CARTESIAN_POINT ( 'NONE',  ( 46.00000000000000000, 500.0000000000002274, 0.000000000000000000 ) ) ;
#11757 = DIRECTION ( 'NONE',  ( 0.000000000000000000, 0.000000000000000000, 1.000000000000000000 ) ) ;
#11758 = VERTEX_POINT ( 'NONE', #1405 ) ;
#11759 = LINE ( 'NONE', #28005, #83784 ) ;
#11760 = ORIENTED_EDGE ( 'NONE', *, *, #105357, .F. ) ;
#11761 = CARTESIAN_POINT ( 'NONE',  ( 88.65969019626136571, -29.99999999999445777, -15.66969482918002932 ) ) ;
#11762 = FACE_OUTER_BOUND ( 'NONE', #10588, .T. ) ;
#11763 = CARTESIAN_POINT ( 'NONE',  ( 3.423905177084550555, -49.17202489992536130, 103.8439100969738291 ) ) ;
#11764 = FACE_BOUND ( 'NONE', #76874, .T. ) ;
#11765 = CARTESIAN_POINT ( 'NONE',  ( 19.32152200345201010, 18.64316884708351552, 33.52312678236467747 ) ) ;
#11766 = CARTESIAN_POINT ( 'NONE',  ( 97.71307967711325659, -30.00000000000000000, 190.7721930600256712 ) ) ;
#11767 =( NAMED_UNIT ( * ) SI_UNIT ( $, .STERADIAN. ) SOLID_ANGLE_UNIT ( ) );
#11768 = ORIENTED_EDGE ( 'NONE', *, *, #89884, .T. ) ;
#11769 = EDGE_CURVE ( 'NONE', #34743, #35444, #67764, .T. ) ;
#11770 = B_SPLINE_CURVE_WITH_KNOTS ( 'NONE', 3,
 ( #17534, #18066, #50924, #90340, #81688, #25100, #75747, #82779, #82238, #1299 ),
 .UNSPECIFIED., .F., .F.,
 ( 4, 2, 2, 2, 4 ),
 ( 0.000000000000000000, 0.2500000000000000000, 0.5000000000000000000, 0.7500000000000000000, 1.000000000000000000 ),
 .UNSPECIFIED. ) ;
#11771 = MECHANICAL_DESIGN_GEOMETRIC_PRESENTATION_REPRESENTATION (  '', ( #104790 ), #37625 ) ;
#11772 = ORIENTED_EDGE ( 'NONE', *, *, #50787, .F. ) ;
#11773 = ORIENTED_EDGE ( 'NONE', *, *, #39246, .T. ) ;
#11774 = CARTESIAN_POINT ( 'NONE',  ( 54.95523992838832328, -46.43685162509488151, 63.01994253229578646 ) ) ;
#11775 = CARTESIAN_POINT ( 'NONE',  ( 5.945587289688900157, 41.44588091670027552, -58.45240130220552288 ) ) ;
#11776 = CARTESIAN_POINT ( 'NONE',  ( -7.500000000000007105, 40.00000000000000000, -59.28631038546422616 ) ) ;
#11777 = EDGE_CURVE ( 'NONE', #43097, #31444, #32037, .T. ) ;
#11778 = ORIENTED_EDGE ( 'NONE', *, *, #24588, .F. ) ;
#11779 = CARTESIAN_POINT ( 'NONE',  ( -88.95530016575696663, -38.38408534947410544, -18.14653258153979820 ) ) ;
#11780 = CIRCLE ( 'NONE', #104804, 3.400000000000000355 ) ;
#11781 = ORIENTED_EDGE ( 'NONE', *, *, #52348, .F. ) ;
#11782 =( NAMED_UNIT ( * ) PLANE_ANGLE_UNIT ( ) SI_UNIT ( $, .RADIAN. ) );
#11783 = CARTESIAN_POINT ( 'NONE',  ( 107.4446830570735898, -38.36127121959084008, 194.0442666557358962 ) ) ;
#11784 = CARTESIAN_POINT ( 'NONE',  ( 13.16322211195412528, 19.50307498396639971, 7.601507676661267254 ) ) ;
#11785 = CARTESIAN_POINT ( 'NONE',  ( 84.91903829920845226, -52.70721903688826160, 9.721747065421782352 ) ) ;
#11786 = CARTESIAN_POINT ( 'NONE',  ( 33.10746446218201555, 427.7639272436880447, 25.07524900334581019 ) ) ;
#11787 = CARTESIAN_POINT ( 'NONE',  ( 7.000000000000000000, -14.05766640829038572, -5.232782735144292374 ) ) ;
#11788 = STYLED_ITEM ( 'NONE', ( #16175 ), #31215 ) ;
#11789 = CARTESIAN_POINT ( 'NONE',  ( 34.35000000000000142, -3.309499999999999886, 4.475777889183790779E-16 ) ) ;
#11790 = CARTESIAN_POINT ( 'NONE',  ( 2.083846472846741813E-15, -8.673617379884035472E-16, 17.01589776168603407 ) ) ;
#11791 = CARTESIAN_POINT ( 'NONE',  ( 4.086538315193108950, 138.2907119265738345, 5.000000000000000000 ) ) ;
#11792 = VERTEX_POINT ( 'NONE', #41882 ) ;
#11793 = DIRECTION ( 'NONE',  ( -1.000000000000000000, 0.000000000000000000, 0.000000000000000000 ) ) ;
#11794 = CARTESIAN_POINT ( 'NONE',  ( 16.58679117417341686, 36.41790041698921954, -24.30698433968622396 ) ) ;
#11795 = CARTESIAN_POINT ( 'NONE',  ( 12.61650669486618881, 1.474610560812782335E-15, 0.000000000000000000 ) ) ;
#11796 = ORIENTED_EDGE ( 'NONE', *, *, #86311, .F. ) ;
#11797 = CARTESIAN_POINT ( 'NONE',  ( -4.959056880045103810, 54.27782031566443521, 6.063933026178952801 ) ) ;
#11798 = AXIS2_PLACEMENT_3D ( 'NONE', #103522, #62545, #57472 ) ;
#11799 = CARTESIAN_POINT ( 'NONE',  ( -37.31364329941698799, 312.6956583181383280, 14.24415654474395332 ) ) ;
#11800 = DIRECTION ( 'NONE',  ( -1.000000000000000000, -0.000000000000000000, -0.000000000000000000 ) ) ;
#11801 = CARTESIAN_POINT ( 'NONE',  ( -12.13034742782337361, 42.00000149755588552, -93.82352941176404215 ) ) ;
#11802 = CARTESIAN_POINT ( 'NONE',  ( -8.000000000000000000, -22.24999999999999289, -9.797174393178825657E-16 ) ) ;
#11803 = CARTESIAN_POINT ( 'NONE',  ( 9.041496991692591578, -13.54857058825676575, 31.94122638330012265 ) ) ;
#11804 = AXIS2_PLACEMENT_3D ( 'NONE', #30935, #96179, #21780 ) ;
#11805 = DIRECTION ( 'NONE',  ( 0.000000000000000000, 0.000000000000000000, 1.000000000000000000 ) ) ;
#11806 = PRESENTATION_LAYER_ASSIGNMENT (  '', '', ( #49691 ) ) ;
#11807 = ORIENTED_EDGE ( 'NONE', *, *, #92115, .T. ) ;
#11808 = CARTESIAN_POINT ( 'NONE',  ( 84.42999968110919440, -42.97261461009923522, 183.7496894034296702 ) ) ;
#11809 = FACE_OUTER_BOUND ( 'NONE', #67899, .T. ) ;
#11810 = CIRCLE ( 'NONE', #75568, 0.9999999999999860112 ) ;
#11811 = CARTESIAN_POINT ( 'NONE',  ( 5.799999999999999822, -4.618802153517009401, -8.000000000000001776 ) ) ;
#11812 = ORIENTED_EDGE ( 'NONE', *, *, #74021, .T. ) ;
#11813 = CARTESIAN_POINT ( 'NONE',  ( -90.66722646538110553, -52.70996686316394886, 67.18204429113762899 ) ) ;
#11814 = CARTESIAN_POINT ( 'NONE',  ( -35.45036406932566564, 436.3203772529605544, 5.179456583033978490 ) ) ;
#11815 = CARTESIAN_POINT ( 'NONE',  ( -9.891797161801505922, -5.000000000000002665, -73.72381496649795452 ) ) ;
#11816 = CARTESIAN_POINT ( 'NONE',  ( 14.92666003044830703, -3.000000000000003109, -87.00284506552866048 ) ) ;
#11817 = CARTESIAN_POINT ( 'NONE',  ( -0.8336975375668531640, -21.31741200790257906, -38.55284189565394115 ) ) ;
#11818 = ADVANCED_FACE ( 'NONE', ( #74770 ), #62979, .F. ) ;
#11819 = EDGE_CURVE ( 'NONE', #9067, #51980, #83940, .T. ) ;
#11820 = CARTESIAN_POINT ( 'NONE',  ( 17.06298066294603188, -60.00000000000001421, 39.92720215783332094 ) ) ;
#11821 = CARTESIAN_POINT ( 'NONE',  ( 21.02493137415513758, -26.37324912420831780, 37.08244595263487042 ) ) ;
#11822 = MECHANICAL_DESIGN_GEOMETRIC_PRESENTATION_REPRESENTATION (  '', ( #97909 ), #101384 ) ;
#11823 = FILL_AREA_STYLE ('',( #86810 ) ) ;
#11824 = CARTESIAN_POINT ( 'NONE',  ( 49.49725558192223929, -29.58889863815145915, 45.82038523203005553 ) ) ;
#11825 = CIRCLE ( 'NONE', #80731, 3.999999999999989786 ) ;
#11826 = ADVANCED_FACE ( 'NONE', ( #92563 ), #6135, .T. ) ;
#11828 = CARTESIAN_POINT ( 'NONE',  ( -12.02757221648704444, 21.76040073964190213, 7.011289084098431879 ) ) ;
#11827 = CARTESIAN_POINT ( 'NONE',  ( -40.06514717946188853, -37.64732419053277823, 49.94544317564937330 ) ) ;
#11829 = CARTESIAN_POINT ( 'NONE',  ( 1.959911964311880306, 298.2559866372270676, -10.00257402834314213 ) ) ;
#11830 = CARTESIAN_POINT ( 'NONE',  ( 7.188101187500001821, -10.06250000204838280, -2.977408999572650483 ) ) ;
#11831 = DIRECTION ( 'NONE',  ( 1.000000000000000000, 0.000000000000000000, 0.000000000000000000 ) ) ;
#11832 = PRESENTATION_LAYER_ASSIGNMENT (  '', '', ( #61852 ) ) ;
#11833 = CARTESIAN_POINT ( 'NONE',  ( 6.692588830498428898, 7.935834885954428763, 0.04058884017440190367 ) ) ;
#11834 = ORIENTED_EDGE ( 'NONE', *, *, #18357, .F. ) ;
#11835 = CARTESIAN_POINT ( 'NONE',  ( -17.50000000000003553, 51.77766888148061497, 61.91533629926085780 ) ) ;
#11836 = ADVANCED_FACE ( 'NONE', ( #34899 ), #28587, .T. ) ;
#11837 = ORIENTED_EDGE ( 'NONE', *, *, #70664, .T. ) ;
#11838 = CARTESIAN_POINT ( 'NONE',  ( -12.83107512063730837, 1.658796432365972739, 14.90858414098761209 ) ) ;
#11839 = CARTESIAN_POINT ( 'NONE',  ( 46.00000000000000000, 487.9613292052891325, 0.4638920459505368465 ) ) ;
#11840 = LINE ( 'NONE', #28609, #9688 ) ;
#11842 = CARTESIAN_POINT ( 'NONE',  ( -22.39027729576407921, -47.40902575964246779, -33.77704283917025663 ) ) ;
#11841 = CARTESIAN_POINT ( 'NONE',  ( 9.989285784994834216, 253.9734242744569030, 0.5301777604595797611 ) ) ;
#11843 = VERTEX_POINT ( 'NONE', #18714 ) ;
#11844 =( GEOMETRIC_REPRESENTATION_CONTEXT ( 3 ) GLOBAL_UNCERTAINTY_ASSIGNED_CONTEXT ( ( #106654 ) ) GLOBAL_UNIT_ASSIGNED_CONTEXT ( ( #61638, #79377, #104179 ) ) REPRESENTATION_CONTEXT ( 'NONE', 'WORKASPACE' ) );
#11845 = CARTESIAN_POINT ( 'NONE',  ( -2.499999999999996003, -8.000000000000000000, 9.184850993605129949E-17 ) ) ;
#11846 = PLANE ( 'NONE',  #92726 ) ;
#11847 = CIRCLE ( 'NONE', #96265, 4.000000000000000888 ) ;
#11848 = ORIENTED_EDGE ( 'NONE', *, *, #6781, .F. ) ;
#11849 = CONICAL_SURFACE ( 'NONE', #99708, 4.000000000000001776, 0.9599310885968808105 ) ;
#11850 = DIRECTION ( 'NONE',  ( -0.000000000000000000, -0.000000000000000000, 1.000000000000000000 ) ) ;
#11851 = VECTOR ( 'NONE', #43286, 1000.000000000000000 ) ;
#11852 = FILL_AREA_STYLE ('',( #93319 ) ) ;
#11853 = CARTESIAN_POINT ( 'NONE',  ( -92.62866349064093185, -59.99999999999999289, 28.48677841314170323 ) ) ;
#11854 = ORIENTED_EDGE ( 'NONE', *, *, #46154, .F. ) ;
#11855 = CARTESIAN_POINT ( 'NONE',  ( 0.000000000000000000, 47.00000000000000000, 60.00000000000000000 ) ) ;
#11856 = CARTESIAN_POINT ( 'NONE',  ( 6.683837171061802529, -3.955946848495957457, 6.851900933636990487 ) ) ;
#11857 = FACE_OUTER_BOUND ( 'NONE', #2396, .T. ) ;
#11858 = CARTESIAN_POINT ( 'NONE',  ( -9.165151389911679658, 29.73704489083662494, 3.999999999999999112 ) ) ;
#11860 = FILL_AREA_STYLE ('',( #53402 ) ) ;
#11859 = DIRECTION ( 'NONE',  ( -1.000000000000000000, 0.000000000000000000, 0.000000000000000000 ) ) ;
#11861 = AXIS2_PLACEMENT_3D ( 'NONE', #18015, #101042, #43345 ) ;
#11862 = CARTESIAN_POINT ( 'NONE',  ( -80.64663750670202091, -56.90986277982133856, 175.6256103212931521 ) ) ;
#11863 = AXIS2_PLACEMENT_3D ( 'NONE', #33566, #91273, #601 ) ;
#11864 = ORIENTED_EDGE ( 'NONE', *, *, #39960, .T. ) ;
#11865 = CARTESIAN_POINT ( 'NONE',  ( -17.01594651245413203, -0.000000000000000000, 1.113195845621175684 ) ) ;
#11866 = ORIENTED_EDGE ( 'NONE', *, *, #17702, .F. ) ;
#11867 = EDGE_LOOP ( 'NONE', ( #86189, #1169, #38242, #92862 ) ) ;
#11868 = CARTESIAN_POINT ( 'NONE',  ( -13.05035048250584495, -5.000000000000000000, -10.38464894538556749 ) ) ;
#11869 = SURFACE_SIDE_STYLE ('',( #87901 ) ) ;
#11870 = ORIENTED_EDGE ( 'NONE', *, *, #100717, .T. ) ;
#11871 = EDGE_CURVE ( 'NONE', #82654, #102372, #101721, .T. ) ;
#11872 = B_SPLINE_CURVE_WITH_KNOTS ( 'NONE', 3,
 ( #69816, #28877, #71934, #38529, #63334, #30980, #79493, #103247, #39053, #7185, #21826, #62794, #54665, #47642, #46594, #81074, #71389, #97264, #14743, #80542 ),
 .UNSPECIFIED., .F., .F.,
 ( 4, 2, 2, 2, 2, 2, 2, 2, 2, 4 ),
 ( 0.000000000000000000, 0.001913256305722581480, 0.003826512611445162960, 0.005739768917167741187, 0.007653025222890320715, 0.009566281528612899376, 0.01052290968147418480, 0.01147953783433547197, 0.01339279414005804282, 0.01530605044578061021 ),
 .UNSPECIFIED. ) ;
#11873 = FILL_AREA_STYLE ('',( #27583 ) ) ;
#11874 = CARTESIAN_POINT ( 'NONE',  ( -93.89056551065039002, -57.67583025180931600, 8.072597750090290347 ) ) ;
#11875 = DIRECTION ( 'NONE',  ( -0.000000000000000000, 1.000000000000000000, -0.000000000000000000 ) ) ;
#11876 = AXIS2_PLACEMENT_3D ( 'NONE', #50153, #32409, #39951 ) ;
#11877 = LINE ( 'NONE', #85803, #20431 ) ;
#11878 = CARTESIAN_POINT ( 'NONE',  ( -9.221346651730840449, 103.9516597993166158, -3.869102247876032852 ) ) ;
#11879 = CARTESIAN_POINT ( 'NONE',  ( -13.45844644947841751, -53.47274863452597771, 23.14343646736056570 ) ) ;
#11880 = CARTESIAN_POINT ( 'NONE',  ( -17.07807050392511528, 37.03766137757074972, -21.83949354139809174 ) ) ;
#11881 = CARTESIAN_POINT ( 'NONE',  ( 95.73610373016691710, -30.00000000000000355, 71.50072510963239836 ) ) ;
#11882 = EDGE_CURVE ( 'NONE', #92683, #29639, #27889, .T. ) ;
#11883 = CARTESIAN_POINT ( 'NONE',  ( -88.35884389454342625, -14.21045842199434794, 197.0605769606054594 ) ) ;
#11884 = CARTESIAN_POINT ( 'NONE',  ( -56.34788879306677956, -25.61643386706129988, 57.53393736018574600 ) ) ;
#11885 = VERTEX_POINT ( 'NONE', #60756 ) ;
#11886 = DIRECTION ( 'NONE',  ( -0.000000000000000000, -0.000000000000000000, -1.000000000000000000 ) ) ;
#11887 = ORIENTED_EDGE ( 'NONE', *, *, #87061, .T. ) ;
#11888 = CARTESIAN_POINT ( 'NONE',  ( -104.0447889127541856, -45.26551436310554521, 172.6622363546740360 ) ) ;
#11889 = PRESENTATION_LAYER_ASSIGNMENT (  '', '', ( #91146 ) ) ;
#11890 = CARTESIAN_POINT ( 'NONE',  ( 5.947762761376474749, 6.880090707843042885, -1.083333333333332593 ) ) ;
#11891 = CARTESIAN_POINT ( 'NONE',  ( 5.656854249492378806, -18.87500000409677270, 5.656854249492381470 ) ) ;
#11892 = EDGE_CURVE ( 'NONE', #11843, #49452, #83405, .T. ) ;
#11893 = AXIS2_PLACEMENT_3D ( 'NONE', #39459, #23281, #24351 ) ;
#11894 = ORIENTED_EDGE ( 'NONE', *, *, #43026, .F. ) ;
#11895 = FACE_OUTER_BOUND ( 'NONE', #85593, .T. ) ;
#11896 = CARTESIAN_POINT ( 'NONE',  ( 36.31862201025842296, 26.04192262955948678, -12.31455456606723331 ) ) ;
#11897 = CARTESIAN_POINT ( 'NONE',  ( -2.977408999572654480, -15.50000000204838635, 7.188101187499999156 ) ) ;
#11898 = CARTESIAN_POINT ( 'NONE',  ( -4.582299834663618121, -65.64808143178194655, 13.11537099594930922 ) ) ;
#11899 = CARTESIAN_POINT ( 'NONE',  ( 69.18888888888888289, 6.915964383211875250E-15, 0.000000000000000000 ) ) ;
#11900 = DIRECTION ( 'NONE',  ( 0.7071067811865521247, 8.659560562354877391E-17, 0.7071067811865430208 ) ) ;
#11901 = CARTESIAN_POINT ( 'NONE',  ( -31.19792890532719198, 414.2215770364159084, 25.44228638033458623 ) ) ;
#11902 = FACE_OUTER_BOUND ( 'NONE', #36520, .T. ) ;
#11903 = CARTESIAN_POINT ( 'NONE',  ( -8.792039765168276233, 18.71881101081278942, 0.000000000000000000 ) ) ;
#11904 = DIRECTION ( 'NONE',  ( 0.5735764363510442720, -0.8191520442889930198, 1.003171929053526349E-16 ) ) ;
#11905 = CARTESIAN_POINT ( 'NONE',  ( -7.500000000000007105, 41.91230289050422186, -61.59623549333881698 ) ) ;
#11906 = CARTESIAN_POINT ( 'NONE',  ( -28.38553437247551514, -49.91375019981702366, 34.43038532363013360 ) ) ;
#11907 = CARTESIAN_POINT ( 'NONE',  ( 32.93292175078001094, 485.0466323666404378, 1.209345195306204657 ) ) ;
#11908 = CARTESIAN_POINT ( 'NONE',  ( 48.40637997785970725, -36.06001625196908122, 47.15397699203993653 ) ) ;
#11909 = ORIENTED_EDGE ( 'NONE', *, *, #26014, .F. ) ;
#11910 = CARTESIAN_POINT ( 'NONE',  ( -32.01581173012083070, 487.4782005592821861, 8.020290309115868155 ) ) ;
#11911 = AXIS2_PLACEMENT_3D ( 'NONE', #103874, #87713, #101759 ) ;
#11912 = CARTESIAN_POINT ( 'NONE',  ( 9.036570576874952465, 10.37119081301008094, -0.1387913946425728406 ) ) ;
#11913 = CARTESIAN_POINT ( 'NONE',  ( -84.38815364029120758, -38.74013734265176367, 198.0659774401191271 ) ) ;
#11914 = ORIENTED_EDGE ( 'NONE', *, *, #1883, .T. ) ;
#11915 = LINE ( 'NONE', #26559, #55456 ) ;
#11916 = CARTESIAN_POINT ( 'NONE',  ( -18.93287512597741795, 49.14208625572008060, 62.08427962429427538 ) ) ;
#11917 = DIRECTION ( 'NONE',  ( -0.000000000000000000, 0.000000000000000000, -1.000000000000000000 ) ) ;
#11918 = CARTESIAN_POINT ( 'NONE',  ( 5.225680565739399874, 40.98154495381307783, -70.87362144414954912 ) ) ;
#11919 = AXIS2_PLACEMENT_3D ( 'NONE', #90054, #87033, #5039 ) ;
#11920 = CARTESIAN_POINT ( 'NONE',  ( -32.99999999999998579, 435.0774731480752280, 11.67986145722083613 ) ) ;
#11921 = CARTESIAN_POINT ( 'NONE',  ( 7.500000000000000888, 1.443375672974059443, -7.063244554130002406 ) ) ;
#11922 = ADVANCED_FACE ( 'NONE', ( #52626 ), #46657, .T. ) ;
#11923 = CARTESIAN_POINT ( 'NONE',  ( 103.8573764746737709, -60.00000000000000711, 200.0859602348770920 ) ) ;
#11924 = DIRECTION ( 'NONE',  ( -1.000000000000000000, -0.000000000000000000, -0.000000000000000000 ) ) ;
#11925 = ORIENTED_EDGE ( 'NONE', *, *, #6918, .T. ) ;
#11926 = CARTESIAN_POINT ( 'NONE',  ( 35.75416653242308485, 438.1735696696630953, 3.975240391340852497 ) ) ;
#11927 = AXIS2_PLACEMENT_3D ( 'NONE', #98087, #6409, #39347 ) ;
#11928 = CARTESIAN_POINT ( 'NONE',  ( -75.95768708191903329, -30.00000000000000000, -17.39747055666823172 ) ) ;
#11929 = VERTEX_POINT ( 'NONE', #66699 ) ;
#11931 = CARTESIAN_POINT ( 'NONE',  ( 32.28552837373269568, 464.7648866755952213, 15.30384310833107975 ) ) ;
#11930 = CARTESIAN_POINT ( 'NONE',  ( -84.11778948446114157, -38.75649915743333906, 197.8756380803732213 ) ) ;
#11932 = CARTESIAN_POINT ( 'NONE',  ( 46.00000000000000711, 438.3662639930333285, 10.23871118457565821 ) ) ;
#11933 = CARTESIAN_POINT ( 'NONE',  ( 11.36650669486618881, 4.000000000000003553, 4.898587196589414801E-16 ) ) ;
#11934 = CARTESIAN_POINT ( 'NONE',  ( 16.14595037822613932, 20.23371447307979665, -4.922994507609789849 ) ) ;
#11935 = CARTESIAN_POINT ( 'NONE',  ( -2.977408999572654480, -12.50000000204838990, 7.188101187499999156 ) ) ;
#11936 = SURFACE_STYLE_USAGE ( .BOTH. , #28173 ) ;
#11937 = AXIS2_PLACEMENT_3D ( 'NONE', #42780, #19086, #92385 ) ;
#11938 = CARTESIAN_POINT ( 'NONE',  ( 44.83349330513380693, 1.593028355512270567E-15, 0.000000000000000000 ) ) ;
#11939 = AXIS2_PLACEMENT_3D ( 'NONE', #2869, #10429, #59541 ) ;
#11941 = VERTEX_POINT ( 'NONE', #29986 ) ;
#11940 = CARTESIAN_POINT ( 'NONE',  ( 4.165977904505311358, 16.00000000000000000, -9.090909090909089940 ) ) ;
#11942 = CARTESIAN_POINT ( 'NONE',  ( 81.96385036426019610, -49.96436916644401549, 176.6379167989905739 ) ) ;
#11943 = CARTESIAN_POINT ( 'NONE',  ( -43.78501619230171116, 462.5250674819244523, 5.126974144517244980 ) ) ;
#11944 = CARTESIAN_POINT ( 'NONE',  ( 9.797936955406315818, 88.46671689770482772, -2.012343231877592675 ) ) ;
#11945 = ORIENTED_EDGE ( 'NONE', *, *, #104724, .F. ) ;
#11946 = DIRECTION ( 'NONE',  ( -1.000000000000000000, -0.000000000000000000, -0.000000000000000000 ) ) ;
#11947 = CARTESIAN_POINT ( 'NONE',  ( 16.83488000812927510, 34.23830427773977902, 24.30698433968583316 ) ) ;
#11948 = SURFACE_STYLE_USAGE ( .BOTH. , #93420 ) ;
#11949 = CARTESIAN_POINT ( 'NONE',  ( -4.660674839411965031, 251.3178248530441010, -3.778981567323766555 ) ) ;
#11950 = CARTESIAN_POINT ( 'NONE',  ( 17.89028079457004239, 43.21736803053038045, 5.218346154640485679 ) ) ;
#11951 = VERTEX_POINT ( 'NONE', #53701 ) ;
#11952 = EDGE_CURVE ( 'NONE', #80767, #95757, #34606, .T. ) ;
#11953 = VECTOR ( 'NONE', #98958, 1000.000000000000000 ) ;
#11954 = CARTESIAN_POINT ( 'NONE',  ( -74.08841422782842301, -29.99999999999999645, -18.54496149897586932 ) ) ;
#11955 = FACE_OUTER_BOUND ( 'NONE', #43102, .T. ) ;
#11956 = LINE ( 'NONE', #14070, #54486 ) ;
#11957 = EDGE_CURVE ( 'NONE', #8490, #59552, #56781, .T. ) ;
#11959 = CARTESIAN_POINT ( 'NONE',  ( 0.000000000000000000, 0.000000000000000000, 0.000000000000000000 ) ) ;
#11958 = CARTESIAN_POINT ( 'NONE',  ( 24.05868969682389036, 1.340359594676612611E-15, 0.000000000000000000 ) ) ;
#11960 = ADVANCED_FACE ( 'NONE', ( #22434 ), #45627, .T. ) ;
#11961 = AXIS2_PLACEMENT_3D ( 'NONE', #5531, #102643, #21231 ) ;
#11962 = CARTESIAN_POINT ( 'NONE',  ( 7.188101187500001821, -28.06250000204838813, -2.977408999572650483 ) ) ;
#11963 = DIRECTION ( 'NONE',  ( 0.000000000000000000, -1.000000000000000000, 0.000000000000000000 ) ) ;
#11964 = DIRECTION ( 'NONE',  ( -1.000000000000000000, -0.000000000000000000, -0.000000000000000000 ) ) ;
#11965 = CIRCLE ( 'NONE', #94693, 7.000000000000000000 ) ;
#11966 = CARTESIAN_POINT ( 'NONE',  ( 7.360624614910192598, -5.000000000000000000, -94.61012438777778755 ) ) ;
#11967 = ITEM_DEFINED_TRANSFORMATION ( 'NONE', 'NONE', #42070,  #10728 ) ;
#11968 = ORIENTED_EDGE ( 'NONE', *, *, #79110, .T. ) ;
#11969 = CARTESIAN_POINT ( 'NONE',  ( 38.63430842791552777, 485.8001267274092925, -4.834053598481960812 ) ) ;
#11970 = EDGE_CURVE ( 'NONE', #52425, #48048, #10461, .T. ) ;
#11971 = DIRECTION ( 'NONE',  ( 0.000000000000000000, -1.000000000000000000, 0.000000000000000000 ) ) ;
#11972 = CARTESIAN_POINT ( 'NONE',  ( -8.308397487231465206, 32.82220968432677211, -5.000000000000000000 ) ) ;
#11973 = CARTESIAN_POINT ( 'NONE',  ( -6.931554132363010545, -3.000000000000119904, -71.13906995426670221 ) ) ;
#11974 = ORIENTED_EDGE ( 'NONE', *, *, #41169, .T. ) ;
#11975 = FACE_OUTER_BOUND ( 'NONE', #20438, .T. ) ;
#11976 = CARTESIAN_POINT ( 'NONE',  ( -33.68177706158874685, 464.5004658938952389, 17.05886715805492315 ) ) ;
#11977 = VERTEX_POINT ( 'NONE', #20336 ) ;
#11978 = COLOUR_RGB ( '', 0.08235294, 0.09019608, 0.10196078) ;
#11979 = CARTESIAN_POINT ( 'NONE',  ( -28.18087625354337789, 34.32284550959429481, 8.149263751191908156 ) ) ;
#11980 = CARTESIAN_POINT ( 'NONE',  ( -8.000000000000000000, -22.53125000409677625, -3.313708498984762496 ) ) ;
#11981 = CARTESIAN_POINT ( 'NONE',  ( 9.253583916535172094, 103.7019609199496557, 3.792462592445557945 ) ) ;
#11982 = CARTESIAN_POINT ( 'NONE',  ( -17.07643158642811798, 37.03581886162301373, 21.84712036628276977 ) ) ;
#11983 = CARTESIAN_POINT ( 'NONE',  ( -94.11619913633441570, -60.00000000000000711, 202.5510252723167355 ) ) ;
#11984 = CARTESIAN_POINT ( 'NONE',  ( 17.50000000000093792, 49.99999999999815259, 59.71562975593438694 ) ) ;
#11985 = AXIS2_PLACEMENT_3D ( 'NONE', #52795, #104527, #45256 ) ;
#11986 = DIRECTION ( 'NONE',  ( -0.000000000000000000, -1.000000000000000000, -0.000000000000000000 ) ) ;
#11987 = CARTESIAN_POINT ( 'NONE',  ( 6.133828225839772941, 53.39918049015730617, -8.207320443802755605 ) ) ;
#11988 = DIRECTION ( 'NONE',  ( -1.000000000000000000, -1.224606353822377258E-16, -0.000000000000000000 ) ) ;
#11989 = CARTESIAN_POINT ( 'NONE',  ( -86.38951205727846627, -17.91597735529700586, 174.1201453181821250 ) ) ;
#11990 = CARTESIAN_POINT ( 'NONE',  ( 35.27776333575812373, 42.56632766162715598, -62.00109374954521257 ) ) ;
#11991 = ORIENTED_EDGE ( 'NONE', *, *, #67566, .F. ) ;
#11992 = CARTESIAN_POINT ( 'NONE',  ( -10.28624191511830155, 45.38549880562041494, -15.40779740156157196 ) ) ;
#11993 = CARTESIAN_POINT ( 'NONE',  ( 3.564365538402894273, -1.135065884989783669, 104.5953911288830085 ) ) ;
#11994 = CARTESIAN_POINT ( 'NONE',  ( -85.05563323462654068, -52.70063638665980932, 5.797456579206149208 ) ) ;
#11995 = VECTOR ( 'NONE', #105669, 1000.000000000000000 ) ;
#11996 = CARTESIAN_POINT ( 'NONE',  ( 7.347880794884118356E-15, 49.50000000000000000, -60.00000000000000000 ) ) ;
#11997 = CARTESIAN_POINT ( 'NONE',  ( 89.06666666666666288, 1.023464760207051730E-14, 0.000000000000000000 ) ) ;
#11998 = CARTESIAN_POINT ( 'NONE',  ( 7.849089830976629933, 70.34685271985473776, -5.000000000009827694 ) ) ;
#11999 = CARTESIAN_POINT ( 'NONE',  ( 0.000000000000000000, 0.000000000000000000, 0.000000000000000000 ) ) ;
#12000 = CARTESIAN_POINT ( 'NONE',  ( 29.83308852626540641, 42.00000000008230927, -51.76085035116526711 ) ) ;
#12001 = CARTESIAN_POINT ( 'NONE',  ( 63.58274112560721392, -14.21045842199431242, 93.96243211080884805 ) ) ;
#12002 = AXIS2_PLACEMENT_3D ( 'NONE', #85078, #19337, #11162 ) ;
#12003 = EDGE_CURVE ( 'NONE', #82223, #17102, #70755, .T. ) ;
#12004 = CARTESIAN_POINT ( 'NONE',  ( -87.60281504538382080, -14.21045842199439946, -3.799590761493521374 ) ) ;
#12005 = CARTESIAN_POINT ( 'NONE',  ( -64.92204483014883465, -36.00903953999379326, 84.15884882200457184 ) ) ;
#12006 = ORIENTED_EDGE ( 'NONE', *, *, #77250, .T. ) ;
#12007 = CARTESIAN_POINT ( 'NONE',  ( 83.30384756245543088, -14.21045842199437992, 194.5080389997825137 ) ) ;
#12008 = CARTESIAN_POINT ( 'NONE',  ( -55.03804888984217314, 40.83927881983959907, 34.70779749804891168 ) ) ;
#12009 = CARTESIAN_POINT ( 'NONE',  ( 75.77503827602937747, -57.67118947225861803, -32.31848336751978934 ) ) ;
#12010 = ORIENTED_EDGE ( 'NONE', *, *, #39557, .T. ) ;
#12011 = CARTESIAN_POINT ( 'NONE',  ( 13.83893552277105776, -57.46712370362125455, 29.12875707416400317 ) ) ;
#12012 = CARTESIAN_POINT ( 'NONE',  ( -2.977408999572654480, -26.00000000204839168, 7.188101187499999156 ) ) ;
#12013 = MECHANICAL_DESIGN_GEOMETRIC_PRESENTATION_REPRESENTATION (  '', ( #80921 ), #56817 ) ;
#12014 = CARTESIAN_POINT ( 'NONE',  ( -5.910690929868578358, -6.135040939068072241, -1.065041252563909913 ) ) ;
#12015 = ORIENTED_EDGE ( 'NONE', *, *, #44309, .T. ) ;
#12016 = DIRECTION ( 'NONE',  ( -0.000000000000000000, -0.000000000000000000, -1.000000000000000000 ) ) ;
#12017 = ORIENTED_EDGE ( 'NONE', *, *, #38944, .F. ) ;
#12018 = FACE_OUTER_BOUND ( 'NONE', #31574, .T. ) ;
#12019 = FILL_AREA_STYLE_COLOUR ( '', #638 ) ;
#12020 = CARTESIAN_POINT ( 'NONE',  ( -36.11448103554893407, -60.00000000000002132, -40.17722562108524187 ) ) ;
#12021 = DIRECTION ( 'NONE',  ( 0.000000000000000000, -1.000000000000000000, 0.000000000000000000 ) ) ;
#12022 = CARTESIAN_POINT ( 'NONE',  ( 7.188101187500000044, -31.53125000204838457, 0.000000000000000000 ) ) ;
#12023 = CARTESIAN_POINT ( 'NONE',  ( -49.19536753090093129, 12.91488588853528618, 16.05939653828475144 ) ) ;
#12024 = CARTESIAN_POINT ( 'NONE',  ( 11.17734400176826348, -4.285714285714295357, 22.67073868809949033 ) ) ;
#12025 = AXIS2_PLACEMENT_3D ( 'NONE', #81269, #47315, #71069 ) ;
#12026 = CARTESIAN_POINT ( 'NONE',  ( 9.596002107491598210, 50.00000000000000000, -77.62543935901993564 ) ) ;
#12027 = EDGE_CURVE ( 'NONE', #26488, #33657, #77320, .T. ) ;
#12028 = ADVANCED_FACE ( 'NONE', ( #103325 ), #62346, .T. ) ;
#12029 = CARTESIAN_POINT ( 'NONE',  ( -7.743982712349853692, 108.4621301476073683, 2.020119794285910153 ) ) ;
#12030 = LINE ( 'NONE', #102648, #73676 ) ;
#12031 = B_SPLINE_CURVE_WITH_KNOTS ( 'NONE', 3,
 ( #68573, #59958, #18434, #52904 ),
 .UNSPECIFIED., .F., .F.,
 ( 4, 4 ),
 ( 4.596659206114855704E-17, 0.001829834443479903209 ),
 .UNSPECIFIED. ) ;
#12032 = AXIS2_PLACEMENT_3D ( 'NONE', #5595, #39039, #38518 ) ;
#12033 = ORIENTED_EDGE ( 'NONE', *, *, #4591, .T. ) ;
#12034 = FILL_AREA_STYLE ('',( #68155 ) ) ;
#12036 = CARTESIAN_POINT ( 'NONE',  ( 32.00609611073077332, -18.67737511809503204, 30.02820132365625483 ) ) ;
#12035 = CARTESIAN_POINT ( 'NONE',  ( -3.707709148200944327, -48.90047616793697927, 104.5934084724859332 ) ) ;
#12037 = CARTESIAN_POINT ( 'NONE',  ( 25.22241582816893413, -4.285714285714286476, 3.301606509414615420 ) ) ;
#12038 = ORIENTED_EDGE ( 'NONE', *, *, #24958, .F. ) ;
#12039 = CARTESIAN_POINT ( 'NONE',  ( -22.37419622807756525, 26.07634736961676580, -31.02968219912407122 ) ) ;
#12040 = CARTESIAN_POINT ( 'NONE',  ( -33.63427961064055438, 325.9154870834976236, -4.827994974213513757 ) ) ;
#12041 = DIRECTION ( 'NONE',  ( 0.000000000000000000, 1.000000000000000000, 0.000000000000000000 ) ) ;
#12042 = CARTESIAN_POINT ( 'NONE',  ( -43.58530483650574183, 484.9293427334362718, 0.7222135195706615995 ) ) ;
#12043 = DIRECTION ( 'NONE',  ( 0.000000000000000000, -1.877893248421449282E-16, 1.000000000000000000 ) ) ;
#12044 = DIRECTION ( 'NONE',  ( 0.000000000000000000, 8.673617379884033500E-16, 1.000000000000000000 ) ) ;
#12045 = CARTESIAN_POINT ( 'NONE',  ( -35.35823899438766915, 463.7178658455626419, 19.28807933141518305 ) ) ;
#12046 = ORIENTED_EDGE ( 'NONE', *, *, #84386, .F. ) ;
#12047 = EDGE_CURVE ( 'NONE', #54691, #22572, #4084, .T. ) ;
#12048 = AXIS2_PLACEMENT_3D ( 'NONE', #16375, #81620, #89752 ) ;
#12049 = CARTESIAN_POINT ( 'NONE',  ( 92.31046174747429234, -59.99999999999999289, 1.374785491484104005 ) ) ;
#12050 = LINE ( 'NONE', #93524, #37837 ) ;
#12051 = FILL_AREA_STYLE_COLOUR ( '', #60041 ) ;
#12052 = CARTESIAN_POINT ( 'NONE',  ( 33.70841932975968547, 485.0774894644218875, 1.934193826885754364 ) ) ;
#12053 = ADVANCED_FACE ( 'NONE', ( #8324 ), #67303, .F. ) ;
#12054 = CARTESIAN_POINT ( 'NONE',  ( -6.592078127955123712, 40.00000000008959944, -71.20206365128680659 ) ) ;
#12055 = CARTESIAN_POINT ( 'NONE',  ( -12.59046650546478929, 9.287358138947649167, -9.291413486181960835 ) ) ;
#12056 = EDGE_LOOP ( 'NONE', ( #13839, #104149, #99801, #24516, #13960, #69049 ) ) ;
#12057 = CARTESIAN_POINT ( 'NONE',  ( -99.88428596410730620, -29.99999999998460609, 199.1606248856587058 ) ) ;
#12058 = ORIENTED_EDGE ( 'NONE', *, *, #74691, .F. ) ;
#12059 = CARTESIAN_POINT ( 'NONE',  ( -9.521849859704259345, -56.44524181890594150, 23.94093251888962470 ) ) ;
#12060 = CARTESIAN_POINT ( 'NONE',  ( -6.158268339717665185E-14, -15.58845726811991739, -11.79422863405993382 ) ) ;
#12061 = CARTESIAN_POINT ( 'NONE',  ( 0.000000000000000000, 0.000000000000000000, 0.000000000000000000 ) ) ;
#12062 = CARTESIAN_POINT ( 'NONE',  ( 14.86018380392216542, 23.02630934695024578, 1.319261379110572285 ) ) ;
#12063 = CARTESIAN_POINT ( 'NONE',  ( 84.38025208974687530, -52.74135128307990072, -14.53858364661402547 ) ) ;
#12064 = CARTESIAN_POINT ( 'NONE',  ( -5.082755093536326818, -33.59375000204838813, 5.082755093536325042 ) ) ;
#12065 = VECTOR ( 'NONE', #70873, 1000.000000000000000 ) ;
#12066 = CARTESIAN_POINT ( 'NONE',  ( -17.52852338478520977, 45.00000000000000711, 63.46670662168261856 ) ) ;
#12067 = CARTESIAN_POINT ( 'NONE',  ( -18.09731462108995714, 304.6346555815379133, 8.890781641607192753 ) ) ;
#12068 = VERTEX_POINT ( 'NONE', #7257 ) ;
#12069 = CARTESIAN_POINT ( 'NONE',  ( 32.88185483055566039, 462.9124542777153692, 11.53073017782671528 ) ) ;
#12070 = ORIENTED_EDGE ( 'NONE', *, *, #27329, .F. ) ;
#12071 = CARTESIAN_POINT ( 'NONE',  ( 5.299999999999999822, 0.000000000000000000, 6.499999999999999112 ) ) ;
#12072 =( NAMED_UNIT ( * ) SI_UNIT ( $, .STERADIAN. ) SOLID_ANGLE_UNIT ( ) );
#12074 = EDGE_LOOP ( 'NONE', ( #69020, #2368, #105010, #63830 ) ) ;
#12073 = DIRECTION ( 'NONE',  ( 0.000000000000000000, 0.000000000000000000, 1.000000000000000000 ) ) ;
#12075 = CARTESIAN_POINT ( 'NONE',  ( 80.62408886127033725, -18.68107705517183348, 129.0749382031092409 ) ) ;
#12076 = ORIENTED_EDGE ( 'NONE', *, *, #3073, .T. ) ;
#12077 = CARTESIAN_POINT ( 'NONE',  ( 4.650424936886119021, -47.72263153603915242, 40.40425276227099971 ) ) ;
#12078 = CARTESIAN_POINT ( 'NONE',  ( 2.977408999572650927, -17.37500000204838457, -7.188101187500000933 ) ) ;
#12079 =( BOUNDED_SURFACE ( )  B_SPLINE_SURFACE ( 3, 2, ( 
 ( #76120, #2216, #35166 ),
 ( #68033, #16289, #33043 ),
 ( #73990, #72, #65909 ),
 ( #98789, #3304, #101471 ) ),
 .UNSPECIFIED., .F., .F., .T. ) 
 B_SPLINE_SURFACE_WITH_KNOTS ( ( 4, 4 ),
 ( 3, 3 ),
 ( 0.000000000000000000, 0.001940382064945962715 ),
 ( 0.000000000000000000, 1.000000000000000000 ),
 .UNSPECIFIED. ) 
 GEOMETRIC_REPRESENTATION_ITEM ( )  RATIONAL_B_SPLINE_SURFACE ( (
 ( 1.000000000000000000, 0.8274249441183172404, 1.000000000000000000),
 ( 1.000000000000000000, 0.8191355677488685316, 1.000000000000000000),
 ( 1.000000000000000000, 0.8101072955758994443, 1.000000000000000000),
 ( 1.000000000000000000, 0.8014084173414376400, 1.000000000000000000) ) ) 
 REPRESENTATION_ITEM ( '' )  SURFACE ( )  );
#12080 = CARTESIAN_POINT ( 'NONE',  ( -85.03051761340829273, -57.56200303720294897, 202.2882931814572487 ) ) ;
#12081 = ORIENTED_EDGE ( 'NONE', *, *, #49730, .T. ) ;
#12082 = STYLED_ITEM ( 'NONE', ( #13338 ), #46250 ) ;
#12083 = B_SPLINE_CURVE_WITH_KNOTS ( 'NONE', 3,
 ( #47621, #80523, #82114, #8234, #97767, #6641, #57833, #108, #56776, #98825, #7693, #97244, #56227, #89165, #16325, #90760, #65945, #48680, #48153, #81052, #49756, #7166, #16876, #73487, #32007, #89699, #32547, #81564, #37606, #65419, #4674, #98314, #71913, #34144 ),
 .UNSPECIFIED., .F., .F.,
 ( 4, 2, 2, 2, 2, 2, 2, 2, 2, 2, 2, 2, 2, 2, 2, 2, 4 ),
 ( 3.576224061345498009E-18, 0.0007951492273476420004, 0.001590298454695280314, 0.002385447682042918845, 0.003180596909390557159, 0.003975746136738195040, 0.004770895364085834221, 0.005566044591433472535, 0.006361193818781110849, 0.007156343046128749164, 0.007951492273476386610, 0.008746641500824025792, 0.009541790728171664973, 0.01033693995551930242, 0.01113208918286694160, 0.01192723841021457905, 0.01272238763756221476 ),
 .UNSPECIFIED. ) ;
#12084 = CARTESIAN_POINT ( 'NONE',  ( -4.813555570991615795, -11.79473796517323159, -3.584128953194782419 ) ) ;
#12085 = CIRCLE ( 'NONE', #23273, 5.000000000000001776 ) ;
#12086 = CARTESIAN_POINT ( 'NONE',  ( -9.699121749566360862, 81.82331239724180705, 2.444499528233564423 ) ) ;
#12087 = CARTESIAN_POINT ( 'NONE',  ( -6.891666673413887896E-15, -70.53271932724189242, 13.00000000000000000 ) ) ;
#12088 = CARTESIAN_POINT ( 'NONE',  ( 4.898587196589412829E-16, -18.31250000409676915, -8.000000000000000000 ) ) ;
#12089 = CARTESIAN_POINT ( 'NONE',  ( -48.03847873877180064, -29.24902813972587978, 43.67456182833235090 ) ) ;
#12090 = CARTESIAN_POINT ( 'NONE',  ( 9.168149550321063046, 15.99999999372935022, 3.997425403567909541 ) ) ;
#12091 = DIRECTION ( 'NONE',  ( -0.000000000000000000, -0.000000000000000000, 1.000000000000000000 ) ) ;
#12092 = CARTESIAN_POINT ( 'NONE',  ( -9.537909130738276176, 87.64614830963394354, -3.010726932293856350 ) ) ;
#12093 = CARTESIAN_POINT ( 'NONE',  ( 46.00000000000000000, 437.9690125970931831, 14.09127711025711349 ) ) ;
#12094 = APPLICATION_PROTOCOL_DEFINITION ( 'draft international standard', 'automotive_design', 1998, #12143 ) ;
#12095 = DIRECTION ( 'NONE',  ( -1.000000000000000000, -0.000000000000000000, -0.000000000000000000 ) ) ;
#12096 = ORIENTED_EDGE ( 'NONE', *, *, #5928, .T. ) ;
#12097 = CARTESIAN_POINT ( 'NONE',  ( -6.167494924855482452, -50.03135609564296260, 39.57077639986113837 ) ) ;
#12098 = PRESENTATION_LAYER_ASSIGNMENT (  '', '', ( #39691 ) ) ;
#12099 = CARTESIAN_POINT ( 'NONE',  ( 11.16922809658906424, -4.977367432874250319, -12.57708011016608296 ) ) ;
#12100 = EDGE_CURVE ( 'NONE', #48783, #67806, #9093, .T. ) ;
#12101 = CARTESIAN_POINT ( 'NONE',  ( 0.6243278333291550908, 8.125659060767901565, 51.58699189189907486 ) ) ;
#12102 = CARTESIAN_POINT ( 'NONE',  ( 4.998341000544551882, -17.97620282888080112, -37.93689352612668131 ) ) ;
#12103 = CARTESIAN_POINT ( 'NONE',  ( -62.52821090568615148, -30.00000000000000711, 73.42485873602892354 ) ) ;
#12104 = ADVANCED_FACE ( 'NONE', ( #74115 ), #32096, .F. ) ;
#12105 = DIRECTION ( 'NONE',  ( -1.000000000000000000, 0.000000000000000000, 0.000000000000000000 ) ) ;
#12106 = ORIENTED_EDGE ( 'NONE', *, *, #82464, .T. ) ;
#12107 = CIRCLE ( 'NONE', #86208, 4.000000000000007105 ) ;
#12108 = CARTESIAN_POINT ( 'NONE',  ( -12.71180608306794291, -4.333298119783883351, 12.63015221170769031 ) ) ;
#12109 = CARTESIAN_POINT ( 'NONE',  ( 75.25576489772180366, -57.56749894965461323, 191.3623090674220180 ) ) ;
#12110 = CARTESIAN_POINT ( 'NONE',  ( 6.145467199749146125, 48.00000000000000711, -77.00333157601821199 ) ) ;
#12112 = CARTESIAN_POINT ( 'NONE',  ( 57.89164812746757605, -37.03233184154265700, -34.65406527698851136 ) ) ;
#12111 = AXIS2_PLACEMENT_3D ( 'NONE', #64850, #83158, #24435 ) ;
#12113 = CARTESIAN_POINT ( 'NONE',  ( 9.500000000000000000, -5.000000000000000000, -20.99851272547260095 ) ) ;
#12114 = CARTESIAN_POINT ( 'NONE',  ( 7.996668423981797780, -3.000000000000002665, -91.14546719974913458 ) ) ;
#12115 = CARTESIAN_POINT ( 'NONE',  ( -65.70695785853703796, -59.99999999999998579, 121.1804584992903528 ) ) ;
#12116 = LINE ( 'NONE', #63353, #89903 ) ;
#12117 = PRESENTATION_LAYER_ASSIGNMENT (  '', '', ( #38036 ) ) ;
#12118 = CARTESIAN_POINT ( 'NONE',  ( 55.22048556080756043, 48.00000000000000000, 34.80214219304977519 ) ) ;
#12119 = CARTESIAN_POINT ( 'NONE',  ( -83.91826887416667091, -61.04048265323336153, 192.1982429797399163 ) ) ;
#12120 = ORIENTED_EDGE ( 'NONE', *, *, #4284, .T. ) ;
#12121 = CARTESIAN_POINT ( 'NONE',  ( 30.80294602723973085, 13.24188206181652383, 41.41355684762679346 ) ) ;
#12122 = CARTESIAN_POINT ( 'NONE',  ( -3.070984519260819834, -53.40251359550288157, 32.78485625322804253 ) ) ;
#12123 = CARTESIAN_POINT ( 'NONE',  ( -5.430162889308253860, 41.93410902331645929, -59.17461592276305993 ) ) ;
#12124 = DIRECTION ( 'NONE',  ( 0.5735764363510468256, 0.8191520442889913545, 0.000000000000000000 ) ) ;
#12125 = SURFACE_STYLE_FILL_AREA ( #61232 ) ;
#12126 = ORIENTED_EDGE ( 'NONE', *, *, #87411, .T. ) ;
#12127 = CARTESIAN_POINT ( 'NONE',  ( -36.66634014091943783, 431.6751349732608105, 5.005327391448617824 ) ) ;
#12128 = CARTESIAN_POINT ( 'NONE',  ( 37.83989825151487452, 491.6297408768496666, 12.44743998625079584 ) ) ;
#12129 = DIRECTION ( 'NONE',  ( 2.742080092235280244E-17, 0.000000000000000000, -1.000000000000000000 ) ) ;
#12130 = LINE ( 'NONE', #4586, #31031 ) ;
#12131 = ORIENTED_EDGE ( 'NONE', *, *, #4690, .T. ) ;
#12132 = MECHANICAL_DESIGN_GEOMETRIC_PRESENTATION_REPRESENTATION (  '', ( #22498 ), #93150 ) ;
#12133 = CARTESIAN_POINT ( 'NONE',  ( 23.73873964903627609, 303.5156351045484371, -9.857263350994356799 ) ) ;
#12134 = CARTESIAN_POINT ( 'NONE',  ( 39.24156521425334176, 307.7088117867400001, -7.003459073692002157 ) ) ;
#12135 =( NAMED_UNIT ( * ) SI_UNIT ( $, .STERADIAN. ) SOLID_ANGLE_UNIT ( ) );
#12136 = EDGE_CURVE ( 'NONE', #37787, #102355, #39660, .T. ) ;
#12137 = CARTESIAN_POINT ( 'NONE',  ( 99.89428240326108721, -30.00000000000003908, 96.08155976150675315 ) ) ;
#12138 = CARTESIAN_POINT ( 'NONE',  ( -81.17881172582528393, -39.50116433889217404, 153.9116840188365813 ) ) ;
#12139 = EDGE_LOOP ( 'NONE', ( #49016, #102623, #62677, #70598, #88685 ) ) ;
#12140 = DIRECTION ( 'NONE',  ( -0.8191520442889975717, 0.000000000000000000, -0.5735764363510378328 ) ) ;
#12141 = DIRECTION ( 'NONE',  ( -1.000000000000000000, -1.224606353822377258E-16, -0.000000000000000000 ) ) ;
#12142 = CARTESIAN_POINT ( 'NONE',  ( 26.18764921593997030, -57.67624503786063883, 43.55245106248555231 ) ) ;
#12143 = APPLICATION_CONTEXT ( 'automotive_design' ) ;
#12144 = CARTESIAN_POINT ( 'NONE',  ( 42.49292640382294906, 334.6996552629477151, 7.623548389374787071 ) ) ;
#12145 = DIRECTION ( 'NONE',  ( 0.000000000000000000, 0.000000000000000000, 1.000000000000000000 ) ) ;
#12146 = ORIENTED_EDGE ( 'NONE', *, *, #74226, .T. ) ;
#12147 = FACE_OUTER_BOUND ( 'NONE', #69492, .T. ) ;
#12148 = CARTESIAN_POINT ( 'NONE',  ( 31.87868955222396750, 439.4198093404291967, 23.54367745888691132 ) ) ;
#12149 = CARTESIAN_POINT ( 'NONE',  ( 5.082755093536324154, -26.84375000204838813, 5.082755093536326818 ) ) ;
#12150 = ORIENTED_EDGE ( 'NONE', *, *, #12358, .F. ) ;
#12151 = DIRECTION ( 'NONE',  ( 0.000000000000000000, 0.000000000000000000, 1.000000000000000000 ) ) ;
#12152 = DIRECTION ( 'NONE',  ( 1.000000000000000000, -8.034710196240773658E-11, 8.034710196240799507E-11 ) ) ;
#12153 = CARTESIAN_POINT ( 'NONE',  ( 6.458627575847655677, 41.53001914941116723, -70.63868815791025213 ) ) ;
#12154 = EDGE_CURVE ( 'NONE', #24916, #70311, #69077, .T. ) ;
#12155 = CARTESIAN_POINT ( 'NONE',  ( 1.369801731157060329E-15, 34.00000000000000711, 11.18527996897366528 ) ) ;
#12156 = CARTESIAN_POINT ( 'NONE',  ( 12.49986889690059222, -3.000000000000002665, -76.70852482682694529 ) ) ;
#12157 = AXIS2_PLACEMENT_3D ( 'NONE', #45491, #33816, #4483 ) ;
#12158 = CARTESIAN_POINT ( 'NONE',  ( 32.99999999999995026, 484.0323588803976804, 1.017072797581088262 ) ) ;
#12159 = ORIENTED_EDGE ( 'NONE', *, *, #85079, .F. ) ;
#12160 = CARTESIAN_POINT ( 'NONE',  ( 63.27042206663746526, -60.00000000000000000, -34.75888330929602432 ) ) ;
#12162 = CARTESIAN_POINT ( 'NONE',  ( 27.33918801737314297, -25.57593558123391375, 29.89066338960705593 ) ) ;
#12161 = CARTESIAN_POINT ( 'NONE',  ( -71.37516729659446924, -14.21045842199439946, 121.5232625957608974 ) ) ;
#12163 = CARTESIAN_POINT ( 'NONE',  ( 1.458152649223318708E-14, 7.666536031838887766, -59.53359981990485750 ) ) ;
#12164 = CARTESIAN_POINT ( 'NONE',  ( -35.84365847796291860, -39.50733013384240877, 35.79938607260854155 ) ) ;
#12165 = ORIENTED_EDGE ( 'NONE', *, *, #64885, .F. ) ;
#12166 = CIRCLE ( 'NONE', #70924, 0.5000000000000004441 ) ;
#12167 = CARTESIAN_POINT ( 'NONE',  ( 34.87679907359152054, 462.5881041932447033, 5.015251600533665588 ) ) ;
#12168 = CARTESIAN_POINT ( 'NONE',  ( -5.833333333333327708, -46.27176886455112026, 103.8776713793258324 ) ) ;
#12169 = CARTESIAN_POINT ( 'NONE',  ( -13.38090213880806978, -54.26192864245579273, 31.11721482942555639 ) ) ;
#12170 = CARTESIAN_POINT ( 'NONE',  ( 23.15769230769230802, 1.411358822780289120E-15, 0.000000000000000000 ) ) ;
#12171 = CARTESIAN_POINT ( 'NONE',  ( 6.928203230275506108, -64.73069070304460126, -4.000000000000002665 ) ) ;
#12172 = DIRECTION ( 'NONE',  ( -1.000000000000000000, -1.224606353822377258E-16, -0.000000000000000000 ) ) ;
#12173 = VERTEX_POINT ( 'NONE', #82211 ) ;
#12174 = CARTESIAN_POINT ( 'NONE',  ( -76.00050994787578418, -38.37788238259345519, 178.3583240899461941 ) ) ;
#12175 = EDGE_CURVE ( 'NONE', #64826, #5970, #67119, .T. ) ;
#12176 = CARTESIAN_POINT ( 'NONE',  ( 89.04598776754650657, -29.99999999999999289, 83.36196907162633352 ) ) ;
#12177 = DIRECTION ( 'NONE',  ( 0.000000000000000000, -1.000000000000000000, 0.000000000000000000 ) ) ;
#12179 = CARTESIAN_POINT ( 'NONE',  ( -4.589925132946516939, -83.93473983707484365, 3.864926970398267603 ) ) ;
#12178 = AXIS2_PLACEMENT_3D ( 'NONE', #49321, #82229, #106503 ) ;
#12180 = CARTESIAN_POINT ( 'NONE',  ( 80.71453622594903266, -30.00000000000000711, -12.60762180172875624 ) ) ;
#12181 = CIRCLE ( 'NONE', #26024, 4.000000000000007105 ) ;
#12182 = EDGE_CURVE ( 'NONE', #95473, #24767, #79369, .T. ) ;
#12183 = CARTESIAN_POINT ( 'NONE',  ( -7.500000000000000888, -4.999999999999997335, -14.04024970282782547 ) ) ;
#12184 = EDGE_LOOP ( 'NONE', ( #82754, #99960 ) ) ;
#12185 = MECHANICAL_DESIGN_GEOMETRIC_PRESENTATION_REPRESENTATION (  '', ( #13866 ), #17371 ) ;
#12186 = ORIENTED_EDGE ( 'NONE', *, *, #53378, .F. ) ;
#12187 = ORIENTED_EDGE ( 'NONE', *, *, #67408, .T. ) ;
#12188 = DIRECTION ( 'NONE',  ( 0.000000000000000000, -0.000000000000000000, 1.000000000000000000 ) ) ;
#12189 = CARTESIAN_POINT ( 'NONE',  ( 46.55033305608798599, 41.07609238384448247, -46.50387254352151700 ) ) ;
#12190 = CARTESIAN_POINT ( 'NONE',  ( 0.000000000000000000, 0.000000000000000000, 61.50000000000000000 ) ) ;
#12191 = CARTESIAN_POINT ( 'NONE',  ( -45.50351044820315138, 397.4513779159573801, 8.242489876862624243 ) ) ;
#12192 = CARTESIAN_POINT ( 'NONE',  ( -1.141441439215143294, -70.08722353079659229, 13.04506332611827801 ) ) ;
#12193 = CARTESIAN_POINT ( 'NONE',  ( -7.551437640244095917, -88.00872462522907824, -2.648272645923386737 ) ) ;
#12194 =( LENGTH_UNIT ( ) NAMED_UNIT ( * ) SI_UNIT ( .MILLI., .METRE. ) );
#12195 = VERTEX_POINT ( 'NONE', #47189 ) ;
#12196 = CARTESIAN_POINT ( 'NONE',  ( -9.999999999999992895, 48.00000000000000000, -86.30899693747680601 ) ) ;
#12197 = CIRCLE ( 'NONE', #7030, 2.999999999999984457 ) ;
#12198 = ORIENTED_EDGE ( 'NONE', *, *, #69028, .F. ) ;
#12199 = CARTESIAN_POINT ( 'NONE',  ( -5.858824175751781382, -61.21420939127642669, -1.318356988357135773 ) ) ;
#12200 = CARTESIAN_POINT ( 'NONE',  ( -7.000000000000000000, 8.572527594031473190E-16, -2.575493252495433261 ) ) ;
#12201 = CARTESIAN_POINT ( 'NONE',  ( 58.67238219402268840, 6.975173280561618775E-15, 0.000000000000000000 ) ) ;
#12202 = EDGE_CURVE ( 'NONE', #106205, #54493, #81146, .T. ) ;
#12203 = CARTESIAN_POINT ( 'NONE',  ( 24.56203592210657760, 295.5996828079419743, 10.09760663225323007 ) ) ;
#12204 = CARTESIAN_POINT ( 'NONE',  ( 0.000000000000000000, 36.79151656018385097, -22.55262289886175964 ) ) ;
#12206 = CARTESIAN_POINT ( 'NONE',  ( 64.78375808736633701, -22.10194954420784086, 76.63010471250390765 ) ) ;
#12205 = PRODUCT ( '12. Movable Jaw', '12. Movable Jaw', '', ( #31506 ) ) ;
#12207 = ORIENTED_EDGE ( 'NONE', *, *, #41966, .T. ) ;
#12208 = CARTESIAN_POINT ( 'NONE',  ( 28.77725283099220732, 13.66028544304340464, -39.99080474963867715 ) ) ;
#12209 = CARTESIAN_POINT ( 'NONE',  ( 29.83349330513380693, 1.593028355512270962E-15, 0.000000000000000000 ) ) ;
#12210 = DIRECTION ( 'NONE',  ( -1.000000000000000000, -1.224606353822377258E-16, -0.000000000000000000 ) ) ;
#12211 = EDGE_LOOP ( 'NONE', ( #100735, #55417, #103120, #53084, #23845, #69797 ) ) ;
#12212 =( NAMED_UNIT ( * ) PLANE_ANGLE_UNIT ( ) SI_UNIT ( $, .RADIAN. ) );
#12213 = DIRECTION ( 'NONE',  ( -1.000000000000000000, -1.224606353822377258E-16, -0.000000000000000000 ) ) ;
#12214 = DIRECTION ( 'NONE',  ( 0.000000000000000000, 0.000000000000000000, 1.000000000000000000 ) ) ;
#12215 = CONICAL_SURFACE ( 'NONE', #20912, 7.000000000000000000, 0.9599310885968753704 ) ;
#12216 = DIRECTION ( 'NONE',  ( 0.000000000000000000, 0.000000000000000000, -1.000000000000000000 ) ) ;
#12217 = TOROIDAL_SURFACE ( 'NONE', #55243, 4.400000000000000355, 0.4000000000000000222 ) ;
#12218 = CARTESIAN_POINT ( 'NONE',  ( -20.05074616892822448, 67.05096163904791240, 10.02537308446411402 ) ) ;
#12219 = CARTESIAN_POINT ( 'NONE',  ( 9.999999999999998224, 15.00000000000000000, -1.734723475976806897E-15 ) ) ;
#12220 = CARTESIAN_POINT ( 'NONE',  ( 86.70382925515318107, -35.44956032792972422, 187.4678705349916470 ) ) ;
#12221 = CARTESIAN_POINT ( 'NONE',  ( -5.197438949454540769, 4.242550593911340151, -24.96153357884654866 ) ) ;
#12222 = CARTESIAN_POINT ( 'NONE',  ( -9.229740628973800654, 139.8534222827340159, 4.999999999999998224 ) ) ;
#12223 = VERTEX_POINT ( 'NONE', #31579 ) ;
#12224 = CARTESIAN_POINT ( 'NONE',  ( 75.12731958518588726, -57.67118848584987489, -32.59161320420232499 ) ) ;
#12225 =( NAMED_UNIT ( * ) PLANE_ANGLE_UNIT ( ) SI_UNIT ( $, .RADIAN. ) );
#12226 = CARTESIAN_POINT ( 'NONE',  ( -6.806778129255477872, 41.25019534346876782, -70.74215739106598733 ) ) ;
#12227 = CARTESIAN_POINT ( 'NONE',  ( 33.89801561537790064, 435.9363418380468715, 7.957186453526370329 ) ) ;
#12228 = CARTESIAN_POINT ( 'NONE',  ( -83.17155174494244818, -30.00000000000000000, 44.27485665655420632 ) ) ;
#12229 = EDGE_CURVE ( 'NONE', #89525, #33789, #1009, .T. ) ;
#12230 = B_SPLINE_CURVE_WITH_KNOTS ( 'NONE', 3,
 ( #67866, #16655, #33392, #18277, #66264, #99152, #10152, #33938, #76474, #34479, #100224, #43066, #424, #84049, #1511, #25310, #49545, #99695, #67346, #51133, #98622, #59255 ),
 .UNSPECIFIED., .F., .F.,
 ( 4, 2, 2, 2, 2, 2, 2, 2, 2, 2, 4 ),
 ( 0.002801246442724396931, 0.003304316507003848043, 0.003555851539143575768, 0.003807386571283303059, 0.004310456635562755039, 0.004561991667702480595, 0.004813526699842207018, 0.005316596764121661600, 0.005819666828401116182, 0.006322736892680569896, 0.006825806956960025346 ),
 .UNSPECIFIED. ) ;
#12231 = DIRECTION ( 'NONE',  ( -1.000000000000000000, -0.000000000000000000, -0.000000000000000000 ) ) ;
#12232 = CARTESIAN_POINT ( 'NONE',  ( 0.002498436923358977966, -57.67120202537410734, 41.61186700447464659 ) ) ;
#12233 = EDGE_CURVE ( 'NONE', #26186, #99054, #97869, .T. ) ;
#12235 = CARTESIAN_POINT ( 'NONE',  ( 3.493042281569127550, 304.8518027749427119, -10.00000000028269120 ) ) ;
#12234 = CARTESIAN_POINT ( 'NONE',  ( 9.958126073916819365, 43.33285415681326924, 15.37489409574949129 ) ) ;
#12236 =( BOUNDED_SURFACE ( )  B_SPLINE_SURFACE ( 3, 2, ( 
 ( #23854, #80446, #98231 ),
 ( #56699, #41596, #74481 ),
 ( #97163, #49135, #15185 ),
 ( #33002, #89622, #15720 ) ),
 .UNSPECIFIED., .F., .F., .F. ) 
 B_SPLINE_SURFACE_WITH_KNOTS ( ( 4, 4 ),
 ( 3, 3 ),
 ( -1.561251128379126385E-17, 0.001949576957921161187 ),
 ( 0.000000000000000000, 1.000000000000000000 ),
 .UNSPECIFIED. ) 
 GEOMETRIC_REPRESENTATION_ITEM ( )  RATIONAL_B_SPLINE_SURFACE ( (
 ( 1.000000000000000000, 0.7964405967476665404, 1.000000000000000000),
 ( 1.000000000000000000, 0.8057025330220294324, 1.000000000000000000),
 ( 1.000000000000000000, 0.8148370924185962538, 1.000000000000000000),
 ( 1.000000000000000000, 0.8238944711860057835, 1.000000000000000000) ) ) 
 REPRESENTATION_ITEM ( '' )  SURFACE ( )  );
#12237 = FACE_OUTER_BOUND ( 'NONE', #10470, .T. ) ;
#12238 = CARTESIAN_POINT ( 'NONE',  ( -17.88715956647400773, 50.00000000000001421, 62.04331920601425310 ) ) ;
#12239 = CARTESIAN_POINT ( 'NONE',  ( -43.03185303983482157, 485.3613526602391062, 6.073233449168601972 ) ) ;
#12240 = CARTESIAN_POINT ( 'NONE',  ( 46.00000000004322942, 486.6678415250559624, 5.056251502143302545 ) ) ;
#12241 = CARTESIAN_POINT ( 'NONE',  ( -0.3425297379985101087, -69.52592981242614201, 12.72818415379369483 ) ) ;
#12242 = CARTESIAN_POINT ( 'NONE',  ( -46.00000000000000000, 500.0000000000002274, 0.000000000000000000 ) ) ;
#12243 = CARTESIAN_POINT ( 'NONE',  ( -87.37974545749381150, -46.42099736837836588, 191.3367129492426102 ) ) ;
#12244 = AXIS2_PLACEMENT_3D ( 'NONE', #64403, #22897, #62811 ) ;
#12245 = AXIS2_PLACEMENT_3D ( 'NONE', #96058, #71234, #104130 ) ;
#12246 = ORIENTED_EDGE ( 'NONE', *, *, #103892, .T. ) ;
#12247 = CARTESIAN_POINT ( 'NONE',  ( 40.38854417759264237, 485.1419806746684458, -4.245955111566214413 ) ) ;
#12248 = CARTESIAN_POINT ( 'NONE',  ( -9.989285784994814676, 108.9734242744570025, 0.5301777604595967475 ) ) ;
#12249 = CARTESIAN_POINT ( 'NONE',  ( -21.04607429833048471, -29.03556388439810121, 29.34454004103736580 ) ) ;
#12250 = VECTOR ( 'NONE', #80506, 1000.000000000000000 ) ;
#12252 = CARTESIAN_POINT ( 'NONE',  ( 0.7782283554130018377, 36.39419318762584510, -29.48168008561355435 ) ) ;
#12251 = DIRECTION ( 'NONE',  ( 1.000000000000000000, 1.224606353822377258E-16, 0.000000000000000000 ) ) ;
#12253 = EDGE_CURVE ( 'NONE', #48472, #12693, #56867, .T. ) ;
#12254 = VERTEX_POINT ( 'NONE', #106483 ) ;
#12255 = COLOUR_RGB ( '', 0.66274510, 0.83137255, 0.94901961) ;
#12256 = ORIENTED_EDGE ( 'NONE', *, *, #91415, .T. ) ;
#12257 = CARTESIAN_POINT ( 'NONE',  ( 27.10511071441197117, -1.200000000000000030E-05, 8.806984339685705265 ) ) ;
#12258 = AXIS2_PLACEMENT_3D ( 'NONE', #9081, #42519, #43589 ) ;
#12259 = AXIS2_PLACEMENT_3D ( 'NONE', #18220, #17149, #25813 ) ;
#12260 = DIRECTION ( 'NONE',  ( 1.000000000000000000, 1.224606353822377258E-16, 0.000000000000000000 ) ) ;
#12261 = EDGE_CURVE ( 'NONE', #69966, #45998, #115, .T. ) ;
#12262 = CARTESIAN_POINT ( 'NONE',  ( -5.656854249492381470, -23.75000000409677270, 5.656854249492379694 ) ) ;
#12263 = ORIENTED_EDGE ( 'NONE', *, *, #77116, .F. ) ;
#12264 = FILL_AREA_STYLE_COLOUR ( '', #99699 ) ;
#12265 = CARTESIAN_POINT ( 'NONE',  ( 3.122376895888458570, 50.00000000000000711, -73.30448186995486992 ) ) ;
#12266 = CARTESIAN_POINT ( 'NONE',  ( 102.3885618088003042, -52.72063632800296773, 191.3672504949884114 ) ) ;
#12268 = DIRECTION ( 'NONE',  ( -0.2039034312715000408, 0.2189633091458940695, 0.9541899496240715539 ) ) ;
#12267 = CARTESIAN_POINT ( 'NONE',  ( -13.50000000000000178, 6.533945317241069084, -0.8419589098297682872 ) ) ;
#12269 = ORIENTED_EDGE ( 'NONE', *, *, #105637, .F. ) ;
#12270 = ORIENTED_EDGE ( 'NONE', *, *, #42121, .T. ) ;
#12271 = ORIENTED_EDGE ( 'NONE', *, *, #72420, .T. ) ;
#12272 = CARTESIAN_POINT ( 'NONE',  ( 22.83110074884478990, 304.5052821938692773, 10.07833457152883128 ) ) ;
#12273 = DIRECTION ( 'NONE',  ( -1.000000000000000000, 0.000000000000000000, 0.000000000000000000 ) ) ;
#12274 = DIRECTION ( 'NONE',  ( -1.000000000000000000, -1.224606353822377258E-16, -0.000000000000000000 ) ) ;
#12276 = EDGE_CURVE ( 'NONE', #35868, #106280, #8771, .T. ) ;
#12275 = ORIENTED_EDGE ( 'NONE', *, *, #73735, .F. ) ;
#12277 = DIRECTION ( 'NONE',  ( 0.000000000000000000, 1.000000000000000000, 0.000000000000000000 ) ) ;
#12278 = CARTESIAN_POINT ( 'NONE',  ( -8.425615494702062946, 6.357254220375858189, -3.971849628822432088 ) ) ;
#12280 = CARTESIAN_POINT ( 'NONE',  ( -95.07610051239151971, -60.00000000000000000, -4.532845324902508466 ) ) ;
#12279 = AXIS2_PLACEMENT_3D ( 'NONE', #73128, #82303, #815 ) ;
#12281 = CARTESIAN_POINT ( 'NONE',  ( 7.986711519608433285, -68.97361903623433932, -0.5300249774147592907 ) ) ;
#12282 = CARTESIAN_POINT ( 'NONE',  ( 31.95254591819974976, -59.99999999999998579, 44.12862274816207275 ) ) ;
#12283 = DIRECTION ( 'NONE',  ( -1.000000000000000000, -1.224606353822377258E-16, -0.000000000000000000 ) ) ;
#12284 = CARTESIAN_POINT ( 'NONE',  ( -5.402794924240495789, 41.73472301521996997, -58.79867575249376443 ) ) ;
#12286 = CARTESIAN_POINT ( 'NONE',  ( 5.156537703247399129, -56.87775452844108770, 33.35875848516817399 ) ) ;
#12285 = CARTESIAN_POINT ( 'NONE',  ( -105.4253011914250067, -14.21045842199428222, 149.5333493894512458 ) ) ;
#12287 = SURFACE_STYLE_USAGE ( .BOTH. , #21482 ) ;
#12288 = CARTESIAN_POINT ( 'NONE',  ( -47.61298378469552972, -53.36243106413825643, 51.28367574756582314 ) ) ;
#12289 = AXIS2_PLACEMENT_3D ( 'NONE', #97268, #9703, #6666 ) ;
#12290 = ORIENTED_EDGE ( 'NONE', *, *, #46788, .F. ) ;
#12291 = CARTESIAN_POINT ( 'NONE',  ( 4.408728476930471644E-15, 0.1588408748199928722, -15.14825148316532832 ) ) ;
#12292 = EDGE_LOOP ( 'NONE', ( #81766, #101694, #74252, #72190 ) ) ;
#12293 = CARTESIAN_POINT ( 'NONE',  ( 41.16726895037042055, 460.1166845890176660, 2.127318685287079347 ) ) ;
#12294 =( NAMED_UNIT ( * ) SI_UNIT ( $, .STERADIAN. ) SOLID_ANGLE_UNIT ( ) );
#12295 = DIRECTION ( 'NONE',  ( -1.000000000000000000, 0.000000000000000000, 0.000000000000000000 ) ) ;
#12296 = ORIENTED_EDGE ( 'NONE', *, *, #52759, .T. ) ;
#12297 = CARTESIAN_POINT ( 'NONE',  ( -9.389245980427300964, -2.447416405268211914, 14.81682632889905626 ) ) ;
#12298 = ORIENTED_EDGE ( 'NONE', *, *, #18103, .F. ) ;
#12299 = CARTESIAN_POINT ( 'NONE',  ( 76.53963492301289762, -29.99999999999329603, -26.83307303577876013 ) ) ;
#12300 =( NAMED_UNIT ( * ) SI_UNIT ( $, .STERADIAN. ) SOLID_ANGLE_UNIT ( ) );
#12301 = FACE_OUTER_BOUND ( 'NONE', #79769, .T. ) ;
#12302 = CARTESIAN_POINT ( 'NONE',  ( 55.00000000000000000, 0.000000000000000000, 0.000000000000000000 ) ) ;
#12303 = CARTESIAN_POINT ( 'NONE',  ( 36.40416150955762475, 42.00000000000001421, -47.37019975555940476 ) ) ;
#12304 = CARTESIAN_POINT ( 'NONE',  ( 98.56603916130582377, -30.00000000000000355, 189.7319824347792405 ) ) ;
#12305 = ADVANCED_FACE ( 'NONE', ( #88729 ), #55266, .T. ) ;
#12306 = DIRECTION ( 'NONE',  ( 0.000000000000000000, 1.000000000000000000, 0.000000000000000000 ) ) ;
#12307 = EDGE_LOOP ( 'NONE', ( #55933, #69282, #62589, #105063, #58848, #86126, #88679 ) ) ;
#12308 = CIRCLE ( 'NONE', #75983, 5.000000000000000888 ) ;
#12309 = VERTEX_POINT ( 'NONE', #105440 ) ;
#12310 = ORIENTED_EDGE ( 'NONE', *, *, #64504, .T. ) ;
#12311 = CARTESIAN_POINT ( 'NONE',  ( 54.48416669372233656, -56.84658666858351950, 66.24332653280961836 ) ) ;
#12312 = FACE_OUTER_BOUND ( 'NONE', #72095, .T. ) ;
#12313 = CARTESIAN_POINT ( 'NONE',  ( -46.00000000000000711, 461.5064854449057066, 9.507889913832133999 ) ) ;
#12314 = EDGE_CURVE ( 'NONE', #102890, #19599, #74017, .T. ) ;
#12315 = ORIENTED_EDGE ( 'NONE', *, *, #103971, .F. ) ;
#12316 = CARTESIAN_POINT ( 'NONE',  ( -88.01924983139112157, -38.37074707933226847, -19.54877242889350342 ) ) ;
#12317 = ORIENTED_EDGE ( 'NONE', *, *, #32550, .F. ) ;
#12318 = CARTESIAN_POINT ( 'NONE',  ( 44.48436518344927038, 465.3427600001839437, 9.644189083063393397 ) ) ;
#12319 = CARTESIAN_POINT ( 'NONE',  ( 101.3911668549956033, -38.45380319144855008, 199.9736433382965402 ) ) ;
#12320 = CARTESIAN_POINT ( 'NONE',  ( 11.50368691626706052, 15.08202484978332336, 9.785078861151950136 ) ) ;
#12321 = CARTESIAN_POINT ( 'NONE',  ( 84.89893217423146154, -52.70949330645067477, 12.33567577723670006 ) ) ;
#12322 = CARTESIAN_POINT ( 'NONE',  ( 42.68463871003257282, 439.3239431036145675, 17.84154235464308158 ) ) ;
#12323 = AXIS2_PLACEMENT_3D ( 'NONE', #32975, #49110, #8665 ) ;
#12325 = EDGE_CURVE ( 'NONE', #18508, #101939, #17224, .T. ) ;
#12324 = AXIS2_PLACEMENT_3D ( 'NONE', #79733, #22602, #14448 ) ;
#12326 = CARTESIAN_POINT ( 'NONE',  ( -43.77364510075356918, 434.9303853139112448, 13.50475697611079973 ) ) ;
#12327 = COLOUR_RGB ( '', 0.66274510, 0.83137255, 0.94901961) ;
#12328 = CARTESIAN_POINT ( 'NONE',  ( -3.857142857142845660, -48.79941684889506348, 103.1763305333244176 ) ) ;
#12329 = ORIENTED_EDGE ( 'NONE', *, *, #81028, .T. ) ;
#12330 = CARTESIAN_POINT ( 'NONE',  ( -10.00000000000000178, 15.00000000000000000, 1.734723475976807489E-15 ) ) ;
#12331 = CARTESIAN_POINT ( 'NONE',  ( 6.928203230275510549, 85.00000000000000000, -4.000000000000000000 ) ) ;
#12332 = CARTESIAN_POINT ( 'NONE',  ( -3.346159239404074892, 120.6791528222331777, 5.000000000000000888 ) ) ;
#12333 = ORIENTED_EDGE ( 'NONE', *, *, #17161, .T. ) ;
#12334 = CARTESIAN_POINT ( 'NONE',  ( 0.000000000000000000, 6.928203230275505220, 4.000000000000006217 ) ) ;
#12335 = CARTESIAN_POINT ( 'NONE',  ( -40.26971465411892837, 320.4908973235161511, 8.181495172785465897 ) ) ;
#12336 = CARTESIAN_POINT ( 'NONE',  ( -10.50000000000000711, -5.000000000000000000, -77.33514508527181874 ) ) ;
#12337 = DIRECTION ( 'NONE',  ( 0.000000000000000000, -1.000000000000000000, 0.000000000000000000 ) ) ;
#12338 = CARTESIAN_POINT ( 'NONE',  ( 5.656854249492380582, -22.81249999999999289, -5.656854249492379694 ) ) ;
#12339 = CARTESIAN_POINT ( 'NONE',  ( 31.24472784702464523, -24.80329577077787206, 39.51072433048258858 ) ) ;
#12340 = VECTOR ( 'NONE', #26209, 1000.000000000000000 ) ;
#12341 = CARTESIAN_POINT ( 'NONE',  ( 0.000000000000000000, 0.000000000000000000, 0.000000000000000000 ) ) ;
#12342 = ORIENTED_EDGE ( 'NONE', *, *, #21437, .F. ) ;
#12343 = CARTESIAN_POINT ( 'NONE',  ( 82.59652397065522678, -60.84044193784809806, 189.6660346993927817 ) ) ;
#12344 = EDGE_CURVE ( 'NONE', #42513, #58193, #84271, .T. ) ;
#12345 = CARTESIAN_POINT ( 'NONE',  ( -48.60240570037294106, 10.21057620019135470, 14.48840219382793038 ) ) ;
#12346 = CARTESIAN_POINT ( 'NONE',  ( -84.44653569564452766, -56.38255921961517458, 190.8904429900520370 ) ) ;
#12347 = ORIENTED_EDGE ( 'NONE', *, *, #24440, .F. ) ;
#12348 = CARTESIAN_POINT ( 'NONE',  ( -95.06236187663560600, -60.15485587419004787, 86.14958005658115781 ) ) ;
#12349 = CARTESIAN_POINT ( 'NONE',  ( 0.000000000000000000, -54.00000000000000711, 27.00000000000000000 ) ) ;
#12350 = DIRECTION ( 'NONE',  ( -1.000000000000000000, 0.000000000000000000, 0.000000000000000000 ) ) ;
#12351 = CARTESIAN_POINT ( 'NONE',  ( 13.75294187950173175, -4.333298119783698610, -11.48770422858942375 ) ) ;
#12352 = CARTESIAN_POINT ( 'NONE',  ( 26.08349330513380337, 1.593028355512270567E-15, 0.000000000000000000 ) ) ;
#12353 = ADVANCED_FACE ( 'NONE', ( #1815 ), #17065, .T. ) ;
#12354 = COLOUR_RGB ( '', 0.31764706, 0.68627451, 0.89019608) ;
#12355 = CARTESIAN_POINT ( 'NONE',  ( 7.822060438254271553, -19.39240910821929376, 35.22573232888181138 ) ) ;
#12356 = CARTESIAN_POINT ( 'NONE',  ( 2.893255198029386133, -0.4647462895689700169, 103.3592142771323665 ) ) ;
#12357 = CARTESIAN_POINT ( 'NONE',  ( 40.55314487144148217, -26.56230035094428743, 36.32082278398921460 ) ) ;
#12358 = EDGE_CURVE ( 'NONE', #4508, #9366, #68720, .T. ) ;
#12360 = CARTESIAN_POINT ( 'NONE',  ( -12.34988716859649394, 17.93113568933560131, 8.716900997220561109 ) ) ;
#12359 = CARTESIAN_POINT ( 'NONE',  ( -35.99893469198357110, -36.03401585327518575, 45.16313413558417977 ) ) ;
#12361 = AXIS2_PLACEMENT_3D ( 'NONE', #42900, #44506, #91976 ) ;
#12362 = CARTESIAN_POINT ( 'NONE',  ( 2.469322996632425049, 298.9266300817046158, -10.00398374146190861 ) ) ;
#12363 = SURFACE_STYLE_USAGE ( .BOTH. , #37214 ) ;
#12364 = CARTESIAN_POINT ( 'NONE',  ( -42.72731753109085417, 485.8496451746398748, 7.279150061871423105 ) ) ;
#12365 = LINE ( 'NONE', #27545, #17312 ) ;
#12366 = ORIENTED_EDGE ( 'NONE', *, *, #11228, .T. ) ;
#12367 = CARTESIAN_POINT ( 'NONE',  ( 0.000000000000000000, 0.000000000000000000, -0.5505556536572887572 ) ) ;
#12368 = ORIENTED_EDGE ( 'NONE', *, *, #24742, .F. ) ;
#12369 = CARTESIAN_POINT ( 'NONE',  ( -15.66846091137126606, -1.219547918084784133, 14.95212397148377548 ) ) ;
#12370 = DIRECTION ( 'NONE',  ( -1.000000000000000000, -0.000000000000000000, -0.000000000000000000 ) ) ;
#12371 = DIRECTION ( 'NONE',  ( -1.000000000000000000, -1.224606353822377258E-16, -0.000000000000000000 ) ) ;
#12372 =( BOUNDED_SURFACE ( )  B_SPLINE_SURFACE ( 2, 3, ( 
 ( #43330, #76211, #36866, #18542, #18004, #19633, #10931, #59524, #34741, #35262, #75685, #50865, #52466, #44395, #20163, #92394, #12008, #60070, #77291, #101565, #3403, #51407, #69216, #83770, #36345, #69734, #58989, #67612, #9881, #84318, #102082, #60596, #53013, #43852, #84848, #28244, #61114, #76742, #44941, #10415, #68130, #1784, #101026, #94001, #2852, #92933, #85937, #19095, #42792, #35806, #68684, #27722, #77825, #91877 ),
 ( #71833, #86475, #22793, #13058, #63238, #29307, #103162, #53544, #79403, #70789, #37927, #38442, #54045, #62706, #62197, #104201, #63770, #47023, #79925, #14646, #47555, #80451, #95083, #20706, #22263, #46507, #6562, #86990, #96658, #6034, #104739, #78869, #39495, #30889, #103685, #29829, #102625, #38957, #55628, #88565, #61665, #95597, #5519, #21215, #88042, #94554, #28783, #12531, #21735, #45466, #45989, #78339, #4457, #55112 ),
 ( #37400, #70261, #30345, #14122, #4996, #54574, #87513, #13593, #71308, #96130, #105276, #41072, #106312, #15727, #33009, #72885, #105796, #16799, #57233, #8696, #33530, #15191, #40013, #16256, #91239, #56704, #66402, #49685, #41604, #48612, #17346, #74487, #73415, #7617, #83122, #82591, #562, #99283, #31422, #32476, #82042, #31935, #57763, #64297, #25462, #58314, #65347, #97169, #81497, #72370, #50221, #24909, #90689, #23316 ) ),
 .UNSPECIFIED., .F., .F., .F. ) 
 B_SPLINE_SURFACE_WITH_KNOTS ( ( 3, 3 ),
 ( 4, 2, 2, 2, 2, 2, 2, 2, 2, 2, 2, 2, 2, 2, 2, 2, 2, 2, 2, 2, 2, 2, 2, 2, 2, 2, 4 ),
 ( 0.000000000000000000, 1.000000000000000000 ),
 ( 0.000000000000000000, 0.01724146208191289220, 0.02586219312286933830, 0.03448292416382578440, 0.04310365520478223050, 0.05172438624573867660, 0.06034511728669512270, 0.06896584832765156881, 0.07758657936860802184, 0.08620731040956446101, 0.1034487724914773532, 0.1120695035324338062, 0.1206902345733902454, 0.1293109656143466846, 0.1379316966553031376, 0.1465524276962595907, 0.1551731587372160437, 0.1637938897781724967, 0.1724146208191289220, 0.1896560829010418003, 0.2068975449829547064, 0.2155182760239111595, 0.2241390070648676125, 0.2413804691467804908, 0.2500012001877369161, 0.2586219312286933691, 0.2758633933106062752 ),
 .UNSPECIFIED. ) 
 GEOMETRIC_REPRESENTATION_ITEM ( )  RATIONAL_B_SPLINE_SURFACE ( (
 ( 1.000000000000000000, 1.000000000000000000, 1.000000000000000000, 1.000000000000000000, 1.000000000000000000, 1.000000000000000000, 1.000000000000000000, 1.000000000000000000, 1.000000000000000000, 1.000000000000000000, 1.000000000000000000, 1.000000000000000000, 1.000000000000000000, 1.000000000000000000, 1.000000000000000000, 1.000000000000000000, 1.000000000000000000, 1.000000000000000000, 1.000000000000000000, 1.000000000000000000, 1.000000000000000000, 1.000000000000000000, 1.000000000000000000, 1.000000000000000000, 1.000000000000000000, 1.000000000000000000, 1.000000000000000000, 1.000000000000000000, 1.000000000000000000, 1.000000000000000000, 1.000000000000000000, 1.000000000000000000, 1.000000000000000000, 1.000000000000000000, 1.000000000000000000, 1.000000000000000000, 1.000000000000000000, 1.000000000000000000, 1.000000000000000000, 1.000000000000000000, 1.000000000000000000, 1.000000000000000000, 1.000000000000000000, 1.000000000000000000, 1.000000000000000000, 1.000000000000000000, 1.000000000000000000, 1.000000000000000000, 1.000000000000000000, 1.000000000000000000, 1.000000000000000000, 1.000000000000000000, 1.000000000000000000, 1.000000000000000000),
 ( 1.857142857142858317, 1.857142857142858317, 1.857142857142858317, 1.857142857142858317, 1.857142857142858317, 1.857142857142858317, 1.857142857142858317, 1.857142857142858317, 1.857142857142858317, 1.857142857142858317, 1.857142857142858317, 1.857142857142858317, 1.857142857142858317, 1.857142857142858317, 1.857142857142858317, 1.857142857142858317, 1.857142857142858317, 1.857142857142858317, 1.857142857142858317, 1.857142857142858317, 1.857142857142858317, 1.857142857142858317, 1.857142857142858317, 1.857142857142858317, 1.857142857142858317, 1.857142857142858317, 1.857142857142858317, 1.857142857142858317, 1.857142857142858317, 1.857142857142858317, 1.857142857142858317, 1.857142857142858317, 1.857142857142858317, 1.857142857142858317, 1.857142857142858317, 1.857142857142858317, 1.857142857142858317, 1.857142857142858317, 1.857142857142858317, 1.857142857142858317, 1.857142857142858317, 1.857142857142858317, 1.857142857142858317, 1.857142857142858317, 1.857142857142858317, 1.857142857142858317, 1.857142857142858317, 1.857142857142858317, 1.857142857142858317, 1.857142857142858317, 1.857142857142858317, 1.857142857142858317, 1.857142857142858317, 1.857142857142858317),
 ( 1.000000000000000000, 1.000000000000000000, 1.000000000000000000, 1.000000000000000000, 1.000000000000000000, 1.000000000000000000, 1.000000000000000000, 1.000000000000000000, 1.000000000000000000, 1.000000000000000000, 1.000000000000000000, 1.000000000000000000, 1.000000000000000000, 1.000000000000000000, 1.000000000000000000, 1.000000000000000000, 1.000000000000000000, 1.000000000000000000, 1.000000000000000000, 1.000000000000000000, 1.000000000000000000, 1.000000000000000000, 1.000000000000000000, 1.000000000000000000, 1.000000000000000000, 1.000000000000000000, 1.000000000000000000, 1.000000000000000000, 1.000000000000000000, 1.000000000000000000, 1.000000000000000000, 1.000000000000000000, 1.000000000000000000, 1.000000000000000000, 1.000000000000000000, 1.000000000000000000, 1.000000000000000000, 1.000000000000000000, 1.000000000000000000, 1.000000000000000000, 1.000000000000000000, 1.000000000000000000, 1.000000000000000000, 1.000000000000000000, 1.000000000000000000, 1.000000000000000000, 1.000000000000000000, 1.000000000000000000, 1.000000000000000000, 1.000000000000000000, 1.000000000000000000, 1.000000000000000000, 1.000000000000000000, 1.000000000000000000) ) ) 
 REPRESENTATION_ITEM ( '' )  SURFACE ( )  );
#12374 = CARTESIAN_POINT ( 'NONE',  ( 7.961997598232706252, -47.40891911902998856, -34.64489477109410132 ) ) ;
#12373 = CARTESIAN_POINT ( 'NONE',  ( 9.797537890442953312, 253.4655779766619048, 2.014215961808876632 ) ) ;
#12375 = ORIENTED_EDGE ( 'NONE', *, *, #95037, .T. ) ;
#12376 = DIRECTION ( 'NONE',  ( -1.000000000000000000, -1.224606353822377258E-16, -0.000000000000000000 ) ) ;
#12377 = CARTESIAN_POINT ( 'NONE',  ( 80.97977184163765685, 1.030564683017419500E-14, 0.000000000000000000 ) ) ;
#12378 = ORIENTED_EDGE ( 'NONE', *, *, #1747, .F. ) ;
#12379 = LINE ( 'NONE', #62549, #60398 ) ;
#12380 = CARTESIAN_POINT ( 'NONE',  ( -46.00000000000000000, 438.4646224975039672, 9.895601460523739235 ) ) ;
#12381 = CARTESIAN_POINT ( 'NONE',  ( -92.03800156008944100, -60.00000000000000000, 19.26534363413594164 ) ) ;
#12382 = ORIENTED_EDGE ( 'NONE', *, *, #73314, .F. ) ;
#12383 = DIRECTION ( 'NONE',  ( -1.000000000000000000, -1.224606353822377258E-16, -0.000000000000000000 ) ) ;
#12384 = CARTESIAN_POINT ( 'NONE',  ( 30.00000000000000000, 488.8442721620239126, 4.433647275927487641 ) ) ;
#12385 = DIRECTION ( 'NONE',  ( -0.000000000000000000, 1.000000000000000000, -0.000000000000000000 ) ) ;
#12386 = CARTESIAN_POINT ( 'NONE',  ( 20.25321052973721692, 294.7697318699768516, 1.919554895086231117 ) ) ;
#12387 = CYLINDRICAL_SURFACE ( 'NONE', #16769, 1.250000000000001110 ) ;
#12388 = CARTESIAN_POINT ( 'NONE',  ( -83.04203994682778500, -39.48694556830105284, 170.2747023245005096 ) ) ;
#12389 = ORIENTED_EDGE ( 'NONE', *, *, #14871, .F. ) ;
#12390 = CARTESIAN_POINT ( 'NONE',  ( -42.42823000592670013, 488.6172904996873854, 9.782215989754741159 ) ) ;
#12391 = ORIENTED_EDGE ( 'NONE', *, *, #68412, .T. ) ;
#12392 = ORIENTED_EDGE ( 'NONE', *, *, #7126, .T. ) ;
#12393 = CARTESIAN_POINT ( 'NONE',  ( 9.999008799016117166, -4.999999999999999112, -14.11099437790398348 ) ) ;
#12394 = CARTESIAN_POINT ( 'NONE',  ( -5.000000000000000000, -13.90268927672064336, 9.980021953238050969 ) ) ;
#12396 = ORIENTED_EDGE ( 'NONE', *, *, #91814, .F. ) ;
#12395 = B_SPLINE_CURVE_WITH_KNOTS ( 'NONE', 3,
 ( #103601, #38879, #29752, #78262, #14042, #62625, #53466, #29234, #95512, #54491, #87962, #88491, #87436, #63695, #46433, #79322, #96583, #5442, #38364, #30266, #22181, #46947, #47475, #3856, #71748, #79848, #22716, #102544, #20624, #28695, #86385, #12453, #15112, #57682 ),
 .UNSPECIFIED., .F., .F.,
 ( 4, 2, 2, 2, 2, 2, 2, 2, 2, 2, 2, 2, 2, 2, 2, 2, 4 ),
 ( 0.01272238763756221476, 0.01351613129786391303, 0.01430987495816561129, 0.01510361861846732691, 0.01589736227876904426, 0.01669110593907075987, 0.01748484959937247549, 0.01827859325967419457, 0.01907233691997591019, 0.01986608058027762580, 0.02065982424057934141, 0.02145356790088105703, 0.02224731156118277264, 0.02304105522148449173, 0.02383479888178620734, 0.02462854254208794377, 0.02542228620238968020 ),
 .UNSPECIFIED. ) ;
#12397 = DIRECTION ( 'NONE',  ( 1.000000000000000000, 0.000000000000000000, -1.224646799147353207E-16 ) ) ;
#12398 = FILL_AREA_STYLE ('',( #78210 ) ) ;
#12399 = CARTESIAN_POINT ( 'NONE',  ( -89.88826151057727998, -57.66708741322880627, -22.42023280972025390 ) ) ;
#12400 = CARTESIAN_POINT ( 'NONE',  ( 7.744168461338432508, -13.46254061715158379, 2.019395720771548053 ) ) ;
#12401 = LINE ( 'NONE', #85247, #4821 ) ;
#12402 = CARTESIAN_POINT ( 'NONE',  ( -9.537291425704607306, 102.3559562266722907, 3.012810007366001130 ) ) ;
#12403 = CYLINDRICAL_SURFACE ( 'NONE', #4632, 8.000000000000000000 ) ;
#12404 = FILL_AREA_STYLE_COLOUR ( '', #14043 ) ;
#12405 =( GEOMETRIC_REPRESENTATION_CONTEXT ( 3 ) GLOBAL_UNCERTAINTY_ASSIGNED_CONTEXT ( ( #75317 ) ) GLOBAL_UNIT_ASSIGNED_CONTEXT ( ( #36232, #44829, #42681 ) ) REPRESENTATION_CONTEXT ( 'NONE', 'WORKASPACE' ) );
#12406 = CARTESIAN_POINT ( 'NONE',  ( 86.47489896066092285, -14.21045842199428932, -14.67047700064687987 ) ) ;
#12407 = AXIS2_PLACEMENT_3D ( 'NONE', #76972, #58128, #59746 ) ;
#12408 = CARTESIAN_POINT ( 'NONE',  ( -75.56794833712217496, -14.21045842199431597, 141.5492349273399952 ) ) ;
#12409 = CARTESIAN_POINT ( 'NONE',  ( -55.71125761005164634, -18.68150336790142418, 53.46817653840955131 ) ) ;
#12410 = VERTEX_POINT ( 'NONE', #18037 ) ;
#12411 = CARTESIAN_POINT ( 'NONE',  ( 6.085184064390054992, 15.01719713745825580, -3.463681541593110147 ) ) ;
#12412 = VERTEX_POINT ( 'NONE', #84884 ) ;
#12413 = CARTESIAN_POINT ( 'NONE',  ( -98.82905336773379190, -37.76367048180233610, 192.0201691225735772 ) ) ;
#12414 = CARTESIAN_POINT ( 'NONE',  ( 102.7253656032815030, -38.00000000000000000, 177.4132030967784033 ) ) ;
#12415 = CARTESIAN_POINT ( 'NONE',  ( -1.249332996999305667, 51.75169767656670672, 8.836784652845731003 ) ) ;
#12416 = ORIENTED_EDGE ( 'NONE', *, *, #3193, .T. ) ;
#12417 = CARTESIAN_POINT ( 'NONE',  ( 7.421727596596154441, -4.999999999999994671, -70.37058874442523404 ) ) ;
#12418 = DIRECTION ( 'NONE',  ( -0.000000000000000000, -1.000000000000000000, -0.000000000000000000 ) ) ;
#12419 = LINE ( 'NONE', #103568, #103610 ) ;
#12420 = CARTESIAN_POINT ( 'NONE',  ( 7.188101187500001821, -16.43750000204838457, -2.977408999572650483 ) ) ;
#12421 = CARTESIAN_POINT ( 'NONE',  ( 23.43684916743750080, 295.2641918988800285, 10.02474406024658293 ) ) ;
#12422 = DIRECTION ( 'NONE',  ( -1.000000000000000000, -1.224606353822377258E-16, -0.000000000000000000 ) ) ;
#12423 = CARTESIAN_POINT ( 'NONE',  ( 8.000086790516061086, -80.99982641893991797, 0.2639471549312816800 ) ) ;
#12424 = CARTESIAN_POINT ( 'NONE',  ( 62.38085580266044872, -29.99999999999999289, 73.03293077709649594 ) ) ;
#12425 = CARTESIAN_POINT ( 'NONE',  ( 35.56416567323501710, 480.2820146177156175, -4.363888856302766683 ) ) ;
#12426 = CARTESIAN_POINT ( 'NONE',  ( -8.241503450148531584, 35.67856248319191792, 0.000000000000000000 ) ) ;
#12427 =( LENGTH_UNIT ( ) NAMED_UNIT ( * ) SI_UNIT ( .MILLI., .METRE. ) );
#12428 = EDGE_CURVE ( 'NONE', #22473, #16299, #99745, .T. ) ;
#12429 = CARTESIAN_POINT ( 'NONE',  ( -5.327003236163648126, 25.27808877631457207, -43.98407828350998727 ) ) ;
#12430 = CARTESIAN_POINT ( 'NONE',  ( -29.47180296636225449, -60.33975193709323293, 36.60485071960074066 ) ) ;
#12431 = AXIS2_PLACEMENT_3D ( 'NONE', #79678, #64052, #62978 ) ;
#12432 = CARTESIAN_POINT ( 'NONE',  ( 48.47115896583378003, -29.13930102312053094, 45.10802347286871594 ) ) ;
#12433 = VECTOR ( 'NONE', #5547, 1000.000000000000000 ) ;
#12434 = CARTESIAN_POINT ( 'NONE',  ( 6.162888688655344005, 3.752776749732565253, 6.499999999999997335 ) ) ;
#12435 = CARTESIAN_POINT ( 'NONE',  ( -1.131038375678608876, 45.55010860757282387, 18.03819305252759264 ) ) ;
#12436 = ADVANCED_FACE ( 'NONE', ( #43363 ), #103222, .T. ) ;
#12437 = AXIS2_PLACEMENT_3D ( 'NONE', #58428, #26109, #27695 ) ;
#12438 = CARTESIAN_POINT ( 'NONE',  ( -93.57730620611623351, -38.49396005077335303, 201.1642509031951249 ) ) ;
#12439 = VERTEX_POINT ( 'NONE', #83807 ) ;
#12440 = CARTESIAN_POINT ( 'NONE',  ( 85.52540355899250812, -38.36029101926790474, -22.36776190553080923 ) ) ;
#12441 = CARTESIAN_POINT ( 'NONE',  ( 83.30308154782368035, -60.00000000000006395, 190.8048519435806440 ) ) ;
#12442 = CARTESIAN_POINT ( 'NONE',  ( -18.91820967797469777, 48.57556059539511750, 62.17047390035803289 ) ) ;
#12443 = CARTESIAN_POINT ( 'NONE',  ( 81.84444444444444855, 4.172000000000019249, 0.000000000000000000 ) ) ;
#12444 = CARTESIAN_POINT ( 'NONE',  ( 6.499946456771120040, 41.29102236647165114, -70.87268750739401924 ) ) ;
#12445 = CARTESIAN_POINT ( 'NONE',  ( -32.05160878076967634, 435.5671699148836638, 16.71734082338229754 ) ) ;
#12446 = CARTESIAN_POINT ( 'NONE',  ( 5.000000000000000000, -23.50449067138091053, -3.099878936449560474 ) ) ;
#12448 = COLOUR_RGB ( '', 0.72549020, 0.75294118, 0.79215686) ;
#12447 = LINE ( 'NONE', #102538, #28085 ) ;
#12449 = CARTESIAN_POINT ( 'NONE',  ( 110.9799143117941043, -60.00000000000001421, 187.5157448101569173 ) ) ;
#12450 = EDGE_CURVE ( 'NONE', #61515, #68693, #57932, .T. ) ;
#12451 = DIRECTION ( 'NONE',  ( -1.000000000000000000, -0.000000000000000000, -0.000000000000000000 ) ) ;
#12452 = EDGE_LOOP ( 'NONE', ( #74843, #76469, #42771, #85446 ) ) ;
#12453 = CARTESIAN_POINT ( 'NONE',  ( 6.944371705245972137, 30.53899691424550511, -3.972324460300560744 ) ) ;
#12454 = DIRECTION ( 'NONE',  ( -1.000000000000000000, -0.000000000000000000, -0.000000000000000000 ) ) ;
#12455 = ORIENTED_EDGE ( 'NONE', *, *, #27425, .T. ) ;
#12457 = CARTESIAN_POINT ( 'NONE',  ( 5.293416525178801457, 18.46906883814961375, -37.84133857137602064 ) ) ;
#12456 = CARTESIAN_POINT ( 'NONE',  ( -72.55053978524345837, -38.32605109717405867, 149.3030407648667222 ) ) ;
#12458 = DIRECTION ( 'NONE',  ( 1.000000000000000000, -0.000000000000000000, 1.224646799147353207E-16 ) ) ;
#12459 = CARTESIAN_POINT ( 'NONE',  ( -4.916373759799319565, -2.999999999999999556, -6.397334739185442487 ) ) ;
#12460 = SURFACE_STYLE_USAGE ( .BOTH. , #55038 ) ;
#12461 = CARTESIAN_POINT ( 'NONE',  ( 7.188101187500000044, -10.53125000204838457, 0.000000000000000000 ) ) ;
#12462 = CARTESIAN_POINT ( 'NONE',  ( -6.145467200813103936, -5.000000000008177459, -92.99666842290147883 ) ) ;
#12463 = CARTESIAN_POINT ( 'NONE',  ( 18.58349330513380337, 1.593028355512270567E-15, 0.000000000000000000 ) ) ;
#12464 = ORIENTED_EDGE ( 'NONE', *, *, #89531, .F. ) ;
#12465 = CARTESIAN_POINT ( 'NONE',  ( 81.41541248120216778, -53.44831681439456617, 177.1204070320672201 ) ) ;
#12466 = CARTESIAN_POINT ( 'NONE',  ( 8.017333092632471292, 103.9739446863702454, 0.000000000000000000 ) ) ;
#12467 = CARTESIAN_POINT ( 'NONE',  ( 4.250000000000000000, 0.000000000000000000, -5.185501489199872083 ) ) ;
#12468 = ORIENTED_EDGE ( 'NONE', *, *, #17693, .F. ) ;
#12469 = DIRECTION ( 'NONE',  ( 1.000000000000000000, 1.224606353822377258E-16, 0.000000000000000000 ) ) ;
#12470 = CARTESIAN_POINT ( 'NONE',  ( 17.86121324767568552, 34.21128550139528102, 23.65650543089517654 ) ) ;
#12471 = CARTESIAN_POINT ( 'NONE',  ( -7.000000000000000000, 8.572527594031471218E-16, -13.00000000000000000 ) ) ;
#12472 = CARTESIAN_POINT ( 'NONE',  ( 30.00000000000000355, 488.8442721620236853, 4.433647275927599551 ) ) ;
#12473 = VECTOR ( 'NONE', #88406, 1000.000000000000000 ) ;
#12474 = CARTESIAN_POINT ( 'NONE',  ( -28.94895647869480726, 13.71030094619075967, -39.84075445247425051 ) ) ;
#12475 = CARTESIAN_POINT ( 'NONE',  ( -20.33030176445824821, 302.8588253227683822, 9.938492008999505245 ) ) ;
#12476 = VERTEX_POINT ( 'NONE', #33694 ) ;
#12477 = EDGE_CURVE ( 'NONE', #33657, #101842, #49130, .T. ) ;
#12478 = APPLICATION_PROTOCOL_DEFINITION ( 'draft international standard', 'automotive_design', 1998, #102408 ) ;
#12480 = CARTESIAN_POINT ( 'NONE',  ( -6.953544250145660577, 296.7171512541748370, 7.191915520096927139 ) ) ;
#12479 = AXIS2_PLACEMENT_3D ( 'NONE', #14821, #89792, #15895 ) ;
#12481 = DIRECTION ( 'NONE',  ( -1.000000000000000000, -1.224606353822377258E-16, -0.000000000000000000 ) ) ;
#12482 = CARTESIAN_POINT ( 'NONE',  ( 0.4964154566687890013, 4.996589667937373136, 7.345652830558761615 ) ) ;
#12483 = EDGE_CURVE ( 'NONE', #72225, #106540, #78235, .T. ) ;
#12484 = ADVANCED_FACE ( 'NONE', ( #66568, #99451 ), #58487, .F. ) ;
#12486 = SURFACE_STYLE_FILL_AREA ( #53497 ) ;
#12485 = DIRECTION ( 'NONE',  ( 0.000000000000000000, 0.000000000000000000, -1.000000000000000000 ) ) ;
#12487 = CARTESIAN_POINT ( 'NONE',  ( 5.082755093536325930, -23.46875000204838457, -5.082755093536325042 ) ) ;
#12488 = CARTESIAN_POINT ( 'NONE',  ( 22.57792046605466041, 1.340359594676612611E-15, 0.000000000000000000 ) ) ;
#12489 = CARTESIAN_POINT ( 'NONE',  ( -4.250000000000000000, 5.204748896376250699E-16, -10.00000000000000000 ) ) ;
#12490 = DIRECTION ( 'NONE',  ( -0.000000000000000000, -0.000000000000000000, -1.000000000000000000 ) ) ;
#12491 = EDGE_LOOP ( 'NONE', ( #90565, #61291, #51792, #105300 ) ) ;
#12492 = DIRECTION ( 'NONE',  ( -1.000000000000000000, -0.000000000000000000, -0.000000000000000000 ) ) ;
#12493 = CYLINDRICAL_SURFACE ( 'NONE', #89172, 13.00000000000003730 ) ;
#12494 = CARTESIAN_POINT ( 'NONE',  ( -9.421434414404789237, 10.25265380207672550, -8.673617380148899465E-16 ) ) ;
#12495 = VECTOR ( 'NONE', #13400, 1000.000000000000000 ) ;
#12496 = DIRECTION ( 'NONE',  ( 0.000000000000000000, -1.000000000000000000, 0.000000000000000000 ) ) ;
#12497 = EDGE_CURVE ( 'NONE', #95018, #102396, #104920, .T. ) ;
#12498 =( GEOMETRIC_REPRESENTATION_CONTEXT ( 3 ) GLOBAL_UNCERTAINTY_ASSIGNED_CONTEXT ( ( #47761 ) ) GLOBAL_UNIT_ASSIGNED_CONTEXT ( ( #41269, #48811, #89829 ) ) REPRESENTATION_CONTEXT ( 'NONE', 'WORKASPACE' ) );
#12499 = EDGE_LOOP ( 'NONE', ( #7798, #94264, #85795, #56602 ) ) ;
#12500 = DIRECTION ( 'NONE',  ( 0.000000000000000000, 0.000000000000000000, -1.000000000000000000 ) ) ;
#12501 = CARTESIAN_POINT ( 'NONE',  ( -7.717304146825799016, 50.00000000000000000, -95.65871486499432308 ) ) ;
#12502 = ORIENTED_EDGE ( 'NONE', *, *, #86694, .T. ) ;
#12503 = ADVANCED_FACE ( 'NONE', ( #70301 ), #82502, .T. ) ;
#12504 = DIRECTION ( 'NONE',  ( 0.000000000000000000, -0.9971933454386585627, -0.07486943176528132460 ) ) ;
#12505 = LINE ( 'NONE', #45436, #43212 ) ;
#12506 = CARTESIAN_POINT ( 'NONE',  ( -9.165151389911699198, 249.9999999999999716, -4.000000000000002665 ) ) ;
#12507 = UNCERTAINTY_MEASURE_WITH_UNIT (LENGTH_MEASURE( 1.000000000000000082E-05 ), #70906, 'distance_accuracy_value', 'NONE');
#12508 = CARTESIAN_POINT ( 'NONE',  ( -112.0710918845811364, -59.99999999999999289, 178.4928572454104483 ) ) ;
#12509 = CARTESIAN_POINT ( 'NONE',  ( 0.000000000000000000, 152.0000000000000000, 5.000000000000000000 ) ) ;
#12510 = CARTESIAN_POINT ( 'NONE',  ( 0.3173508448886528388, -8.480771745766398695, -1.310872448937994150 ) ) ;
#12511 = DIRECTION ( 'NONE',  ( -1.000000000000000000, -1.224606353822377258E-16, -0.000000000000000000 ) ) ;
#12512 = ADVANCED_FACE ( 'NONE', ( #61149 ), #67841, .T. ) ;
#12513 = SURFACE_STYLE_FILL_AREA ( #69713 ) ;
#12514 = CARTESIAN_POINT ( 'NONE',  ( -83.34697557531410439, -46.52569824882559857, 181.7021836014866949 ) ) ;
#12515 = CARTESIAN_POINT ( 'NONE',  ( 43.55653793352204417, 41.43733932821601229, -50.61966037282592623 ) ) ;
#12516 = VERTEX_POINT ( 'NONE', #94036 ) ;
#12517 = CARTESIAN_POINT ( 'NONE',  ( 7.999999999999998224, -26.09374999999999645, 3.313708498984766049 ) ) ;
#12518 = CYLINDRICAL_SURFACE ( 'NONE', #68059, 1.250000000000001110 ) ;
#12519 = CARTESIAN_POINT ( 'NONE',  ( -86.98955879380979184, -60.18195689495087208, -5.047257192535347770 ) ) ;
#12520 = DIRECTION ( 'NONE',  ( 0.000000000000000000, -1.000000000000000000, 0.000000000000000000 ) ) ;
#12521 = CARTESIAN_POINT ( 'NONE',  ( -4.075111047341576587, 138.1306820922419547, -4.999999999999997335 ) ) ;
#12522 = CARTESIAN_POINT ( 'NONE',  ( 2.869468778192039160, 87.32905104808958185, -5.000000000000000888 ) ) ;
#12523 = LINE ( 'NONE', #70252, #66598 ) ;
#12524 = CARTESIAN_POINT ( 'NONE',  ( -23.57730434126679597, 18.64316884711713485, 30.67950393662591324 ) ) ;
#12525 = CARTESIAN_POINT ( 'NONE',  ( 86.31905819422470927, -30.00000000000006750, 198.0863690661441296 ) ) ;
#12526 = CARTESIAN_POINT ( 'NONE',  ( -1.600194386257964019E-15, 60.33964880548970200, 13.06657876680918662 ) ) ;
#12527 = CARTESIAN_POINT ( 'NONE',  ( -86.47621369144106040, -14.21045842199425735, -14.66750133381012589 ) ) ;
#12528 = CARTESIAN_POINT ( 'NONE',  ( -66.02922395999594585, -18.62684786674785187, 78.34317924958739354 ) ) ;
#12529 = ORIENTED_EDGE ( 'NONE', *, *, #29997, .F. ) ;
#12530 = CARTESIAN_POINT ( 'NONE',  ( 91.09720049356627669, -14.21045842199416143, 197.8400994950010272 ) ) ;
#12531 = CARTESIAN_POINT ( 'NONE',  ( 64.56043141426960119, 39.42554324411963762, -8.108556725190846137 ) ) ;
#12532 = CARTESIAN_POINT ( 'NONE',  ( 71.72808885978980697, -60.00000000001963940, 173.2180474971540605 ) ) ;
#12533 = ORIENTED_EDGE ( 'NONE', *, *, #807, .F. ) ;
#12534 = LINE ( 'NONE', #53547, #42424 ) ;
#12535 = CARTESIAN_POINT ( 'NONE',  ( 4.401442555609581635E-16, -20.65625000204838813, -7.188101187500000044 ) ) ;
#12536 = CIRCLE ( 'NONE', #24668, 5.000000000000001776 ) ;
#12537 = CARTESIAN_POINT ( 'NONE',  ( -5.477578620271509102, -6.834985609838969189, -2.459398706554655423 ) ) ;
#12538 = EDGE_LOOP ( 'NONE', ( #103859, #88873, #29982, #47975 ) ) ;
#12539 = CARTESIAN_POINT ( 'NONE',  ( -11.53285117555248007, 45.44727734447007350, 14.28089210442085921 ) ) ;
#12540 = ORIENTED_EDGE ( 'NONE', *, *, #23345, .F. ) ;
#12541 = CYLINDRICAL_SURFACE ( 'NONE', #56201, 4.000000000000000888 ) ;
#12542 = CIRCLE ( 'NONE', #43527, 4.000000000000007105 ) ;
#12543 = CARTESIAN_POINT ( 'NONE',  ( 46.92395915124532024, 18.83177588379324163, -15.01493731818186816 ) ) ;
#12544 = CARTESIAN_POINT ( 'NONE',  ( -13.94972454548224405, -60.00000000000000000, -42.23494151491821924 ) ) ;
#12545 = CARTESIAN_POINT ( 'NONE',  ( 35.98289756235140402, 343.5663561902737797, -0.4926348694814616791 ) ) ;
#12546 = CARTESIAN_POINT ( 'NONE',  ( -5.082755093536326818, -33.59375000204838813, 5.082755093536325042 ) ) ;
#12547 = CARTESIAN_POINT ( 'NONE',  ( 32.84229071576313430, 485.9543065954273970, 5.517463591349936358 ) ) ;
#12548 = TOROIDAL_SURFACE ( 'NONE', #19546, 14.78272384904389192, 0.5000000000000000000 ) ;
#12549 =( NAMED_UNIT ( * ) SI_UNIT ( $, .STERADIAN. ) SOLID_ANGLE_UNIT ( ) );
#12550 =( NAMED_UNIT ( * ) SI_UNIT ( $, .STERADIAN. ) SOLID_ANGLE_UNIT ( ) );
#12551 = DIRECTION ( 'NONE',  ( -0.8191520442889884679, 1.003171929053520679E-16, 0.5735764363510508224 ) ) ;
#12552 = CARTESIAN_POINT ( 'NONE',  ( 39.82092066244369022, 436.5808519682737483, 5.503544575420478147 ) ) ;
#12553 = ADVANCED_FACE ( 'NONE', ( #20197 ), #54473, .T. ) ;
#12554 = CARTESIAN_POINT ( 'NONE',  ( 30.00000000000000000, 0.000000000000000000, 0.000000000000000000 ) ) ;
#12555 = ORIENTED_EDGE ( 'NONE', *, *, #73428, .F. ) ;
#12556 = DIRECTION ( 'NONE',  ( -1.000000000000000000, -1.224606353822377258E-16, -0.000000000000000000 ) ) ;
#12557 = CARTESIAN_POINT ( 'NONE',  ( 4.792515968931314596, -2.702239074782193384, 102.4138677444059766 ) ) ;
#12558 = B_SPLINE_CURVE_WITH_KNOTS ( 'NONE', 3,
 ( #85090, #93180, #66778, #99119, #100727, #34450, #26889, #92640, #51644, #84564, #76448, #50563, #11174, #83480, #35505, #67320, #33366, #101278, #27429, #58141, #91069, #17176, #1486, #33909, #99667, #42492, #26366, #59230, #92103, #18246, #84022, #5236, #52706, #53773, #11709, #37641 ),
 .UNSPECIFIED., .F., .F.,
 ( 4, 2, 2, 2, 2, 2, 2, 2, 2, 2, 2, 2, 2, 2, 2, 2, 2, 4 ),
 ( 1.734723475976807094E-18, 0.0007996222028895917872, 0.001599244405779181840, 0.003198488811558361511, 0.003998111014447950154, 0.004797733217337540532, 0.005597355420227129175, 0.006396977623116717818, 0.006796788724561513874, 0.007196599826006308195, 0.007996222028895896838, 0.008795844231785485481, 0.009595466434675074124, 0.01039508863756466277, 0.01119471084045425141, 0.01159452194189904313, 0.01199433304334383658, 0.01279395524623341482 ),
 .UNSPECIFIED. ) ;
#12559 = AXIS2_PLACEMENT_3D ( 'NONE', #84232, #10326, #35173 ) ;
#12561 = CARTESIAN_POINT ( 'NONE',  ( 32.97681988584721324, -36.02474376031975822, 33.68276379229053674 ) ) ;
#12560 = CARTESIAN_POINT ( 'NONE',  ( -3.459690225512181083, -48.89101625908396187, 104.5059395991341376 ) ) ;
#12562 = ORIENTED_EDGE ( 'NONE', *, *, #55159, .T. ) ;
#12563 = EDGE_CURVE ( 'NONE', #91003, #34395, #21816, .T. ) ;
#12564 = CARTESIAN_POINT ( 'NONE',  ( -6.145467199749146125, 48.00000000000000000, -77.00333157601821199 ) ) ;
#12565 = EDGE_CURVE ( 'NONE', #21060, #70045, #16293, .T. ) ;
#12567 = CARTESIAN_POINT ( 'NONE',  ( 0.000000000000000000, 0.000000000000000000, 0.000000000000000000 ) ) ;
#12566 = DIRECTION ( 'NONE',  ( 0.000000000000000000, 0.000000000000000000, 1.000000000000000000 ) ) ;
#12568 = FACE_OUTER_BOUND ( 'NONE', #1037, .T. ) ;
#12569 = FACE_OUTER_BOUND ( 'NONE', #100330, .T. ) ;
#12570 = CARTESIAN_POINT ( 'NONE',  ( -40.20451861284639250, 437.0088225241107693, 5.689194366313575557 ) ) ;
#12571 = DIRECTION ( 'NONE',  ( -0.000000000000000000, -0.000000000000000000, -1.000000000000000000 ) ) ;
#12572 = CARTESIAN_POINT ( 'NONE',  ( 5.299999999999999822, 0.000000000000000000, -4.400000000000000355 ) ) ;
#12573 = ORIENTED_EDGE ( 'NONE', *, *, #11413, .F. ) ;
#12574 = CARTESIAN_POINT ( 'NONE',  ( 91.89176552790895869, -59.99999999999999289, 9.187668761806360607 ) ) ;
#12575 = CARTESIAN_POINT ( 'NONE',  ( 81.26467260280679739, -2.002967142162725287E-29, 5.000000000000011546 ) ) ;
#12576 = CARTESIAN_POINT ( 'NONE',  ( 33.00496812083877529, 465.6658704666191966, 15.15901827093884968 ) ) ;
#12577 = EDGE_CURVE ( 'NONE', #62895, #54301, #23357, .T. ) ;
#12578 = ADVANCED_FACE ( 'NONE', ( #105314 ), #6075, .T. ) ;
#12579 = VECTOR ( 'NONE', #75732, 1000.000000000000114 ) ;
#12580 = CARTESIAN_POINT ( 'NONE',  ( -6.806778129255477872, 41.25019534346876782, -70.74215739106598733 ) ) ;
#12581 = CARTESIAN_POINT ( 'NONE',  ( -14.01679991993937868, 20.87195963505847374, -6.206891275040918643 ) ) ;
#12582 = VERTEX_POINT ( 'NONE', #73455 ) ;
#12583 = CARTESIAN_POINT ( 'NONE',  ( -103.8379607931385777, -30.00000000000037303, 196.7236767739510128 ) ) ;
#12584 = ORIENTED_EDGE ( 'NONE', *, *, #93605, .T. ) ;
#12585 = CARTESIAN_POINT ( 'NONE',  ( 16.64348903516523848, -1.200000000000000030E-05, 5.407797401561420969 ) ) ;
#12586 = LINE ( 'NONE', #37448, #79869 ) ;
#12587 = CARTESIAN_POINT ( 'NONE',  ( 15.72449985194334943, 22.05660461081444268, 3.876398783277453131 ) ) ;
#12588 = FILL_AREA_STYLE_COLOUR ( '', #87405 ) ;
#12589 = AXIS2_PLACEMENT_3D ( 'NONE', #59311, #2644, #44188 ) ;
#12590 = CARTESIAN_POINT ( 'NONE',  ( -1.320432766682874540E-15, -33.40625000204838813, 7.188101187500000044 ) ) ;
#12591 = CARTESIAN_POINT ( 'NONE',  ( -17.50415200142436234, 45.00000000000000711, 63.77658534312520544 ) ) ;
#12592 = CARTESIAN_POINT ( 'NONE',  ( -3.291807555861496315, 304.8518027751348995, 8.936999415071573694 ) ) ;
#12593 = CARTESIAN_POINT ( 'NONE',  ( 88.48689482502902592, 6.123233995736582872E-16, -5.000000000000011546 ) ) ;
#12594 = ORIENTED_EDGE ( 'NONE', *, *, #79181, .T. ) ;
#12596 = ORIENTED_EDGE ( 'NONE', *, *, #74241, .T. ) ;
#12595 = CARTESIAN_POINT ( 'NONE',  ( 26.08349330513380337, 1.593028355512270567E-15, 0.000000000000000000 ) ) ;
#12597 = CARTESIAN_POINT ( 'NONE',  ( 81.09557302793662359, -22.15391159154729195, 134.4882534712255904 ) ) ;
#12598 = PRESENTATION_STYLE_ASSIGNMENT (( #103748 ) ) ;
#12599 = ORIENTED_EDGE ( 'NONE', *, *, #37721, .T. ) ;
#12600 = CARTESIAN_POINT ( 'NONE',  ( 4.781207304706819983, -47.39297744640040122, 40.35843253569867528 ) ) ;
#12601 = CARTESIAN_POINT ( 'NONE',  ( 2.977408999572652260, -16.43750000204838813, 7.188101187500000044 ) ) ;
#12602 = CARTESIAN_POINT ( 'NONE',  ( -80.15954706948889452, -57.50857130571672826, 199.0044224626226139 ) ) ;
#12603 = VERTEX_POINT ( 'NONE', #90191 ) ;
#12604 = PRESENTATION_STYLE_ASSIGNMENT (( #103234 ) ) ;
#12605 = DIRECTION ( 'NONE',  ( 0.000000000000000000, 1.000000000000000000, 0.000000000000000000 ) ) ;
#12606 = CARTESIAN_POINT ( 'NONE',  ( -9.165151389911681434, 84.99999999999998579, -4.000000000000000000 ) ) ;
#12607 = EDGE_CURVE ( 'NONE', #104803, #78936, #40722, .T. ) ;
#12608 = DIRECTION ( 'NONE',  ( 0.000000000000000000, 0.000000000000000000, 1.000000000000000000 ) ) ;
#12609 = CARTESIAN_POINT ( 'NONE',  ( 3.313708498984762052, -15.40625000409677092, -8.000000000000000000 ) ) ;
#12610 = DIRECTION ( 'NONE',  ( -1.000000000000000000, -1.224606353822377258E-16, -0.000000000000000000 ) ) ;
#12611 = CARTESIAN_POINT ( 'NONE',  ( 56.22793774957824553, 4.000000000000013323, 0.000000000000000000 ) ) ;
#12612 = STYLED_ITEM ( 'NONE', ( #20543 ), #54542 ) ;
#12613 = CARTESIAN_POINT ( 'NONE',  ( -1.000000000000000000, -68.32597503900204572, 12.04364623808024781 ) ) ;
#12614 = DIRECTION ( 'NONE',  ( 0.000000000000000000, 1.000000000000000000, 0.000000000000000000 ) ) ;
#12615 = CARTESIAN_POINT ( 'NONE',  ( 4.960693420635299056, 51.41875661953385190, 8.497939143228606440 ) ) ;
#12616 = CIRCLE ( 'NONE', #98691, 4.000000000000001776 ) ;
#12617 = CARTESIAN_POINT ( 'NONE',  ( -38.11708234716855515, 104.1183258647170362, 378.2207925529395993 ) ) ;
#12618 = CARTESIAN_POINT ( 'NONE',  ( 2.048435453982682120, -30.00000000000000355, -7.401063805010598351 ) ) ;
#12619 = ORIENTED_EDGE ( 'NONE', *, *, #88842, .F. ) ;
#12620 = CARTESIAN_POINT ( 'NONE',  ( -1.921192241758119978, -49.89471155215800735, 44.77608010490040158 ) ) ;
#12621 = CARTESIAN_POINT ( 'NONE',  ( 11.04680601421287278, -4.985848638097940544, -12.57695916701952576 ) ) ;
#12622 = AXIS2_PLACEMENT_3D ( 'NONE', #78715, #46883, #53406 ) ;
#12623 = DIRECTION ( 'NONE',  ( -1.000000000000000000, -0.000000000000000000, -0.000000000000000000 ) ) ;
#12624 = CARTESIAN_POINT ( 'NONE',  ( -65.25607705482885024, -29.77640809674063860, -22.97023434858075319 ) ) ;
#12625 = CARTESIAN_POINT ( 'NONE',  ( -79.77046542224586290, -30.00000000000000355, 132.9793268207660333 ) ) ;
#12626 = EDGE_CURVE ( 'NONE', #60578, #48387, #43797, .T. ) ;
#12627 = DIRECTION ( 'NONE',  ( 1.000000000000000000, 1.224606353822377258E-16, 0.000000000000000000 ) ) ;
#12628 = B_SPLINE_CURVE_WITH_KNOTS ( 'NONE', 3,
 ( #79379, #5500, #38423, #3913 ),
 .UNSPECIFIED., .F., .F.,
 ( 4, 4 ),
 ( 6.938893903907228378E-18, 0.002366282582215003139 ),
 .UNSPECIFIED. ) ;
#12629 = ORIENTED_EDGE ( 'NONE', *, *, #90343, .T. ) ;
#12630 = CARTESIAN_POINT ( 'NONE',  ( 0.000000000000000000, 0.000000000000000000, 0.000000000000000000 ) ) ;
#12631 = STYLED_ITEM ( 'NONE', ( #17257 ), #21310 ) ;
#12632 = CARTESIAN_POINT ( 'NONE',  ( 77.76963947670292043, -57.51447515414862011, 196.2475803584244147 ) ) ;
#12633 = CARTESIAN_POINT ( 'NONE',  ( 69.47333816740184886, -60.22837470586443231, -26.63215147159283802 ) ) ;
#12634 = CARTESIAN_POINT ( 'NONE',  ( 0.2813450144774453654, -7.667988119308889239, -6.122077150241866939 ) ) ;
#12635 = CARTESIAN_POINT ( 'NONE',  ( -14.59912249378909443, 22.21173916952167815, -3.991112248694528297 ) ) ;
#12636 = CARTESIAN_POINT ( 'NONE',  ( 40.92692307692308162, 1.411358822780289120E-15, 0.000000000000000000 ) ) ;
#12637 = CARTESIAN_POINT ( 'NONE',  ( -52.62616307540574212, -60.00000000000000711, 78.63067357585181583 ) ) ;
#12638 = DIRECTION ( 'NONE',  ( 0.000000000000000000, 0.000000000000000000, 1.000000000000000000 ) ) ;
#12639 = CARTESIAN_POINT ( 'NONE',  ( -32.15166163075724626, 486.0589784586660471, 5.199393881400879103 ) ) ;
#12640 = ADVANCED_FACE ( 'NONE', ( #97208, #22833 ), #56194, .T. ) ;
#12641 = CARTESIAN_POINT ( 'NONE',  ( -11.91432047182436094, 49.99999999999999289, 64.17585289259305625 ) ) ;
#12642 = CARTESIAN_POINT ( 'NONE',  ( -85.09823223632439237, -46.56888121716310280, 187.7722408975631652 ) ) ;
#12644 = EDGE_LOOP ( 'NONE', ( #92912, #96560, #40310, #18296, #36493 ) ) ;
#12643 = AXIS2_PLACEMENT_3D ( 'NONE', #102297, #78546, #4143 ) ;
#12645 = CARTESIAN_POINT ( 'NONE',  ( 35.20405031252158068, 355.7307837764093961, 2.598712449362419186 ) ) ;
#12646 = CARTESIAN_POINT ( 'NONE',  ( -17.08544069068336668, 304.5690947107618740, -10.06009145438461161 ) ) ;
#12647 = CARTESIAN_POINT ( 'NONE',  ( -6.986467899046544971, 41.76526127512707376, -59.56845298218130580 ) ) ;
#12648 = CARTESIAN_POINT ( 'NONE',  ( 35.02595189227434247, 491.4435019764543995, 12.32055256812844668 ) ) ;
#12649 = COLOUR_RGB ( '', 0.66274510, 0.83137255, 0.94901961) ;
#12650 = DIRECTION ( 'NONE',  ( 0.000000000000000000, 0.000000000000000000, -1.000000000000000000 ) ) ;
#12651 = CARTESIAN_POINT ( 'NONE',  ( -31.06063738904513016, 311.6677864819774868, -8.170013517389778102 ) ) ;
#12652 = CIRCLE ( 'NONE', #45413, 13.50000000000000000 ) ;
#12653 = CARTESIAN_POINT ( 'NONE',  ( 44.35000000000000142, 3.309500000000003439, 4.052968581778167743E-16 ) ) ;
#12654 = SURFACE_SIDE_STYLE ('',( #30470 ) ) ;
#12655 = CARTESIAN_POINT ( 'NONE',  ( 83.28888888888889142, 1.023464760207051730E-14, 0.000000000000000000 ) ) ;
#12656 =( GEOMETRIC_REPRESENTATION_CONTEXT ( 3 ) GLOBAL_UNCERTAINTY_ASSIGNED_CONTEXT ( ( #27651 ) ) GLOBAL_UNIT_ASSIGNED_CONTEXT ( ( #95144, #78938, #100162 ) ) REPRESENTATION_CONTEXT ( 'NONE', 'WORKASPACE' ) );
#12657 = EDGE_LOOP ( 'NONE', ( #24893, #74320, #104654, #25191 ) ) ;
#12658 = CARTESIAN_POINT ( 'NONE',  ( 18.22111540436264221, 50.00000000000000711, 61.60966662904773017 ) ) ;
#12659 = CARTESIAN_POINT ( 'NONE',  ( 46.08349330513379982, -7.703719777548943412E-31, 4.000000000000001776 ) ) ;
#12660 = CARTESIAN_POINT ( 'NONE',  ( 22.03900363279368690, -4.285714285714963268, -12.70248734011530622 ) ) ;
#12661 =( LENGTH_UNIT ( ) NAMED_UNIT ( * ) SI_UNIT ( .MILLI., .METRE. ) );
#12662 = CARTESIAN_POINT ( 'NONE',  ( 90.16383085397569630, -14.21045842199434084, 52.56522323202336366 ) ) ;
#12663 = CARTESIAN_POINT ( 'NONE',  ( -77.52747395753381454, -56.84636302205639424, 148.6058317181106077 ) ) ;
#12664 = PRODUCT_DEFINITION ( 'UNKNOWN', '', #95586, #82334 ) ;
#12665 = ORIENTED_EDGE ( 'NONE', *, *, #50931, .T. ) ;
#12666 = PRESENTATION_STYLE_ASSIGNMENT (( #35942 ) ) ;
#12667 = CARTESIAN_POINT ( 'NONE',  ( 6.738100180926640093, 41.71798714554645215, -59.05424661244425266 ) ) ;
#12668 = CARTESIAN_POINT ( 'NONE',  ( 18.26666949864142353, -57.67159702739868266, 41.99773675405111106 ) ) ;
#12669 = CARTESIAN_POINT ( 'NONE',  ( 56.15646638878826735, 50.00000000000000711, 28.58272340641810771 ) ) ;
#12670 = CARTESIAN_POINT ( 'NONE',  ( 35.26778407330819221, 324.1042954016264162, -4.804630642184931411 ) ) ;
#12671 = DIRECTION ( 'NONE',  ( -1.000000000000000000, -1.224606353822377258E-16, -0.000000000000000000 ) ) ;
#12672 = EDGE_LOOP ( 'NONE', ( #71150, #67387, #68825, #73278, #79971 ) ) ;
#12673 = CARTESIAN_POINT ( 'NONE',  ( 4.650896588451713498, 54.30650138372552505, -6.203625354536873360 ) ) ;
#12674 = CARTESIAN_POINT ( 'NONE',  ( 31.66834350436152690, 439.0151449066551663, 23.43599344638407800 ) ) ;
#12675 = CARTESIAN_POINT ( 'NONE',  ( -7.188101187500000044, -25.90625000204838813, -8.802885111219163269E-16 ) ) ;
#12676 = VERTEX_POINT ( 'NONE', #30386 ) ;
#12678 = CARTESIAN_POINT ( 'NONE',  ( 44.26028122668510179, 485.3157014729748653, 1.872110468833780406 ) ) ;
#12677 =( BOUNDED_SURFACE ( )  B_SPLINE_SURFACE ( 3, 2, ( 
 ( #52917, #12967, #77733 ),
 ( #102533, #4363, #36250 ),
 ( #70165, #29738, #62611 ),
 ( #85841, #94458, #78769 ),
 ( #38353, #86894, #69119 ),
 ( #28150, #3844, #61026 ),
 ( #70698, #37834, #95497 ),
 ( #71213, #36775, #20069 ),
 ( #53455, #86375, #54475 ),
 ( #87424, #45367, #78250 ),
 ( #103069, #13498, #79307 ),
 ( #60505, #93390, #19536 ),
 ( #52373, #97597, #105182 ),
 ( #30794, #32380, #47984 ),
 ( #30250, #23223, #7002 ),
 ( #16160, #63679, #31327 ),
 ( #105699, #22702, #89537 ),
 ( #8066, #72278, #80891 ),
 ( #24294, #65252, #79832 ),
 ( #63138, #55539, #49047 ),
 ( #64209, #81944, #31841 ),
 ( #22164, #72794, #55013 ),
 ( #96038, #38864, #14027 ),
 ( #40978, #104642, #39922 ),
 ( #7522, #57143, #56612 ),
 ( #73866, #48520, #15097 ),
 ( #64723, #87945, #71730 ),
 ( #46933, #73320, #97079 ),
 ( #81411, #89002, #23764 ),
 ( #15628, #96567, #98142 ),
 ( #88476, #5937, #56062 ),
 ( #14551, #47460, #40440 ),
 ( #106216, #80353, #90056 ),
 ( #6468, #39400, #83550 ),
 ( #9123, #66311, #92171 ),
 ( #58217, #67909, #91142 ),
 ( #66852, #17252, #84629 ),
 ( #74915, #99741, #67390 ),
 ( #32909, #75463, #43632 ),
 ( #99192, #50123, #8600 ),
 ( #50632, #25911, #26956 ),
 ( #92710, #100796, #75994 ),
 ( #59836, #10716, #43106 ),
 ( #58767, #41502, #18870 ),
 ( #16700, #98664, #24816 ),
 ( #91665, #74390, #9650 ),
 ( #17779, #83032, #42560 ),
 ( #51714, #25354, #59299 ),
 ( #106761, #42033, #1556 ),
 ( #65786, #34521, #2092 ),
 ( #57668, #999, #33980 ),
 ( #100272, #90591, #26434 ),
 ( #18321, #82499, #51171 ),
 ( #49591, #10194, #84094 ),
 ( #35045, #469, #33437 ),
 ( #70578, #52785, #60375 ),
 ( #85156, #29105, #61432 ),
 ( #13370, #19945, #12843 ),
 ( #37174, #93250, #78638 ),
 ( #21005, #28551, #70035 ),
 ( #86247, #77061, #4773 ),
 ( #11784, #77603, #53329 ),
 ( #19413, #52247, #45762 ),
 ( #94326, #11245, #95377 ),
 ( #20491, #62486, #78124 ),
 ( #3177, #44174, #53845 ),
 ( #36123, #101346, #2632 ),
 ( #76521, #61973, #101867 ),
 ( #68992, #28027, #60896 ),
 ( #102939, #4240, #93784 ),
 ( #54349, #94864, #86776 ),
 ( #12320, #102401, #103465 ),
 ( #21513, #29614, #37715 ),
 ( #87291, #35578, #68451 ),
 ( #45245, #85707, #27500 ),
 ( #44714, #3721, #36651 ),
 ( #69516, #46818, #89419 ),
 ( #6338, #47863, #48401 ),
 ( #72680, #71614, #38231 ),
 ( #96967, #72158, #73195 ),
 ( #97477, #65127, #22585 ),
 ( #7407, #57021, #15511 ),
 ( #105066, #87825, #98024 ),
 ( #63015, #71095, #103985 ),
 ( #89935, #79715, #81291 ),
 ( #39280, #80770, #40320 ),
 ( #32247, #14967, #38743 ),
 ( #104516, #24177, #88356 ),
 ( #30127, #106098, #23102 ),
 ( #46297, #79186, #30668 ),
 ( #31722, #6885, #5311 ),
 ( #95913, #64607, #22037 ) ),
 .UNSPECIFIED., .F., .F., .F. ) 
 B_SPLINE_SURFACE_WITH_KNOTS ( ( 4, 2, 2, 2, 2, 2, 2, 2, 2, 2, 2, 2, 2, 2, 2, 2, 2, 2, 2, 2, 2, 2, 2, 2, 2, 2, 2, 2, 2, 2, 2, 2, 2, 2, 2, 2, 2, 2, 2, 2, 2, 2, 2, 2, 2, 4 ),
 ( 3, 3 ),
 ( 0.06669982031955556945, 0.06876509657217773352, 0.06979773469848882250, 0.07083037282479989760, 0.07289564907742207556, 0.07392828720373315066, 0.07496092533004423963, 0.07702620158266640371, 0.07805883970897749269, 0.07909147783528858167, 0.08115675408791074574, 0.08322203034053290982, 0.08425466846684398492, 0.08528730659315507390, 0.08735258284577723797, 0.08838522097208832695, 0.08941785909839941593, 0.09148313535102158001, 0.09251577347733266898, 0.09354841160364374408, 0.09561368785626592204, 0.09664632598257699714, 0.09767896410888808612, 0.09974424036151025019, 0.1007768784878213253, 0.1018095166141324143, 0.1038747928667545783, 0.1059400691193767563, 0.1069727072456878314, 0.1080053453719989204, 0.1100706216246210845, 0.1111032597509321734, 0.1121358978772432624, 0.1142011741298654265, 0.1152338122561765155, 0.1162664503824875906, 0.1172990885087986657, 0.1183317266351097546, 0.1203970028877319187, 0.1224622791403540967, 0.1245275553929762608, 0.1255601935192873497, 0.1265928316455984248, 0.1286581078982206028, 0.1307233841508427807, 0.1327886604034649309 ),
 ( 0.000000000000000000, 1.000000000000000000 ),
 .UNSPECIFIED. ) 
 GEOMETRIC_REPRESENTATION_ITEM ( )  RATIONAL_B_SPLINE_SURFACE ( (
 ( 1.000000000000000000, 0.7574005004452292189, 1.000000000000000000),
 ( 1.000000000000000000, 0.7677881811269363643, 1.000000000000000000),
 ( 1.000000000000000000, 0.7789318350104040833, 1.000000000000000000),
 ( 1.000000000000000000, 0.7960806233368639129, 1.000000000000000000),
 ( 1.000000000000000000, 0.8018814668295082271, 1.000000000000000000),
 ( 1.000000000000000000, 0.8133644828828667794, 1.000000000000000000),
 ( 1.000000000000000000, 0.8190665470845299723, 1.000000000000000000),
 ( 1.000000000000000000, 0.8359369182568276990, 1.000000000000000000),
 ( 1.000000000000000000, 0.8468678900967679946, 1.000000000000000000),
 ( 1.000000000000000000, 0.8623942012808557545, 1.000000000000000000),
 ( 1.000000000000000000, 0.8674321864558991457, 1.000000000000000000),
 ( 1.000000000000000000, 0.8770051489341853523, 1.000000000000000000),
 ( 1.000000000000000000, 0.8815607036504458094, 1.000000000000000000),
 ( 1.000000000000000000, 0.8944702760352207793, 1.000000000000000000),
 ( 1.000000000000000000, 0.9020741755135933682, 1.000000000000000000),
 ( 1.000000000000000000, 0.9116398635700204700, 1.000000000000000000),
 ( 1.000000000000000000, 0.9145203804056111219, 1.000000000000000000),
 ( 1.000000000000000000, 0.9195812072905432677, 1.000000000000000000),
 ( 1.000000000000000000, 0.9216946987500304056, 1.000000000000000000),
 ( 1.000000000000000000, 0.9268367359168875330, 1.000000000000000000),
 ( 1.000000000000000000, 0.9286336546224613908, 1.000000000000000000),
 ( 1.000000000000000000, 0.9286071640124593518, 1.000000000000000000),
 ( 1.000000000000000000, 0.9267923817204344328, 1.000000000000000000),
 ( 1.000000000000000000, 0.9216310222028860633, 1.000000000000000000),
 ( 1.000000000000000000, 0.9194923251911391038, 1.000000000000000000),
 ( 1.000000000000000000, 0.9144746405666180911, 1.000000000000000000),
 ( 1.000000000000000000, 0.9116205049900496515, 1.000000000000000000),
 ( 1.000000000000000000, 0.9021468917526797027, 1.000000000000000000),
 ( 1.000000000000000000, 0.8946191197500281689, 1.000000000000000000),
 ( 1.000000000000000000, 0.8818899456451816388, 1.000000000000000000),
 ( 1.000000000000000000, 0.8773890157683175151, 1.000000000000000000),
 ( 1.000000000000000000, 0.8680974434632235948, 1.000000000000000000),
 ( 1.000000000000000000, 0.8632987000236833630, 1.000000000000000000),
 ( 1.000000000000000000, 0.8485654811955887222, 1.000000000000000000),
 ( 1.000000000000000000, 0.8382874571751192105, 1.000000000000000000),
 ( 1.000000000000000000, 0.8227376552933685083, 1.000000000000000000),
 ( 1.000000000000000000, 0.8175323482194468694, 1.000000000000000000),
 ( 1.000000000000000000, 0.8073811642434209901, 1.000000000000000000),
 ( 1.000000000000000000, 0.8024119013038333303, 1.000000000000000000),
 ( 1.000000000000000000, 0.7880089399916923032, 1.000000000000000000),
 ( 1.000000000000000000, 0.7790711632268805253, 1.000000000000000000),
 ( 1.000000000000000000, 0.7675359669597019430, 1.000000000000000000),
 ( 1.000000000000000000, 0.7639873508355347065, 1.000000000000000000),
 ( 1.000000000000000000, 0.7577827882268577397, 1.000000000000000000),
 ( 1.000000000000000000, 0.7551371035826408562, 1.000000000000000000),
 ( 1.000000000000000000, 0.7486932950123758035, 1.000000000000000000),
 ( 1.000000000000000000, 0.7463960882512324924, 1.000000000000000000),
 ( 1.000000000000000000, 0.7463222396104609579, 1.000000000000000000),
 ( 1.000000000000000000, 0.7468675288289394754, 1.000000000000000000),
 ( 1.000000000000000000, 0.7490620983608700101, 1.000000000000000000),
 ( 1.000000000000000000, 0.7507019908674972264, 1.000000000000000000),
 ( 1.000000000000000000, 0.7570958978920665494, 1.000000000000000000),
 ( 1.000000000000000000, 0.7633320146645002913, 1.000000000000000000),
 ( 1.000000000000000000, 0.7788212728674728247, 1.000000000000000000),
 ( 1.000000000000000000, 0.7878352555929534207, 1.000000000000000000),
 ( 1.000000000000000000, 0.8023450074323924541, 1.000000000000000000),
 ( 1.000000000000000000, 0.8073489187299826009, 1.000000000000000000),
 ( 1.000000000000000000, 0.8175636883870323057, 1.000000000000000000),
 ( 1.000000000000000000, 0.8227765755982912044, 1.000000000000000000),
 ( 1.000000000000000000, 0.8383040332954234675, 1.000000000000000000),
 ( 1.000000000000000000, 0.8485844023486135423, 1.000000000000000000),
 ( 1.000000000000000000, 0.8633419897287184508, 1.000000000000000000),
 ( 1.000000000000000000, 0.8681522541980656316, 1.000000000000000000),
 ( 1.000000000000000000, 0.8774719602938952923, 1.000000000000000000),
 ( 1.000000000000000000, 0.8819611993470838351, 1.000000000000000000),
 ( 1.000000000000000000, 0.8946520234114340164, 1.000000000000000000),
 ( 1.000000000000000000, 0.9021503839376829870, 1.000000000000000000),
 ( 1.000000000000000000, 0.9115857724357809833, 1.000000000000000000),
 ( 1.000000000000000000, 0.9144281988544517015, 1.000000000000000000),
 ( 1.000000000000000000, 0.9194277157626919994, 1.000000000000000000),
 ( 1.000000000000000000, 0.9215935472969858377, 1.000000000000000000),
 ( 1.000000000000000000, 0.9250730986170641046, 1.000000000000000000),
 ( 1.000000000000000000, 0.9263961809546490400, 1.000000000000000000),
 ( 1.000000000000000000, 0.9281725017696547120, 1.000000000000000000),
 ( 1.000000000000000000, 0.9286249391977352552, 1.000000000000000000),
 ( 1.000000000000000000, 0.9286114671366180184, 1.000000000000000000),
 ( 1.000000000000000000, 0.9268058022047847011, 1.000000000000000000),
 ( 1.000000000000000000, 0.9199284077393417025, 1.000000000000000000),
 ( 1.000000000000000000, 0.9147782303380489477, 1.000000000000000000),
 ( 1.000000000000000000, 0.9019685211012331560, 1.000000000000000000),
 ( 1.000000000000000000, 0.8943002565130824255, 1.000000000000000000),
 ( 1.000000000000000000, 0.8812085285205289997, 1.000000000000000000),
 ( 1.000000000000000000, 0.8765859265514783782, 1.000000000000000000),
 ( 1.000000000000000000, 0.8669906351561719182, 1.000000000000000000),
 ( 1.000000000000000000, 0.8620032267436350537, 1.000000000000000000),
 ( 1.000000000000000000, 0.8465577714266654397, 1.000000000000000000),
 ( 1.000000000000000000, 0.8356129422299747311, 1.000000000000000000),
 ( 1.000000000000000000, 0.8129121367137768228, 1.000000000000000000),
 ( 1.000000000000000000, 0.8014017695925140794, 1.000000000000000000),
 ( 1.000000000000000000, 0.7788404441292630098, 1.000000000000000000),
 ( 1.000000000000000000, 0.7677783875764762067, 1.000000000000000000),
 ( 1.000000000000000000, 0.7574005004452295520, 1.000000000000000000) ) ) 
 REPRESENTATION_ITEM ( '' )  SURFACE ( )  );
#12679 = CYLINDRICAL_SURFACE ( 'NONE', #75616, 4.000000000000000888 ) ;
#12680 = CARTESIAN_POINT ( 'NONE',  ( 5.175365594622103771, 41.93912328290134184, -69.86374199123662265 ) ) ;
#12681 = CARTESIAN_POINT ( 'NONE',  ( 27.10511071441198894, 36.88665068479745912, 7.556984339683237906 ) ) ;
#12682 = DIRECTION ( 'NONE',  ( 0.000000000000000000, -1.000000000000000000, 0.000000000000000000 ) ) ;
#12683 = VECTOR ( 'NONE', #34215, 1000.000000000000000 ) ;
#12684 = CARTESIAN_POINT ( 'NONE',  ( 16.96105790261473345, 43.64123098144456492, -4.188549414824395356 ) ) ;
#12685 = VERTEX_POINT ( 'NONE', #104240 ) ;
#12686 = LINE ( 'NONE', #76356, #64469 ) ;
#12688 = CARTESIAN_POINT ( 'NONE',  ( 26.36601463560733194, -46.43337520415909125, 33.26297091638029713 ) ) ;
#12687 = CARTESIAN_POINT ( 'NONE',  ( -58.28906562901213562, -14.21045842199421294, 78.48115787639689245 ) ) ;
#12689 = CARTESIAN_POINT ( 'NONE',  ( 39.18206537991729022, 57.18445727710330573, 19.59103268995865221 ) ) ;
#12690 = VERTEX_POINT ( 'NONE', #71873 ) ;
#12691 = EDGE_CURVE ( 'NONE', #59308, #66067, #45160, .T. ) ;
#12692 = UNCERTAINTY_MEASURE_WITH_UNIT (LENGTH_MEASURE( 1.000000000000000082E-05 ), #65789, 'distance_accuracy_value', 'NONE');
#12693 = VERTEX_POINT ( 'NONE', #7656 ) ;
#12694 = CARTESIAN_POINT ( 'NONE',  ( -1.650803255657547375, -4.285714285714296246, -25.22241582816893057 ) ) ;
#12695 =( NAMED_UNIT ( * ) SI_UNIT ( $, .STERADIAN. ) SOLID_ANGLE_UNIT ( ) );
#12696 = CARTESIAN_POINT ( 'NONE',  ( -13.38905016575103168, -54.52753545736232610, 31.09099597011418226 ) ) ;
#12697 = PRESENTATION_LAYER_ASSIGNMENT (  '', '', ( #36844 ) ) ;
#12698 = CARTESIAN_POINT ( 'NONE',  ( -32.93513049338658760, 465.6726574193328361, 10.66039033145138326 ) ) ;
#12699 = CARTESIAN_POINT ( 'NONE',  ( 29.98176661990081371, 1.340359594676612611E-15, 0.000000000000000000 ) ) ;
#12700 = FACE_OUTER_BOUND ( 'NONE', #66154, .T. ) ;
#12701 = VERTEX_POINT ( 'NONE', #79961 ) ;
#12702 = CARTESIAN_POINT ( 'NONE',  ( 98.43072231738531741, -29.99999999999995737, 140.5709701892116072 ) ) ;
#12703 = CARTESIAN_POINT ( 'NONE',  ( -10.89640271560199913, 9.008026361043889096, 10.01173798417218741 ) ) ;
#12704 = CIRCLE ( 'NONE', #90240, 4.000000000000007105 ) ;
#12705 = CARTESIAN_POINT ( 'NONE',  ( 1.749814335632528417, 15.56087475005694643, 9.852235012526419311 ) ) ;
#12706 = ADVANCED_FACE ( 'NONE', ( #38997 ), #51022, .F. ) ;
#12707 = CARTESIAN_POINT ( 'NONE',  ( 81.57847679930965512, -29.99999999999999645, -5.537912221079761999 ) ) ;
#12708 = AXIS2_PLACEMENT_3D ( 'NONE', #104333, #70397, #103296 ) ;
#12709 =( BOUNDED_SURFACE ( )  B_SPLINE_SURFACE ( 3, 2, ( 
 ( #3638, #69441, #12765 ),
 ( #85083, #4166, #84556 ),
 ( #11167, #76440, #94243 ),
 ( #12239, #10640, #94788 ) ),
 .UNSPECIFIED., .F., .F., .F. ) 
 B_SPLINE_SURFACE_WITH_KNOTS ( ( 4, 4 ),
 ( 3, 3 ),
 ( 1.301042606982605321E-17, 0.002002951328326080076 ),
 ( 0.000000000000000000, 1.000000000000000000 ),
 .UNSPECIFIED. ) 
 GEOMETRIC_REPRESENTATION_ITEM ( )  RATIONAL_B_SPLINE_SURFACE ( (
 ( 1.000000000000000000, 0.7699558187665428433, 1.000000000000000000),
 ( 1.000000000000000000, 0.7788467038584532265, 1.000000000000000000),
 ( 1.000000000000000000, 0.7876570642905753594, 1.000000000000000000),
 ( 1.000000000000000000, 0.7964405967476247961, 1.000000000000000000) ) ) 
 REPRESENTATION_ITEM ( '' )  SURFACE ( )  );
#12710 = ADVANCED_FACE ( 'NONE', ( #80486 ), #6712, .T. ) ;
#12711 = DIRECTION ( 'NONE',  ( 0.000000000000000000, -1.000000000000000000, 0.000000000000000000 ) ) ;
#12712 = ORIENTED_EDGE ( 'NONE', *, *, #43450, .F. ) ;
#12713 = B_SPLINE_CURVE_WITH_KNOTS ( 'NONE', 3,
 ( #44370, #37903, #69711, #103659, #62685, #12510, #79378, #102604 ),
 .UNSPECIFIED., .F., .F.,
 ( 4, 2, 2, 4 ),
 ( 0.004673709593152160051, 0.005837709341827647738, 0.007001709090503134558, 0.009329708587854108198 ),
 .UNSPECIFIED. ) ;
#12714 = B_SPLINE_CURVE_WITH_KNOTS ( 'NONE', 3,
 ( #70814, #87535, #29853, #13618 ),
 .UNSPECIFIED., .F., .F.,
 ( 4, 4 ),
 ( 0.000000000000000000, 0.4999999999999996114 ),
 .UNSPECIFIED. ) ;
#12715 = ORIENTED_EDGE ( 'NONE', *, *, #104878, .T. ) ;
#12716 = ORIENTED_EDGE ( 'NONE', *, *, #104489, .F. ) ;
#12717 = CARTESIAN_POINT ( 'NONE',  ( -6.750000000000018652, 11.69134295108991317, 0.000000000000000000 ) ) ;
#12718 = DIRECTION ( 'NONE',  ( 8.160201061530222974E-17, 0.7456561006171790185, -0.6663309835302448914 ) ) ;
#12719 = DIRECTION ( 'NONE',  ( -1.000000000000000000, -1.224606353822377258E-16, -0.000000000000000000 ) ) ;
#12720 = LINE ( 'NONE', #14303, #51445 ) ;
#12721 = SURFACE_STYLE_FILL_AREA ( #21917 ) ;
#12722 = CARTESIAN_POINT ( 'NONE',  ( 5.290067270632397012, 54.20842449845690680, 6.031152949374294359 ) ) ;
#12723 = DIRECTION ( 'NONE',  ( 0.000000000000000000, -1.000000000000000000, 0.000000000000000000 ) ) ;
#12724 = ORIENTED_EDGE ( 'NONE', *, *, #72401, .F. ) ;
#12725 = CARTESIAN_POINT ( 'NONE',  ( 8.737863884121436442, 48.00000000000000000, -79.96381019768851672 ) ) ;
#12726 = VERTEX_POINT ( 'NONE', #72921 ) ;
#12727 = CARTESIAN_POINT ( 'NONE',  ( -5.856955515201466511, -61.21710941119133764, 1.326217528971461279 ) ) ;
#12728 = DIRECTION ( 'NONE',  ( -1.000000000000000000, -1.224606353822377258E-16, -0.000000000000000000 ) ) ;
#12729 = CARTESIAN_POINT ( 'NONE',  ( 6.337538409676599689E-15, 7.746009256456446224, 51.75000000000000711 ) ) ;
#12730 = CARTESIAN_POINT ( 'NONE',  ( 23.98803262824752380, 303.9357235565888686, 10.17341870318404418 ) ) ;
#12731 = CARTESIAN_POINT ( 'NONE',  ( 0.2480848965973885545, 295.3545306174075904, -10.00000000001854694 ) ) ;
#12732 = CARTESIAN_POINT ( 'NONE',  ( 63.70598834999947968, -49.91021569056980667, 87.81644791561008390 ) ) ;
#12733 = VECTOR ( 'NONE', #57975, 1000.000000000000000 ) ;
#12734 = VERTEX_POINT ( 'NONE', #26044 ) ;
#12735 = CARTESIAN_POINT ( 'NONE',  ( -2.617478843592799365, -3.000000000000003109, -94.73972676668314818 ) ) ;
#12736 = CARTESIAN_POINT ( 'NONE',  ( -57.73274652580165878, -37.01956164141905958, -34.70034953516653786 ) ) ;
#12737 = DIRECTION ( 'NONE',  ( 0.000000000000000000, 0.09744402424415131436, 0.9952410070626639405 ) ) ;
#12738 = VECTOR ( 'NONE', #34405, 1000.000000000000000 ) ;
#12739 = CARTESIAN_POINT ( 'NONE',  ( -9.180591118468083067, 51.37400502630696053, 3.869057452854628654 ) ) ;
#12740 =( GEOMETRIC_REPRESENTATION_CONTEXT ( 3 ) GLOBAL_UNCERTAINTY_ASSIGNED_CONTEXT ( ( #83395 ) ) GLOBAL_UNIT_ASSIGNED_CONTEXT ( ( #43666, #60413, #45800 ) ) REPRESENTATION_CONTEXT ( 'NONE', 'WORKASPACE' ) );
#12741 = ORIENTED_EDGE ( 'NONE', *, *, #38225, .T. ) ;
#12742 =( LENGTH_UNIT ( ) NAMED_UNIT ( * ) SI_UNIT ( .MILLI., .METRE. ) );
#12743 = DIRECTION ( 'NONE',  ( -1.000000000000000000, -0.000000000000000000, -0.000000000000000000 ) ) ;
#12744 = FILL_AREA_STYLE_COLOUR ( '', #519 ) ;
#12745 = DIRECTION ( 'NONE',  ( -1.000000000000000000, -1.224606353822377258E-16, -0.000000000000000000 ) ) ;
#12746 = PLANE ( 'NONE',  #42707 ) ;
#12747 = EDGE_CURVE ( 'NONE', #36282, #24510, #74524, .T. ) ;
#12748 = CARTESIAN_POINT ( 'NONE',  ( 0.000000000000000000, -30.00000000000000000, 8.000000000000000000 ) ) ;
#12749 = DIRECTION ( 'NONE',  ( 1.000000000000000000, 1.224606353822377258E-16, 0.000000000000000000 ) ) ;
#12750 = CARTESIAN_POINT ( 'NONE',  ( 86.49757777737477227, -42.81999918254669524, 189.1461807675101738 ) ) ;
#12751 = CARTESIAN_POINT ( 'NONE',  ( -5.221552941240854118, 7.001034474524052698, -27.46988742860714794 ) ) ;
#12752 = CARTESIAN_POINT ( 'NONE',  ( -4.504915916856424118, 9.260147447997045589, 5.000000000000000000 ) ) ;
#12753 = CARTESIAN_POINT ( 'NONE',  ( 7.986452802927059835, -6.026902423081146765, 0.5332468218996346820 ) ) ;
#12754 = DIRECTION ( 'NONE',  ( 0.000000000000000000, -1.000000000000000000, 0.000000000000000000 ) ) ;
#12755 = CARTESIAN_POINT ( 'NONE',  ( 6.162888688655344893, -3.752776749732565253, 6.499999999999999112 ) ) ;
#12756 = DIRECTION ( 'NONE',  ( -1.000000000000000000, -1.224606353822377258E-16, -0.000000000000000000 ) ) ;
#12757 = CARTESIAN_POINT ( 'NONE',  ( -97.94054855731607745, -30.00000000000000355, 137.0914856574075884 ) ) ;
#12758 = EDGE_CURVE ( 'NONE', #87964, #54573, #58379, .T. ) ;
#12759 = COLOUR_RGB ( '', 0.31764706, 0.68627451, 0.89019608) ;
#12760 = CARTESIAN_POINT ( 'NONE',  ( 28.06569167955347055, -57.67949617772409709, 44.31129476918351884 ) ) ;
#12762 = CARTESIAN_POINT ( 'NONE',  ( 13.76424046522695122, 304.5457540960956067, -10.06505265514019065 ) ) ;
#12761 = DIRECTION ( 'NONE',  ( -1.000000000000000000, -1.224606353822377258E-16, -0.000000000000000000 ) ) ;
#12763 = CARTESIAN_POINT ( 'NONE',  ( -42.00498316483441386, 460.5526920487833991, 2.538979661987313730 ) ) ;
#12764 = CARTESIAN_POINT ( 'NONE',  ( -19.16958797051855612, 50.00000000000000000, 60.35583957385809128 ) ) ;
#12765 = CARTESIAN_POINT ( 'NONE',  ( -43.41290683822509067, 487.0833545439620593, 7.569976829064880341 ) ) ;
#12766 = DIRECTION ( 'NONE',  ( -1.000000000000000000, -0.000000000000000000, -0.000000000000000000 ) ) ;
#12767 = VECTOR ( 'NONE', #82008, 1000.000000000000000 ) ;
#12768 =( NAMED_UNIT ( * ) PLANE_ANGLE_UNIT ( ) SI_UNIT ( $, .RADIAN. ) );
#12769 = EDGE_CURVE ( 'NONE', #40311, #31698, #49236, .T. ) ;
#12770 = CARTESIAN_POINT ( 'NONE',  ( -17.49999999999999645, -2.499999999999999556, 25.00000000000000000 ) ) ;
#12771 = AXIS2_PLACEMENT_3D ( 'NONE', #83908, #82312, #8422 ) ;
#12772 = FILL_AREA_STYLE_COLOUR ( '', #97009 ) ;
#12773 = ORIENTED_EDGE ( 'NONE', *, *, #35328, .T. ) ;
#12774 = CARTESIAN_POINT ( 'NONE',  ( 40.72262571688381882, 485.0559992917314389, -4.084589505546340149 ) ) ;
#12775 = CARTESIAN_POINT ( 'NONE',  ( -2.691542343445430419, -49.46338946410779869, 103.4273627254628423 ) ) ;
#12776 = CARTESIAN_POINT ( 'NONE',  ( -18.71324380705060975, -25.55240577479218445, 28.53076995190656362 ) ) ;
#12777 = ADVANCED_FACE ( 'NONE', ( #1144 ), #61876, .T. ) ;
#12779 = CARTESIAN_POINT ( 'NONE',  ( 0.000000000000000000, 0.000000000000000000, 0.000000000000000000 ) ) ;
#12778 = CARTESIAN_POINT ( 'NONE',  ( -86.14485785028760745, -59.99999999999995026, 15.73779263674076212 ) ) ;
#12780 = ORIENTED_EDGE ( 'NONE', *, *, #26095, .F. ) ;
#12781 = ORIENTED_EDGE ( 'NONE', *, *, #4254, .F. ) ;
#12782 = CARTESIAN_POINT ( 'NONE',  ( -13.43739347944073792, 42.84543662633798533, -92.02663817126700962 ) ) ;
#12783 = ADVANCED_FACE ( 'NONE', ( #67521 ), #104894, .T. ) ;
#12784 = CARTESIAN_POINT ( 'NONE',  ( 16.01236629286577084, 3.722328191965672772, -0.3359674915983867916 ) ) ;
#12785 = CARTESIAN_POINT ( 'NONE',  ( -1.008312940004822522, 54.10577091759437707, -8.243645369945518553 ) ) ;
#12786 = ORIENTED_EDGE ( 'NONE', *, *, #69541, .F. ) ;
#12787 = CARTESIAN_POINT ( 'NONE',  ( -12.99999999999996625, -1.778091562876227272E-14, 0.000000000000000000 ) ) ;
#12788 = DIRECTION ( 'NONE',  ( 0.000000000000000000, 1.000000000000000000, 0.000000000000000000 ) ) ;
#12789 = CARTESIAN_POINT ( 'NONE',  ( 104.6932645544404750, -60.15174171467819519, 188.9584721480441658 ) ) ;
#12791 = CARTESIAN_POINT ( 'NONE',  ( -28.99999999999998934, 0.000000000000000000, 0.000000000000000000 ) ) ;
#12790 = FACE_OUTER_BOUND ( 'NONE', #104299, .T. ) ;
#12792 = EDGE_CURVE ( 'NONE', #84655, #79894, #59287, .T. ) ;
#12793 = VERTEX_POINT ( 'NONE', #10323 ) ;
#12795 = EDGE_CURVE ( 'NONE', #63010, #43496, #22053, .T. ) ;
#12794 =( GEOMETRIC_REPRESENTATION_CONTEXT ( 3 ) GLOBAL_UNCERTAINTY_ASSIGNED_CONTEXT ( ( #52636 ) ) GLOBAL_UNIT_ASSIGNED_CONTEXT ( ( #6914, #82404, #73227 ) ) REPRESENTATION_CONTEXT ( 'NONE', 'WORKASPACE' ) );
#12796 = ORIENTED_EDGE ( 'NONE', *, *, #30006, .F. ) ;
#12797 = VERTEX_POINT ( 'NONE', #51847 ) ;
#12798 = CARTESIAN_POINT ( 'NONE',  ( 23.15833479403198680, 305.7594302588016149, 10.13509876207107219 ) ) ;
#12799 = AXIS2_PLACEMENT_3D ( 'NONE', #46454, #29771, #69671 ) ;
#12800 = DIRECTION ( 'NONE',  ( 0.000000000000000000, -1.000000000000000000, 0.000000000000000000 ) ) ;
#12801 = CARTESIAN_POINT ( 'NONE',  ( -14.84266821126070468, 4.606643506668206989, -5.685020543978184904 ) ) ;
#12802 = EDGE_LOOP ( 'NONE', ( #72566, #68423, #38087, #7104, #2271 ) ) ;
#12803 = PRODUCT_DEFINITION_FORMATION_WITH_SPECIFIED_SOURCE ( 'ANY', '', #43795, .NOT_KNOWN. ) ;
#12804 = CARTESIAN_POINT ( 'NONE',  ( 25.59999999999999787, 3.309500000000003439, 4.052968581778167743E-16 ) ) ;
#12805 = CARTESIAN_POINT ( 'NONE',  ( -6.487288085721814035, 4.944722507271262835, -4.967589210256464050 ) ) ;
#12806 = AXIS2_PLACEMENT_3D ( 'NONE', #52263, #85177, #17798 ) ;
#12807 = CARTESIAN_POINT ( 'NONE',  ( -94.62662591020489344, -60.00000000000486011, -13.08416834391727512 ) ) ;
#12808 = CARTESIAN_POINT ( 'NONE',  ( 7.744329845603314944, -68.46288230153457732, -2.018701143083234228 ) ) ;
#12809 = CARTESIAN_POINT ( 'NONE',  ( 88.33048940779720226, -60.00000000001467271, -24.74029235082771194 ) ) ;
#12810 = CARTESIAN_POINT ( 'NONE',  ( 11.93415444004271464, -5.000000000000000000, 11.28339104396314774 ) ) ;
#12811 = CARTESIAN_POINT ( 'NONE',  ( -6.798790223523980103, 41.26122158754633062, -58.42041485083363028 ) ) ;
#12813 = CARTESIAN_POINT ( 'NONE',  ( 11.56881156677787814, -60.35887278456814187, 33.98181144888569349 ) ) ;
#12812 = CARTESIAN_POINT ( 'NONE',  ( -107.3073691194147443, -59.99999999999994316, 109.8427349246714613 ) ) ;
#12814 = LINE ( 'NONE', #78092, #70608 ) ;
#12815 = CARTESIAN_POINT ( 'NONE',  ( -48.33525847096109374, -42.98408013933313754, 49.20298293444408699 ) ) ;
#12816 = LINE ( 'NONE', #71064, #31524 ) ;
#12817 = VERTEX_POINT ( 'NONE', #1696 ) ;
#12818 = CARTESIAN_POINT ( 'NONE',  ( 38.09999999999998721, 4.475777889183789793E-16, -3.309499999999999886 ) ) ;
#12819 = DIRECTION ( 'NONE',  ( 0.000000000000000000, 0.000000000000000000, 1.000000000000000000 ) ) ;
#12820 = DIRECTION ( 'NONE',  ( 0.000000000000000000, -0.000000000000000000, 1.000000000000000000 ) ) ;
#12821 = VERTEX_POINT ( 'NONE', #58354 ) ;
#12822 = VERTEX_POINT ( 'NONE', #26563 ) ;
#12823 = CARTESIAN_POINT ( 'NONE',  ( 90.02033453618058445, -29.99999999997217159, -9.423705806685745756 ) ) ;
#12824 = CARTESIAN_POINT ( 'NONE',  ( 3.454253436624922902, -49.15858197120396511, 103.7259032015043090 ) ) ;
#12825 = CARTESIAN_POINT ( 'NONE',  ( 6.914390625618707986, 41.80417612998946453, -59.57688307474369793 ) ) ;
#12826 = CARTESIAN_POINT ( 'NONE',  ( 59.23741894013591036, 42.00000000000000711, -7.754160006507188285 ) ) ;
#12827 = CARTESIAN_POINT ( 'NONE',  ( 97.98369069848891399, -30.00000000000000000, 190.5473186706665842 ) ) ;
#12828 = ADVANCED_FACE ( 'NONE', ( #18452 ), #23936, .T. ) ;
#12829 = DIRECTION ( 'NONE',  ( 0.7071067811865431318, 8.659560562354987092E-17, 0.7071067811865517916 ) ) ;
#12830 = EDGE_LOOP ( 'NONE', ( #11321, #46813, #34060, #80981 ) ) ;
#12831 = CIRCLE ( 'NONE', #21502, 4.000000000000000888 ) ;
#12832 = ORIENTED_EDGE ( 'NONE', *, *, #10656, .T. ) ;
#12833 = ORIENTED_EDGE ( 'NONE', *, *, #99267, .T. ) ;
#12834 = CARTESIAN_POINT ( 'NONE',  ( 54.64156605188832572, -53.37664899715956324, 65.16901697101967272 ) ) ;
#12835 = LINE ( 'NONE', #21506, #52487 ) ;
#12836 = ADVANCED_FACE ( 'NONE', ( #69122 ), #28153, .F. ) ;
#12837 = CARTESIAN_POINT ( 'NONE',  ( 13.68764148674883430, 294.5450735065955996, 9.871802096439328267 ) ) ;
#12838 = ORIENTED_EDGE ( 'NONE', *, *, #73620, .T. ) ;
#12839 = CARTESIAN_POINT ( 'NONE',  ( -81.87992184396165385, -38.35665926185938446, -25.31435275803445251 ) ) ;
#12840 = VERTEX_POINT ( 'NONE', #71217 ) ;
#12841 = PLANE ( 'NONE',  #48309 ) ;
#12842 = CARTESIAN_POINT ( 'NONE',  ( 105.2162103339291264, -38.38992852922254428, 197.2646886752842761 ) ) ;
#12843 = CARTESIAN_POINT ( 'NONE',  ( 12.42143139619339998, 22.57321393022593981, 6.089946764847198324 ) ) ;
#12844 = COLOUR_RGB ( '', 0.31764706, 0.68627451, 0.89019608) ;
#12845 = CARTESIAN_POINT ( 'NONE',  ( 83.67122112447796667, -45.28247169777900893, 12.12148471621375556 ) ) ;
#12846 = CARTESIAN_POINT ( 'NONE',  ( 0.5805565836007618996, 3.752776749732569250, 6.499999999999997335 ) ) ;
#12847 = STYLED_ITEM ( 'NONE', ( #98260 ), #27947 ) ;
#12848 = CARTESIAN_POINT ( 'NONE',  ( 40.93067809230030463, 381.6511011474903512, 26.75444701802409497 ) ) ;
#12849 = AXIS2_PLACEMENT_3D ( 'NONE', #65467, #8278, #16372 ) ;
#12850 = CARTESIAN_POINT ( 'NONE',  ( 72.85555555555556850, 6.915964383211875250E-15, 0.000000000000000000 ) ) ;
#12851 = MECHANICAL_DESIGN_GEOMETRIC_PRESENTATION_REPRESENTATION (  '', ( #33589 ), #35299 ) ;
#12852 = CARTESIAN_POINT ( 'NONE',  ( 0.000000000000000000, 45.50000000000000711, 0.000000000000000000 ) ) ;
#12853 =( NAMED_UNIT ( * ) PLANE_ANGLE_UNIT ( ) SI_UNIT ( $, .RADIAN. ) );
#12854 = ORIENTED_EDGE ( 'NONE', *, *, #18507, .F. ) ;
#12855 = EDGE_CURVE ( 'NONE', #81401, #1618, #31331, .T. ) ;
#12856 = CARTESIAN_POINT ( 'NONE',  ( -5.656854249492379694, -10.62500000409677092, -5.656854249492380582 ) ) ;
#12857 = CARTESIAN_POINT ( 'NONE',  ( 39.44615384615384812, -4.171999999999999709, 0.000000000000000000 ) ) ;
#12858 = CARTESIAN_POINT ( 'NONE',  ( -26.78447284414440333, 36.99601554321866814, 7.587964289499315562 ) ) ;
#12859 = ORIENTED_EDGE ( 'NONE', *, *, #98205, .T. ) ;
#12860 = CARTESIAN_POINT ( 'NONE',  ( -23.15282783083631202, 305.4172466244119732, -8.878502953368174744 ) ) ;
#12861 = CARTESIAN_POINT ( 'NONE',  ( -29.20681473986357446, 312.6947595059442051, 12.31531419807666872 ) ) ;
#12862 = CARTESIAN_POINT ( 'NONE',  ( -10.85300161404138031, -4.996537049337243630, -77.21885189817174933 ) ) ;
#12863 = CARTESIAN_POINT ( 'NONE',  ( 8.000000000000000000, -21.40624999999999289, -3.313708498984761608 ) ) ;
#12864 = CARTESIAN_POINT ( 'NONE',  ( 51.98481497594274714, -29.99999999999999645, 49.99891310834441782 ) ) ;
#12865 =( BOUNDED_CURVE ( )  B_SPLINE_CURVE ( 2, ( #2133, #99785, #56248, #48696, #89183, #6658, #81583, #72456, #74961 ),
 .UNSPECIFIED., .F., .F. ) 
 B_SPLINE_CURVE_WITH_KNOTS ( ( 3, 2, 2, 2, 3 ),
 ( 0.7205882352941177516, 0.7279411764705883137, 0.7352941176470589868, 0.7426470588235295489, 0.7500000000000001110 ),
 .UNSPECIFIED. ) 
 CURVE ( )  GEOMETRIC_REPRESENTATION_ITEM ( )  RATIONAL_B_SPLINE_CURVE ( ( 0.9999999999999988898, 0.9238795325112878487, 1.000000000000000000, 0.9238795325112867385, 1.000000000000000000, 0.9238795325112867385, 1.000000000000000000, 0.9238795325112856283, 1.000000000000001110 ) ) 
 REPRESENTATION_ITEM ( '' )  );
#12866 = ADVANCED_FACE ( 'NONE', ( #22168 ), #14864, .T. ) ;
#12867 = DIRECTION ( 'NONE',  ( -0.8191520442889881348, 1.003171929053520186E-16, 0.5735764363510513775 ) ) ;
#12868 = VERTEX_POINT ( 'NONE', #80358 ) ;
#12869 = CARTESIAN_POINT ( 'NONE',  ( 85.62023018141502462, -28.60500254207639159, 178.8567084087247849 ) ) ;
#12870 = CARTESIAN_POINT ( 'NONE',  ( 24.63846153846153797, 1.411358822780289120E-15, 0.000000000000000000 ) ) ;
#12871 = EDGE_CURVE ( 'NONE', #15319, #47413, #64727, .T. ) ;
#12872 = B_SPLINE_CURVE_WITH_KNOTS ( 'NONE', 3,
 ( #51910, #102600, #60568, #51374, #93979, #85907, #28752, #60044, #36840, #3908, #28219, #36318, #61088, #20133, #44911, #84289, #10383, #68659, #4429, #102058, #43822, #70234, #11439, #37369, #53517, #27691, #35781, #61635, #69187, #11981, #86444, #77797, #94526, #20678 ),
 .UNSPECIFIED., .F., .F.,
 ( 4, 2, 2, 2, 2, 2, 2, 2, 2, 2, 2, 2, 2, 2, 2, 2, 4 ),
 ( 1.409296014025916843E-17, 0.0007899309203816184607, 0.001579861840763222827, 0.002369792761144826759, 0.003159723681526431342, 0.003949654601908035925, 0.004739585522289639641, 0.005529516442671244224, 0.006319447363052848807, 0.007109378283434453390, 0.007899309203816057973, 0.008689240124197661688, 0.009479171044579265404, 0.01026910196496087085, 0.01105903288534247457, 0.01184896380572408002, 0.01263889472610568374 ),
 .UNSPECIFIED. ) ;
#12873 = SURFACE_SIDE_STYLE ('',( #88384 ) ) ;
#12874 = EDGE_LOOP ( 'NONE', ( #64962, #153, #91078, #96720 ) ) ;
#12875 = CARTESIAN_POINT ( 'NONE',  ( -93.88781582325293584, -52.71009071215733854, 86.64102402054331264 ) ) ;
#12876 = CARTESIAN_POINT ( 'NONE',  ( 47.33349330513379982, -4.000000000000000888, 4.898587196589416773E-16 ) ) ;
#12877 = DIRECTION ( 'NONE',  ( 0.000000000000000000, 0.000000000000000000, 1.000000000000000000 ) ) ;
#12878 = CARTESIAN_POINT ( 'NONE',  ( -30.92866670662964523, 8.704003156311230782, 40.98833526575327113 ) ) ;
#12879 = DIRECTION ( 'NONE',  ( 0.000000000000000000, -1.000000000000000000, 0.000000000000000000 ) ) ;
#12880 = AXIS2_PLACEMENT_3D ( 'NONE', #48816, #56912, #99500 ) ;
#12881 = EDGE_CURVE ( 'NONE', #51129, #84766, #37325, .T. ) ;
#12882 = CARTESIAN_POINT ( 'NONE',  ( 10.82237006604675145, -20.57234134931101011, 35.45079542051080779 ) ) ;
#12883 = FILL_AREA_STYLE_COLOUR ( '', #1410 ) ;
#12884 = CARTESIAN_POINT ( 'NONE',  ( 51.58436202480620381, -29.92082885799144876, 49.33144644358862507 ) ) ;
#12886 = CARTESIAN_POINT ( 'NONE',  ( -12.32115138270090249, 22.37014720597713335, 6.335230956775115274 ) ) ;
#12885 = FILL_AREA_STYLE ('',( #94905 ) ) ;
#12887 = CARTESIAN_POINT ( 'NONE',  ( 3.001409217434625187, 294.8245242021975514, -9.555569693282839339 ) ) ;
#12888 = CARTESIAN_POINT ( 'NONE',  ( -16.32725980561048829, 43.86428832234518183, -4.195806562069138046 ) ) ;
#12889 = CARTESIAN_POINT ( 'NONE',  ( 9.999999999999996447, 15.00000000000000000, -4.582575694955844270 ) ) ;
#12890 = FACE_OUTER_BOUND ( 'NONE', #103743, .T. ) ;
#12891 = CARTESIAN_POINT ( 'NONE',  ( -87.09641169487616708, -38.00000000000000000, 60.23192446987157211 ) ) ;
#12892 = ORIENTED_EDGE ( 'NONE', *, *, #63025, .T. ) ;
#12893 = CARTESIAN_POINT ( 'NONE',  ( -15.00905689107410090, -0.1007854530124032977, 15.00123387746082315 ) ) ;
#12894 = ADVANCED_FACE ( 'NONE', ( #38357 ), #56140, .F. ) ;
#12896 = CARTESIAN_POINT ( 'NONE',  ( 9.320906537292072969, -21.77036391677812688, -30.31143086060786374 ) ) ;
#12895 = CARTESIAN_POINT ( 'NONE',  ( 40.73953790046563483, -18.92596047533412573, -20.36976895023282097 ) ) ;
#12897 = CIRCLE ( 'NONE', #54243, 4.000000000000001776 ) ;
#12898 = ORIENTED_EDGE ( 'NONE', *, *, #6181, .F. ) ;
#12899 = CARTESIAN_POINT ( 'NONE',  ( 7.968863443239238009, 4.547634245050472757, -8.057411785091789014 ) ) ;
#12900 = CARTESIAN_POINT ( 'NONE',  ( 0.5805565836007643421, -3.752776749732575468, -6.499999999999999112 ) ) ;
#12901 = ORIENTED_EDGE ( 'NONE', *, *, #16673, .T. ) ;
#12902 = VECTOR ( 'NONE', #28418, 1000.000000000000000 ) ;
#12903 = EDGE_CURVE ( 'NONE', #59296, #80603, #101741, .T. ) ;
#12904 = CARTESIAN_POINT ( 'NONE',  ( 30.29857313018901266, 7.759641293511155169, -41.94607130693972152 ) ) ;
#12905 = CARTESIAN_POINT ( 'NONE',  ( -4.000000000000000000, 0.000000000000000000, -1.161000000000000032 ) ) ;
#12906 = AXIS2_PLACEMENT_3D ( 'NONE', #28222, #101545, #19612 ) ;
#12907 = CARTESIAN_POINT ( 'NONE',  ( -92.14734929965659660, -59.99999999999999289, 21.43942582026355836 ) ) ;
#12908 = EDGE_LOOP ( 'NONE', ( #86702, #2054, #15051, #77258, #61403, #88351, #86181 ) ) ;
#12909 = CARTESIAN_POINT ( 'NONE',  ( -1.816153886384274108, 42.00000000000000711, -59.31995585001073579 ) ) ;
#12910 = AXIS2_PLACEMENT_3D ( 'NONE', #99038, #11093, #18711 ) ;
#12911 = LINE ( 'NONE', #29682, #26460 ) ;
#12912 = CIRCLE ( 'NONE', #73200, 3.400000000000000355 ) ;
#12913 = CARTESIAN_POINT ( 'NONE',  ( -9.646083234704169840, 26.98709390976521405, -2.643797197754292672 ) ) ;
#12914 = AXIS2_PLACEMENT_3D ( 'NONE', #21853, #55746, #38554 ) ;
#12916 = DIRECTION ( 'NONE',  ( -1.000000000000000000, -1.224606353822377258E-16, -0.000000000000000000 ) ) ;
#12915 =( LENGTH_UNIT ( ) NAMED_UNIT ( * ) SI_UNIT ( .MILLI., .METRE. ) );
#12917 = CARTESIAN_POINT ( 'NONE',  ( -80.43218294797944168, -60.42267903133028284, 179.0676953134927203 ) ) ;
#12918 = ORIENTED_EDGE ( 'NONE', *, *, #73366, .T. ) ;
#12919 = VECTOR ( 'NONE', #9631, 1000.000000000000000 ) ;
#12920 = CARTESIAN_POINT ( 'NONE',  ( -15.29468310206709347, -0.000000000000000000, 7.540179673766518320 ) ) ;
#12921 = ORIENTED_EDGE ( 'NONE', *, *, #24339, .F. ) ;
#12922 = VECTOR ( 'NONE', #42197, 1000.000000000000000 ) ;
#12923 = ORIENTED_EDGE ( 'NONE', *, *, #102852, .T. ) ;
#12924 = CARTESIAN_POINT ( 'NONE',  ( -7.255520619063071663, -4.332661967060333907, 16.69105336089183211 ) ) ;
#12925 = CARTESIAN_POINT ( 'NONE',  ( -4.933275777332625012, -67.91368662472184781, 13.89515823646121184 ) ) ;
#12926 = CARTESIAN_POINT ( 'NONE',  ( 21.67692307692307452, 1.411358822780289120E-15, 0.000000000000000000 ) ) ;
#12927 = ORIENTED_EDGE ( 'NONE', *, *, #43625, .F. ) ;
#12928 = PRESENTATION_STYLE_ASSIGNMENT (( #96528 ) ) ;
#12929 = DIRECTION ( 'NONE',  ( 0.000000000000000000, -1.000000000000000000, 0.000000000000000000 ) ) ;
#12930 = CARTESIAN_POINT ( 'NONE',  ( -93.85239982658497127, -57.67543968518839392, 9.450824874790988872 ) ) ;
#12931 = CARTESIAN_POINT ( 'NONE',  ( -5.382057749264594904, -67.99826798403944395, -2.659775980967107767 ) ) ;
#12932 = CARTESIAN_POINT ( 'NONE',  ( 43.53992551105506692, 465.2531359679902607, 9.299628767491899595 ) ) ;
#12933 = CARTESIAN_POINT ( 'NONE',  ( -9.646083234704169840, 101.9870939097652069, -2.643797197754281569 ) ) ;
#12934 = CARTESIAN_POINT ( 'NONE',  ( 0.000000000000000000, -30.00000000000000000, 0.000000000000000000 ) ) ;
#12935 = CARTESIAN_POINT ( 'NONE',  ( -17.97938082339169341, 36.40366709787543442, -23.34517568653161490 ) ) ;
#12936 = CARTESIAN_POINT ( 'NONE',  ( 57.68379620845067279, -29.99999999999995026, -33.51799637603287607 ) ) ;
#12937 = CARTESIAN_POINT ( 'NONE',  ( -52.32131825073019371, -14.21045842199420584, 63.24190059944674402 ) ) ;
#12938 = CARTESIAN_POINT ( 'NONE',  ( -54.49468904511509493, -36.03252814681875549, 57.85336393633966168 ) ) ;
#12939 = ORIENTED_EDGE ( 'NONE', *, *, #95754, .F. ) ;
#12940 = CARTESIAN_POINT ( 'NONE',  ( 42.29287336469166547, 486.6964296286180911, 8.722237745845980328 ) ) ;
#12941 = ORIENTED_EDGE ( 'NONE', *, *, #7066, .F. ) ;
#12942 = CARTESIAN_POINT ( 'NONE',  ( -102.0386490841828078, -52.71615882625160765, 192.0067383440280935 ) ) ;
#12943 = CARTESIAN_POINT ( 'NONE',  ( 38.54515645702225868, 3.851859888774471706E-31, 5.000000000000001776 ) ) ;
#12944 = ORIENTED_EDGE ( 'NONE', *, *, #20820, .F. ) ;
#12945 = CARTESIAN_POINT ( 'NONE',  ( 18.91882778223193284, 48.67756978012194935, 62.16217564495511283 ) ) ;
#12946 = CARTESIAN_POINT ( 'NONE',  ( -5.646069974130150548, -59.99999999999998579, 39.61802077795142907 ) ) ;
#12947 = DIRECTION ( 'NONE',  ( 0.000000000000000000, -1.000000000000000000, 0.000000000000000000 ) ) ;
#12948 = CARTESIAN_POINT ( 'NONE',  ( -2.977408999572654480, -14.00000000204838457, 7.188101187499999156 ) ) ;
#12949 = CARTESIAN_POINT ( 'NONE',  ( 6.683837171061802529, -3.955946848495957457, 6.851900933636990487 ) ) ;
#12950 = DIRECTION ( 'NONE',  ( 1.000000000000000000, 1.224606353822377258E-16, 0.000000000000000000 ) ) ;
#12951 = CARTESIAN_POINT ( 'NONE',  ( 7.412906595240168706, -82.35811727147745387, 3.014362223629233561 ) ) ;
#12952 = CARTESIAN_POINT ( 'NONE',  ( 62.36520093333108861, -30.00000000000001421, 72.99138914944688850 ) ) ;
#12953 = CARTESIAN_POINT ( 'NONE',  ( -9.059498534015210325, 43.97148598410754516, -13.86662515133364160 ) ) ;
#12954 = CARTESIAN_POINT ( 'NONE',  ( 6.249999999999998224, 1.502314598737158834E-15, -7.999999999999998224 ) ) ;
#12955 = ADVANCED_FACE ( 'NONE', ( #50125 ), #24818, .F. ) ;
#12956 = DIRECTION ( 'NONE',  ( 1.000000000000000000, 0.000000000000000000, 0.000000000000000000 ) ) ;
#12957 = CARTESIAN_POINT ( 'NONE',  ( -27.61222033232023776, -46.43752918860366208, 33.58974296575833307 ) ) ;
#12958 = VERTEX_POINT ( 'NONE', #11117 ) ;
#12959 = ORIENTED_EDGE ( 'NONE', *, *, #2626, .F. ) ;
#12960 = CARTESIAN_POINT ( 'NONE',  ( 47.68197102969904222, -42.98161286699893679, 48.22189115465704390 ) ) ;
#12961 = CARTESIAN_POINT ( 'NONE',  ( -0.6243543237748914176, 8.125635866029588428, 51.58700165176743013 ) ) ;
#12962 = EDGE_CURVE ( 'NONE', #87056, #63425, #2, .T. ) ;
#12963 = FACE_OUTER_BOUND ( 'NONE', #55033, .T. ) ;
#12964 = CARTESIAN_POINT ( 'NONE',  ( -110.2894375318718829, -38.35608233796805422, 184.0685881230607492 ) ) ;
#12965 = ORIENTED_EDGE ( 'NONE', *, *, #102416, .F. ) ;
#12966 = CARTESIAN_POINT ( 'NONE',  ( 90.65944472992794090, -38.34295313743801614, 8.876429703253217340 ) ) ;
#12967 = CARTESIAN_POINT ( 'NONE',  ( 14.35785620000817886, 3.948300967435878661, -4.282865182293611461 ) ) ;
#12968 = CARTESIAN_POINT ( 'NONE',  ( -18.93152581076188312, 49.12231756752685641, 62.08966917159322207 ) ) ;
#12969 = CARTESIAN_POINT ( 'NONE',  ( 10.45102250067199812, 43.95277330377771108, 12.91605047380969218 ) ) ;
#12970 = CARTESIAN_POINT ( 'NONE',  ( 6.035341166382893974, 41.06696360509113219, -71.06135895768771604 ) ) ;
#12971 = CARTESIAN_POINT ( 'NONE',  ( -33.50732914388991901, 434.8932056792464778, 13.71429463173124219 ) ) ;
#12972 = CARTESIAN_POINT ( 'NONE',  ( -33.67444716837086105, 489.3309112354448871, 10.55021651976761987 ) ) ;
#12973 = CARTESIAN_POINT ( 'NONE',  ( 12.50000000000000178, -3.000000000000000000, -34.12705337366765690 ) ) ;
#12974 = CARTESIAN_POINT ( 'NONE',  ( 109.2852756154741201, -60.00000000000002132, 193.0479011121091730 ) ) ;
#12975 = AXIS2_PLACEMENT_3D ( 'NONE', #59485, #83207, #25550 ) ;
#12976 = CARTESIAN_POINT ( 'NONE',  ( -15.64672812219209241, 34.65657699850147111, 23.72309513107661161 ) ) ;
#12977 = ORIENTED_EDGE ( 'NONE', *, *, #2495, .F. ) ;
#12978 = EDGE_CURVE ( 'NONE', #71772, #20242, #36526, .T. ) ;
#12979 = CYLINDRICAL_SURFACE ( 'NONE', #97911, 4.000000000000001776 ) ;
#12980 = CARTESIAN_POINT ( 'NONE',  ( -7.344133061198930612, 27.55505607319423689, 3.176267128233874359 ) ) ;
#12981 = EDGE_LOOP ( 'NONE', ( #76272, #68404, #47011, #34384, #38469 ) ) ;
#12983 = CARTESIAN_POINT ( 'NONE',  ( 5.293277849528764456, 18.43946955771025031, -37.81464980344904347 ) ) ;
#12982 = CARTESIAN_POINT ( 'NONE',  ( -106.1106007292416251, -38.37460074271928079, 196.2185828438378792 ) ) ;
#12984 = CARTESIAN_POINT ( 'NONE',  ( 12.50000000000000000, -2.999999999999996891, -14.34180675897363955 ) ) ;
#12985 = DIRECTION ( 'NONE',  ( 1.000000000000000000, 0.000000000000000000, 0.000000000000000000 ) ) ;
#12986 =( LENGTH_UNIT ( ) NAMED_UNIT ( * ) SI_UNIT ( .MILLI., .METRE. ) );
#12987 = CARTESIAN_POINT ( 'NONE',  ( 7.188101187500000044, -12.03125000204838635, 0.000000000000000000 ) ) ;
#12988 = MECHANICAL_DESIGN_GEOMETRIC_PRESENTATION_REPRESENTATION (  '', ( #35450 ), #100832 ) ;
#12989 = CARTESIAN_POINT ( 'NONE',  ( -1.308996937483428491, -5.000000000000002665, -75.00000000000001421 ) ) ;
#12990 = AXIS2_PLACEMENT_3D ( 'NONE', #21197, #96108, #21714 ) ;
#12991 = AXIS2_PLACEMENT_3D ( 'NONE', #37128, #62441, #69993 ) ;
#12992 = CARTESIAN_POINT ( 'NONE',  ( 30.59538916938560860, 12.96143355072255687, -41.71318167414167277 ) ) ;
#12994 = ORIENTED_EDGE ( 'NONE', *, *, #33671, .T. ) ;
#12993 = CARTESIAN_POINT ( 'NONE',  ( -33.77559172535808329, 464.7834715296604600, 7.192701217093225630 ) ) ;
#12995 = CARTESIAN_POINT ( 'NONE',  ( 82.51382183231068268, -46.47490132111590810, 176.1494215204247951 ) ) ;
#12996 = CARTESIAN_POINT ( 'NONE',  ( 8.216389926104845642, 36.83924058556462455, -1.301042606982605124E-15 ) ) ;
#12997 = VECTOR ( 'NONE', #49466, 1000.000000000000000 ) ;
#12998 = CARTESIAN_POINT ( 'NONE',  ( 6.826425371444816648, -2.641426549045784444, -6.344843397090118131 ) ) ;
#12999 = ORIENTED_EDGE ( 'NONE', *, *, #20568, .T. ) ;
#13000 = DIRECTION ( 'NONE',  ( 1.000000000000000000, -0.000000000000000000, 1.224646799147353207E-16 ) ) ;
#13001 = CARTESIAN_POINT ( 'NONE',  ( -46.83368825529026225, 18.87956456981594755, 15.22947487994887616 ) ) ;
#13002 = CARTESIAN_POINT ( 'NONE',  ( -1.469576158976823947E-15, -29.37499999999999645, 8.000000000000000000 ) ) ;
#13003 = DIRECTION ( 'NONE',  ( 0.000000000000000000, -1.000000000000000000, 0.000000000000000000 ) ) ;
#13004 = DIRECTION ( 'NONE',  ( 1.000000000000000000, 1.224606353822377258E-16, 0.000000000000000000 ) ) ;
#13005 =( BOUNDED_SURFACE ( )  B_SPLINE_SURFACE ( 3, 2, ( 
 ( #52722, #86190, #20956 ),
 ( #53788, #29560, #45704 ),
 ( #62431, #54291, #46240 ),
 ( #71036, #103927, #5766 ) ),
 .UNSPECIFIED., .F., .F., .F. ) 
 B_SPLINE_SURFACE_WITH_KNOTS ( ( 4, 4 ),
 ( 3, 3 ),
 ( 2.844946500601963635E-15, 0.001000220508150799449 ),
 ( 0.000000000000000000, 1.000000000000000000 ),
 .UNSPECIFIED. ) 
 GEOMETRIC_REPRESENTATION_ITEM ( )  RATIONAL_B_SPLINE_SURFACE ( (
 ( 1.000000000000000000, 0.9039444415359472185, 1.000000000000000000),
 ( 1.000000000000000000, 0.9074142757225887035, 1.000000000000000000),
 ( 1.000000000000000000, 0.9095719689034493793, 1.000000000000000000),
 ( 1.000000000000000000, 0.9103180234519272496, 1.000000000000000000) ) ) 
 REPRESENTATION_ITEM ( '' )  SURFACE ( )  );
#13006 = CARTESIAN_POINT ( 'NONE',  ( 5.799999999999999822, 0.000000000000000000, 0.000000000000000000 ) ) ;
#13007 = ORIENTED_EDGE ( 'NONE', *, *, #102184, .F. ) ;
#13008 = CARTESIAN_POINT ( 'NONE',  ( -8.083669201034920704, 295.7559805939946500, 5.917592079150272077 ) ) ;
#13009 = CARTESIAN_POINT ( 'NONE',  ( 37.88747170836497702, 25.37001114043394878, 13.42513980240604177 ) ) ;
#13010 = CARTESIAN_POINT ( 'NONE',  ( 0.000000000000000000, 0.000000000000000000, 0.000000000000000000 ) ) ;
#13012 = CARTESIAN_POINT ( 'NONE',  ( -48.02835407290516656, -1.200000000000000030E-05, 14.35535821593516559 ) ) ;
#13011 = CARTESIAN_POINT ( 'NONE',  ( 42.91610777304483548, 434.7038292574866887, 17.44089724611159653 ) ) ;
#13013 = CARTESIAN_POINT ( 'NONE',  ( -7.188101187500001821, -18.50000000204838457, -2.977408999572651371 ) ) ;
#13014 = CARTESIAN_POINT ( 'NONE',  ( 27.99999999999999645, 1.347111479062088405E-15, 11.00000000000000000 ) ) ;
#13015 = CARTESIAN_POINT ( 'NONE',  ( 1.308679155693521556, -5.000000000000001776, 10.00000000000000533 ) ) ;
#13016 = CONTEXT_DEPENDENT_SHAPE_REPRESENTATION ( #92781, #30510 ) ;
#13017 = ORIENTED_EDGE ( 'NONE', *, *, #103803, .F. ) ;
#13018 = CARTESIAN_POINT ( 'NONE',  ( 43.00000000000000000, 435.1719937645106029, 7.191579780909999720 ) ) ;
#13019 = CARTESIAN_POINT ( 'NONE',  ( 42.98746414932995208, -5.000000000000000888, 6.123233995736769241E-16 ) ) ;
#13020 = AXIS2_PLACEMENT_3D ( 'NONE', #1480, #91589, #50558 ) ;
#13021 = CARTESIAN_POINT ( 'NONE',  ( -8.755878939502101943, 19.75811540481800677, 6.351289142183231468E-13 ) ) ;
#13022 = CARTESIAN_POINT ( 'NONE',  ( 96.86866073052655679, 1.030564683017419500E-14, 0.000000000000000000 ) ) ;
#13023 = ADVANCED_FACE ( 'NONE', ( #40980 ), #67633, .T. ) ;
#13024 = CARTESIAN_POINT ( 'NONE',  ( -14.83949740352256796, 1.410031051014996262, 2.190466161101272125 ) ) ;
#13025 = EDGE_LOOP ( 'NONE', ( #77328, #102266, #67734, #101989 ) ) ;
#13026 = ADVANCED_FACE ( 'NONE', ( #74392 ), #65788, .F. ) ;
#13027 = PRESENTATION_STYLE_ASSIGNMENT (( #79891 ) ) ;
#13028 = VERTEX_POINT ( 'NONE', #4117 ) ;
#13029 = EDGE_CURVE ( 'NONE', #7841, #34210, #45611, .T. ) ;
#13030 = CARTESIAN_POINT ( 'NONE',  ( -27.65271972678647927, 34.30554982303950595, 9.933614217763615528 ) ) ;
#13031 = FACE_OUTER_BOUND ( 'NONE', #50927, .T. ) ;
#13032 = CARTESIAN_POINT ( 'NONE',  ( -42.39103542892770804, 39.51255807744743009, -49.77354649102187523 ) ) ;
#13033 = CARTESIAN_POINT ( 'NONE',  ( -16.83415698846535236, 37.10146012410931604, 21.80698433968611383 ) ) ;
#13034 = CARTESIAN_POINT ( 'NONE',  ( -106.1675901372213531, -59.99999999999999289, 198.0953892983058040 ) ) ;
#13035 = DIRECTION ( 'NONE',  ( -0.000000000000000000, 0.000000000000000000, 1.000000000000000000 ) ) ;
#13036 = CARTESIAN_POINT ( 'NONE',  ( 11.80095105920531040, 304.5943220891977035, -9.054726562005919632 ) ) ;
#13037 = DIRECTION ( 'NONE',  ( -0.000000000000000000, 1.000000000000000000, -0.000000000000000000 ) ) ;
#13038 = CARTESIAN_POINT ( 'NONE',  ( 18.09999999999999787, 1.533819458162526451E-15, 0.000000000000000000 ) ) ;
#13039 = CARTESIAN_POINT ( 'NONE',  ( -84.35187283706933670, -35.91723947740675271, 176.6996256281102546 ) ) ;
#13040 = AXIS2_PLACEMENT_3D ( 'NONE', #45702, #55878, #46759 ) ;
#13041 = DIRECTION ( 'NONE',  ( -1.000000000000000000, -0.000000000000000000, -0.000000000000000000 ) ) ;
#13042 = EDGE_CURVE ( 'NONE', #31444, #1310, #21524, .T. ) ;
#13043 = EDGE_LOOP ( 'NONE', ( #7552, #98787, #13470, #11648 ) ) ;
#13044 = DIRECTION ( 'NONE',  ( 1.000000000000000000, 1.224606353822377258E-16, 0.000000000000000000 ) ) ;
#13046 = CARTESIAN_POINT ( 'NONE',  ( 4.905018583967751589, -67.02359985679677834, -3.459768807258292167 ) ) ;
#13045 = AXIS2_PLACEMENT_3D ( 'NONE', #101757, #36009, #20375 ) ;
#13047 = CARTESIAN_POINT ( 'NONE',  ( -86.42387036193130712, -60.14814614128767545, 21.61025827088693063 ) ) ;
#13048 = DIRECTION ( 'NONE',  ( 1.000000000000000000, 1.224606353822377258E-16, 0.000000000000000000 ) ) ;
#13049 = CARTESIAN_POINT ( 'NONE',  ( -3.742296071587391637, 132.3180728667387314, -5.000000000000000888 ) ) ;
#13050 = CARTESIAN_POINT ( 'NONE',  ( 9.239881047873264919, 139.9679065713606860, 0.000000000000000000 ) ) ;
#13051 = CARTESIAN_POINT ( 'NONE',  ( 19.32152200345201010, 18.64316884708351552, 33.52312678236467747 ) ) ;
#13052 = CARTESIAN_POINT ( 'NONE',  ( 109.5593579388806091, -60.00000000000008527, 197.6560947019162597 ) ) ;
#13053 = CARTESIAN_POINT ( 'NONE',  ( -0.000000000000000000, 4.501353321498349658, -60.59507871780017751 ) ) ;
#13054 = CARTESIAN_POINT ( 'NONE',  ( -105.2983529938406519, -30.00000000000006750, 128.8794261209098124 ) ) ;
#13055 = CARTESIAN_POINT ( 'NONE',  ( -65.00259538333476428, -18.62595769467823814, 75.48159003049013904 ) ) ;
#13056 = CIRCLE ( 'NONE', #23425, 4.000000000000007105 ) ;
#13057 = ORIENTED_EDGE ( 'NONE', *, *, #79476, .T. ) ;
#13058 = CARTESIAN_POINT ( 'NONE',  ( -61.99922069412622960, 39.42506226776489342, -19.74808858303288872 ) ) ;
#13059 = CARTESIAN_POINT ( 'NONE',  ( 81.98093513041146707, -59.99999999999619860, 201.2291763324874125 ) ) ;
#13060 = CIRCLE ( 'NONE', #30347, 3.309500000000001663 ) ;
#13062 = ORIENTED_EDGE ( 'NONE', *, *, #48061, .T. ) ;
#13061 = PRESENTATION_LAYER_ASSIGNMENT (  '', '', ( #69981 ) ) ;
#13063 = DIRECTION ( 'NONE',  ( 0.000000000000000000, -1.000000000000000000, 0.000000000000000000 ) ) ;
#13065 = AXIS2_PLACEMENT_3D ( 'NONE', #27579, #91742, #93337 ) ;
#13064 = CARTESIAN_POINT ( 'NONE',  ( -5.082755093536325042, -17.46875000204838813, -5.082755093536325930 ) ) ;
#13066 = ORIENTED_EDGE ( 'NONE', *, *, #1677, .F. ) ;
#13067 = PRODUCT_DEFINITION_SHAPE ( 'NONE', 'NONE',  #106794 ) ;
#13068 = CARTESIAN_POINT ( 'NONE',  ( -7.000000000000000000, -4.000000000000003553, 39.12435565298213902 ) ) ;
#13069 = ORIENTED_EDGE ( 'NONE', *, *, #39543, .F. ) ;
#13070 = DIRECTION ( 'NONE',  ( 0.000000000000000000, -1.000000000000000000, 0.000000000000000000 ) ) ;
#13072 = AXIS2_PLACEMENT_3D ( 'NONE', #15331, #57368, #90287 ) ;
#13071 = CARTESIAN_POINT ( 'NONE',  ( -11.16652874660464789, -60.00000000000000000, -42.37729182859549582 ) ) ;
#13073 = CARTESIAN_POINT ( 'NONE',  ( 15.05785784214677392, 3.824195276769925655, -4.604276673498363337 ) ) ;
#13074 = CARTESIAN_POINT ( 'NONE',  ( 4.401442555609581635E-16, -31.15625000204838813, -7.188101187500000044 ) ) ;
#13075 = DIRECTION ( 'NONE',  ( -1.000000000000000000, 0.000000000000000000, 0.000000000000000000 ) ) ;
#13076 = AXIS2_PLACEMENT_3D ( 'NONE', #37229, #78176, #4827 ) ;
#13077 = DIRECTION ( 'NONE',  ( -1.000000000000000000, -0.000000000000000000, -0.000000000000000000 ) ) ;
#13078 = CARTESIAN_POINT ( 'NONE',  ( 5.000000000000000000, -46.95251766935337656, 6.320350040254264279 ) ) ;
#13079 = CARTESIAN_POINT ( 'NONE',  ( 9.739726766105679445, 49.99999999999999289, -82.38252115500968387 ) ) ;
#13080 = CARTESIAN_POINT ( 'NONE',  ( -7.801339272325196639, 108.5873147195970319, -1.788609912539670388 ) ) ;
#13081 = EDGE_CURVE ( 'NONE', #21120, #3985, #62856, .T. ) ;
#13082 = CARTESIAN_POINT ( 'NONE',  ( 29.83277460719668639, 307.6570928728218632, -8.908988355798932446 ) ) ;
#13083 = ORIENTED_EDGE ( 'NONE', *, *, #105168, .F. ) ;
#13084 = CARTESIAN_POINT ( 'NONE',  ( -9.806112067865916160, 53.43729364773486168, -2.589978564625472046 ) ) ;
#13085 = LINE ( 'NONE', #87536, #18045 ) ;
#13086 = AXIS2_PLACEMENT_3D ( 'NONE', #4790, #27514, #69007 ) ;
#13087 = CARTESIAN_POINT ( 'NONE',  ( 37.34060288484600676, -46.42986010551973663, 38.17736329578391974 ) ) ;
#13088 = CARTESIAN_POINT ( 'NONE',  ( -8.569529079651847070, -1.734723475976807094E-15, 14.86825985028331942 ) ) ;
#13089 = ORIENTED_EDGE ( 'NONE', *, *, #8896, .T. ) ;
#13090 = EDGE_CURVE ( 'NONE', #106028, #61960, #74898, .T. ) ;
#13091 = ADVANCED_FACE ( 'NONE', ( #13247 ), #9238, .F. ) ;
#13092 = CARTESIAN_POINT ( 'NONE',  ( 3.400000000000000355, 0.000000000000000000, -7.259124522925831435 ) ) ;
#13094 = CARTESIAN_POINT ( 'NONE',  ( -34.06332199976886699, 330.0526646846329299, -3.810096259360388427 ) ) ;
#13093 = CARTESIAN_POINT ( 'NONE',  ( 5.299999999999999822, 3.752776749732553263, -6.499999999999999112 ) ) ;
#13095 = DIRECTION ( 'NONE',  ( 1.000000000000000000, 1.224606353822377258E-16, 0.000000000000000000 ) ) ;
#13096 = CARTESIAN_POINT ( 'NONE',  ( 8.099999999999999645, 0.000000000000000000, 4.000000000000000888 ) ) ;
#13097 = CARTESIAN_POINT ( 'NONE',  ( 0.000000000000000000, 34.00000000000000000, 0.000000000000000000 ) ) ;
#13098 = CARTESIAN_POINT ( 'NONE',  ( 27.10511071441197117, 36.60571256639528315, 10.05698433968570704 ) ) ;
#13099 = CARTESIAN_POINT ( 'NONE',  ( -46.00000000000000000, 450.0000000000002274, -1.797577426246302013 ) ) ;
#13100 = LINE ( 'NONE', #31459, #57286 ) ;
#13101 = EDGE_LOOP ( 'NONE', ( #27321, #2820 ) ) ;
#13102 = CARTESIAN_POINT ( 'NONE',  ( 92.69363537619402393, -60.00000000000000711, -4.651207231870288616 ) ) ;
#13103 = CARTESIAN_POINT ( 'NONE',  ( 28.19275368886287580, 34.18006324415607367, -9.428753190584984623 ) ) ;
#13104 = CARTESIAN_POINT ( 'NONE',  ( 24.83349330513380337, 4.000000000000003553, 0.000000000000000000 ) ) ;
#13105 = VECTOR ( 'NONE', #68142, 1000.000000000000000 ) ;
#13106 = CARTESIAN_POINT ( 'NONE',  ( -5.255459963615564334, 41.40616545433940132, -70.76123437048775600 ) ) ;
#13107 = CARTESIAN_POINT ( 'NONE',  ( 42.61650669486618881, 1.474610560812782335E-15, 0.000000000000000000 ) ) ;
#13108 = EDGE_LOOP ( 'NONE', ( #5319, #28807, #56157, #95901, #21461 ) ) ;
#13109 = EDGE_CURVE ( 'NONE', #91673, #93450, #57918, .T. ) ;
#13110 = CARTESIAN_POINT ( 'NONE',  ( -54.99362396314259627, -30.00000000000000711, 55.63568590878308839 ) ) ;
#13111 = ORIENTED_EDGE ( 'NONE', *, *, #40103, .F. ) ;
#13112 = DIRECTION ( 'NONE',  ( -1.000000000000000000, 0.000000000000000000, 0.000000000000000000 ) ) ;
#13113 = CARTESIAN_POINT ( 'NONE',  ( 30.11650669486618881, 4.898587196589413815E-16, -4.000000000000000888 ) ) ;
#13114 = CARTESIAN_POINT ( 'NONE',  ( 14.37769637048558380, 21.52932494092931037, -5.240976541679501111 ) ) ;
#13115 = PRESENTATION_STYLE_ASSIGNMENT (( #96191 ) ) ;
#13116 = CARTESIAN_POINT ( 'NONE',  ( 2.977408999572651815, -30.31250000204838813, 7.188101187500000933 ) ) ;
#13117 = CARTESIAN_POINT ( 'NONE',  ( -44.27627315854449819, 485.3728101450737427, 2.282345336902423583 ) ) ;
#13118 = CYLINDRICAL_SURFACE ( 'NONE', #85031, 10.00000000000000355 ) ;
#13119 = EDGE_CURVE ( 'NONE', #102083, #60384, #64996, .T. ) ;
#13120 = ORIENTED_EDGE ( 'NONE', *, *, #14992, .F. ) ;
#13121 = B_SPLINE_CURVE_WITH_KNOTS ( 'NONE', 3,
 ( #11259, #101882, #52260, #29629, #28563, #12334 ),
 .UNSPECIFIED., .F., .F.,
 ( 4, 2, 4 ),
 ( 2.380731629586569301E-07, 0.002336973833157552933, 0.004673709593152147040 ),
 .UNSPECIFIED. ) ;
#13122 = EDGE_CURVE ( 'NONE', #58651, #96607, #10468, .T. ) ;
#13124 = ORIENTED_EDGE ( 'NONE', *, *, #86157, .F. ) ;
#13123 =( NAMED_UNIT ( * ) SI_UNIT ( $, .STERADIAN. ) SOLID_ANGLE_UNIT ( ) );
#13125 = CARTESIAN_POINT ( 'NONE',  ( 79.97645733512185018, -39.49688154037509236, 145.6660021679025760 ) ) ;
#13126 = STYLED_ITEM ( 'NONE', ( #40085 ), #65896 ) ;
#13127 = CARTESIAN_POINT ( 'NONE',  ( 14.99550388410314028, 1.250601500879723993, 0.4346214790721553145 ) ) ;
#13128 = EDGE_LOOP ( 'NONE', ( #55173, #34032, #28595, #43085, #37741 ) ) ;
#13129 = CARTESIAN_POINT ( 'NONE',  ( 14.83349330513380337, -4.000000000000000000, 4.898587196589415787E-16 ) ) ;
#13130 = CARTESIAN_POINT ( 'NONE',  ( -7.188101187500000044, -18.40625000204838457, -8.802885111219163269E-16 ) ) ;
#13131 = CARTESIAN_POINT ( 'NONE',  ( -76.58308308725453628, -57.53248158402972479, 194.3307878365576187 ) ) ;
#13132 = COLOUR_RGB ( '', 0.08235294, 0.09019608, 0.10196078) ;
#13133 = VERTEX_POINT ( 'NONE', #44451 ) ;
#13134 = FILL_AREA_STYLE_COLOUR ( '', #10880 ) ;
#13135 = CARTESIAN_POINT ( 'NONE',  ( 0.000000000000000000, 49.50000000000000000, 0.000000000000000000 ) ) ;
#13136 = CARTESIAN_POINT ( 'NONE',  ( 0.000000000000000000, 16.00000000000000000, 0.000000000000000000 ) ) ;
#13137 = CARTESIAN_POINT ( 'NONE',  ( -9.177080501238302546, 84.46653057145729804, -3.972956046786644713 ) ) ;
#13138 = CARTESIAN_POINT ( 'NONE',  ( -37.56673239365863282, -1.200000000000000030E-05, -12.20617127781024713 ) ) ;
#13139 = CIRCLE ( 'NONE', #44114, 4.000000000000007105 ) ;
#13140 = CARTESIAN_POINT ( 'NONE',  ( 3.313708498984762496, -11.46875000409677092, 7.999999999999998224 ) ) ;
#13141 = CARTESIAN_POINT ( 'NONE',  ( -51.40127918372997584, -29.90090478647314498, 48.99973797973098044 ) ) ;
#13142 = AXIS2_PLACEMENT_3D ( 'NONE', #46862, #79757, #5863 ) ;
#13143 = CARTESIAN_POINT ( 'NONE',  ( -37.40742181597744320, 25.81285809103578543, 10.95617127781060418 ) ) ;
#13144 = CIRCLE ( 'NONE', #16624, 5.000000000000001776 ) ;
#13145 = CARTESIAN_POINT ( 'NONE',  ( 66.00571552735603120, 6.975173280561618775E-15, 0.000000000000000000 ) ) ;
#13146 = CARTESIAN_POINT ( 'NONE',  ( 4.036241782280404422, 52.01032325769635634, 7.154377370704869676 ) ) ;
#13147 = CARTESIAN_POINT ( 'NONE',  ( -28.11708234716858712, 104.1183258647170362, 161.0998715582510670 ) ) ;
#13148 = CARTESIAN_POINT ( 'NONE',  ( -9.698972129396508990, 33.17629712741938874, -2.445345647270327216 ) ) ;
#13149 = ORIENTED_EDGE ( 'NONE', *, *, #56286, .T. ) ;
#13151 = AXIS2_PLACEMENT_3D ( 'NONE', #76747, #75688, #50341 ) ;
#13150 = CARTESIAN_POINT ( 'NONE',  ( -4.578626833785902406, -52.33922769183001833, 40.23114928973193827 ) ) ;
#13152 = CARTESIAN_POINT ( 'NONE',  ( 1.530808498934192310E-16, -1.200000000000000030E-05, 16.25000000000000000 ) ) ;
#13153 = DIRECTION ( 'NONE',  ( 1.000000000000000000, 0.000000000000000000, 0.000000000000000000 ) ) ;
#13154 = CARTESIAN_POINT ( 'NONE',  ( -3.265580259469881064, -17.82470403459646136, -37.95109814934059500 ) ) ;
#13155 = CARTESIAN_POINT ( 'NONE',  ( -84.24772247247709345, -30.00000000000000711, 163.2342536007591320 ) ) ;
#13156 = CARTESIAN_POINT ( 'NONE',  ( 7.500000000000007105, 42.00000000000000711, -59.28631038546475907 ) ) ;
#13157 = ADVANCED_FACE ( 'NONE', ( #43910 ), #78852, .T. ) ;
#13158 = ORIENTED_EDGE ( 'NONE', *, *, #22066, .T. ) ;
#13159 = ADVANCED_FACE ( 'NONE', ( #33714 ), #51991, .F. ) ;
#13160 = CARTESIAN_POINT ( 'NONE',  ( -25.89174952812846797, 37.21031890518617047, -8.494939486733640521 ) ) ;
#13161 = CARTESIAN_POINT ( 'NONE',  ( 84.69200348729471273, -57.55678680253502932, 202.1247301444829532 ) ) ;
#13162 = CARTESIAN_POINT ( 'NONE',  ( 65.77516868540070050, -47.40891819904962290, -25.69697480624873620 ) ) ;
#13163 = EDGE_CURVE ( 'NONE', #4002, #13133, #102488, .T. ) ;
#13164 = EDGE_CURVE ( 'NONE', #34686, #82136, #2904, .T. ) ;
#13165 = DIRECTION ( 'NONE',  ( -0.000000000000000000, -1.000000000000000000, -0.000000000000000000 ) ) ;
#13166 = CARTESIAN_POINT ( 'NONE',  ( 5.290067270632455632, 51.34639538792298197, 8.531152949374481764 ) ) ;
#13167 = DIRECTION ( 'NONE',  ( 0.000000000000000000, -0.8660254037844381525, -0.5000000000000008882 ) ) ;
#13168 = CARTESIAN_POINT ( 'NONE',  ( -50.53956664665770404, -60.00000000000000711, 73.16161570676207759 ) ) ;
#13169 = CARTESIAN_POINT ( 'NONE',  ( 43.71217423904096222, 435.6632154632235938, 9.092528312217307729 ) ) ;
#13170 = ADVANCED_FACE ( 'NONE', ( #27241, #60128 ), #18602, .F. ) ;
#13171 = CARTESIAN_POINT ( 'NONE',  ( -37.84772257691307829, 50.00000000000000000, 50.69408796163851605 ) ) ;
#13172 = CIRCLE ( 'NONE', #27009, 4.000000000000007105 ) ;
#13173 = CARTESIAN_POINT ( 'NONE',  ( -86.39152420209940431, -17.34348802733059713, 179.9401184627342332 ) ) ;
#13174 = ORIENTED_EDGE ( 'NONE', *, *, #42157, .F. ) ;
#13175 = CARTESIAN_POINT ( 'NONE',  ( 35.43306991796931271, 355.8922504090353414, 1.638683078167634477 ) ) ;
#13176 = CARTESIAN_POINT ( 'NONE',  ( -18.69420657816679210, 304.6310092840336097, -10.04693110555011160 ) ) ;
#13177 = EDGE_CURVE ( 'NONE', #41710, #99036, #81741, .T. ) ;
#13178 = EDGE_CURVE ( 'NONE', #66028, #83796, #99471, .T. ) ;
#13179 = CARTESIAN_POINT ( 'NONE',  ( -6.245851558170836704, 41.90677382336576073, -59.22337183934418903 ) ) ;
#13180 = CARTESIAN_POINT ( 'NONE',  ( -6.928203230275509661, -10.26930929695540229, -4.000000000000000000 ) ) ;
#13181 = CARTESIAN_POINT ( 'NONE',  ( -83.96832662571230799, -52.72755687222642962, -15.30586875041439932 ) ) ;
#13182 = DIRECTION ( 'NONE',  ( 0.000000000000000000, 0.000000000000000000, 1.000000000000000000 ) ) ;
#13183 = DIRECTION ( 'NONE',  ( 0.000000000000000000, 0.000000000000000000, -1.000000000000000000 ) ) ;
#13184 = ORIENTED_EDGE ( 'NONE', *, *, #52493, .F. ) ;
#13185 = CARTESIAN_POINT ( 'NONE',  ( 18.01960457320383213, 50.00000000000000000, 61.86176977369216701 ) ) ;
#13186 = CARTESIAN_POINT ( 'NONE',  ( 13.43938057902250804, 24.49812678790979703, 2.259581829312952372 ) ) ;
#13187 = CARTESIAN_POINT ( 'NONE',  ( 22.03900363279161567, -4.285714285712638016, 12.70248734011606828 ) ) ;
#13188 = CARTESIAN_POINT ( 'NONE',  ( -36.16987904212881944, 464.0305726607188603, 19.55197929207396967 ) ) ;
#13189 = CARTESIAN_POINT ( 'NONE',  ( 86.84200744108139247, -14.21045842199445630, 3.673032677714961558 ) ) ;
#13190 = CARTESIAN_POINT ( 'NONE',  ( -77.89482686549987989, -49.90756091378847970, 143.7070462317983583 ) ) ;
#13191 = VERTEX_POINT ( 'NONE', #92991 ) ;
#13192 = DIRECTION ( 'NONE',  ( -0.000000000000000000, 1.000000000000000000, -0.000000000000000000 ) ) ;
#13193 = CARTESIAN_POINT ( 'NONE',  ( 4.472135954999580498, 250.1357920494656355, 4.000000000000003553 ) ) ;
#13194 = CARTESIAN_POINT ( 'NONE',  ( 78.03174936499274850, -57.51149409110730204, 196.6180056380835310 ) ) ;
#13195 = CARTESIAN_POINT ( 'NONE',  ( 54.98690275242383052, 50.00000000000000000, 30.77418336387238540 ) ) ;
#13196 = UNCERTAINTY_MEASURE_WITH_UNIT (LENGTH_MEASURE( 1.000000000000000082E-05 ), #58303, 'distance_accuracy_value', 'NONE');
#13197 = AXIS2_PLACEMENT_3D ( 'NONE', #46075, #48171, #40618 ) ;
#13198 = CARTESIAN_POINT ( 'NONE',  ( 43.35640344742173369, 355.0162362535172065, 11.71587114036690025 ) ) ;
#13199 = CARTESIAN_POINT ( 'NONE',  ( 14.34999999999999787, -3.309499999999999886, 0.000000000000000000 ) ) ;
#13200 = ORIENTED_EDGE ( 'NONE', *, *, #90747, .F. ) ;
#13201 = AXIS2_PLACEMENT_3D ( 'NONE', #75749, #92458, #100552 ) ;
#13202 = CARTESIAN_POINT ( 'NONE',  ( 4.205231606200393379, 53.86394433159298956, -7.921949934137936467 ) ) ;
#13203 = CARTESIAN_POINT ( 'NONE',  ( 31.74528079355457777, 439.0126391975445586, 23.49833913028905030 ) ) ;
#13204 = CARTESIAN_POINT ( 'NONE',  ( -16.58710573300773561, 37.15623819652538629, 21.80698433968612449 ) ) ;
#13205 = CARTESIAN_POINT ( 'NONE',  ( -5.082755093536325042, -23.09375000204838457, -5.082755093536325930 ) ) ;
#13206 = DIRECTION ( 'NONE',  ( 0.000000000000000000, -1.000000000000000000, 0.000000000000000000 ) ) ;
#13207 = DIRECTION ( 'NONE',  ( 0.000000000000000000, -1.000000000000000000, 0.000000000000000000 ) ) ;
#13208 = CARTESIAN_POINT ( 'NONE',  ( 6.503418564380250899, 41.93912275385427080, -68.91429206611401526 ) ) ;
#13209 = CARTESIAN_POINT ( 'NONE',  ( -16.72321626032217523, 45.57697876764352429, -6.657797401561673212 ) ) ;
#13210 = FACE_OUTER_BOUND ( 'NONE', #53447, .T. ) ;
#13211 = B_SPLINE_CURVE_WITH_KNOTS ( 'NONE', 3,
 ( #539, #50194, #91212, #83096 ),
 .UNSPECIFIED., .F., .F.,
 ( 4, 4 ),
 ( 1.734723475976807094E-18, 0.002366282582213706433 ),
 .UNSPECIFIED. ) ;
#13212 = CARTESIAN_POINT ( 'NONE',  ( -34.16642289233710983, 463.8422268500497125, 18.98106911353875148 ) ) ;
#13213 = ORIENTED_EDGE ( 'NONE', *, *, #57784, .T. ) ;
#13214 = CARTESIAN_POINT ( 'NONE',  ( 41.50669491856072568, 6.123233995736772199E-16, -5.000000000000001776 ) ) ;
#13215 = MECHANICAL_DESIGN_GEOMETRIC_PRESENTATION_REPRESENTATION (  '', ( #63205 ), #88993 ) ;
#13216 = CIRCLE ( 'NONE', #83828, 4.000000000000001776 ) ;
#13218 = CARTESIAN_POINT ( 'NONE',  ( 26.01855909204189743, -22.09186832850629045, 28.98036754413648808 ) ) ;
#13217 = CARTESIAN_POINT ( 'NONE',  ( -73.11793949506163415, -30.00000000000001776, 143.8487384131749423 ) ) ;
#13219 = CARTESIAN_POINT ( 'NONE',  ( -6.738183602098732403E-15, 17.51648154115788714, 55.02144460582525909 ) ) ;
#13220 = ORIENTED_EDGE ( 'NONE', *, *, #6541, .F. ) ;
#13221 = ADVANCED_FACE ( 'NONE', ( #1292 ), #43896, .T. ) ;
#13222 = VERTEX_POINT ( 'NONE', #42308 ) ;
#13223 = CIRCLE ( 'NONE', #82127, 4.000000000000007105 ) ;
#13224 = CARTESIAN_POINT ( 'NONE',  ( 32.99999999999997868, 463.5362553048591963, 6.739467187734351938 ) ) ;
#13225 = AXIS2_PLACEMENT_3D ( 'NONE', #11703, #103907, #104434 ) ;
#13226 = SURFACE_SIDE_STYLE ('',( #52624 ) ) ;
#13227 = LINE ( 'NONE', #47715, #27565 ) ;
#13228 = AXIS2_PLACEMENT_3D ( 'NONE', #7661, #9262, #16297 ) ;
#13229 = MECHANICAL_DESIGN_GEOMETRIC_PRESENTATION_REPRESENTATION (  '', ( #33987 ), #47716 ) ;
#13230 = CARTESIAN_POINT ( 'NONE',  ( 5.691929483231188414, -5.629165124598859649, -3.250000000000000000 ) ) ;
#13231 = CARTESIAN_POINT ( 'NONE',  ( -27.99999999999999645, 0.000000000000000000, 0.000000000000000000 ) ) ;
#13232 = EDGE_LOOP ( 'NONE', ( #83488, #82351, #104105, #76348, #86745, #49815 ) ) ;
#13233 = CARTESIAN_POINT ( 'NONE',  ( 0.000000000000000000, 0.000000000000000000, 0.000000000000000000 ) ) ;
#13234 = CARTESIAN_POINT ( 'NONE',  ( 90.21985533091218201, -30.00000000000004619, 190.0404579620991115 ) ) ;
#13235 = CARTESIAN_POINT ( 'NONE',  ( -10.05892818186027426, 14.73916874890172757, -10.42188144405744588 ) ) ;
#13236 = AXIS2_PLACEMENT_3D ( 'NONE', #84985, #101166, #85525 ) ;
#13237 = CARTESIAN_POINT ( 'NONE',  ( 0.000000000000000000, 1.500000000000000444, -61.23540616453487218 ) ) ;
#13238 = CARTESIAN_POINT ( 'NONE',  ( 80.70865640423915011, -30.00000000000000355, -12.62041422021882475 ) ) ;
#13239 = LINE ( 'NONE', #46163, #41563 ) ;
#13240 = EDGE_LOOP ( 'NONE', ( #37355, #47183 ) ) ;
#13241 = ORIENTED_EDGE ( 'NONE', *, *, #98530, .T. ) ;
#13242 = EDGE_LOOP ( 'NONE', ( #45662, #88612, #1277, #40669 ) ) ;
#13243 = CARTESIAN_POINT ( 'NONE',  ( 7.500000000000007105, 152.0000000000000000, -5.000000000000000000 ) ) ;
#13244 = CARTESIAN_POINT ( 'NONE',  ( 0.000000000000000000, 304.8518027762758038, 8.936999415352287812 ) ) ;
#13245 = DIRECTION ( 'NONE',  ( -1.000000000000000000, 0.000000000000000000, -0.000000000000000000 ) ) ;
#13246 = DIRECTION ( 'NONE',  ( -1.000000000000000000, -1.224606353822377258E-16, -0.000000000000000000 ) ) ;
#13247 = FACE_OUTER_BOUND ( 'NONE', #94606, .T. ) ;
#13248 = CARTESIAN_POINT ( 'NONE',  ( -8.000086790516061086, -89.00017358106008203, 0.2639471549312816800 ) ) ;
#13249 = DIRECTION ( 'NONE',  ( 0.000000000000000000, -1.000000000000000000, 0.000000000000000000 ) ) ;
#13250 = ORIENTED_EDGE ( 'NONE', *, *, #99359, .F. ) ;
#13251 = ADVANCED_FACE ( 'NONE', ( #19154 ), #89271, .T. ) ;
#13252 = CARTESIAN_POINT ( 'NONE',  ( -7.996668422904766871, 48.00000000000000000, -91.14546720082618947 ) ) ;
#13253 = ORIENTED_EDGE ( 'NONE', *, *, #105197, .F. ) ;
#13254 =( NAMED_UNIT ( * ) SI_UNIT ( $, .STERADIAN. ) SOLID_ANGLE_UNIT ( ) );
#13255 = DIRECTION ( 'NONE',  ( 0.000000000000000000, 0.000000000000000000, -1.000000000000000000 ) ) ;
#13256 = CARTESIAN_POINT ( 'NONE',  ( -38.69275568811816157, 485.6230355318863872, -4.306148472019762252 ) ) ;
#13257 = EDGE_CURVE ( 'NONE', #38500, #7327, #64536, .T. ) ;
#13258 = CIRCLE ( 'NONE', #11474, 7.500000000000000000 ) ;
#13259 = CARTESIAN_POINT ( 'NONE',  ( 3.397147169706663750, 299.9647928271241994, -10.00714482582972487 ) ) ;
#13260 = CARTESIAN_POINT ( 'NONE',  ( 63.44158566079609329, -32.53091779288278218, 78.14191095953113120 ) ) ;
#13261 = ORIENTED_EDGE ( 'NONE', *, *, #17533, .T. ) ;
#13262 = DIRECTION ( 'NONE',  ( -0.000000000000000000, -0.000000000000000000, 1.000000000000000000 ) ) ;
#13263 = VECTOR ( 'NONE', #94061, 1000.000000000000000 ) ;
#13264 = DIRECTION ( 'NONE',  ( -1.000000000000000000, -1.224606353822377258E-16, -0.000000000000000000 ) ) ;
#13265 = DIRECTION ( 'NONE',  ( 0.000000000000000000, 1.000000000000000000, -0.000000000000000000 ) ) ;
#13266 = CARTESIAN_POINT ( 'NONE',  ( -8.880609241544023646, 51.45519007158284808, 4.000283470555588750 ) ) ;
#13267 = ORIENTED_EDGE ( 'NONE', *, *, #78931, .F. ) ;
#13268 = CARTESIAN_POINT ( 'NONE',  ( -4.878909776184771925E-16, 0.6351314446025499993, 6.500000000000000888 ) ) ;
#13269 = CARTESIAN_POINT ( 'NONE',  ( -8.647636768531977935, -60.00000000000002842, -36.71923688686057119 ) ) ;
#13270 = CARTESIAN_POINT ( 'NONE',  ( 35.58361799548379167, 5.000000000000002665, 0.000000000000000000 ) ) ;
#13271 = CARTESIAN_POINT ( 'NONE',  ( 8.000000000000000000, -33.68750000409677625, 0.000000000000000000 ) ) ;
#13272 = CARTESIAN_POINT ( 'NONE',  ( 9.380155525692144280, 15.95825086476136612, 3.484792534604217895 ) ) ;
#13273 = CARTESIAN_POINT ( 'NONE',  ( 86.20424334727701421, -57.42790586652574092, 193.3016074490970482 ) ) ;
#13274 = CARTESIAN_POINT ( 'NONE',  ( -5.221363059330018430, 6.978633969780313251, -27.44954744754475229 ) ) ;
#13275 = AXIS2_PLACEMENT_3D ( 'NONE', #44867, #106658, #370 ) ;
#13276 = CARTESIAN_POINT ( 'NONE',  ( -8.571529135731710269, 24.05510615523603946, 1.271403623727559017E-12 ) ) ;
#13277 = CARTESIAN_POINT ( 'NONE',  ( 7.896165657598944065, -6.210888686280283011, -1.307894402814547163 ) ) ;
#13278 = CARTESIAN_POINT ( 'NONE',  ( 44.97663383827099182, -26.29691875582094340, -29.22557715210724893 ) ) ;
#13279 = CARTESIAN_POINT ( 'NONE',  ( 14.00172459590632457, -49.99988873354983809, 26.85642925593120722 ) ) ;
#13280 = CARTESIAN_POINT ( 'NONE',  ( 17.23461538461538467, 1.411358822780289120E-15, 0.000000000000000000 ) ) ;
#13281 = CARTESIAN_POINT ( 'NONE',  ( -100.6459466783282579, -30.00000000000000000, 181.8192848642643469 ) ) ;
#13282 = AXIS2_PLACEMENT_3D ( 'NONE', #92652, #2038, #2573 ) ;
#13283 = CIRCLE ( 'NONE', #2978, 13.50000000000000178 ) ;
#13284 = CARTESIAN_POINT ( 'NONE',  ( 26.51134585607502103, -57.67681482525394898, 43.69224471368552543 ) ) ;
#13286 = CARTESIAN_POINT ( 'NONE',  ( 43.18901105328356493, 465.6357412882384210, 10.74839809640436350 ) ) ;
#13285 = CARTESIAN_POINT ( 'NONE',  ( 29.68315524076926692, 13.47185074185900255, -42.10535821593530414 ) ) ;
#13287 = EDGE_CURVE ( 'NONE', #93762, #65995, #76601, .T. ) ;
#13288 = EDGE_CURVE ( 'NONE', #30156, #88814, #95559, .T. ) ;
#13289 = SURFACE_SIDE_STYLE ('',( #6257 ) ) ;
#13290 = CYLINDRICAL_SURFACE ( 'NONE', #17017, 1.999999999999998224 ) ;
#13291 = CARTESIAN_POINT ( 'NONE',  ( -9.926810856659471938, 15.46725112412266512, 1.404490565848834027 ) ) ;
#13292 = CARTESIAN_POINT ( 'NONE',  ( 46.00000000000000000, 488.5500823953246368, 3.682191395179805316 ) ) ;
#13293 = CIRCLE ( 'NONE', #71901, 8.400000000000000355 ) ;
#13294 = AXIS2_PLACEMENT_3D ( 'NONE', #18980, #9767, #26023 ) ;
#13295 = CARTESIAN_POINT ( 'NONE',  ( 0.000000000000000000, 0.000000000000000000, 4.000000000000000000 ) ) ;
#13296 = FILL_AREA_STYLE_COLOUR ( '', #52761 ) ;
#13297 = CARTESIAN_POINT ( 'NONE',  ( -87.29625452526420304, -42.75230380456551416, 190.3644472096953848 ) ) ;
#13298 = EDGE_LOOP ( 'NONE', ( #21950, #42109, #63129, #30414, #40022 ) ) ;
#13299 = CARTESIAN_POINT ( 'NONE',  ( 38.69275568812167876, 485.6230355318869556, -4.306148472021480877 ) ) ;
#13300 = CARTESIAN_POINT ( 'NONE',  ( 33.66378992667857517, 439.0645769355539301, 24.00942065012661786 ) ) ;
#13301 = STYLED_ITEM ( 'NONE', ( #13115 ), #15930 ) ;
#13302 = CARTESIAN_POINT ( 'NONE',  ( -11.56863480372296848, -60.36581770793299739, 33.98298590360514027 ) ) ;
#13303 = ADVANCED_FACE ( 'NONE', ( #17670 ), #65679, .T. ) ;
#13304 =( BOUNDED_SURFACE ( )  B_SPLINE_SURFACE ( 2, 3, ( 
 ( #66343, #51206, #84127, #43142, #35612, #42065, #35075, #76023, #2122, #8636, #100825, #74952, #67944, #43662, #26993, #41536, #59871, #84663, #76550, #2662, #57700, #3752 ),
 ( #45276, #53356, #54380, #101897, #36683, #69547, #4274, #19972, #28579, #69024, #70069, #29646, #78154, #37202, #77632, #28057, #85744, #95405, #60929, #21545, #52818, #11815 ),
 ( #93816, #44747, #85189, #11274, #102437, #53873, #94895, #102971, #44208, #61467, #46328, #21039, #29135, #70604, #62005, #93287, #94359, #86804, #86278, #87326, #62521, #37744 ) ),
 .UNSPECIFIED., .F., .F., .F. ) 
 B_SPLINE_SURFACE_WITH_KNOTS ( ( 3, 3 ),
 ( 4, 2, 2, 2, 2, 2, 2, 2, 2, 2, 4 ),
 ( 0.000000000000000000, 1.000000000000000000 ),
 ( 0.7200910805559007644, 0.9402275871953454933, 1.490568853793957427, 2.040910120392569471, 2.591251386991181072, 3.141592653589793116, 3.691933920188405160, 4.242275186787017205, 4.792616453385628361, 5.342957719984240406, 5.563094226623684690 ),
 .UNSPECIFIED. ) 
 GEOMETRIC_REPRESENTATION_ITEM ( )  RATIONAL_B_SPLINE_SURFACE ( (
 ( 1.000000000000000000, 1.000000000000000000, 1.000000000000000000, 1.000000000000000000, 1.000000000000000000, 1.000000000000000000, 1.000000000000000000, 1.000000000000000000, 1.000000000000000000, 1.000000000000000000, 1.000000000000000000, 1.000000000000000000, 1.000000000000000000, 1.000000000000000000, 1.000000000000000000, 1.000000000000000000, 1.000000000000000000, 1.000000000000000000, 1.000000000000000000, 1.000000000000000000, 1.000000000000000000, 1.000000000000000000),
 ( 1.857142857142858317, 1.857142857142858317, 1.857142857142858317, 1.857142857142858317, 1.857142857142858317, 1.857142857142858317, 1.857142857142858317, 1.857142857142858317, 1.857142857142858317, 1.857142857142858317, 1.857142857142858317, 1.857142857142858317, 1.857142857142858317, 1.857142857142858317, 1.857142857142858317, 1.857142857142858317, 1.857142857142858317, 1.857142857142858317, 1.857142857142858317, 1.857142857142858317, 1.857142857142858317, 1.857142857142858317),
 ( 1.000000000000000000, 1.000000000000000000, 1.000000000000000000, 1.000000000000000000, 1.000000000000000000, 1.000000000000000000, 1.000000000000000000, 1.000000000000000000, 1.000000000000000000, 1.000000000000000000, 1.000000000000000000, 1.000000000000000000, 1.000000000000000000, 1.000000000000000000, 1.000000000000000000, 1.000000000000000000, 1.000000000000000000, 1.000000000000000000, 1.000000000000000000, 1.000000000000000000, 1.000000000000000000, 1.000000000000000000) ) ) 
 REPRESENTATION_ITEM ( '' )  SURFACE ( )  );
#13305 = AXIS2_PLACEMENT_3D ( 'NONE', #67882, #85130, #11217 ) ;
#13306 = EDGE_CURVE ( 'NONE', #55271, #77629, #61159, .T. ) ;
#13308 = CARTESIAN_POINT ( 'NONE',  ( 5.088838845617632778, -61.74461508817817901, 13.90681500082671462 ) ) ;
#13307 = LINE ( 'NONE', #4175, #98175 ) ;
#13309 = VERTEX_POINT ( 'NONE', #10095 ) ;
#13310 = CARTESIAN_POINT ( 'NONE',  ( 15.68120647348477625, 6.021684053265039971, -7.051923121165705410 ) ) ;
#13311 = CARTESIAN_POINT ( 'NONE',  ( -13.42788529234582029, 42.83958909155323624, -92.03970976739232412 ) ) ;
#13312 = CYLINDRICAL_SURFACE ( 'NONE', #94317, 7.000000000000000000 ) ;
#13313 = AXIS2_PLACEMENT_3D ( 'NONE', #89676, #48130, #6088 ) ;
#13314 = CARTESIAN_POINT ( 'NONE',  ( -1.014206878838883386, 53.56122919495654600, -9.748765210281540305 ) ) ;
#13315 = ORIENTED_EDGE ( 'NONE', *, *, #29658, .T. ) ;
#13316 = FACE_OUTER_BOUND ( 'NONE', #7080, .T. ) ;
#13318 = CARTESIAN_POINT ( 'NONE',  ( 60.63333333333333286, 3.309500000000014541, 0.000000000000000000 ) ) ;
#13317 = CARTESIAN_POINT ( 'NONE',  ( 48.47273764080328817, -37.70810654209444124, 47.74218356993235801 ) ) ;
#13320 = AXIS2_PLACEMENT_3D ( 'NONE', #54579, #104744, #7103 ) ;
#13319 = DIRECTION ( 'NONE',  ( 0.000000000000000000, -1.000000000000000000, 0.000000000000000000 ) ) ;
#13321 = VERTEX_POINT ( 'NONE', #91038 ) ;
#13322 = ORIENTED_EDGE ( 'NONE', *, *, #46991, .F. ) ;
#13324 = CARTESIAN_POINT ( 'NONE',  ( -24.89405656119140176, 307.3881902170397211, 10.51505289473285742 ) ) ;
#13323 = PRESENTATION_LAYER_ASSIGNMENT (  '', '', ( #21992 ) ) ;
#13325 = VERTEX_POINT ( 'NONE', #33872 ) ;
#13326 = CARTESIAN_POINT ( 'NONE',  ( 21.62181873392152198, 304.1214363623988675, 9.994727137517363857 ) ) ;
#13327 = CARTESIAN_POINT ( 'NONE',  ( 8.000000000000000000, -14.18750000409677092, 0.000000000000000000 ) ) ;
#13328 = CARTESIAN_POINT ( 'NONE',  ( -14.44768974034866815, 5.957293599828318520, -7.129930386717086677 ) ) ;
#13329 = VERTEX_POINT ( 'NONE', #91564 ) ;
#13330 = CARTESIAN_POINT ( 'NONE',  ( -6.101170145166853409, 41.83126053482132534, -70.32427505980624005 ) ) ;
#13331 = CARTESIAN_POINT ( 'NONE',  ( -76.25153216073499607, -60.00000000000000711, 194.9697643434355427 ) ) ;
#13332 = CARTESIAN_POINT ( 'NONE',  ( 46.00000000000000000, 487.9627413807705807, 0.8148295974572986600 ) ) ;
#13333 = CARTESIAN_POINT ( 'NONE',  ( 90.43359995430249398, -59.99999999998527045, -22.43322211268118593 ) ) ;
#13334 = CARTESIAN_POINT ( 'NONE',  ( 27.61650669486618881, 1.474610560812782335E-15, 0.000000000000000000 ) ) ;
#13335 = CARTESIAN_POINT ( 'NONE',  ( -6.661867480585052625, 41.56276523291556657, -58.70509806605610237 ) ) ;
#13337 = CARTESIAN_POINT ( 'NONE',  ( 8.082812510549141294, -29.02946823534357890, 28.72076172514474734 ) ) ;
#13336 = CARTESIAN_POINT ( 'NONE',  ( -105.2983529938406519, -30.00000000000006750, 128.8794261209098124 ) ) ;
#13338 = PRESENTATION_STYLE_ASSIGNMENT (( #12287 ) ) ;
#13339 = COLOUR_RGB ( '', 0.66274510, 0.83137255, 0.94901961) ;
#13340 = ADVANCED_FACE ( 'NONE', ( #92072 ), #89888, .F. ) ;
#13341 = CARTESIAN_POINT ( 'NONE',  ( -48.74031821977154522, -56.82868487743887442, 54.29775784473008571 ) ) ;
#13342 = CARTESIAN_POINT ( 'NONE',  ( 28.86650669486618881, -3.851859888774471706E-31, 4.000000000000000888 ) ) ;
#13343 = ORIENTED_EDGE ( 'NONE', *, *, #34277, .T. ) ;
#13344 = CARTESIAN_POINT ( 'NONE',  ( 0.9982104683319775740, 8.901057192202040724, -51.25567227449372609 ) ) ;
#13345 = CIRCLE ( 'NONE', #73629, 3.000000000000009326 ) ;
#13346 = DIRECTION ( 'NONE',  ( -1.000000000000000000, -1.224606353822377258E-16, -0.000000000000000000 ) ) ;
#13347 = VERTEX_POINT ( 'NONE', #94215 ) ;
#13348 = CARTESIAN_POINT ( 'NONE',  ( -15.26380556289074697, -5.957643091172989180, 13.77816202113101163 ) ) ;
#13349 = COLOUR_RGB ( '', 0.72549020, 0.75294118, 0.79215686) ;
#13350 = VERTEX_POINT ( 'NONE', #101245 ) ;
#13351 = CARTESIAN_POINT ( 'NONE',  ( 101.4679014012201890, -30.00000000000100542, 198.4634389564624257 ) ) ;
#13352 = DIRECTION ( 'NONE',  ( 0.000000000000000000, 1.000000000000000000, 0.000000000000000000 ) ) ;
#13353 = CARTESIAN_POINT ( 'NONE',  ( 7.049753237835907349, 41.74264190701163102, -59.69459104953257622 ) ) ;
#13354 = CARTESIAN_POINT ( 'NONE',  ( -10.04205104288555184, 18.64316884714294886, -37.36680950593608230 ) ) ;
#13355 = CARTESIAN_POINT ( 'NONE',  ( 100.4793545649653908, -30.00000000000000711, 182.9758932259915127 ) ) ;
#13356 = ADVANCED_FACE ( 'NONE', ( #3069 ), #44070, .T. ) ;
#13357 = FACE_OUTER_BOUND ( 'NONE', #75662, .T. ) ;
#13358 = ORIENTED_EDGE ( 'NONE', *, *, #648, .T. ) ;
#13359 = EDGE_LOOP ( 'NONE', ( #32761, #56534, #104398, #19438 ) ) ;
#13360 = ORIENTED_EDGE ( 'NONE', *, *, #8628, .F. ) ;
#13361 = CIRCLE ( 'NONE', #22027, 4.000000000000000888 ) ;
#13362 = CARTESIAN_POINT ( 'NONE',  ( -27.26469077191609003, 36.55125769914398859, 10.05698433968617067 ) ) ;
#13363 = CARTESIAN_POINT ( 'NONE',  ( -43.78232966352139499, 435.5778410705178771, 9.443172893404664592 ) ) ;
#13364 = CARTESIAN_POINT ( 'NONE',  ( -27.10511071441192144, -1.200000000000000030E-05, -7.556984339685890006 ) ) ;
#13365 = VERTEX_POINT ( 'NONE', #28444 ) ;
#13366 = CYLINDRICAL_SURFACE ( 'NONE', #73530, 4.000000000000000000 ) ;
#13367 = EDGE_LOOP ( 'NONE', ( #71869, #96792, #90411, #27182, #2188 ) ) ;
#13368 = LINE ( 'NONE', #70576, #79355 ) ;
#13369 = CARTESIAN_POINT ( 'NONE',  ( 94.03355356640217622, -38.49242504296974232, 201.1935302665664267 ) ) ;
#13370 = CARTESIAN_POINT ( 'NONE',  ( 14.20818530214469355, 21.14724737011036382, 5.805003007643574797 ) ) ;
#13371 = CARTESIAN_POINT ( 'NONE',  ( 84.93372689366950112, -52.71121740197983030, 14.92205009592277243 ) ) ;
#13372 = CARTESIAN_POINT ( 'NONE',  ( 0.000000000000000000, 5.629165124598848990, 3.250000000000002220 ) ) ;
#13373 = AXIS2_PLACEMENT_3D ( 'NONE', #27435, #26373, #1494 ) ;
#13374 = CONICAL_SURFACE ( 'NONE', #63383, 3.309500000000007880, 0.9599310885968770357 ) ;
#13375 = DIRECTION ( 'NONE',  ( -1.000000000000000000, -0.000000000000000000, -0.000000000000000000 ) ) ;
#13376 = CIRCLE ( 'NONE', #92611, 5.000000000000002665 ) ;
#13377 = CARTESIAN_POINT ( 'NONE',  ( 8.000000000000000000, -24.59375000409677270, -3.313708498984761164 ) ) ;
#13378 = EDGE_CURVE ( 'NONE', #87282, #105636, #67990, .T. ) ;
#13379 = DIRECTION ( 'NONE',  ( 0.000000000000000000, -1.000000000000000000, 0.000000000000000000 ) ) ;
#13380 =( NAMED_UNIT ( * ) SI_UNIT ( $, .STERADIAN. ) SOLID_ANGLE_UNIT ( ) );
#13381 = DIRECTION ( 'NONE',  ( -0.000000000000000000, -0.000000000000000000, 1.000000000000000000 ) ) ;
#13382 = COLOUR_RGB ( '', 0.08235294, 0.09019608, 0.10196078) ;
#13383 = ORIENTED_EDGE ( 'NONE', *, *, #38825, .F. ) ;
#13384 = ADVANCED_FACE ( 'NONE', ( #51612 ), #36017, .T. ) ;
#13385 = DIRECTION ( 'NONE',  ( 0.000000000000000000, 1.000000000000000000, 0.000000000000000000 ) ) ;
#13386 = DIRECTION ( 'NONE',  ( 0.000000000000000000, -1.000000000000000000, 0.000000000000000000 ) ) ;
#13387 = CARTESIAN_POINT ( 'NONE',  ( -25.89663754417259511, 37.12989468761069389, 9.165637236921460484 ) ) ;
#13388 = ORIENTED_EDGE ( 'NONE', *, *, #17425, .T. ) ;
#13389 =( GEOMETRIC_REPRESENTATION_CONTEXT ( 3 ) GLOBAL_UNCERTAINTY_ASSIGNED_CONTEXT ( ( #39822 ) ) GLOBAL_UNIT_ASSIGNED_CONTEXT ( ( #36309, #1195, #9839 ) ) REPRESENTATION_CONTEXT ( 'NONE', 'WORKASPACE' ) );
#13390 = CARTESIAN_POINT ( 'NONE',  ( -42.35751940687926265, 435.3789575403023377, 19.45706151680432328 ) ) ;
#13391 = CARTESIAN_POINT ( 'NONE',  ( -29.60711761872594394, 297.6843837922882017, 2.559186976436628402 ) ) ;
#13392 = FACE_OUTER_BOUND ( 'NONE', #98686, .T. ) ;
#13393 = CARTESIAN_POINT ( 'NONE',  ( -3.313708498984765161, -20.46874999999999645, 7.999999999999998224 ) ) ;
#13394 = CARTESIAN_POINT ( 'NONE',  ( 5.095333818548398064, -15.20659882116594197, 34.52546233959761679 ) ) ;
#13395 = CARTESIAN_POINT ( 'NONE',  ( 79.82022815836235452, 1.016364837396684119E-14, 0.000000000000000000 ) ) ;
#13396 = EDGE_LOOP ( 'NONE', ( #102594, #18378 ) ) ;
#13397 = CARTESIAN_POINT ( 'NONE',  ( 83.55767777431796617, -53.73583656280342069, 187.8032102058423618 ) ) ;
#13399 = AXIS2_PLACEMENT_3D ( 'NONE', #89125, #13623, #63268 ) ;
#13398 = CARTESIAN_POINT ( 'NONE',  ( -49.25933966097106520, 7.764757817614880153, 15.83577412118870242 ) ) ;
#13400 = DIRECTION ( 'NONE',  ( -0.9396926207859142011, 0.000000000000000000, -0.3420201433256527812 ) ) ;
#13401 = VERTEX_POINT ( 'NONE', #68891 ) ;
#13402 = ADVANCED_FACE ( 'NONE', ( #101764 ), #36548, .T. ) ;
#13403 = CARTESIAN_POINT ( 'NONE',  ( 93.91931937583731838, -57.67556979900897574, 7.281222044530942128 ) ) ;
#13404 = CARTESIAN_POINT ( 'NONE',  ( 32.28930913498045641, 488.2717154064766873, 9.213726894932154465 ) ) ;
#13405 = CARTESIAN_POINT ( 'NONE',  ( -42.74851244753510571, 465.8913837062016796, 12.61547527226740328 ) ) ;
#13406 = CARTESIAN_POINT ( 'NONE',  ( 14.93248505798278103, -4.333298119783776770, 9.906141972414001629 ) ) ;
#13407 = CARTESIAN_POINT ( 'NONE',  ( -2.064720489383732094, -21.35870767192724173, -38.55174460350388443 ) ) ;
#13408 = VECTOR ( 'NONE', #89731, 1000.000000000000000 ) ;
#13409 = CARTESIAN_POINT ( 'NONE',  ( 20.58069253160714851, -26.08373819371554347, 36.97345864217716382 ) ) ;
#13410 = CARTESIAN_POINT ( 'NONE',  ( 3.214365674771622938, -1.015224780326832832, 104.3190434908430859 ) ) ;
#13411 = CARTESIAN_POINT ( 'NONE',  ( 51.67980559806123608, -29.93021853868486915, 49.50601613781095978 ) ) ;
#13412 = AXIS2_PLACEMENT_3D ( 'NONE', #79163, #54876, #87806 ) ;
#13414 = CARTESIAN_POINT ( 'NONE',  ( -12.61127845791341073, 9.233498968002802343, 9.278883048239569220 ) ) ;
#13413 = CYLINDRICAL_SURFACE ( 'NONE', #49988, 4.000000000000000000 ) ;
#13415 = LINE ( 'NONE', #95957, #64263 ) ;
#13416 = CARTESIAN_POINT ( 'NONE',  ( 40.93435977689158989, 414.3154843149413296, 27.72243992809649527 ) ) ;
#13417 = CARTESIAN_POINT ( 'NONE',  ( 43.67705350351986482, 402.9939091379218894, 16.14668318356454790 ) ) ;
#13418 = DIRECTION ( 'NONE',  ( -0.7092840680488620153, -0.7049227693953836749, 0.000000000000000000 ) ) ;
#13419 = VECTOR ( 'NONE', #105664, 1000.000000000000000 ) ;
#13420 = CARTESIAN_POINT ( 'NONE',  ( -97.86738100951825459, -38.00000000000002842, 125.1133639519820804 ) ) ;
#13421 = AXIS2_PLACEMENT_3D ( 'NONE', #18910, #50671, #18360 ) ;
#13422 = EDGE_LOOP ( 'NONE', ( #14121, #29377, #16243, #102370, #15690 ) ) ;
#13423 = CARTESIAN_POINT ( 'NONE',  ( -10.15372854770908617, -0.7067373757843724569, 20.10246628052868090 ) ) ;
#13424 = CARTESIAN_POINT ( 'NONE',  ( 0.7145311798163210826, 4.618802153517001408, -8.000000000000000000 ) ) ;
#13425 = EDGE_CURVE ( 'NONE', #53278, #67995, #2546, .T. ) ;
#13426 = CARTESIAN_POINT ( 'NONE',  ( 4.589357672516644726, -63.93793969022779322, -3.865585121226772447 ) ) ;
#13427 = ADVANCED_FACE ( 'NONE', ( #94763 ), #100279, .F. ) ;
#13429 = CARTESIAN_POINT ( 'NONE',  ( 4.704252628927049429, -34.58962660028700498, -32.59883165265136995 ) ) ;
#13428 = CARTESIAN_POINT ( 'NONE',  ( 87.62222222222222001, 1.023464760207051730E-14, 0.000000000000000000 ) ) ;
#13430 = ORIENTED_EDGE ( 'NONE', *, *, #21019, .F. ) ;
#13431 = CARTESIAN_POINT ( 'NONE',  ( -0.04725809328185200109, 9.175759667312519241, -8.057670357645360326 ) ) ;
#13432 = CARTESIAN_POINT ( 'NONE',  ( -32.84237740334621236, 485.2251842821281116, 5.746442123025396143 ) ) ;
#13433 = CIRCLE ( 'NONE', #54789, 7.000000000000000000 ) ;
#13434 = ORIENTED_EDGE ( 'NONE', *, *, #83418, .F. ) ;
#13435 = AXIS2_PLACEMENT_3D ( 'NONE', #85519, #103290, #69338 ) ;
#13436 = ADVANCED_FACE ( 'NONE', ( #57303 ), #14327, .F. ) ;
#13437 = FACE_OUTER_BOUND ( 'NONE', #100092, .T. ) ;
#13438 = DIRECTION ( 'NONE',  ( -1.000000000000000000, -0.000000000000000000, -0.000000000000000000 ) ) ;
#13439 = CARTESIAN_POINT ( 'NONE',  ( -92.54188115047482199, -60.00000000000000000, -10.97361708650449330 ) ) ;
#13440 = ORIENTED_EDGE ( 'NONE', *, *, #100852, .F. ) ;
#13441 = CARTESIAN_POINT ( 'NONE',  ( -1.843592604519083133, 42.00000000000000000, -60.21617040574370350 ) ) ;
#13442 = CARTESIAN_POINT ( 'NONE',  ( 30.00000000000000000, 488.7105273189918648, 4.072454560256274725 ) ) ;
#13443 = CIRCLE ( 'NONE', #89309, 1.999999999999998224 ) ;
#13444 = CARTESIAN_POINT ( 'NONE',  ( 19.30602504899448846, 294.6887084256098888, 1.902826926857465573 ) ) ;
#13446 = CARTESIAN_POINT ( 'NONE',  ( 16.08349330513380337, 1.593028355512270962E-15, 0.000000000000000000 ) ) ;
#13445 = CARTESIAN_POINT ( 'NONE',  ( -8.000000000000001776, -26.65624999999999645, 3.313708498984759387 ) ) ;
#13447 = CARTESIAN_POINT ( 'NONE',  ( -85.34039993398450008, -18.60225220077080976, 158.4019857972550653 ) ) ;
#13448 = ORIENTED_EDGE ( 'NONE', *, *, #17572, .T. ) ;
#13449 = B_SPLINE_CURVE_WITH_KNOTS ( 'NONE', 3,
 ( #2331, #2865, #69746, #60608, #75696, #28797, #35818, #26659, #1795, #84331, #18012, #85397, #44408, #101038, #43342, #67624, #50877, #83781, #42802, #76225, #35273, #19109, #27193, #68699, #60083, #45480, #95608, #38973, #12545, #55642, #54586, #78351, #29842, #53556, #6047, #96670, #62719, #88577, #46520, #21750, #4473, #62210, #21229, #63251 ),
 .UNSPECIFIED., .F., .F.,
 ( 4, 2, 2, 2, 2, 2, 2, 2, 2, 2, 2, 2, 2, 2, 2, 2, 2, 2, 2, 2, 2, 4 ),
 ( -6.000000002574998152E-08, 0.002244305247072118665, 0.004488670494144262994, 0.005610853117680367035, 0.006733035741216471075, 0.008977400988288671349, 0.01009958361182477539, 0.01122176623536087943, 0.01346613148243323149, 0.01795486197657778643, 0.02019922722365013676, 0.02244359247072248709, 0.02693232296486719121, 0.03590978395315644334, 0.05386470592973494759, 0.06284216691802418930, 0.07181962790631343796, 0.08079708889460268662, 0.08977454988289193527, 0.1077294718594705991, 0.1256843938360492630, 0.1436393158126279268 ),
 .UNSPECIFIED. ) ;
#13450 = FACE_OUTER_BOUND ( 'NONE', #971, .T. ) ;
#13451 = ORIENTED_EDGE ( 'NONE', *, *, #41292, .T. ) ;
#13452 = ORIENTED_EDGE ( 'NONE', *, *, #52220, .F. ) ;
#13453 = CARTESIAN_POINT ( 'NONE',  ( 0.000000000000000000, 0.000000000000000000, 0.000000000000000000 ) ) ;
#13454 = ORIENTED_EDGE ( 'NONE', *, *, #90647, .T. ) ;
#13455 = CARTESIAN_POINT ( 'NONE',  ( -32.88185469562447594, 462.9125115710301088, 11.53071783310444509 ) ) ;
#13456 = VECTOR ( 'NONE', #18798, 1000.000000000000000 ) ;
#13457 = CARTESIAN_POINT ( 'NONE',  ( -9.999999999999998224, 15.00000000000000000, -0.7768758660233218150 ) ) ;
#13458 = CARTESIAN_POINT ( 'NONE',  ( -88.64096389254642361, -57.60155557764662149, 203.6424623121221487 ) ) ;
#13459 = CARTESIAN_POINT ( 'NONE',  ( -5.093234209761996034, -67.44467773464910465, 3.176141468578046467 ) ) ;
#13460 = DIRECTION ( 'NONE',  ( 0.5735764363510468256, 0.8191520442889913545, 0.000000000000000000 ) ) ;
#13461 = CARTESIAN_POINT ( 'NONE',  ( -9.948688207305192321, 101.1297685050981841, -1.044946705213430915 ) ) ;
#13462 = CARTESIAN_POINT ( 'NONE',  ( -14.00175760317098117, -49.99974274319190926, 26.85746939222903151 ) ) ;
#13463 = CARTESIAN_POINT ( 'NONE',  ( 3.648665620917453278, 15.00000000000000178, -9.999999999999998224 ) ) ;
#13464 = CARTESIAN_POINT ( 'NONE',  ( 87.19843643122861465, -14.21045842199432307, -12.73007766572366606 ) ) ;
#13465 = CARTESIAN_POINT ( 'NONE',  ( -57.89926771889555113, -60.00000000000002132, 101.6232698676003139 ) ) ;
#13466 = EDGE_CURVE ( 'NONE', #48174, #52776, #57835, .T. ) ;
#13467 = CARTESIAN_POINT ( 'NONE',  ( -54.92400839910345667, -25.62426591033550238, 54.65035495193780690 ) ) ;
#13468 = CIRCLE ( 'NONE', #27318, 6.999999999999999112 ) ;
#13469 = VERTEX_POINT ( 'NONE', #87190 ) ;
#13470 = ORIENTED_EDGE ( 'NONE', *, *, #46332, .T. ) ;
#13471 = CARTESIAN_POINT ( 'NONE',  ( -98.96223960978490197, -37.77284757735001364, 191.9112265713812064 ) ) ;
#13472 = CARTESIAN_POINT ( 'NONE',  ( -0.4151059376575879090, 51.29107746579092719, 10.18202427744692073 ) ) ;
#13473 = AXIS2_PLACEMENT_3D ( 'NONE', #2085, #18313, #44708 ) ;
#13474 = ORIENTED_EDGE ( 'NONE', *, *, #4807, .T. ) ;
#13475 = CARTESIAN_POINT ( 'NONE',  ( 4.000000000000000000, 4.898587196589412829E-16, -5.703399999999999359 ) ) ;
#13476 = CARTESIAN_POINT ( 'NONE',  ( -19.73380473719229755, -59.99999999999997868, 40.16716399201472854 ) ) ;
#13477 = FACE_OUTER_BOUND ( 'NONE', #69069, .T. ) ;
#13478 = CARTESIAN_POINT ( 'NONE',  ( -5.082755093536325042, -9.968750002048384573, -5.082755093536325930 ) ) ;
#13479 = CARTESIAN_POINT ( 'NONE',  ( -3.855727343237526750, -67.78910435866291095, 13.12451945574045453 ) ) ;
#13480 = CARTESIAN_POINT ( 'NONE',  ( 51.01037695545453232, 500.0000000000002274, 5.000000000000001776 ) ) ;
#13481 = CARTESIAN_POINT ( 'NONE',  ( 7.344505440741524893, -82.55381072701295864, -3.175463080953003558 ) ) ;
#13482 = CARTESIAN_POINT ( 'NONE',  ( 61.68718524083860189, -30.00000000000000000, 71.20902493795223620 ) ) ;
#13483 = CARTESIAN_POINT ( 'NONE',  ( -10.20347334622529978, 43.27386994973568335, -15.40779740156156841 ) ) ;
#13484 = ADVANCED_FACE ( 'NONE', ( #106386 ), #65946, .F. ) ;
#13485 = CARTESIAN_POINT ( 'NONE',  ( -1.219945943888230522, 34.73238240055653847, 28.18370779043763008 ) ) ;
#13486 = CARTESIAN_POINT ( 'NONE',  ( 4.000000000000000000, 4.898587196589412829E-16, -0.02540000000000007530 ) ) ;
#13487 = UNCERTAINTY_MEASURE_WITH_UNIT (LENGTH_MEASURE( 1.000000000000000082E-05 ), #1886, 'distance_accuracy_value', 'NONE');
#13488 = CARTESIAN_POINT ( 'NONE',  ( -27.03615454696757681, -18.62292616071563955, 28.59941848166171141 ) ) ;
#13489 = CIRCLE ( 'NONE', #75550, 15.80007993603364724 ) ;
#13490 = ORIENTED_EDGE ( 'NONE', *, *, #19731, .T. ) ;
#13491 = ORIENTED_EDGE ( 'NONE', *, *, #36971, .F. ) ;
#13492 = CARTESIAN_POINT ( 'NONE',  ( 48.40635062956359747, -60.28088182408914264, 54.82487149384981961 ) ) ;
#13493 = CARTESIAN_POINT ( 'NONE',  ( -1.235584394549037901, 10.15213688280110738, 50.72542580235119658 ) ) ;
#13494 = DIRECTION ( 'NONE',  ( -1.000000000000000000, -1.224606353822377258E-16, -0.000000000000000000 ) ) ;
#13495 = CARTESIAN_POINT ( 'NONE',  ( -110.5675750054071642, -38.35612456673099047, 181.7435868639444436 ) ) ;
#13496 = ORIENTED_EDGE ( 'NONE', *, *, #87929, .T. ) ;
#13497 = CARTESIAN_POINT ( 'NONE',  ( 91.23346586961952198, -38.40218125908411650, -11.00096301738425453 ) ) ;
#13498 = CARTESIAN_POINT ( 'NONE',  ( 12.33236296408734844, 7.452231929829893353, -8.337237077754760861 ) ) ;
#13499 = CARTESIAN_POINT ( 'NONE',  ( -19.47277721183689891, 49.99121553149272756, 60.38168132464637239 ) ) ;
#13500 = PRESENTATION_STYLE_ASSIGNMENT (( #54477 ) ) ;
#13501 = DIRECTION ( 'NONE',  ( 0.000000000000000000, 1.000000000000000000, 0.000000000000000000 ) ) ;
#13502 = SURFACE_STYLE_FILL_AREA ( #88480 ) ;
#13503 = CARTESIAN_POINT ( 'NONE',  ( -31.32116823360330571, 437.4185521953219791, 20.45661977021549660 ) ) ;
#13504 = CARTESIAN_POINT ( 'NONE',  ( 18.58349330513380337, 4.898587196589405926E-16, -4.000000000000001776 ) ) ;
#13505 = CARTESIAN_POINT ( 'NONE',  ( 12.50000000000000000, -3.000000000000000000, -9.904958390907863119 ) ) ;
#13506 = CONICAL_SURFACE ( 'NONE', #32481, 4.000000000000000000, 0.9599310885968912466 ) ;
#13507 = CARTESIAN_POINT ( 'NONE',  ( 103.4063488952136822, -59.99999999999999289, 200.3742664542178886 ) ) ;
#13508 = CIRCLE ( 'NONE', #15284, 7.000000000000000000 ) ;
#13509 = CARTESIAN_POINT ( 'NONE',  ( -43.43869229197126458, 464.9661605157749591, 13.42065392471462637 ) ) ;
#13510 = EDGE_LOOP ( 'NONE', ( #45341, #63609, #28477, #55997 ) ) ;
#13511 = EDGE_CURVE ( 'NONE', #25171, #53605, #50290, .T. ) ;
#13512 = CARTESIAN_POINT ( 'NONE',  ( -29.05729197575431755, 306.7584490568243041, -9.121552549401764409 ) ) ;
#13513 = CARTESIAN_POINT ( 'NONE',  ( -9.789044728060147804, 294.6486233851416614, -2.043184600577789833 ) ) ;
#13514 = CARTESIAN_POINT ( 'NONE',  ( 46.00000000000000000, 488.9831568219304927, 4.757012338623754388 ) ) ;
#13515 = VERTEX_POINT ( 'NONE', #38135 ) ;
#13517 = CARTESIAN_POINT ( 'NONE',  ( 5.346341838538793745, 32.51490075182633177, -50.48043416745477430 ) ) ;
#13516 = CARTESIAN_POINT ( 'NONE',  ( -91.43843089045226691, -38.39238805426494139, -8.451921997045049650 ) ) ;
#13518 = CARTESIAN_POINT ( 'NONE',  ( 0.000000000000000000, 0.000000000000000000, 112.0000000000000000 ) ) ;
#13519 = CARTESIAN_POINT ( 'NONE',  ( -1.047197551196599630, -2.999999999999999556, 8.000000000000000000 ) ) ;
#13521 = DIRECTION ( 'NONE',  ( -0.5735764363510459374, -0.8191520442889919096, 0.000000000000000000 ) ) ;
#13520 = CIRCLE ( 'NONE', #20446, 5.000000000000010658 ) ;
#13522 = CARTESIAN_POINT ( 'NONE',  ( -1.320432766682874540E-15, -15.40625000204838635, 7.188101187500000044 ) ) ;
#13523 = CARTESIAN_POINT ( 'NONE',  ( -8.737863884121431113, -3.000000000000002665, -90.03618980231151170 ) ) ;
#13524 = ADVANCED_FACE ( 'NONE', ( #79082 ), #87036, .F. ) ;
#13525 = AXIS2_PLACEMENT_3D ( 'NONE', #47873, #22595, #359 ) ;
#13526 = ADVANCED_FACE ( 'NONE', ( #75626 ), #38820, .T. ) ;
#13527 = AXIS2_PLACEMENT_3D ( 'NONE', #49622, #82530, #41009 ) ;
#13528 = CARTESIAN_POINT ( 'NONE',  ( 9.349999999999997868, -3.309499999999999886, 0.000000000000000000 ) ) ;
#13530 = ORIENTED_EDGE ( 'NONE', *, *, #56516, .T. ) ;
#13529 = DIRECTION ( 'NONE',  ( 0.000000000000000000, 0.000000000000000000, 1.000000000000000000 ) ) ;
#13531 = CARTESIAN_POINT ( 'NONE',  ( 83.42202203922076365, -39.47238757521779462, 173.7499749762425267 ) ) ;
#13532 = DIRECTION ( 'NONE',  ( 0.000000000000000000, -1.000000000000000000, 0.000000000000000000 ) ) ;
#13533 = DIRECTION ( 'NONE',  ( 0.000000000000000000, -1.000000000000000000, 0.000000000000000000 ) ) ;
#13534 = VERTEX_POINT ( 'NONE', #35202 ) ;
#13535 = CARTESIAN_POINT ( 'NONE',  ( -33.40226379760697029, 315.1786766184623048, -7.050876513733235207 ) ) ;
#13536 = EDGE_CURVE ( 'NONE', #74863, #866, #100432, .T. ) ;
#13537 = CARTESIAN_POINT ( 'NONE',  ( 17.16204799116226809, 34.18975596472709100, 24.24075866926950340 ) ) ;
#13538 = FACE_OUTER_BOUND ( 'NONE', #89932, .T. ) ;
#13539 = SURFACE_SIDE_STYLE ('',( #47500 ) ) ;
#13540 = DIRECTION ( 'NONE',  ( -1.000000000000000000, -0.000000000000000000, -0.000000000000000000 ) ) ;
#13541 = VERTEX_POINT ( 'NONE', #75080 ) ;
#13542 = AXIS2_PLACEMENT_3D ( 'NONE', #13572, #55606, #14623 ) ;
#13543 = CARTESIAN_POINT ( 'NONE',  ( -9.014154628132734715, 295.0480661387584860, 4.340608627653916862 ) ) ;
#13544 = CARTESIAN_POINT ( 'NONE',  ( -1.000000000000000000, -40.36500490292975485, -0.7636728796494194338 ) ) ;
#13545 = LINE ( 'NONE', #61609, #2835 ) ;
#13548 = AXIS2_PLACEMENT_3D ( 'NONE', #2766, #50259, #1697 ) ;
#13547 =( NAMED_UNIT ( * ) PLANE_ANGLE_UNIT ( ) SI_UNIT ( $, .RADIAN. ) );
#13546 = FACE_OUTER_BOUND ( 'NONE', #44296, .T. ) ;
#13549 = CONICAL_SURFACE ( 'NONE', #65221, 5.000000000000001776, 0.9599310885968803664 ) ;
#13550 = CARTESIAN_POINT ( 'NONE',  ( 7.188101187500000044, -22.15625000204838457, 0.000000000000000000 ) ) ;
#13551 = CARTESIAN_POINT ( 'NONE',  ( 13.41576242262104302, 302.5494855022793672, -10.06425233116351059 ) ) ;
#13552 = DIRECTION ( 'NONE',  ( 0.000000000000000000, 0.000000000000000000, -1.000000000000000000 ) ) ;
#13553 = AXIS2_PLACEMENT_3D ( 'NONE', #100885, #27049, #59934 ) ;
#13554 = ORIENTED_EDGE ( 'NONE', *, *, #2080, .F. ) ;
#13555 = CARTESIAN_POINT ( 'NONE',  ( 10.38582326156070401, 6.955909371148003117, 0.000000000000000000 ) ) ;
#13556 = CARTESIAN_POINT ( 'NONE',  ( 4.988960626530190971E-15, 27.29656849860388235, 40.75000000000000000 ) ) ;
#13557 = CARTESIAN_POINT ( 'NONE',  ( -3.241829659524363638, 35.62537785594091844, -5.000000000000000000 ) ) ;
#13558 = FACE_OUTER_BOUND ( 'NONE', #87252, .T. ) ;
#13559 = EDGE_CURVE ( 'NONE', #39684, #59572, #68075, .T. ) ;
#13560 = CARTESIAN_POINT ( 'NONE',  ( 6.162888688655344005, 3.752776749732565253, 6.499999999999997335 ) ) ;
#13561 = EDGE_LOOP ( 'NONE', ( #85551, #77996, #76616, #20937 ) ) ;
#13562 = CONICAL_SURFACE ( 'NONE', #44628, 4.172000000000001485, 0.9599310885968750373 ) ;
#13563 = DIRECTION ( 'NONE',  ( 0.000000000000000000, 1.000000000000000000, 0.000000000000000000 ) ) ;
#13564 = CARTESIAN_POINT ( 'NONE',  ( 92.82022815836235452, 5.000000000000023093, 6.123233995736781074E-16 ) ) ;
#13565 = ORIENTED_EDGE ( 'NONE', *, *, #61572, .T. ) ;
#13566 = EDGE_CURVE ( 'NONE', #22177, #53932, #28357, .T. ) ;
#13567 = DIRECTION ( 'NONE',  ( 0.5735764363510466035, -0.8191520442889914655, 1.003171929053524500E-16 ) ) ;
#13568 =( LENGTH_UNIT ( ) NAMED_UNIT ( * ) SI_UNIT ( .MILLI., .METRE. ) );
#13569 = DIRECTION ( 'NONE',  ( -0.000000000000000000, 1.000000000000000000, -0.000000000000000000 ) ) ;
#13570 = UNCERTAINTY_MEASURE_WITH_UNIT (LENGTH_MEASURE( 1.000000000000000082E-05 ), #31284, 'distance_accuracy_value', 'NONE');
#13571 = CARTESIAN_POINT ( 'NONE',  ( -109.0438932907287182, -59.99999999999999289, 136.2887194836895617 ) ) ;
#13572 = CARTESIAN_POINT ( 'NONE',  ( 0.000000000000000000, 35.00000000000000000, 0.000000000000000000 ) ) ;
#13573 = CARTESIAN_POINT ( 'NONE',  ( 18.54170707414674979, 304.6552822257318098, -9.041841629248555279 ) ) ;
#13574 = CARTESIAN_POINT ( 'NONE',  ( 21.09715123528542691, 5.000000000000004441, 6.123233995736770227E-16 ) ) ;
#13575 = PRESENTATION_STYLE_ASSIGNMENT (( #37379 ) ) ;
#13576 = CARTESIAN_POINT ( 'NONE',  ( -83.13834745119730485, -50.08347900195551716, 183.9098975223591310 ) ) ;
#13577 = CARTESIAN_POINT ( 'NONE',  ( 19.68171092263090216, 43.94894922844405016, -83.44212096724145056 ) ) ;
#13578 = EDGE_LOOP ( 'NONE', ( #104440, #54115, #74906, #36727, #85205, #27746 ) ) ;
#13579 = CARTESIAN_POINT ( 'NONE',  ( 0.000000000000000000, 0.000000000000000000, 0.000000000000000000 ) ) ;
#13580 = EDGE_CURVE ( 'NONE', #69803, #67441, #42264, .T. ) ;
#13581 = CARTESIAN_POINT ( 'NONE',  ( 5.383284837158154090, -68.00049343515777878, 2.657356347551696363 ) ) ;
#13582 = CARTESIAN_POINT ( 'NONE',  ( -84.87627867855697161, -45.26544462712148231, 33.56767573986881814 ) ) ;
#13583 = CARTESIAN_POINT ( 'NONE',  ( -1.459252261598892542, -6.102732174931079889, -13.75226092436777137 ) ) ;
#13584 = CARTESIAN_POINT ( 'NONE',  ( 7.955546711083004041, 98.60610140865000517, 0.000000000000000000 ) ) ;
#13585 = CARTESIAN_POINT ( 'NONE',  ( -3.978477517404915176, -5.573260695678979637, -6.171287963165205781 ) ) ;
#13586 = CARTESIAN_POINT ( 'NONE',  ( 30.67950393662592745, 18.64316884711713485, 23.57730434126678887 ) ) ;
#13587 = AXIS2_PLACEMENT_3D ( 'NONE', #98573, #106663, #7428 ) ;
#13588 = CARTESIAN_POINT ( 'NONE',  ( 108.4902253387283793, -59.99999999999992184, 199.0859659658876524 ) ) ;
#13589 = CARTESIAN_POINT ( 'NONE',  ( -103.8766418169371093, -14.21045842199435860, 137.3606855625607182 ) ) ;
#13590 = EDGE_CURVE ( 'NONE', #27686, #97818, #69845, .T. ) ;
#13591 = CARTESIAN_POINT ( 'NONE',  ( -65.57779507755935811, -46.43844589625626895, 91.59816456652244199 ) ) ;
#13592 = ORIENTED_EDGE ( 'NONE', *, *, #14083, .T. ) ;
#13593 = CARTESIAN_POINT ( 'NONE',  ( -63.69848661309710991, 38.95268708794027646, -2.134519030202793655 ) ) ;
#13594 = CARTESIAN_POINT ( 'NONE',  ( 88.92543633794424807, -59.99999999998018296, 204.2227067804597027 ) ) ;
#13595 = VECTOR ( 'NONE', #61871, 1000.000000000000000 ) ;
#13596 = EDGE_LOOP ( 'NONE', ( #40728, #28399, #63481 ) ) ;
#13597 = CARTESIAN_POINT ( 'NONE',  ( 13.53380759260212329, -56.00905799123083284, 30.58586009444553611 ) ) ;
#13598 = CARTESIAN_POINT ( 'NONE',  ( -7.188101187500002709, -20.18750000204838813, 2.977408999572647819 ) ) ;
#13599 = DIRECTION ( 'NONE',  ( -1.000000000000000000, 0.000000000000000000, 0.000000000000000000 ) ) ;
#13600 = VERTEX_POINT ( 'NONE', #78284 ) ;
#13601 = DIRECTION ( 'NONE',  ( -1.000000000000000000, -1.224606353822377258E-16, -0.000000000000000000 ) ) ;
#13602 = ADVANCED_FACE ( 'NONE', ( #21166 ), #16403, .T. ) ;
#13603 = ORIENTED_EDGE ( 'NONE', *, *, #48254, .F. ) ;
#13604 = CARTESIAN_POINT ( 'NONE',  ( 11.53285117555237171, 45.44727734447008061, -14.28089210442093915 ) ) ;
#13605 = DIRECTION ( 'NONE',  ( -1.000000000000000000, -1.224606353822377258E-16, -0.000000000000000000 ) ) ;
#13606 = CARTESIAN_POINT ( 'NONE',  ( -92.54656138765464846, -60.00000000000001421, -10.92108962363814051 ) ) ;
#13607 = DIRECTION ( 'NONE',  ( 0.000000000000000000, -1.000000000000000000, 0.000000000000000000 ) ) ;
#13608 = CARTESIAN_POINT ( 'NONE',  ( -7.188101187500002709, -30.68750000204839168, 2.977408999572648707 ) ) ;
#13609 = FACE_OUTER_BOUND ( 'NONE', #63895, .T. ) ;
#13610 = CARTESIAN_POINT ( 'NONE',  ( 5.000000000000000000, -57.62779005937431265, 11.09695692297539971 ) ) ;
#13611 = CARTESIAN_POINT ( 'NONE',  ( 6.145467200820246667, 48.00000000000000000, -77.00333157708931253 ) ) ;
#13612 = CARTESIAN_POINT ( 'NONE',  ( -30.00000000000000000, -54.00000000000000711, 27.11721482942554928 ) ) ;
#13613 = EDGE_CURVE ( 'NONE', #18077, #65653, #99077, .T. ) ;
#13614 = CARTESIAN_POINT ( 'NONE',  ( -41.71680995862502783, 325.2945054222758472, 5.423733409817787177 ) ) ;
#13615 = CARTESIAN_POINT ( 'NONE',  ( 31.58792830376275873, 310.4493673141303702, -8.232059693113699339 ) ) ;
#13616 = CIRCLE ( 'NONE', #86033, 3.309500000000001663 ) ;
#13617 = ORIENTED_EDGE ( 'NONE', *, *, #26494, .T. ) ;
#13618 = CARTESIAN_POINT ( 'NONE',  ( 6.201636426617084574E-15, 39.99999999999999289, -70.00365511371767013 ) ) ;
#13619 = DIRECTION ( 'NONE',  ( -1.000000000000000000, -1.224606353822377258E-16, -0.000000000000000000 ) ) ;
#13620 = CARTESIAN_POINT ( 'NONE',  ( 34.39988281114163016, -56.83016256492278728, 38.30024153359905625 ) ) ;
#13621 = CARTESIAN_POINT ( 'NONE',  ( 4.453875240779016309, -1.734723475976807094E-15, -16.57301948837565675 ) ) ;
#13622 = ORIENTED_EDGE ( 'NONE', *, *, #67576, .T. ) ;
#13623 = DIRECTION ( 'NONE',  ( -1.000000000000000000, -1.224606353822377258E-16, -0.000000000000000000 ) ) ;
#13624 = AXIS2_PLACEMENT_3D ( 'NONE', #3970, #46025, #103718 ) ;
#13625 = ORIENTED_EDGE ( 'NONE', *, *, #38290, .F. ) ;
#13627 = CARTESIAN_POINT ( 'NONE',  ( -35.76482652855951017, 405.2378813769876729, 6.148826621638260548 ) ) ;
#13626 = CARTESIAN_POINT ( 'NONE',  ( 0.000000000000000000, 0.000000000000000000, 0.000000000000000000 ) ) ;
#13628 = DIRECTION ( 'NONE',  ( -0.3144882010791185678, 0.9492613820134156999, 0.000000000000000000 ) ) ;
#13629 = CARTESIAN_POINT ( 'NONE',  ( 18.09999999999999787, 1.533819458162526451E-15, 0.000000000000000000 ) ) ;
#13630 = CARTESIAN_POINT ( 'NONE',  ( 45.94900261086841198, 1.482358050883964840E-15, 0.000000000000000000 ) ) ;
#13631 = DIRECTION ( 'NONE',  ( 0.000000000000000000, 1.000000000000000000, 0.000000000000000000 ) ) ;
#13632 = CARTESIAN_POINT ( 'NONE',  ( 4.472135954999579610, -85.27077220067363328, 4.000000000000002665 ) ) ;
#13633 = DIRECTION ( 'NONE',  ( 0.000000000000000000, 0.000000000000000000, 1.000000000000000000 ) ) ;
#13635 = ORIENTED_EDGE ( 'NONE', *, *, #83797, .F. ) ;
#13634 = CIRCLE ( 'NONE', #99716, 6.000000000000012434 ) ;
#13636 = CARTESIAN_POINT ( 'NONE',  ( 95.45105784953814521, -60.00000000000000000, 52.25429896273150376 ) ) ;
#13637 = FILL_AREA_STYLE ('',( #106759 ) ) ;
#13638 = FACE_OUTER_BOUND ( 'NONE', #55374, .T. ) ;
#13639 =( BOUNDED_SURFACE ( )  B_SPLINE_SURFACE ( 3, 2, ( 
 ( #26594, #93948, #44332 ),
 ( #85875, #19570, #60010 ),
 ( #91822, #69669, #102567 ),
 ( #28713, #92867, #19035 ) ),
 .UNSPECIFIED., .F., .F., .T. ) 
 B_SPLINE_SURFACE_WITH_KNOTS ( ( 4, 4 ),
 ( 3, 3 ),
 ( 5.160802341031001106E-17, 0.0004290382097890881952 ),
 ( 0.000000000000000000, 1.000000000000000000 ),
 .UNSPECIFIED. ) 
 GEOMETRIC_REPRESENTATION_ITEM ( )  RATIONAL_B_SPLINE_SURFACE ( (
 ( 1.000000000000000000, 0.7888522786293986622, 1.000000000000000000),
 ( 1.000000000000000000, 0.7909287578648700467, 1.000000000000000000),
 ( 1.000000000000000000, 0.7929954621609184295, 1.000000000000000000),
 ( 1.000000000000000000, 0.7950530193018779945, 1.000000000000000000) ) ) 
 REPRESENTATION_ITEM ( '' )  SURFACE ( )  );
#13640 = FACE_OUTER_BOUND ( 'NONE', #50609, .T. ) ;
#13641 = LINE ( 'NONE', #104249, #4716 ) ;
#13642 = ORIENTED_EDGE ( 'NONE', *, *, #36687, .T. ) ;
#13643 = ADVANCED_FACE ( 'NONE', ( #38388 ), #31897, .T. ) ;
#13644 = CARTESIAN_POINT ( 'NONE',  ( -74.36474976291079031, -30.00000000000002132, 110.0129636005011946 ) ) ;
#13645 = VERTEX_POINT ( 'NONE', #20649 ) ;
#13646 = CIRCLE ( 'NONE', #29259, 56.99999999999999289 ) ;
#13647 = FILL_AREA_STYLE_COLOUR ( '', #101999 ) ;
#13648 = DIRECTION ( 'NONE',  ( -0.000000000000000000, -1.000000000000000000, -0.000000000000000000 ) ) ;
#13649 = CARTESIAN_POINT ( 'NONE',  ( 6.281178480976150169, 7.505553499465141165, 5.007024290797836712E-17 ) ) ;
#13650 = CARTESIAN_POINT ( 'NONE',  ( 14.59912249379336657, 22.21173916953564387, -3.991112248664791640 ) ) ;
#13651 =( NAMED_UNIT ( * ) PLANE_ANGLE_UNIT ( ) SI_UNIT ( $, .RADIAN. ) );
#13652 = CARTESIAN_POINT ( 'NONE',  ( -7.188101187500001821, -30.87500000204838813, -2.977408999572651371 ) ) ;
#13653 = DIRECTION ( 'NONE',  ( -0.5735764363510459374, -0.8191520442889919096, 0.000000000000000000 ) ) ;
#13654 = DIRECTION ( 'NONE',  ( 0.000000000000000000, 0.000000000000000000, 1.000000000000000000 ) ) ;
#13656 = ADVANCED_FACE ( 'NONE', ( #36808 ), #54517, .T. ) ;
#13655 =( LENGTH_UNIT ( ) NAMED_UNIT ( * ) SI_UNIT ( .MILLI., .METRE. ) );
#13657 = ORIENTED_EDGE ( 'NONE', *, *, #36375, .T. ) ;
#13658 = AXIS2_PLACEMENT_3D ( 'NONE', #103822, #88183, #79022 ) ;
#13660 = EDGE_LOOP ( 'NONE', ( #73843, #73595, #49294 ) ) ;
#13659 = DIRECTION ( 'NONE',  ( -1.000000000000000000, -1.224606353822377258E-16, -0.000000000000000000 ) ) ;
#13661 = CARTESIAN_POINT ( 'NONE',  ( 79.40402211849792025, -22.14576379642964810, 126.4721508377499788 ) ) ;
#13662 = CARTESIAN_POINT ( 'NONE',  ( -38.56060268544248260, 27.32095725847138823, -12.96889906080386901 ) ) ;
#13663 = EDGE_LOOP ( 'NONE', ( #68138, #36181, #614, #47585 ) ) ;
#13664 = EDGE_CURVE ( 'NONE', #106696, #77934, #30203, .T. ) ;
#13665 = DIRECTION ( 'NONE',  ( 0.5735764363510466035, -0.8191520442889914655, 1.003171929053524500E-16 ) ) ;
#13666 = ADVANCED_FACE ( 'NONE', ( #28186 ), #79346, .T. ) ;
#13667 = DIRECTION ( 'NONE',  ( 0.000000000000000000, 0.000000000000000000, 1.000000000000000000 ) ) ;
#13668 = CARTESIAN_POINT ( 'NONE',  ( 7.188101187500000933, -20.56250000204838813, -2.977408999572650483 ) ) ;
#13669 = CARTESIAN_POINT ( 'NONE',  ( -46.61116709543701120, -57.68144024183414587, 68.72738526911024337 ) ) ;
#13670 = CARTESIAN_POINT ( 'NONE',  ( 15.77372286590048311, 302.5604438122106785, 9.875089768359858411 ) ) ;
#13671 = ORIENTED_EDGE ( 'NONE', *, *, #55710, .F. ) ;
#13672 =( NAMED_UNIT ( * ) PLANE_ANGLE_UNIT ( ) SI_UNIT ( $, .RADIAN. ) );
#13673 = DIRECTION ( 'NONE',  ( 0.000000000000000000, 0.000000000000000000, 1.000000000000000000 ) ) ;
#13674 = CARTESIAN_POINT ( 'NONE',  ( 2.955793532184386674, 53.34242613923570531, 5.000000000000000000 ) ) ;
#13675 = CARTESIAN_POINT ( 'NONE',  ( 6.931965211968624807, 41.62851022707389603, -59.01894829855800140 ) ) ;
#13676 = DIRECTION ( 'NONE',  ( -1.000000000000000000, -1.224606353822377258E-16, -0.000000000000000000 ) ) ;
#13677 = CARTESIAN_POINT ( 'NONE',  ( -1.469576158976823947E-15, -13.06250000409676915, 8.000000000000000000 ) ) ;
#13678 = CARTESIAN_POINT ( 'NONE',  ( -17.75574951819011105, -16.19080177579213498, 31.52114076861774095 ) ) ;
#13679 = MECHANICAL_DESIGN_GEOMETRIC_PRESENTATION_REPRESENTATION (  '', ( #91169 ), #36068 ) ;
#13680 = CARTESIAN_POINT ( 'NONE',  ( 14.83349330513380337, -4.000000000000000888, 4.898587196589416773E-16 ) ) ;
#13681 = CARTESIAN_POINT ( 'NONE',  ( 5.347321875081102682, 33.30354557871893917, -51.19160682728892908 ) ) ;
#13682 = B_SPLINE_CURVE_WITH_KNOTS ( 'NONE', 3,
 ( #66348, #17292, #1049, #83068 ),
 .UNSPECIFIED., .F., .F.,
 ( 4, 4 ),
 ( 0.000000000000000000, 0.001739938677313634333 ),
 .UNSPECIFIED. ) ;
#13683 = SHAPE_DEFINITION_REPRESENTATION ( #45916, #74292 ) ;
#13684 = CARTESIAN_POINT ( 'NONE',  ( 16.65484354297773351, -5.000000000000000000, 0.000000000000000000 ) ) ;
#13685 = ORIENTED_EDGE ( 'NONE', *, *, #49238, .T. ) ;
#13686 = CARTESIAN_POINT ( 'NONE',  ( -2.210743487168307375, -53.78942310434221241, 40.82584008148600674 ) ) ;
#13687 = CARTESIAN_POINT ( 'NONE',  ( -1.510421413154896753, 15.23810023151367332, 9.910377230550597716 ) ) ;
#13688 = DIRECTION ( 'NONE',  ( 1.000000000000000000, 0.000000000000000000, 0.000000000000000000 ) ) ;
#13689 = CARTESIAN_POINT ( 'NONE',  ( -72.36027791898858652, -30.15764493038331295, -28.80863952084724389 ) ) ;
#13690 = CARTESIAN_POINT ( 'NONE',  ( -66.53608649180739576, -30.00000000000000000, 84.68920165401893030 ) ) ;
#13691 = CARTESIAN_POINT ( 'NONE',  ( -43.00000000000000000, 450.0000000000002274, 1.202422573753698876 ) ) ;
#13692 = EDGE_CURVE ( 'NONE', #41831, #101431, #5220, .T. ) ;
#13693 = CIRCLE ( 'NONE', #22368, 4.000000000000001776 ) ;
#13694 = ORIENTED_EDGE ( 'NONE', *, *, #31258, .T. ) ;
#13695 = CARTESIAN_POINT ( 'NONE',  ( 7.999999999999998224, -9.781250004096767370, 3.313708498984766049 ) ) ;
#13696 = CARTESIAN_POINT ( 'NONE',  ( 96.35553945990194791, -57.62197075410178826, 204.4943201522608547 ) ) ;
#13697 = LINE ( 'NONE', #5097, #101644 ) ;
#13698 = EDGE_CURVE ( 'NONE', #39211, #64041, #56020, .T. ) ;
#13699 = VECTOR ( 'NONE', #13375, 1000.000000000000000 ) ;
#13700 = DIRECTION ( 'NONE',  ( 0.000000000000000000, -1.000000000000000000, 0.000000000000000000 ) ) ;
#13701 = CARTESIAN_POINT ( 'NONE',  ( -16.11127471224471464, 21.68306317501279779, 1.725009018224902047 ) ) ;
#13702 = CARTESIAN_POINT ( 'NONE',  ( 1.308996938995746318, -3.000000000000003553, -75.00000000000002842 ) ) ;
#13703 = CARTESIAN_POINT ( 'NONE',  ( -61.36110657752745112, -60.00000000000001421, 105.0795332954127161 ) ) ;
#13704 = SURFACE_SIDE_STYLE ('',( #87621 ) ) ;
#13705 = DIRECTION ( 'NONE',  ( -1.000000000000000000, -1.224606353822377258E-16, -0.000000000000000000 ) ) ;
#13706 = PRESENTATION_LAYER_ASSIGNMENT (  '', '', ( #92938 ) ) ;
#13707 = CARTESIAN_POINT ( 'NONE',  ( -62.59524157945776324, 49.99999999999999289, 18.50207713769457030 ) ) ;
#13708 = CARTESIAN_POINT ( 'NONE',  ( -84.89290109919227234, -50.19755532556953881, 188.9997143009229319 ) ) ;
#13709 = VERTEX_POINT ( 'NONE', #97117 ) ;
#13710 = CARTESIAN_POINT ( 'NONE',  ( 32.83570112080939651, 321.3375211077556060, -5.977635819836277342 ) ) ;
#13711 = CIRCLE ( 'NONE', #74931, 2.000000000000000888 ) ;
#13712 = DIRECTION ( 'NONE',  ( 0.000000000000000000, 1.000000000000000000, 0.000000000000000000 ) ) ;
#13713 = ADVANCED_FACE ( 'NONE', ( #14591 ), #7563, .T. ) ;
#13714 = DIRECTION ( 'NONE',  ( -0.000000000000000000, 0.000000000000000000, -1.000000000000000000 ) ) ;
#13715 = CARTESIAN_POINT ( 'NONE',  ( -85.00188143483111958, -60.19486081470527949, -16.06405287040371022 ) ) ;
#13716 = VECTOR ( 'NONE', #70342, 1000.000000000000000 ) ;
#13717 = LINE ( 'NONE', #95197, #4621 ) ;
#13718 = DIRECTION ( 'NONE',  ( -1.000000000000000000, -1.224606353822377258E-16, -0.000000000000000000 ) ) ;
#13719 = EDGE_LOOP ( 'NONE', ( #48946, #15070, #37737, #73424, #91395, #55704 ) ) ;
#13720 = CARTESIAN_POINT ( 'NONE',  ( 18.88506184278858058, 49.99999999999999289, 60.74108293188928798 ) ) ;
#13721 = CARTESIAN_POINT ( 'NONE',  ( 11.54949964087943037, 7.317938515390196130, 9.354107198949744628 ) ) ;
#13722 = ADVANCED_FACE ( 'NONE', ( #24333 ), #30834, .T. ) ;
#13723 = CARTESIAN_POINT ( 'NONE',  ( 12.70248734011628500, -4.285714285714347760, 22.03900363279280583 ) ) ;
#13724 = CARTESIAN_POINT ( 'NONE',  ( -3.294958164819228319E-15, 5.948846446048902337, -2.696295709017757503 ) ) ;
#13725 = CONICAL_SURFACE ( 'NONE', #62038, 4.172000000000009479, 0.9599310885968813656 ) ;
#13726 = CARTESIAN_POINT ( 'NONE',  ( 71.63670194497801447, -60.00000000000009948, -34.46961289685300045 ) ) ;
#13727 = CARTESIAN_POINT ( 'NONE',  ( -79.92344898003078413, -42.96984901787218547, 149.1617487676861060 ) ) ;
#13728 = EDGE_LOOP ( 'NONE', ( #63913, #29247, #61287, #49194 ) ) ;
#13729 = DIRECTION ( 'NONE',  ( 0.000000000000000000, 1.000000000000000000, 0.000000000000000000 ) ) ;
#13730 = CARTESIAN_POINT ( 'NONE',  ( 99.10278221369861740, -57.62556558655981576, 204.1493198101848918 ) ) ;
#13731 = CARTESIAN_POINT ( 'NONE',  ( 53.87696817191028487, 49.99999999999999289, -33.03141454126155452 ) ) ;
#13732 = CARTESIAN_POINT ( 'NONE',  ( 37.51494864192159184, 304.8000952021329226, -7.711197196030624035 ) ) ;
#13733 = CARTESIAN_POINT ( 'NONE',  ( -13.99268144847940576, 6.886032338477331649, 7.933613737989179349 ) ) ;
#13734 = ORIENTED_EDGE ( 'NONE', *, *, #84601, .T. ) ;
#13735 = CARTESIAN_POINT ( 'NONE',  ( 0.000000000000000000, 0.000000000000000000, 0.000000000000000000 ) ) ;
#13736 = CARTESIAN_POINT ( 'NONE',  ( 32.02497098277217447, 438.9490321865996521, 23.64594912808245297 ) ) ;
#13738 = CARTESIAN_POINT ( 'NONE',  ( -104.4234376084712750, -52.71018726599390902, 156.3605036308566980 ) ) ;
#13737 = FACE_OUTER_BOUND ( 'NONE', #20437, .T. ) ;
#13739 = CARTESIAN_POINT ( 'NONE',  ( -1.320432766682874540E-15, -25.53125000204838813, 7.188101187500000044 ) ) ;
#13740 = CARTESIAN_POINT ( 'NONE',  ( -3.400000000000000355, 4.163799117101001052E-16, -6.418875477074183600 ) ) ;
#13741 = CARTESIAN_POINT ( 'NONE',  ( 9.999999999999996447, 15.00000000000000000, -10.00000000000000000 ) ) ;
#13742 = CARTESIAN_POINT ( 'NONE',  ( 7.099152780515114891, 41.70084721948487072, -59.82719249545999674 ) ) ;
#13743 = CARTESIAN_POINT ( 'NONE',  ( 26.10600422010756105, 37.18654406599299023, 8.037532972182770408 ) ) ;
#13744 = DIRECTION ( 'NONE',  ( 0.000000000000000000, 0.000000000000000000, 1.000000000000000000 ) ) ;
#13745 = CARTESIAN_POINT ( 'NONE',  ( -23.38389609179523632, 28.08052868592283957, -30.70617127781034483 ) ) ;
#13746 = EDGE_LOOP ( 'NONE', ( #80081, #83090, #34403, #95995, #3448 ) ) ;
#13747 = CARTESIAN_POINT ( 'NONE',  ( 44.08840282922852083, 485.7747746244177733, 4.178803824087951924 ) ) ;
#13749 = CARTESIAN_POINT ( 'NONE',  ( 27.18724732262417731, -22.09952160911303665, 29.24440674777745386 ) ) ;
#13748 = CARTESIAN_POINT ( 'NONE',  ( -63.58375344335239987, -14.21045842199425024, 93.96584349151677884 ) ) ;
#13750 = AXIS2_PLACEMENT_3D ( 'NONE', #19712, #12091, #36428 ) ;
#13751 = DIRECTION ( 'NONE',  ( 0.000000000000000000, 0.000000000000000000, -1.000000000000000000 ) ) ;
#13752 = ORIENTED_EDGE ( 'NONE', *, *, #11649, .T. ) ;
#13753 = UNCERTAINTY_MEASURE_WITH_UNIT (LENGTH_MEASURE( 1.000000000000000082E-05 ), #69387, 'distance_accuracy_value', 'NONE');
#13754 = EDGE_LOOP ( 'NONE', ( #101563, #57280, #100630, #89491 ) ) ;
#13755 = FILL_AREA_STYLE_COLOUR ( '', #68119 ) ;
#13756 = CARTESIAN_POINT ( 'NONE',  ( 47.33333333333331439, 59.99999999999999289, -23.66666666666664653 ) ) ;
#13757 = CARTESIAN_POINT ( 'NONE',  ( -44.14911905790385305, 464.3766534541991859, 9.623404994945861546 ) ) ;
#13758 = DIRECTION ( 'NONE',  ( -1.000000000000000000, 0.000000000000000000, 0.000000000000000000 ) ) ;
#13759 = CARTESIAN_POINT ( 'NONE',  ( 0.000000000000000000, 3.004629197474323585E-15, 8.000000000000000000 ) ) ;
#13760 = CARTESIAN_POINT ( 'NONE',  ( 0.2960616276314126383, 18.79208194970808776, -49.28345773665818541 ) ) ;
#13761 = ORIENTED_EDGE ( 'NONE', *, *, #6457, .F. ) ;
#13762 =( NAMED_UNIT ( * ) SI_UNIT ( $, .STERADIAN. ) SOLID_ANGLE_UNIT ( ) );
#13763 = DIRECTION ( 'NONE',  ( -1.000000000000000000, -1.224606353822377258E-16, -0.000000000000000000 ) ) ;
#13764 = CARTESIAN_POINT ( 'NONE',  ( -13.29119999941515218, 24.23229826355910177, 3.185837010029002769 ) ) ;
#13765 = CARTESIAN_POINT ( 'NONE',  ( 7.500000000000000888, -2.930060224340425901, -0.4701183149080217505 ) ) ;
#13766 = CARTESIAN_POINT ( 'NONE',  ( 81.13768354825626261, -29.99999999999999645, 1.847970586771182644 ) ) ;
#13767 = CARTESIAN_POINT ( 'NONE',  ( 17.33349330513380337, -4.000000000000000888, 4.898587196589416773E-16 ) ) ;
#13768 = VERTEX_POINT ( 'NONE', #80932 ) ;
#13769 = ADVANCED_FACE ( 'NONE', ( #22740 ), #72832, .T. ) ;
#13770 = AXIS2_PLACEMENT_3D ( 'NONE', #49012, #92141, #100762 ) ;
#13771 = ORIENTED_EDGE ( 'NONE', *, *, #46719, .F. ) ;
#13772 = ORIENTED_EDGE ( 'NONE', *, *, #28690, .T. ) ;
#13773 = DIRECTION ( 'NONE',  ( -0.000000000000000000, -0.000000000000000000, -1.000000000000000000 ) ) ;
#13774 = DIRECTION ( 'NONE',  ( 1.224646799147352468E-16, 0.000000000000000000, -1.000000000000000000 ) ) ;
#13775 = LINE ( 'NONE', #94190, #94813 ) ;
#13776 = CARTESIAN_POINT ( 'NONE',  ( -43.65265878650696862, 415.2984488955513598, 15.97998194705296093 ) ) ;
#13777 = CARTESIAN_POINT ( 'NONE',  ( -46.00000000000000000, 488.0072389889709257, 1.487873763370969327 ) ) ;
#13778 = CARTESIAN_POINT ( 'NONE',  ( 6.683837171061802529, -3.955946848495957457, 6.851900933636990487 ) ) ;
#13780 = ORIENTED_EDGE ( 'NONE', *, *, #23812, .T. ) ;
#13779 = PRESENTATION_LAYER_ASSIGNMENT (  '', '', ( #25849 ) ) ;
#13782 = EDGE_CURVE ( 'NONE', #19325, #45319, #14695, .T. ) ;
#13781 = CARTESIAN_POINT ( 'NONE',  ( 2.617478844989858722, 48.00000000000000000, -94.73972676610448218 ) ) ;
#13783 = EDGE_LOOP ( 'NONE', ( #77580, #88427, #82724, #49959, #2734 ) ) ;
#13784 = DIRECTION ( 'NONE',  ( 0.000000000000000000, 1.000000000000000000, 0.000000000000000000 ) ) ;
#13785 = DIRECTION ( 'NONE',  ( 0.6293714829493385343, 0.5427490687641790545, 0.5561609342679212364 ) ) ;
#13786 = CARTESIAN_POINT ( 'NONE',  ( 32.61650669486618881, -3.999999999999998224, 0.000000000000000000 ) ) ;
#13787 = CARTESIAN_POINT ( 'NONE',  ( 1.047247153709808698, 296.8411687940693469, -10.00073012113939086 ) ) ;
#13788 = CARTESIAN_POINT ( 'NONE',  ( 62.48344698558671695, -53.38692339959598598, 85.99248783803911067 ) ) ;
#13789 = ORIENTED_EDGE ( 'NONE', *, *, #46985, .T. ) ;
#13791 = ADVANCED_FACE ( 'NONE', ( #76639 ), #35382, .F. ) ;
#13790 = AXIS2_PLACEMENT_3D ( 'NONE', #47462, #95499, #39924 ) ;
#13792 = CARTESIAN_POINT ( 'NONE',  ( 39.86313086746753243, 464.8578212083490371, 17.96044624995279193 ) ) ;
#13793 = CARTESIAN_POINT ( 'NONE',  ( -65.78405188338429355, -37.94845061455978907, -32.58029113018389467 ) ) ;
#13794 = CYLINDRICAL_SURFACE ( 'NONE', #48909, 13.00000000000003730 ) ;
#13795 = B_SPLINE_CURVE_WITH_KNOTS ( 'NONE', 3,
 ( #45633, #27363, #78508, #12179, #44574, #4107, #2490, #76922, #4642, #77464, #35439, #18723, #68310, #3033, #60241, #37034, #94180, #70437, #3577, #69902, #102801, #69380, #61832, #51577, #29479, #92573, #36512, #35982, #93110, #84493, #10585, #102262, #19283, #52109, #85021, #11104 ),
 .UNSPECIFIED., .F., .F.,
 ( 4, 2, 2, 2, 2, 2, 2, 2, 2, 2, 2, 2, 2, 2, 2, 2, 2, 4 ),
 ( 0.01291936762762758983, 0.01372441420841339667, 0.01452946078919920350, 0.01533450736998501034, 0.01613955395077081717, 0.01694460053155662227, 0.01774964711234243084, 0.01855469369312823594, 0.01935974027391404451, 0.02016478685469984961, 0.02096983343548565470, 0.02177488001627146327, 0.02257992659705727184, 0.02338497317784307694, 0.02419001975862888204, 0.02459254304902178806, 0.02499506633941468714, 0.02580011292020053387 ),
 .UNSPECIFIED. ) ;
#13796 = CONICAL_SURFACE ( 'NONE', #22470, 7.000000000000000000, 0.9599310885968753704 ) ;
#13797 = CARTESIAN_POINT ( 'NONE',  ( -9.773556239149636227, 51.26923793256161588, 3.090446767225991209 ) ) ;
#13798 = VERTEX_POINT ( 'NONE', #31879 ) ;
#13799 = AXIS2_PLACEMENT_3D ( 'NONE', #52960, #84268, #35212 ) ;
#13800 =( NAMED_UNIT ( * ) SI_UNIT ( $, .STERADIAN. ) SOLID_ANGLE_UNIT ( ) );
#13801 = CARTESIAN_POINT ( 'NONE',  ( 47.14764774813721715, 18.53760837137042472, 14.71662980465857906 ) ) ;
#13802 = CARTESIAN_POINT ( 'NONE',  ( -25.56287369367873197, -60.00000000000002132, -35.59544240314404107 ) ) ;
#13803 = DIRECTION ( 'NONE',  ( 0.000000000000000000, 0.000000000000000000, -1.000000000000000000 ) ) ;
#13804 = CARTESIAN_POINT ( 'NONE',  ( 3.313708498984762052, -31.90625000409677270, -8.000000000000000000 ) ) ;
#13805 = CARTESIAN_POINT ( 'NONE',  ( 8.000000000000000000, -4.999999999999998224, 2.094395098902538166 ) ) ;
#13806 = CARTESIAN_POINT ( 'NONE',  ( 85.77546328330258518, -61.05395614131151660, 194.1409842555038097 ) ) ;
#13807 = CARTESIAN_POINT ( 'NONE',  ( -5.202336047186821411, 4.778347419875773383, -25.44939864730328338 ) ) ;
#13808 = VECTOR ( 'NONE', #8281, 1000.000000000000114 ) ;
#13809 = CARTESIAN_POINT ( 'NONE',  ( -9.316042626355404366, 11.20129626813108636, 4.999999999999999112 ) ) ;
#13810 = CARTESIAN_POINT ( 'NONE',  ( 6.928203230275508773, -10.00000000000001066, -4.000000000000000000 ) ) ;
#13811 = CARTESIAN_POINT ( 'NONE',  ( -6.231493956936419387, 147.8264543773111654, 5.000000000000000000 ) ) ;
#13812 = VERTEX_POINT ( 'NONE', #24851 ) ;
#13813 = CARTESIAN_POINT ( 'NONE',  ( 13.56225034990342948, -52.22121833032962002, 23.52491571494838851 ) ) ;
#13814 = CARTESIAN_POINT ( 'NONE',  ( 27.10511071441176156, 34.47735702144343861, -10.05698433968637673 ) ) ;
#13815 = CARTESIAN_POINT ( 'NONE',  ( 12.95434620903975365, -59.99999999999999289, 39.71337736509555327 ) ) ;
#13816 = CARTESIAN_POINT ( 'NONE',  ( -99.12369170486120140, -29.99999999999999289, 145.9994480237029961 ) ) ;
#13817 = EDGE_CURVE ( 'NONE', #66563, #79201, #20752, .T. ) ;
#13818 = DIRECTION ( 'NONE',  ( -1.000000000000000000, 0.000000000000000000, 0.000000000000000000 ) ) ;
#13819 = CARTESIAN_POINT ( 'NONE',  ( 61.52046739279862209, -57.67782001033483397, 112.8653612915162086 ) ) ;
#13820 = AXIS2_PLACEMENT_3D ( 'NONE', #59887, #70084, #69562 ) ;
#13821 = CARTESIAN_POINT ( 'NONE',  ( -0.4145643374704980344, 25.19212045144282541, -40.68227741578153456 ) ) ;
#13822 = ADVANCED_FACE ( 'NONE', ( #49627 ), #32418, .F. ) ;
#13823 = EDGE_CURVE ( 'NONE', #2814, #68944, #1592, .T. ) ;
#13824 = CARTESIAN_POINT ( 'NONE',  ( -40.69645897022445524, 459.9644416451193933, 1.990281397237554151 ) ) ;
#13825 = AXIS2_PLACEMENT_3D ( 'NONE', #88876, #106639, #95911 ) ;
#13826 = CARTESIAN_POINT ( 'NONE',  ( -18.17171551426997667, 50.00000000000001421, 61.67088195560315711 ) ) ;
#13827 = CARTESIAN_POINT ( 'NONE',  ( -9.673800154115149041, 15.30085158940939039, 2.563280883359885909 ) ) ;
#13828 = CARTESIAN_POINT ( 'NONE',  ( 43.71503333927361723, 486.3083204931234604, 5.911991965207032962 ) ) ;
#13829 = DIRECTION ( 'NONE',  ( 1.000000000000000000, 0.000000000000000000, 0.000000000000000000 ) ) ;
#13830 = FILL_AREA_STYLE ('',( #47262 ) ) ;
#13831 = CARTESIAN_POINT ( 'NONE',  ( -9.165151389911679658, 105.0000000000000000, 4.000000000000001776 ) ) ;
#13832 =( NAMED_UNIT ( * ) SI_UNIT ( $, .STERADIAN. ) SOLID_ANGLE_UNIT ( ) );
#13833 = ORIENTED_EDGE ( 'NONE', *, *, #56229, .T. ) ;
#13834 = CARTESIAN_POINT ( 'NONE',  ( 17.49999999999741007, 49.48689581941909665, 62.41113125630858605 ) ) ;
#13835 = CARTESIAN_POINT ( 'NONE',  ( 41.68543143493056391, 436.0813452458257871, 20.68254226408532404 ) ) ;
#13836 = CARTESIAN_POINT ( 'NONE',  ( -15.78049985857718163, -46.43928016077322951, 31.81775410195077924 ) ) ;
#13838 = CARTESIAN_POINT ( 'NONE',  ( 0.000000000000000000, 0.000000000000000000, -3.500000000000000000 ) ) ;
#13837 = LINE ( 'NONE', #94797, #37943 ) ;
#13839 = ORIENTED_EDGE ( 'NONE', *, *, #41645, .T. ) ;
#13840 = AXIS2_PLACEMENT_3D ( 'NONE', #15475, #64056, #40285 ) ;
#13841 = CARTESIAN_POINT ( 'NONE',  ( 9.833493305133805151, -4.000000000000000888, 4.898587196589416773E-16 ) ) ;
#13842 = FACE_OUTER_BOUND ( 'NONE', #6854, .T. ) ;
#13843 = DIRECTION ( 'NONE',  ( -1.000000000000000000, 0.000000000000000000, 0.000000000000000000 ) ) ;
#13844 = DIRECTION ( 'NONE',  ( -0.6297424739191580523, 0.1980345732175763651, -0.7511369544581807389 ) ) ;
#13845 = CARTESIAN_POINT ( 'NONE',  ( 61.63246250162482909, -59.99999999999999289, 106.0070534118292755 ) ) ;
#13846 = DIRECTION ( 'NONE',  ( 0.000000000000000000, 0.000000000000000000, -1.000000000000000000 ) ) ;
#13847 = ORIENTED_EDGE ( 'NONE', *, *, #41292, .F. ) ;
#13848 = FACE_OUTER_BOUND ( 'NONE', #24543, .T. ) ;
#13849 = CARTESIAN_POINT ( 'NONE',  ( 27.33349330513380693, 1.593028355512270962E-15, 0.000000000000000000 ) ) ;
#13850 = B_SPLINE_CURVE_WITH_KNOTS ( 'NONE', 3,
 ( #83345, #40231, #97932, #82818, #98457, #24085, #48834, #81724, #73646, #33761, #7851, #788, #41823, #57998, #25140, #58556, #40756, #260, #32703, #106550, #66633, #99518 ),
 .UNSPECIFIED., .F., .F.,
 ( 4, 2, 2, 2, 2, 2, 2, 2, 2, 2, 4 ),
 ( 2.469733450048283490E-18, 0.0009764592657812548029, 0.001464688898671880849, 0.001952918531562507004, 0.002929377797343762132, 0.003905837063125017043, 0.004882296328906272388, 0.005858755594687526866, 0.006835214860468781344, 0.007323444493359409016, 0.007811674126250036689 ),
 .UNSPECIFIED. ) ;
#13851 = DIRECTION ( 'NONE',  ( 0.000000000000000000, 0.000000000000000000, -1.000000000000000000 ) ) ;
#13852 = EDGE_CURVE ( 'NONE', #50280, #74417, #90228, .T. ) ;
#13853 = CARTESIAN_POINT ( 'NONE',  ( 3.443305032968370760, 124.1406189207604172, -4.999999999999999112 ) ) ;
#13854 = ORIENTED_EDGE ( 'NONE', *, *, #70678, .T. ) ;
#13855 = EDGE_LOOP ( 'NONE', ( #42750, #8531, #23802, #20332, #8080, #100520 ) ) ;
#13856 = CARTESIAN_POINT ( 'NONE',  ( -29.98402147317631972, 322.2345601114735700, 14.46678133052209425 ) ) ;
#13857 = VERTEX_POINT ( 'NONE', #53613 ) ;
#13858 = CARTESIAN_POINT ( 'NONE',  ( 22.07841018086242357, 305.2842913584914299, 9.030126516642127399 ) ) ;
#13859 = VECTOR ( 'NONE', #90855, 1000.000000000000227 ) ;
#13860 = CARTESIAN_POINT ( 'NONE',  ( 3.313708498984761608, -13.90625000409677092, -8.000000000000000000 ) ) ;
#13861 = CARTESIAN_POINT ( 'NONE',  ( 3.313708498984722972, -12.40625000409676737, -8.000000000000040856 ) ) ;
#13862 = ORIENTED_EDGE ( 'NONE', *, *, #49055, .T. ) ;
#13863 =( NAMED_UNIT ( * ) PLANE_ANGLE_UNIT ( ) SI_UNIT ( $, .RADIAN. ) );
#13864 = CARTESIAN_POINT ( 'NONE',  ( 4.999999999999959144, -12.50629439489329364, 11.30430831584017604 ) ) ;
#13865 = CARTESIAN_POINT ( 'NONE',  ( -80.03450769258309094, -60.00000000000743228, 199.7433096331160698 ) ) ;
#13866 = STYLED_ITEM ( 'NONE', ( #76310 ), #79178 ) ;
#13867 = CARTESIAN_POINT ( 'NONE',  ( 46.00000000000000000, 488.2691388620956445, 2.804837155789654979 ) ) ;
#13868 = CARTESIAN_POINT ( 'NONE',  ( 74.50860608132113327, -60.00000000000000000, 177.2089907105977886 ) ) ;
#13869 = CARTESIAN_POINT ( 'NONE',  ( 13.98998652022258682, -5.000000000000000000, 8.603073681314127086 ) ) ;
#13870 = FACE_OUTER_BOUND ( 'NONE', #97221, .T. ) ;
#13872 = CARTESIAN_POINT ( 'NONE',  ( 9.120188071644534489, -29.02951018409794770, 28.72938299554262542 ) ) ;
#13871 = CARTESIAN_POINT ( 'NONE',  ( -108.9224886339666085, -60.00000000000004263, 119.6925845435806650 ) ) ;
#13873 = DIRECTION ( 'NONE',  ( 0.000000000000000000, -1.000000000000000000, 0.000000000000000000 ) ) ;
#13874 = CARTESIAN_POINT ( 'NONE',  ( -45.55848940769042343, -42.98694371728178254, 45.30845615562359541 ) ) ;
#13875 = FACE_OUTER_BOUND ( 'NONE', #98099, .T. ) ;
#13876 = ORIENTED_EDGE ( 'NONE', *, *, #84176, .T. ) ;
#13877 = CARTESIAN_POINT ( 'NONE',  ( 1.250982008297754300, 10.43118007883091103, -50.60792131318659415 ) ) ;
#13878 = CARTESIAN_POINT ( 'NONE',  ( 16.75187969033571989, 37.11970326878314097, 21.80698433968582961 ) ) ;
#13879 = FACE_OUTER_BOUND ( 'NONE', #62993, .T. ) ;
#13880 = ORIENTED_EDGE ( 'NONE', *, *, #98804, .T. ) ;
#13881 = CARTESIAN_POINT ( 'NONE',  ( -15.71446116343726906, -4.300810710832455364, 14.38220008862084143 ) ) ;
#13882 = ORIENTED_EDGE ( 'NONE', *, *, #99777, .F. ) ;
#13883 = CARTESIAN_POINT ( 'NONE',  ( 84.08753936534863271, -30.00000000001337952, 196.4773746771908236 ) ) ;
#13884 = DIRECTION ( 'NONE',  ( -1.000000000000000000, -1.224606353822377258E-16, -0.000000000000000000 ) ) ;
#13885 = CARTESIAN_POINT ( 'NONE',  ( 0.000000000000000000, 1.502314598737159228E-15, -8.000000000000000000 ) ) ;
#13886 = CARTESIAN_POINT ( 'NONE',  ( 99.09030147775226283, -29.99999999999999645, 188.6124528200056432 ) ) ;
#13887 = DIRECTION ( 'NONE',  ( 0.000000000000000000, 0.000000000000000000, 1.000000000000000000 ) ) ;
#13888 = ORIENTED_EDGE ( 'NONE', *, *, #104526, .T. ) ;
#13889 = EDGE_CURVE ( 'NONE', #6205, #699, #64615, .T. ) ;
#13890 = ORIENTED_EDGE ( 'NONE', *, *, #22361, .F. ) ;
#13891 = ORIENTED_EDGE ( 'NONE', *, *, #59427, .F. ) ;
#13892 = CARTESIAN_POINT ( 'NONE',  ( -27.10511071441183262, 36.88665068479722464, 7.556984339686156460 ) ) ;
#13893 = DIRECTION ( 'NONE',  ( -0.5735764363510497121, 0.8191520442889892450, 1.003171929053521665E-16 ) ) ;
#13894 = AXIS2_PLACEMENT_3D ( 'NONE', #81641, #74094, #180 ) ;
#13895 = CARTESIAN_POINT ( 'NONE',  ( 0.000000000000000000, 294.8518027762758038, 9.936999415352289589 ) ) ;
#13896 = EDGE_CURVE ( 'NONE', #36313, #65228, #104352, .T. ) ;
#13897 = ORIENTED_EDGE ( 'NONE', *, *, #97311, .F. ) ;
#13899 = EDGE_CURVE ( 'NONE', #24875, #55315, #48599, .T. ) ;
#13898 = DIRECTION ( 'NONE',  ( 1.000000000000000000, 1.224606353822377258E-16, 0.000000000000000000 ) ) ;
#13900 = CIRCLE ( 'NONE', #29438, 4.000000000000001776 ) ;
#13901 = ORIENTED_EDGE ( 'NONE', *, *, #53294, .F. ) ;
#13902 = FACE_OUTER_BOUND ( 'NONE', #76896, .T. ) ;
#13903 = CARTESIAN_POINT ( 'NONE',  ( 105.2827503557284530, -38.38876419932554285, 197.1931609343118055 ) ) ;
#13904 = CARTESIAN_POINT ( 'NONE',  ( 14.83349330513380337, 1.593028355512270567E-15, 0.000000000000000000 ) ) ;
#13905 = CARTESIAN_POINT ( 'NONE',  ( 86.97481562723852733, -60.21415714265000929, -9.168737641558012186 ) ) ;
#13906 = CARTESIAN_POINT ( 'NONE',  ( 56.96819746998301781, -37.99999999999999289, 64.01309078521055085 ) ) ;
#13907 = CARTESIAN_POINT ( 'NONE',  ( 31.47235159143802719, 326.8924023395367158, 15.83378027818456069 ) ) ;
#13908 = CARTESIAN_POINT ( 'NONE',  ( -42.90606796452293992, 465.0680163534665326, 12.12009592787024559 ) ) ;
#13909 = LINE ( 'NONE', #103470, #79192 ) ;
#13910 = ADVANCED_FACE ( 'NONE', ( #53091 ), #87101, .T. ) ;
#13911 = EDGE_CURVE ( 'NONE', #105180, #76218, #37344, .T. ) ;
#13912 = CARTESIAN_POINT ( 'NONE',  ( -40.11988102503829623, 460.2461986766760447, 2.235918385955120158 ) ) ;
#13913 = FACE_OUTER_BOUND ( 'NONE', #13561, .T. ) ;
#13914 = ORIENTED_EDGE ( 'NONE', *, *, #66865, .F. ) ;
#13915 = CARTESIAN_POINT ( 'NONE',  ( -9.907626560209530808, 15.45483377860037777, -1.400881274228119144 ) ) ;
#13916 = CARTESIAN_POINT ( 'NONE',  ( -34.86856670768426625, 461.8421341769301876, 3.992206518671553628 ) ) ;
#13917 = CIRCLE ( 'NONE', #41489, 12.00000000000001066 ) ;
#13918 = CARTESIAN_POINT ( 'NONE',  ( -25.85367364129496082, 37.19423504344951681, 8.748924795912675023 ) ) ;
#13919 = ORIENTED_EDGE ( 'NONE', *, *, #14896, .T. ) ;
#13920 = DIRECTION ( 'NONE',  ( 0.000000000000000000, 0.000000000000000000, 1.000000000000000000 ) ) ;
#13921 = CARTESIAN_POINT ( 'NONE',  ( -35.29817125695181801, 303.6633776229971318, 3.966975762445377196 ) ) ;
#13922 = COLOUR_RGB ( '', 0.09019608, 0.27058824, 0.51372549) ;
#13923 = DIRECTION ( 'NONE',  ( 0.000000000000000000, -1.000000000000000000, 0.000000000000000000 ) ) ;
#13924 = CARTESIAN_POINT ( 'NONE',  ( 0.01372220897661389702, -5.309964801958108715, 3.802871176606130721 ) ) ;
#13925 = CARTESIAN_POINT ( 'NONE',  ( 5.656854249492378806, -14.18749999999999112, 5.656854249492381470 ) ) ;
#13926 = CARTESIAN_POINT ( 'NONE',  ( -45.71963733757689852, -30.00000000000002842, 56.30991746768104633 ) ) ;
#13927 = DIRECTION ( 'NONE',  ( 0.06744659395759022846, -0.6445107564563566926, -0.7616146281260456341 ) ) ;
#13928 = ORIENTED_EDGE ( 'NONE', *, *, #74003, .T. ) ;
#13929 = CARTESIAN_POINT ( 'NONE',  ( 84.44843645170369939, -46.56741310714842541, 186.0904281661588300 ) ) ;
#13930 = CARTESIAN_POINT ( 'NONE',  ( 6.394337469123806628, -7.552703473009533042, -1.902911509106785533E-15 ) ) ;
#13931 = FILL_AREA_STYLE ('',( #35070 ) ) ;
#13932 = ORIENTED_EDGE ( 'NONE', *, *, #65003, .T. ) ;
#13933 = CARTESIAN_POINT ( 'NONE',  ( 94.08407939083754457, -57.67277868574831245, 20.70298615612919946 ) ) ;
#13934 = AXIS2_PLACEMENT_3D ( 'NONE', #18337, #99758, #35059 ) ;
#13935 = CARTESIAN_POINT ( 'NONE',  ( 35.75766626156808314, 437.8288023593613616, 4.424845182004494504 ) ) ;
#13936 = FACE_OUTER_BOUND ( 'NONE', #77747, .T. ) ;
#13937 = CARTESIAN_POINT ( 'NONE',  ( -11.52459393585250069, -23.01655209608192720, -38.54135265537715327 ) ) ;
#13938 =( BOUNDED_SURFACE ( )  B_SPLINE_SURFACE ( 3, 2, ( 
 ( #77642, #71130, #103502 ),
 ( #45803, #28589, #3220 ),
 ( #86285, #37208, #36691 ),
 ( #37749, #60936, #19979 ),
 ( #87334, #101905, #5350 ),
 ( #78680, #62009, #70077 ),
 ( #85751, #12356, #78161 ),
 ( #69554, #102978, #52824 ),
 ( #13410, #94902, #21043 ),
 ( #29654, #104022, #38271 ) ),
 .UNSPECIFIED., .F., .F., .F. ) 
 B_SPLINE_SURFACE_WITH_KNOTS ( ( 4, 2, 2, 2, 4 ),
 ( 3, 3 ),
 ( -1.185673698477823590E-05, 0.001059589481406208620, 0.002131035699797195326, 0.003202481918188181814, 0.004273928136579168736 ),
 ( 0.000000000000000000, 1.000000000000000000 ),
 .UNSPECIFIED. ) 
 GEOMETRIC_REPRESENTATION_ITEM ( )  RATIONAL_B_SPLINE_SURFACE ( (
 ( 1.000000000000000000, 1.000000000000000000, 1.000000000000000000),
 ( 1.000000000000000000, 0.9999922502423259640, 1.000000000000000000),
 ( 1.000000000000000000, 0.9961090584666545400, 1.000000000000000000),
 ( 1.000000000000000000, 0.9800114100223529245, 1.000000000000000000),
 ( 1.000000000000000000, 0.9677016975217730410, 1.000000000000000000),
 ( 1.000000000000000000, 0.9345728642048093393, 1.000000000000000000),
 ( 1.000000000000000000, 0.9137480076086517133, 1.000000000000000000),
 ( 1.000000000000000000, 0.8628371017894029826, 1.000000000000000000),
 ( 1.000000000000000000, 0.8327438998405827242, 1.000000000000000000),
 ( 1.000000000000000000, 0.7973879088788905500, 1.000000000000000000) ) ) 
 REPRESENTATION_ITEM ( '' )  SURFACE ( )  );
#13939 = COLOUR_RGB ( '', 0.08235294, 0.09019608, 0.10196078) ;
#13940 = B_SPLINE_CURVE_WITH_KNOTS ( 'NONE', 3,
 ( #73174, #73719, #34378, #65644, #66165, #858, #50500, #48903, #66708, #99048, #65107, #49980, #100129, #26296, #8986, #32228, #41890, #59156, #92039, #106079, #16023, #24157, #98529, #7924, #106622, #32772, #24675, #57528, #45109, #69901, #34906, #85567, #67771, #20873, #42967, #51576, #26819, #69379, #53707, #10584, #60763, #37033, #19282, #59692, #102260, #84491, #28409, #27896, #3031, #86639, #93108, #86107, #101728, #3574, #92571, #77988, #43500, #52635, #61831, #76377, #100658, #11643, #2488, #4105, #93651, #68309, #75859, #35981, #19799, #44573 ),
 .UNSPECIFIED., .F., .F.,
 ( 4, 2, 2, 2, 1, 1, 1, 1, 1, 2, 2, 2, 2, 2, 1, 1, 1, 1, 1, 1, 2, 2, 2, 2, 2, 2, 1, 1, 1, 1, 1, 1, 2, 2, 2, 2, 2, 1, 1, 1, 1, 1, 2, 2, 2, 4 ),
 ( 0.000000000000000000, 0.06249999999979889698, 0.09374999999969835240, 0.1093749999996480732, 0.1171874999996228711, 0.1210937499996100064, 0.1230468749996035255, 0.1240234374996002781, 0.1245117187495986960, 0.1247558593745979189, 0.1249999999995971278, 0.1874999999994058364, 0.2187499999993102739, 0.2343749999992621735, 0.2421874999992381372, 0.2460937499992256472, 0.2480468749992193744, 0.2490234374992167377, 0.2495117187492148225, 0.2497558593742143507, 0.2498779296867145727, 0.2499999999992147948, 0.3124999999992655875, 0.3749999999993163802, 0.4374999999993672284, 0.4687499999993925970, 0.4843749999994054756, 0.4921874999994120814, 0.4960937499994153010, 0.4980468749994169664, 0.4990234374994177990, 0.4995117187494180211, 0.4997558593744183542, 0.4999999999994186872, 0.6249999999995474731, 0.6874999999996117550, 0.7187499999996438405, 0.7343749999996600497, 0.7421874999996682654, 0.7460937499996723732, 0.7480468749996741495, 0.7490234374996752598, 0.7495117187496758149, 0.7499999999996762590, 0.8749999999998381295, 1.000000000000000000 ),
 .UNSPECIFIED. ) ;
#13941 = VECTOR ( 'NONE', #71665, 1000.000000000000000 ) ;
#13942 = CARTESIAN_POINT ( 'NONE',  ( 8.790745035565722176, -19.73282221811500037, 35.28722622678527898 ) ) ;
#13943 =( GEOMETRIC_REPRESENTATION_CONTEXT ( 3 ) GLOBAL_UNCERTAINTY_ASSIGNED_CONTEXT ( ( #85020 ) ) GLOBAL_UNIT_ASSIGNED_CONTEXT ( ( #62566, #37256, #29694 ) ) REPRESENTATION_CONTEXT ( 'NONE', 'WORKASPACE' ) );
#13944 = CARTESIAN_POINT ( 'NONE',  ( 10.00000000000000000, -5.000000000000000000, -2.617993873628171375 ) ) ;
#13945 = CARTESIAN_POINT ( 'NONE',  ( 0.2779000157839520702, 8.820699686765056668, -7.928862157988307402 ) ) ;
#13947 = CARTESIAN_POINT ( 'NONE',  ( -15.18386540887443914, 5.234509037293391565, 6.306189099687723676 ) ) ;
#13946 = CARTESIAN_POINT ( 'NONE',  ( 0.000000000000000000, 4.898587196589413815E-16, -4.000000000000000888 ) ) ;
#13948 = EDGE_CURVE ( 'NONE', #15446, #7894, #26851, .T. ) ;
#13949 =( GEOMETRIC_REPRESENTATION_CONTEXT ( 3 ) GLOBAL_UNCERTAINTY_ASSIGNED_CONTEXT ( ( #33263 ) ) GLOBAL_UNIT_ASSIGNED_CONTEXT ( ( #48945, #16599, #96990 ) ) REPRESENTATION_CONTEXT ( 'NONE', 'WORKASPACE' ) );
#13950 = FACE_BOUND ( 'NONE', #52472, .T. ) ;
#13951 =( NAMED_UNIT ( * ) SI_UNIT ( $, .STERADIAN. ) SOLID_ANGLE_UNIT ( ) );
#13952 = CARTESIAN_POINT ( 'NONE',  ( 9.373884331924955404, 15.95332971149351842, -3.487646406148425804 ) ) ;
#13953 = FACE_OUTER_BOUND ( 'NONE', #53011, .T. ) ;
#13954 = CARTESIAN_POINT ( 'NONE',  ( -102.8326201182668029, -37.99999999999999289, 173.0413610677699694 ) ) ;
#13955 = VERTEX_POINT ( 'NONE', #22872 ) ;
#13956 = CARTESIAN_POINT ( 'NONE',  ( -7.852494914944515791, -0.7890738855012446873, 15.46605827214583329 ) ) ;
#13957 = CARTESIAN_POINT ( 'NONE',  ( 0.000000000000000000, 69.00000000000000000, 0.000000000000000000 ) ) ;
#13958 = LINE ( 'NONE', #97527, #80366 ) ;
#13959 = CARTESIAN_POINT ( 'NONE',  ( -50.82590375189641207, -47.40886325391449674, -29.75599597189977530 ) ) ;
#13960 = ORIENTED_EDGE ( 'NONE', *, *, #40811, .F. ) ;
#13961 = CIRCLE ( 'NONE', #91532, 4.000000000000000888 ) ;
#13962 = CARTESIAN_POINT ( 'NONE',  ( 7.847095227763524861, 4.129731495738483638, -7.493596212620240671 ) ) ;
#13963 = ORIENTED_EDGE ( 'NONE', *, *, #98620, .F. ) ;
#13964 = CIRCLE ( 'NONE', #74266, 5.000000000000001776 ) ;
#13965 = DIRECTION ( 'NONE',  ( 1.000000000000000000, -0.000000000000000000, 1.224646799147353207E-16 ) ) ;
#13966 = CYLINDRICAL_SURFACE ( 'NONE', #83826, 4.999999999999999112 ) ;
#13967 = CARTESIAN_POINT ( 'NONE',  ( -91.90010039950615806, -60.00000000000001421, -14.32662728741797054 ) ) ;
#13968 = ORIENTED_EDGE ( 'NONE', *, *, #28158, .T. ) ;
#13969 = CARTESIAN_POINT ( 'NONE',  ( 9.789044728060087408, 294.6486233851415477, -2.043184600578025201 ) ) ;
#13970 = CARTESIAN_POINT ( 'NONE',  ( -8.559508646656389885, 53.96349637827586321, -1.531152949374502859 ) ) ;
#13971 = CARTESIAN_POINT ( 'NONE',  ( -3.568931636294713439, -49.06947573042521071, 103.4741166605240323 ) ) ;
#13972 = ADVANCED_FACE ( 'NONE', ( #90229 ), #102644, .T. ) ;
#13974 = DIRECTION ( 'NONE',  ( 0.000000000000000000, 1.000000000000000000, 0.000000000000000000 ) ) ;
#13973 = CARTESIAN_POINT ( 'NONE',  ( 95.70911704725124025, 6.123233995736582872E-16, -5.000000000000011546 ) ) ;
#13975 = EDGE_CURVE ( 'NONE', #93114, #26330, #19998, .T. ) ;
#13976 = CARTESIAN_POINT ( 'NONE',  ( -80.44522044428813956, -49.91460793207095037, 162.4354708053286913 ) ) ;
#13977 = ORIENTED_EDGE ( 'NONE', *, *, #18780, .T. ) ;
#13978 = CARTESIAN_POINT ( 'NONE',  ( -13.52487676487832680, 0.000000000000000000, -10.38441970549514970 ) ) ;
#13979 = EDGE_LOOP ( 'NONE', ( #33977, #16376, #57665, #81588, #95670 ) ) ;
#13980 = ORIENTED_EDGE ( 'NONE', *, *, #26895, .T. ) ;
#13981 = CARTESIAN_POINT ( 'NONE',  ( 16.64670748672000755, -5.000000000000000000, -1.019662339603576440 ) ) ;
#13982 = B_SPLINE_CURVE_WITH_KNOTS ( 'NONE', 3,
 ( #67601, #42779, #9867, #10403 ),
 .UNSPECIFIED., .F., .F.,
 ( 4, 4 ),
 ( 0.000000000000000000, 0.0004475792522134777827 ),
 .UNSPECIFIED. ) ;
#13983 = SURFACE_STYLE_USAGE ( .BOTH. , #11869 ) ;
#13984 = FACE_OUTER_BOUND ( 'NONE', #91968, .T. ) ;
#13985 = ORIENTED_EDGE ( 'NONE', *, *, #100305, .F. ) ;
#13986 = AXIS2_PLACEMENT_3D ( 'NONE', #80099, #69382, #77993 ) ;
#13987 = CARTESIAN_POINT ( 'NONE',  ( -34.88692374364642035, 481.7037037884593360, 14.61727889479850617 ) ) ;
#13988 = CARTESIAN_POINT ( 'NONE',  ( -9.999999999999998224, 15.00000000000000000, 1.734723475976807489E-15 ) ) ;
#13989 = CARTESIAN_POINT ( 'NONE',  ( -108.9175987578229297, -57.66477069964600588, 197.8260142395344303 ) ) ;
#13990 = CARTESIAN_POINT ( 'NONE',  ( -9.988806003742208617, 294.6431196884677206, 0.5781234520571254532 ) ) ;
#13991 = CARTESIAN_POINT ( 'NONE',  ( 7.531577814756222656E-15, 0.000000000000000000, -61.50000000000000000 ) ) ;
#13992 = CARTESIAN_POINT ( 'NONE',  ( -13.59366797464709720, -51.99143461894139762, 23.64820470065338753 ) ) ;
#13993 = CARTESIAN_POINT ( 'NONE',  ( 95.02194560458454475, -59.99999999999987210, -3.233414228271875857 ) ) ;
#13994 = CARTESIAN_POINT ( 'NONE',  ( -44.76022593139747840, -29.99999999999992539, 54.38475608328532473 ) ) ;
#13995 = CARTESIAN_POINT ( 'NONE',  ( -56.19539967535489922, -18.67843576544961337, 54.42036842179090428 ) ) ;
#13996 = EDGE_LOOP ( 'NONE', ( #61365, #79710, #80191, #61905, #40012, #44100, #97901, #76306, #20082, #46460 ) ) ;
#13997 = DIRECTION ( 'NONE',  ( 1.000000000000000000, 0.000000000000000000, 0.000000000000000000 ) ) ;
#13998 = VERTEX_POINT ( 'NONE', #65951 ) ;
#13999 = CARTESIAN_POINT ( 'NONE',  ( -99.09551672418950830, -37.78131862766355198, 191.7927793575313160 ) ) ;
#14000 = CARTESIAN_POINT ( 'NONE',  ( 4.000000000000000000, 17.85270131633358304, 5.744562646538042827 ) ) ;
#14001 = ORIENTED_EDGE ( 'NONE', *, *, #22258, .F. ) ;
#14003 = B_SPLINE_CURVE_WITH_KNOTS ( 'NONE', 3,
 ( #16103, #58708, #49529, #8538 ),
 .UNSPECIFIED., .F., .F.,
 ( 4, 4 ),
 ( 0.000000000000000000, 0.002500010780266304685 ),
 .UNSPECIFIED. ) ;
#14002 = CARTESIAN_POINT ( 'NONE',  ( 18.91772294158841206, 48.18298762545486369, 62.18609455207796088 ) ) ;
#14004 = CARTESIAN_POINT ( 'NONE',  ( 90.24191362537470695, -38.39941249341406859, -15.35752588949901210 ) ) ;
#14005 = DIRECTION ( 'NONE',  ( 0.000000000000000000, -1.000000000000000000, 0.000000000000000000 ) ) ;
#14006 = CARTESIAN_POINT ( 'NONE',  ( 7.188101187500000044, -10.53125000204838457, 0.000000000000000000 ) ) ;
#14007 = VECTOR ( 'NONE', #71630, 1000.000000000000000 ) ;
#14008 = CARTESIAN_POINT ( 'NONE',  ( -0.9522838070410156730, 294.8487785428199004, 1.936375223474096519 ) ) ;
#14009 = DIRECTION ( 'NONE',  ( -1.000000000000000000, 0.000000000000000000, 0.000000000000000000 ) ) ;
#14011 = CARTESIAN_POINT ( 'NONE',  ( 59.60496295899294950, -30.00000000000001066, 65.94430785219442726 ) ) ;
#14010 = UNCERTAINTY_MEASURE_WITH_UNIT (LENGTH_MEASURE( 1.000000000000000082E-05 ), #80653, 'distance_accuracy_value', 'NONE');
#14012 = PRESENTATION_LAYER_ASSIGNMENT (  '', '', ( #209 ) ) ;
#14013 = DIRECTION ( 'NONE',  ( -1.000000000000000000, -1.224606353822377258E-16, -0.000000000000000000 ) ) ;
#14014 = CARTESIAN_POINT ( 'NONE',  ( 4.506266729858585229, -48.81716041225653413, 104.3949571352749643 ) ) ;
#14015 = CARTESIAN_POINT ( 'NONE',  ( 8.099999999999999645, 0.000000000000000000, 0.000000000000000000 ) ) ;
#14016 = AXIS2_PLACEMENT_3D ( 'NONE', #87756, #47789, #4710 ) ;
#14017 = ORIENTED_EDGE ( 'NONE', *, *, #4837, .T. ) ;
#14018 = ORIENTED_EDGE ( 'NONE', *, *, #92223, .T. ) ;
#14019 = CARTESIAN_POINT ( 'NONE',  ( 50.52129209761249484, -49.90308930700556544, 55.20093448208132969 ) ) ;
#14020 = CARTESIAN_POINT ( 'NONE',  ( -1.106297339054949314, 12.12138970700505958, 49.90201418493064267 ) ) ;
#14021 = VECTOR ( 'NONE', #6836, 999.9999999999998863 ) ;
#14022 = CARTESIAN_POINT ( 'NONE',  ( -5.890693798151878546, 14.30979422482011820, -3.781785903083254574 ) ) ;
#14023 = AXIS2_PLACEMENT_3D ( 'NONE', #63593, #77640, #96482 ) ;
#14024 = CARTESIAN_POINT ( 'NONE',  ( -109.0363367054505233, -38.35639537931302812, 190.0084180073488938 ) ) ;
#14025 = ORIENTED_EDGE ( 'NONE', *, *, #56668, .T. ) ;
#14026 = CARTESIAN_POINT ( 'NONE',  ( 91.43679786253925101, -38.39287896914650844, -8.456874844154592452 ) ) ;
#14027 = CARTESIAN_POINT ( 'NONE',  ( 10.06671572987654706, 15.03217639615420076, -10.38938273639670840 ) ) ;
#14028 = CARTESIAN_POINT ( 'NONE',  ( -7.150000000000001243, 41.64999999999999147, -68.91429205801802027 ) ) ;
#14029 = FACE_OUTER_BOUND ( 'NONE', #55580, .T. ) ;
#14030 = SURFACE_STYLE_FILL_AREA ( #46935 ) ;
#14031 = CARTESIAN_POINT ( 'NONE',  ( 29.68315524077034695, -1.200000000000000030E-05, 40.85535821593451544 ) ) ;
#14032 = CARTESIAN_POINT ( 'NONE',  ( 3.313708498984743844, -26.46875000409677270, 8.000000000000017764 ) ) ;
#14033 = CARTESIAN_POINT ( 'NONE',  ( 32.95646543402821749, 485.7809766657146611, 5.067016726498376755 ) ) ;
#14034 = FACE_OUTER_BOUND ( 'NONE', #40495, .T. ) ;
#14035 = CARTESIAN_POINT ( 'NONE',  ( -30.00000000000000000, 486.4444101590584637, 4.645498354854257883 ) ) ;
#14036 = CARTESIAN_POINT ( 'NONE',  ( 100.6213230593580050, -60.00000000000000000, 201.6927024307212548 ) ) ;
#14037 = EDGE_CURVE ( 'NONE', #34646, #43584, #80003, .T. ) ;
#14038 = ORIENTED_EDGE ( 'NONE', *, *, #18377, .F. ) ;
#14039 = CARTESIAN_POINT ( 'NONE',  ( 56.50624196457695803, -22.14518791754317206, 56.45264507296375456 ) ) ;
#14040 = EDGE_CURVE ( 'NONE', #103934, #102391, #116, .T. ) ;
#14041 = CARTESIAN_POINT ( 'NONE',  ( -32.76713765336180018, 299.3368522934601970, -9.004512236813274839 ) ) ;
#14042 = CARTESIAN_POINT ( 'NONE',  ( 7.045755811259134305, 31.30341603013552643, 3.790843699961854885 ) ) ;
#14043 = COLOUR_RGB ( '', 0.31764706, 0.68627451, 0.89019608) ;
#14044 = CARTESIAN_POINT ( 'NONE',  ( -8.000113193197767814, 25.99977361354138594, -0.2613481123984617849 ) ) ;
#14045 = ORIENTED_EDGE ( 'NONE', *, *, #99441, .F. ) ;
#14047 = CARTESIAN_POINT ( 'NONE',  ( -9.204611235795193025, -52.70218221418006976, 30.90985867601607850 ) ) ;
#14046 = CARTESIAN_POINT ( 'NONE',  ( -95.01326126541965778, -38.35584031613350930, 58.06921072743757861 ) ) ;
#14048 = DIRECTION ( 'NONE',  ( -1.000000000000000000, 0.000000000000000000, 0.000000000000000000 ) ) ;
#14049 = CARTESIAN_POINT ( 'NONE',  ( 30.96065734108625023, 348.7708920524887617, 19.04886383678881145 ) ) ;
#14050 = CARTESIAN_POINT ( 'NONE',  ( 3.313708498984762052, -30.21874999999999645, -8.000000000000000000 ) ) ;
#14051 = VECTOR ( 'NONE', #49027, 1000.000000000000000 ) ;
#14052 = CARTESIAN_POINT ( 'NONE',  ( -9.739726766104286781, -3.000000000000002665, -87.61747884499033034 ) ) ;
#14053 = STYLED_ITEM ( 'NONE', ( #101630 ), #104040 ) ;
#14054 = PRODUCT ( '14. Sleeve', '14. Sleeve', '', ( #41163 ) ) ;
#14055 = DIRECTION ( 'NONE',  ( -1.000000000000000000, -0.000000000000000000, -0.000000000000000000 ) ) ;
#14056 = VERTEX_POINT ( 'NONE', #39575 ) ;
#14057 = CARTESIAN_POINT ( 'NONE',  ( 83.47826123857470293, -39.47038229126598452, 174.2395583309989036 ) ) ;
#14058 = CARTESIAN_POINT ( 'NONE',  ( 9.209506619794041171, 139.6161984561731799, -1.301042606982606899E-15 ) ) ;
#14059 = CARTESIAN_POINT ( 'NONE',  ( -41.98109406947484246, 462.0607394890939759, 3.143716936936614470 ) ) ;
#14060 = ORIENTED_EDGE ( 'NONE', *, *, #103875, .F. ) ;
#14061 = CARTESIAN_POINT ( 'NONE',  ( -37.69154825673145837, 413.5836300137029298, 6.418259979187027398 ) ) ;
#14062 = CARTESIAN_POINT ( 'NONE',  ( 7.498343863766716133, -2.970317092009080895, -20.23009517155373871 ) ) ;
#14063 = CARTESIAN_POINT ( 'NONE',  ( 40.35113499395451697, 477.0942685543254242, -2.239294154288959948 ) ) ;
#14064 = DIRECTION ( 'NONE',  ( 0.000000000000000000, -1.000000000000000000, 0.000000000000000000 ) ) ;
#14065 = DIRECTION ( 'NONE',  ( 0.000000000000000000, 0.000000000000000000, -1.000000000000000000 ) ) ;
#14066 = CARTESIAN_POINT ( 'NONE',  ( -4.472135954999577834, 250.2732990351264561, -4.000000000000002665 ) ) ;
#14067 = ORIENTED_EDGE ( 'NONE', *, *, #34964, .F. ) ;
#14068 = CARTESIAN_POINT ( 'NONE',  ( -81.03185928260310789, -30.00000000000000000, 21.53690394037695555 ) ) ;
#14069 = CARTESIAN_POINT ( 'NONE',  ( -1.000000000000000000, -51.24344465336813670, 3.816021516725665030 ) ) ;
#14070 = CARTESIAN_POINT ( 'NONE',  ( 2.499999999999999556, -30.00000000000000000, 14.79019945774903633 ) ) ;
#14072 = CARTESIAN_POINT ( 'NONE',  ( -11.65716286615917952, 15.89043748982164139, -9.577315898548507178 ) ) ;
#14071 = CARTESIAN_POINT ( 'NONE',  ( -2.843030712961830186, -18.20086595765178927, 35.02953871394988283 ) ) ;
#14073 = EDGE_CURVE ( 'NONE', #36994, #95902, #48687, .T. ) ;
#14074 = CARTESIAN_POINT ( 'NONE',  ( 7.188101187499999156, -20.75000000204839523, 2.977408999572654924 ) ) ;
#14075 = CARTESIAN_POINT ( 'NONE',  ( -11.91432047156633622, 40.83906611472538373, 64.17585289266233417 ) ) ;
#14076 = CARTESIAN_POINT ( 'NONE',  ( -7.126148247341459019, 41.12758119229484066, -58.55282700859728351 ) ) ;
#14077 = EDGE_LOOP ( 'NONE', ( #52730, #10744, #78900, #27368, #95321 ) ) ;
#14078 = AXIS2_PLACEMENT_3D ( 'NONE', #631, #33598, #83187 ) ;
#14079 =( NAMED_UNIT ( * ) SI_UNIT ( $, .STERADIAN. ) SOLID_ANGLE_UNIT ( ) );
#14080 = CARTESIAN_POINT ( 'NONE',  ( 7.500000000000000000, 0.7723602884924073431, -7.026388801734293033 ) ) ;
#14081 = VECTOR ( 'NONE', #7548, 1000.000000000000000 ) ;
#14082 = CARTESIAN_POINT ( 'NONE',  ( -4.857429444120077378, 7.134197903804992080, -5.000000000000000000 ) ) ;
#14083 = EDGE_CURVE ( 'NONE', #48559, #88005, #23941, .T. ) ;
#14084 = SURFACE_SIDE_STYLE ('',( #69700 ) ) ;
#14085 = EDGE_CURVE ( 'NONE', #87776, #68832, #94020, .T. ) ;
#14086 = CARTESIAN_POINT ( 'NONE',  ( -37.56673239365851913, 25.75719283951025673, 10.95617127780993449 ) ) ;
#14087 = ORIENTED_EDGE ( 'NONE', *, *, #101283, .F. ) ;
#14088 = CARTESIAN_POINT ( 'NONE',  ( 15.75384615384615294, 4.172000000000003261, 5.109226446042759579E-16 ) ) ;
#14089 = CARTESIAN_POINT ( 'NONE',  ( 5.656854249492380582, -21.50000000409676915, -5.656854249492379694 ) ) ;
#14091 = EDGE_LOOP ( 'NONE', ( #72744, #66382 ) ) ;
#14090 = COLOUR_RGB ( '', 0.31764706, 0.68627451, 0.89019608) ;
#14092 = AXIS2_PLACEMENT_3D ( 'NONE', #21955, #46732, #70489 ) ;
#14093 = CARTESIAN_POINT ( 'NONE',  ( -1.150658033319299881E-13, -1.200000000000000030E-05, -51.75000000000000711 ) ) ;
#14094 = CARTESIAN_POINT ( 'NONE',  ( 6.338255145484064990, 2.729868969638910681, -6.500000000000574651 ) ) ;
#14095 = CARTESIAN_POINT ( 'NONE',  ( -112.0805244979449924, -60.00000000000000000, 178.3222598195121407 ) ) ;
#14096 = FACE_OUTER_BOUND ( 'NONE', #75947, .T. ) ;
#14097 = CARTESIAN_POINT ( 'NONE',  ( 30.12932728364529922, 334.4140447340107585, 17.11298374841474867 ) ) ;
#14098 = CARTESIAN_POINT ( 'NONE',  ( 6.496772124874876653, 53.67412401770713615, -6.918302629204984733 ) ) ;
#14099 = CARTESIAN_POINT ( 'NONE',  ( 17.37694393396142090, 34.80682117732449399, -21.96264255479069405 ) ) ;
#14100 = ADVANCED_FACE ( 'NONE', ( #56782 ), #47101, .F. ) ;
#14101 = CARTESIAN_POINT ( 'NONE',  ( -82.27752543006228336, -49.99667767229193771, 179.0212925606178374 ) ) ;
#14102 = ORIENTED_EDGE ( 'NONE', *, *, #64833, .T. ) ;
#14103 = CARTESIAN_POINT ( 'NONE',  ( 34.55488935567512243, 42.66466471040279629, -62.99488116903847867 ) ) ;
#14104 = ORIENTED_EDGE ( 'NONE', *, *, #7127, .F. ) ;
#14105 = SURFACE_STYLE_USAGE ( .BOTH. , #87498 ) ;
#14106 = ADVANCED_FACE ( 'NONE', ( #81061 ), #89706, .T. ) ;
#14107 = CARTESIAN_POINT ( 'NONE',  ( 5.910690929868579246, -68.86495906093195174, -1.065041252563907248 ) ) ;
#14108 = CARTESIAN_POINT ( 'NONE',  ( -83.78263966539077501, -45.26573403153773256, 18.52797371739886145 ) ) ;
#14109 = AXIS2_PLACEMENT_3D ( 'NONE', #65140, #40862, #7955 ) ;
#14110 = CARTESIAN_POINT ( 'NONE',  ( -11.62074180716757787, 304.6006955855707474, 8.883628396986859244 ) ) ;
#14111 = SURFACE_STYLE_USAGE ( .BOTH. , #77279 ) ;
#14112 = AXIS2_PLACEMENT_3D ( 'NONE', #67889, #66831, #27479 ) ;
#14113 = CARTESIAN_POINT ( 'NONE',  ( 8.224467148746322565, 36.45870262746143453, -4.999999999999998224 ) ) ;
#14114 = LINE ( 'NONE', #3925, #52810 ) ;
#14115 = CARTESIAN_POINT ( 'NONE',  ( 19.32152200343512760, 18.64316884711617561, -33.52312678240317467 ) ) ;
#14116 = ADVANCED_FACE ( 'NONE', ( #24475 ), #42346, .T. ) ;
#14117 = CARTESIAN_POINT ( 'NONE',  ( 94.89952817683000319, -60.00000000000002842, 205.0337064426678921 ) ) ;
#14118 = CARTESIAN_POINT ( 'NONE',  ( -90.16416446821634167, -14.21045842199442077, 52.56827875477732448 ) ) ;
#14119 = VECTOR ( 'NONE', #25702, 999.9999999999998863 ) ;
#14120 = CARTESIAN_POINT ( 'NONE',  ( -64.91042575604046760, -25.57878275972089099, 78.74603656798815621 ) ) ;
#14121 = ORIENTED_EDGE ( 'NONE', *, *, #66029, .F. ) ;
#14122 = CARTESIAN_POINT ( 'NONE',  ( -60.72861731925209483, 38.95313093343226996, -19.34325272470447388 ) ) ;
#14123 = CARTESIAN_POINT ( 'NONE',  ( 71.04344271742604633, -59.99999999997053379, 166.1842289479795056 ) ) ;
#14124 = ORIENTED_EDGE ( 'NONE', *, *, #41092, .T. ) ;
#14125 = CARTESIAN_POINT ( 'NONE',  ( 2.000806171155364410, -32.51041572883302422, 29.30576361108121120 ) ) ;
#14126 = CARTESIAN_POINT ( 'NONE',  ( -7.188101187500000044, -18.78125000204838457, -8.802885111219163269E-16 ) ) ;
#14127 = CARTESIAN_POINT ( 'NONE',  ( -32.39813942120886026, 439.6661968104009475, 24.00603005215511843 ) ) ;
#14128 = EDGE_LOOP ( 'NONE', ( #19079, #10666, #75311, #94340 ) ) ;
#14129 = CARTESIAN_POINT ( 'NONE',  ( -10.69637036727096557, 45.32132628290195697, 15.34161786853266740 ) ) ;
#14130 = EDGE_LOOP ( 'NONE', ( #39997, #9004, #83688, #100107, #102610 ) ) ;
#14131 = CARTESIAN_POINT ( 'NONE',  ( 10.69637036727085722, 45.32132628290193566, -15.34161786853273846 ) ) ;
#14132 = ADVANCED_FACE ( 'NONE', ( #106393 ), #68147, .T. ) ;
#14133 = CARTESIAN_POINT ( 'NONE',  ( -2.977408999572654480, -29.00000000204838813, 7.188101187499999156 ) ) ;
#14134 = CARTESIAN_POINT ( 'NONE',  ( -111.0127739589412101, -60.00000000000000000, 187.2454623874871800 ) ) ;
#14135 = DIRECTION ( 'NONE',  ( -1.000000000000000000, -1.224606353822377258E-16, -0.000000000000000000 ) ) ;
#14136 = CARTESIAN_POINT ( 'NONE',  ( 2.977408999572651815, -24.31250000204838813, 7.188101187500000933 ) ) ;
#14137 = CARTESIAN_POINT ( 'NONE',  ( 61.85555555555556140, 6.915964383211875250E-15, 0.000000000000000000 ) ) ;
#14138 = DIRECTION ( 'NONE',  ( -1.000000000000000000, 0.000000000000000000, 0.000000000000000000 ) ) ;
#14139 = FILL_AREA_STYLE_COLOUR ( '', #8139 ) ;
#14140 = CARTESIAN_POINT ( 'NONE',  ( 9.999999999999994671, 48.00000000000000000, -86.30899693747679180 ) ) ;
#14141 = CARTESIAN_POINT ( 'NONE',  ( 33.00000000000000000, 439.7597899781497972, 24.16317522621304192 ) ) ;
#14142 = CARTESIAN_POINT ( 'NONE',  ( -43.09506620288802026, 346.7888432250930464, 10.17652556260325447 ) ) ;
#14143 = CARTESIAN_POINT ( 'NONE',  ( 105.1762604897960642, -60.00000000000003553, 187.0183921652874233 ) ) ;
#14144 = CARTESIAN_POINT ( 'NONE',  ( -36.03617376588638166, -42.97141350977175733, 36.59660582833075182 ) ) ;
#14145 = VERTEX_POINT ( 'NONE', #1180 ) ;
#14146 = CARTESIAN_POINT ( 'NONE',  ( -35.42320619547098914, 462.9369672597862859, 4.219439332230974671 ) ) ;
#14147 = CARTESIAN_POINT ( 'NONE',  ( 32.78518692970002490, -32.55594928816752542, 32.94813001952291387 ) ) ;
#14148 = CARTESIAN_POINT ( 'NONE',  ( 16.57301948837259786, 0.000000000000000000, 4.453875240779975542 ) ) ;
#14149 = ORIENTED_EDGE ( 'NONE', *, *, #59589, .T. ) ;
#14150 = PLANE ( 'NONE',  #66776 ) ;
#14151 = CARTESIAN_POINT ( 'NONE',  ( -73.95166045995811999, -38.32671827097075834, 159.9448648323593432 ) ) ;
#14152 = VERTEX_POINT ( 'NONE', #9292 ) ;
#14154 = CARTESIAN_POINT ( 'NONE',  ( -31.14694070047868735, 432.3293837220155069, 24.29762062537629319 ) ) ;
#14153 = CARTESIAN_POINT ( 'NONE',  ( 9.364662338062446523, -5.000000000000000000, -18.68129556872268893 ) ) ;
#14155 = CARTESIAN_POINT ( 'NONE',  ( 16.18722300313225304, 37.20509570188509230, 21.93860808728192779 ) ) ;
#14156 = CARTESIAN_POINT ( 'NONE',  ( -34.86892522199585898, 473.1724139605213395, 16.84268715836331864 ) ) ;
#14157 = CARTESIAN_POINT ( 'NONE',  ( 0.1684601300089527409, 44.08548369317414029, -16.25000000000000000 ) ) ;
#14158 = CARTESIAN_POINT ( 'NONE',  ( 2.500000000000041300, -26.27793508735800643, 28.26590473652897018 ) ) ;
#14159 = CARTESIAN_POINT ( 'NONE',  ( -48.26750065955930324, 16.22349350713446725, -14.37287707152977667 ) ) ;
#14160 = CARTESIAN_POINT ( 'NONE',  ( -4.717378471607711177, -47.48249719118609846, 42.90183931269586992 ) ) ;
#14161 = CARTESIAN_POINT ( 'NONE',  ( 97.17610485295698197, -60.00000000000001421, 63.76203667182203816 ) ) ;
#14163 = CARTESIAN_POINT ( 'NONE',  ( -44.11327730584680751, 485.7407519190547305, 4.043905406375500000 ) ) ;
#14162 = CIRCLE ( 'NONE', #48652, 1.000000000000000888 ) ;
#14164 = AXIS2_PLACEMENT_3D ( 'NONE', #26075, #50808, #32551 ) ;
#14165 = DIRECTION ( 'NONE',  ( 0.000000000000000000, 0.000000000000000000, 1.000000000000000000 ) ) ;
#14166 = CARTESIAN_POINT ( 'NONE',  ( -33.94429683745519810, 489.7044232354981546, 10.92862313941522601 ) ) ;
#14167 = ORIENTED_EDGE ( 'NONE', *, *, #53785, .T. ) ;
#14168 = EDGE_CURVE ( 'NONE', #69611, #69218, #21682, .T. ) ;
#14169 = CARTESIAN_POINT ( 'NONE',  ( -84.65603397918647488, -29.99999999999999289, 167.0549101427932044 ) ) ;
#14170 = EDGE_LOOP ( 'NONE', ( #319, #104568, #49693, #45411 ) ) ;
#14171 = CARTESIAN_POINT ( 'NONE',  ( 1.401122807519727897E-15, -4.999999999999988454, -95.00000000000000000 ) ) ;
#14172 = CARTESIAN_POINT ( 'NONE',  ( -15.43758579534935294, 2.782614627094442739, 1.951547078892869491 ) ) ;
#14173 = PRESENTATION_STYLE_ASSIGNMENT (( #47606 ) ) ;
#14174 = CARTESIAN_POINT ( 'NONE',  ( 32.16765183830260355, 415.4432000669583545, 25.54511159463929815 ) ) ;
#14175 = CARTESIAN_POINT ( 'NONE',  ( 2.977408999572650927, -29.75000000204838813, -7.188101187500001821 ) ) ;
#14177 = EDGE_CURVE ( 'NONE', #71900, #23399, #30837, .T. ) ;
#14176 = CARTESIAN_POINT ( 'NONE',  ( -43.97568020413746126, 485.1298675218507128, -0.2854751263280810858 ) ) ;
#14178 = DIRECTION ( 'NONE',  ( -0.5735764363510512664, 0.8191520442889881348, 1.003171929053520309E-16 ) ) ;
#14179 = CARTESIAN_POINT ( 'NONE',  ( 14.34999999999999787, 3.309500000000003439, 4.052968581778167743E-16 ) ) ;
#14180 = ORIENTED_EDGE ( 'NONE', *, *, #57664, .F. ) ;
#14181 = B_SPLINE_CURVE_WITH_KNOTS ( 'NONE', 3,
 ( #58023, #66662, #91995, #34333 ),
 .UNSPECIFIED., .F., .F.,
 ( 4, 4 ),
 ( 0.000000000000000000, 0.0002767692171813939143 ),
 .UNSPECIFIED. ) ;
#14182 =( REPRESENTATION_RELATIONSHIP ('NONE','NONE', #69581, #84690 ) REPRESENTATION_RELATIONSHIP_WITH_TRANSFORMATION ( #17960 )SHAPE_REPRESENTATION_RELATIONSHIP( ) );
#14184 = ORIENTED_EDGE ( 'NONE', *, *, #27581, .T. ) ;
#14183 = DIRECTION ( 'NONE',  ( -1.000000000000000000, 0.000000000000000000, 0.000000000000000000 ) ) ;
#14185 = CARTESIAN_POINT ( 'NONE',  ( 80.68051088453421471, -36.02887340626132584, 146.2889946952470837 ) ) ;
#14186 = CARTESIAN_POINT ( 'NONE',  ( 15.26104615578792689, 3.717029890768877021, -4.293899008410894780 ) ) ;
#14187 = ORIENTED_EDGE ( 'NONE', *, *, #86062, .F. ) ;
#14188 = DIRECTION ( 'NONE',  ( 0.000000000000000000, 0.000000000000000000, 1.000000000000000000 ) ) ;
#14189 =( NAMED_UNIT ( * ) PLANE_ANGLE_UNIT ( ) SI_UNIT ( $, .RADIAN. ) );
#14190 = CARTESIAN_POINT ( 'NONE',  ( 5.082755093536324154, -13.34375000204838457, 5.082755093536326818 ) ) ;
#14191 = CARTESIAN_POINT ( 'NONE',  ( 10.92801675053753918, 45.30201443972635644, 15.24347305256516449 ) ) ;
#14192 = CARTESIAN_POINT ( 'NONE',  ( 15.57837800091703606, 302.5584965806573337, 9.874655054472732729 ) ) ;
#14193 = ADVANCED_FACE ( 'NONE', ( #35756 ), #4400, .T. ) ;
#14194 = ORIENTED_EDGE ( 'NONE', *, *, #39322, .F. ) ;
#14195 = COLOUR_RGB ( '', 0.31764706, 0.68627451, 0.89019608) ;
#14196 = PRODUCT_CONTEXT ( 'NONE', #41757, 'mechanical' ) ;
#14197 = SURFACE_SIDE_STYLE ('',( #6646 ) ) ;
#14198 = TOROIDAL_SURFACE ( 'NONE', #102053, 11.00000000000000533, 4.000000000000000000 ) ;
#14199 = CARTESIAN_POINT ( 'NONE',  ( 20.00000000000000711, 5.000000000000000888, 25.00000000000000000 ) ) ;
#14200 = CARTESIAN_POINT ( 'NONE',  ( 7.303354934956394651, 41.37531465094661343, -59.25981217162325265 ) ) ;
#14201 = EDGE_CURVE ( 'NONE', #1618, #14152, #73273, .T. ) ;
#14202 = ORIENTED_EDGE ( 'NONE', *, *, #70487, .T. ) ;
#14203 = CARTESIAN_POINT ( 'NONE',  ( -5.656854249492379694, -9.125000004096769146, -5.656854249492380582 ) ) ;
#14204 = CARTESIAN_POINT ( 'NONE',  ( -26.97617564603512008, -20.23387011012641068, 31.73410695181273766 ) ) ;
#14205 = CARTESIAN_POINT ( 'NONE',  ( 9.999999999999996447, 15.00000000000000000, 3.648665620917586505 ) ) ;
#14206 = AXIS2_PLACEMENT_3D ( 'NONE', #62247, #104254, #45519 ) ;
#14207 = DIRECTION ( 'NONE',  ( 0.000000000000000000, 0.000000000000000000, -1.000000000000000000 ) ) ;
#14208 = B_SPLINE_CURVE_WITH_KNOTS ( 'NONE', 3,
 ( #90525, #8534, #50058, #98606, #15568, #58150, #56543, #40911, #48983, #73800, #33919, #16637, #67330, #41441, #83491, #937, #66790, #1496, #74332, #407, #82968, #48457 ),
 .UNSPECIFIED., .F., .F.,
 ( 4, 2, 2, 2, 2, 2, 2, 2, 2, 2, 4 ),
 ( 0.002937870026032432698, 0.003442696458882132677, 0.003947522891731832656, 0.004199936108156682862, 0.004452349324581533069, 0.004957175757431232614, 0.005462002190280932160, 0.005714415406705783233, 0.005966828623130632572, 0.006471655055980334720, 0.006976481488830035133 ),
 .UNSPECIFIED. ) ;
#14209 = CARTESIAN_POINT ( 'NONE',  ( 7.500000000000004441, 23.94542680926433320, -45.46585527945179450 ) ) ;
#14210 = B_SPLINE_CURVE_WITH_KNOTS ( 'NONE', 3,
 ( #45912, #44861, #28168, #61581, #37320, #29238, #19555, #94472, #77749, #95009, #60520, #36269, #2778, #4380, #12984 ),
 .UNSPECIFIED., .F., .F.,
 ( 4, 2, 1, 2, 2, 1, 1, 2, 4 ),
 ( 0.000000000000000000, 0.4999999999999985567, 0.5624999999999986677, 0.5703124999999995559, 0.5781250000000004441, 0.5937500000000016653, 0.6250000000000032196, 0.7500000000000021094, 1.000000000000000000 ),
 .UNSPECIFIED. ) ;
#14211 = PRODUCT_CONTEXT ( 'NONE', #76878, 'mechanical' ) ;
#14212 = CARTESIAN_POINT ( 'NONE',  ( -9.798380800342663122, 33.46800654315502754, -2.010350564680328134 ) ) ;
#14213 = VERTEX_POINT ( 'NONE', #67027 ) ;
#14214 = CARTESIAN_POINT ( 'NONE',  ( -4.973615039726302811, -46.53039117003746838, 42.61927381063142661 ) ) ;
#14215 = CARTESIAN_POINT ( 'NONE',  ( 104.9555555555555486, 1.023464760207051730E-14, 0.000000000000000000 ) ) ;
#14216 = CARTESIAN_POINT ( 'NONE',  ( -0.5360553870754001249, 13.87989746200968710, -6.984358482147105640 ) ) ;
#14217 = CARTESIAN_POINT ( 'NONE',  ( 59.59397680088719085, -37.32224043100899991, -34.30598283333988974 ) ) ;
#14218 = CARTESIAN_POINT ( 'NONE',  ( -70.01690189409367804, -30.00000000000000000, 95.37921460274809249 ) ) ;
#14219 = EDGE_CURVE ( 'NONE', #35426, #58076, #58395, .T. ) ;
#14220 = DIRECTION ( 'NONE',  ( -1.000000000000000000, -1.224606353822377258E-16, -0.000000000000000000 ) ) ;
#14221 = ORIENTED_EDGE ( 'NONE', *, *, #33519, .F. ) ;
#14222 = CARTESIAN_POINT ( 'NONE',  ( -4.250000000000000000, 5.204748896376250699E-16, -10.00000000000000000 ) ) ;
#14223 = CARTESIAN_POINT ( 'NONE',  ( 86.66021973090251151, -57.58270229864219658, 202.9715953032458913 ) ) ;
#14224 = CARTESIAN_POINT ( 'NONE',  ( 71.33015776002258690, -47.40890048900647713, -23.55054361855370715 ) ) ;
#14225 = DIRECTION ( 'NONE',  ( 1.000000000000000000, 1.224606353822377258E-16, 0.000000000000000000 ) ) ;
#14226 = CARTESIAN_POINT ( 'NONE',  ( -15.64030048137919593, 21.26710225494723616, 5.626279437267545092 ) ) ;
#14227 = CARTESIAN_POINT ( 'NONE',  ( -6.048905432935242743, 53.95601670924679638, 6.275204406079152086 ) ) ;
#14228 = CARTESIAN_POINT ( 'NONE',  ( -72.04210314899036405, -60.00000000000000711, 154.5921861510713882 ) ) ;
#14229 = AXIS2_PLACEMENT_3D ( 'NONE', #39891, #56582, #16668 ) ;
#14230 =( NAMED_UNIT ( * ) PLANE_ANGLE_UNIT ( ) SI_UNIT ( $, .RADIAN. ) );
#14231 = DIRECTION ( 'NONE',  ( -1.000000000000000000, 0.000000000000000000, 0.000000000000000000 ) ) ;
#14232 = CARTESIAN_POINT ( 'NONE',  ( 11.91432047181420195, 49.99999999997997691, 64.17585289263315929 ) ) ;
#14233 = CARTESIAN_POINT ( 'NONE',  ( -85.62538340443454388, -39.27472187846874618, 185.8546422728782943 ) ) ;
#14234 = MECHANICAL_DESIGN_GEOMETRIC_PRESENTATION_REPRESENTATION (  '', ( #69404 ), #22905 ) ;
#14235 = VERTEX_POINT ( 'NONE', #99907 ) ;
#14236 = CARTESIAN_POINT ( 'NONE',  ( 34.53439992527028579, 338.2648225848022889, -0.8894174731781776533 ) ) ;
#14237 = VECTOR ( 'NONE', #71663, 1000.000000000000000 ) ;
#14238 = CARTESIAN_POINT ( 'NONE',  ( 11.72777639070659639, -4.888764692996097061, -76.94183081656832712 ) ) ;
#14239 = ADVANCED_FACE ( 'NONE', ( #75631 ), #35209, .F. ) ;
#14240 = CARTESIAN_POINT ( 'NONE',  ( -13.99999999999998046, 59.99999999999999289, -6.999999999999994671 ) ) ;
#14241 = CARTESIAN_POINT ( 'NONE',  ( -83.32935752366911686, -45.25870497630614153, -13.82694917655253342 ) ) ;
#14242 = CARTESIAN_POINT ( 'NONE',  ( 44.20231929237302637, 435.2535292332384529, 14.52165647984069707 ) ) ;
#14243 = ORIENTED_EDGE ( 'NONE', *, *, #81063, .F. ) ;
#14244 = CIRCLE ( 'NONE', #74542, 8.605212085995399107 ) ;
#14245 = EDGE_CURVE ( 'NONE', #72492, #13768, #30291, .T. ) ;
#14246 = CARTESIAN_POINT ( 'NONE',  ( 19.16286804424708023, 49.99999999999998579, 60.36494180815562771 ) ) ;
#14247 = CARTESIAN_POINT ( 'NONE',  ( 10.29006311568609000, 16.62392477665889956, 10.00613480464933858 ) ) ;
#14248 = ADVANCED_FACE ( 'NONE', ( #18490 ), #51353, .T. ) ;
#14249 = CARTESIAN_POINT ( 'NONE',  ( -22.23822744035697241, -8.673617379884035472E-16, 2.910977163147204116 ) ) ;
#14250 = DIRECTION ( 'NONE',  ( -1.000000000000000000, 0.000000000000000000, 0.000000000000000000 ) ) ;
#14251 = CARTESIAN_POINT ( 'NONE',  ( 87.78053949331578565, -14.21045842199421294, -8.623972743651103556 ) ) ;
#14252 = CARTESIAN_POINT ( 'NONE',  ( -81.82243040554628521, -18.68629064860443378, 135.0887551966091564 ) ) ;
#14253 = ORIENTED_EDGE ( 'NONE', *, *, #105091, .T. ) ;
#14254 = CARTESIAN_POINT ( 'NONE',  ( 31.71028148999514329, -14.21045842199427156, 37.70122135646843731 ) ) ;
#14255 = CARTESIAN_POINT ( 'NONE',  ( 4.590682673078532616, 251.0679175731215764, 3.864023243754595605 ) ) ;
#14256 = CARTESIAN_POINT ( 'NONE',  ( 106.9737785243404176, -57.65419793449832753, 200.1203704123164471 ) ) ;
#14257 = CARTESIAN_POINT ( 'NONE',  ( 46.29078044294533356, 50.00000000000000711, 42.75143139671600068 ) ) ;
#14258 = CARTESIAN_POINT ( 'NONE',  ( 33.46531914086286719, 315.4140312057836582, -6.991426414924862165 ) ) ;
#14259 = DIRECTION ( 'NONE',  ( -0.5735764363510497121, 0.8191520442889892450, 1.003171929053521665E-16 ) ) ;
#14260 = EDGE_LOOP ( 'NONE', ( #66622, #88050, #79197, #97584 ) ) ;
#14261 = CARTESIAN_POINT ( 'NONE',  ( 92.53532739719321398, -5.000000000000000888, 6.123233995736779101E-16 ) ) ;
#14262 = EDGE_CURVE ( 'NONE', #32527, #72439, #75055, .T. ) ;
#14263 = EDGE_CURVE ( 'NONE', #58641, #63624, #101511, .T. ) ;
#14264 = DIRECTION ( 'NONE',  ( -0.000000000000000000, -1.000000000000000000, -0.000000000000000000 ) ) ;
#14266 = CARTESIAN_POINT ( 'NONE',  ( -103.6844849286397334, -52.71031556485471725, 149.2130235818372626 ) ) ;
#14265 = CARTESIAN_POINT ( 'NONE',  ( -17.49999999999999645, 2.500000000000000444, 25.00000000000000000 ) ) ;
#14267 = CARTESIAN_POINT ( 'NONE',  ( -7.188101187500000044, -18.40625000204838457, -8.802885111219163269E-16 ) ) ;
#14268 = DIRECTION ( 'NONE',  ( 0.000000000000000000, -0.6177654251562640919, -0.7863624351922594569 ) ) ;
#14269 =( BOUNDED_SURFACE ( )  B_SPLINE_SURFACE ( 3, 2, ( 
 ( #90296, #16406, #74098 ),
 ( #47701, #97852, #74629 ),
 ( #7242, #49288, #15879 ),
 ( #7773, #23473, #72517 ),
 ( #39649, #80600, #708 ),
 ( #24010, #33680, #57914 ),
 ( #186, #33151, #6723 ),
 ( #81646, #90837, #105424 ) ),
 .UNSPECIFIED., .F., .F., .F. ) 
 B_SPLINE_SURFACE_WITH_KNOTS ( ( 4, 2, 2, 4 ),
 ( 3, 3 ),
 ( 0.03851319102641419245, 0.04314724750133520914, 0.04546427573879571749, 0.04778130397625623277 ),
 ( 0.000000000000000000, 1.000000000000000000 ),
 .UNSPECIFIED. ) 
 GEOMETRIC_REPRESENTATION_ITEM ( )  RATIONAL_B_SPLINE_SURFACE ( (
 ( 1.000000000000000000, 0.8047781573724569482, 1.000000000000000000),
 ( 1.000000000000000000, 0.8123768202407029015, 1.000000000000000000),
 ( 1.000000000000000000, 0.8190667609308867059, 1.000000000000000000),
 ( 1.000000000000000000, 0.8191933927156084261, 1.000000000000000000),
 ( 1.000000000000000000, 0.8176088169850088683, 1.000000000000000000),
 ( 1.000000000000000000, 0.8122958474542694152, 1.000000000000000000),
 ( 1.000000000000000000, 0.8086309703845092622, 1.000000000000000000),
 ( 1.000000000000000000, 0.8047712409910817710, 1.000000000000000000) ) ) 
 REPRESENTATION_ITEM ( '' )  SURFACE ( )  );
#14270 = MECHANICAL_DESIGN_GEOMETRIC_PRESENTATION_REPRESENTATION (  '', ( #88364 ), #7415 ) ;
#14271 = CARTESIAN_POINT ( 'NONE',  ( -1.469576158976823947E-15, -23.37499999999999289, 8.000000000000000000 ) ) ;
#14272 = DIRECTION ( 'NONE',  ( 0.000000000000000000, 0.000000000000000000, -1.000000000000000000 ) ) ;
#14273 = CARTESIAN_POINT ( 'NONE',  ( -17.49999999999997513, 50.00000000000000000, -500000.0000000000582 ) ) ;
#14274 = CARTESIAN_POINT ( 'NONE',  ( 2.499999999999984457, -21.99834388059804269, -30.53959902372158908 ) ) ;
#14275 = DIRECTION ( 'NONE',  ( 1.000000000000000000, 0.000000000000000000, -0.000000000000000000 ) ) ;
#14276 = ORIENTED_EDGE ( 'NONE', *, *, #14263, .F. ) ;
#14277 = CARTESIAN_POINT ( 'NONE',  ( 8.099999999999999645, 0.000000000000000000, 0.000000000000000000 ) ) ;
#14278 = VECTOR ( 'NONE', #20367, 1000.000000000000000 ) ;
#14280 = CARTESIAN_POINT ( 'NONE',  ( 26.75709676130376025, -56.86611455124082681, 35.15177554598145804 ) ) ;
#14279 = CARTESIAN_POINT ( 'NONE',  ( 0.9999999999999940048, -50.00000000000000000, 101.0455488498966758 ) ) ;
#14281 = CARTESIAN_POINT ( 'NONE',  ( 24.23707248033631245, 27.31414015027110764, -32.69896640055604564 ) ) ;
#14282 = ORIENTED_EDGE ( 'NONE', *, *, #5400, .T. ) ;
#14283 = ORIENTED_EDGE ( 'NONE', *, *, #32974, .F. ) ;
#14284 = DIRECTION ( 'NONE',  ( 0.000000000000000000, -1.000000000000000000, 0.000000000000000000 ) ) ;
#14285 = DIRECTION ( 'NONE',  ( 0.000000000000000000, -1.000000000000000000, 0.000000000000000000 ) ) ;
#14286 = CARTESIAN_POINT ( 'NONE',  ( 7.150000000000005684, 41.64999999999999147, -68.91429206202190016 ) ) ;
#14287 = CARTESIAN_POINT ( 'NONE',  ( -8.000000000000000000, 9.797174393178825657E-16, 3.469446951953614189E-15 ) ) ;
#14288 = ORIENTED_EDGE ( 'NONE', *, *, #51124, .F. ) ;
#14289 = CARTESIAN_POINT ( 'NONE',  ( 7.063177057909296508, -60.00000000000000000, -42.52329933592234568 ) ) ;
#14290 = CARTESIAN_POINT ( 'NONE',  ( 22.13522383661086934, 25.65748311883131905, -32.60130617687421761 ) ) ;
#14291 = CARTESIAN_POINT ( 'NONE',  ( -10.08052270137817352, 15.05801543190454694, -10.37155938391993537 ) ) ;
#14292 = CARTESIAN_POINT ( 'NONE',  ( -84.71861686120296042, -56.33758301279731029, -15.23115818338405170 ) ) ;
#14293 = CARTESIAN_POINT ( 'NONE',  ( 6.463647488011506681, -2.646730816809992781, 6.840026438643557860 ) ) ;
#14294 = DIRECTION ( 'NONE',  ( -1.000000000000000000, -1.224606353822377258E-16, -0.000000000000000000 ) ) ;
#14295 = ORIENTED_EDGE ( 'NONE', *, *, #80384, .T. ) ;
#14296 = EDGE_CURVE ( 'NONE', #76811, #54633, #50082, .T. ) ;
#14297 = ORIENTED_EDGE ( 'NONE', *, *, #83066, .T. ) ;
#14298 = ORIENTED_EDGE ( 'NONE', *, *, #718, .F. ) ;
#14299 = CARTESIAN_POINT ( 'NONE',  ( -11.28351131189991641, 9.073918974790284864, -0.5344654698445947538 ) ) ;
#14300 = DIRECTION ( 'NONE',  ( -1.160749806054361473E-16, 0.000000000000000000, -1.000000000000000000 ) ) ;
#14301 = CARTESIAN_POINT ( 'NONE',  ( -38.93743777631283365, 438.0716041117389636, 23.12360524549970719 ) ) ;
#14302 = DIRECTION ( 'NONE',  ( -0.5735764363510459374, -0.8191520442889919096, 0.000000000000000000 ) ) ;
#14303 = CARTESIAN_POINT ( 'NONE',  ( 7.681258945454893382E-14, -1.200000000000000030E-05, 40.75000000000000000 ) ) ;
#14304 = DIRECTION ( 'NONE',  ( -1.000000000000000000, -1.224606353822377258E-16, -0.000000000000000000 ) ) ;
#14305 = CARTESIAN_POINT ( 'NONE',  ( -43.77726364514326463, 485.1149290089483657, -0.7626395446676972334 ) ) ;
#14307 = EDGE_CURVE ( 'NONE', #27343, #55436, #19044, .T. ) ;
#14306 = CARTESIAN_POINT ( 'NONE',  ( 6.463344223170840230, -4.601472318010336515, 5.710032555828793654 ) ) ;
#14308 = ORIENTED_EDGE ( 'NONE', *, *, #41762, .F. ) ;
#14309 = CARTESIAN_POINT ( 'NONE',  ( 1.308996937480704670, 48.00000000000000000, -75.00000000000001421 ) ) ;
#14310 = VERTEX_POINT ( 'NONE', #51882 ) ;
#14311 = CARTESIAN_POINT ( 'NONE',  ( 8.559508646656407649, 53.96349637827586321, 1.531152949374444239 ) ) ;
#14312 = FACE_OUTER_BOUND ( 'NONE', #70797, .T. ) ;
#14313 = CARTESIAN_POINT ( 'NONE',  ( -40.50232667759595984, 485.1162572728906071, -4.198421296053835405 ) ) ;
#14314 = CIRCLE ( 'NONE', #53960, 5.400000000000001243 ) ;
#14315 = CARTESIAN_POINT ( 'NONE',  ( 0.000000000000000000, 6.123233995736767268E-16, -5.000000000000000888 ) ) ;
#14316 = CARTESIAN_POINT ( 'NONE',  ( 63.91119737789728816, -36.00602109814766294, 81.23386328541809576 ) ) ;
#14317 = AXIS2_PLACEMENT_3D ( 'NONE', #58544, #34828, #17560 ) ;
#14318 = ORIENTED_EDGE ( 'NONE', *, *, #31122, .F. ) ;
#14319 = LINE ( 'NONE', #21401, #51333 ) ;
#14320 = PRESENTATION_LAYER_ASSIGNMENT (  '', '', ( #5713 ) ) ;
#14321 = DIRECTION ( 'NONE',  ( 1.734723475976807094E-16, 0.000000000000000000, 1.000000000000000000 ) ) ;
#14322 = DIRECTION ( 'NONE',  ( 0.000000000000000000, 0.000000000000000000, -1.000000000000000000 ) ) ;
#14323 = ADVANCED_FACE ( 'NONE', ( #84799, #10883 ), #43798, .T. ) ;
#14324 = EDGE_LOOP ( 'NONE', ( #76604, #36094, #34161, #82168, #105716 ) ) ;
#14325 = PRESENTATION_STYLE_ASSIGNMENT (( #66075 ) ) ;
#14326 = DIRECTION ( 'NONE',  ( -0.000000000000000000, -0.000000000000000000, -1.000000000000000000 ) ) ;
#14327 = PLANE ( 'NONE',  #54193 ) ;
#14328 = DIRECTION ( 'NONE',  ( 0.5735764363510440500, 0.8191520442889932418, 0.000000000000000000 ) ) ;
#14329 = CARTESIAN_POINT ( 'NONE',  ( -3.313708498984760720, -31.71875000409677625, -8.000000000000000000 ) ) ;
#14330 = CARTESIAN_POINT ( 'NONE',  ( 0.000000000000000000, -4.999999999999998224, 8.000000000000000000 ) ) ;
#14331 = CARTESIAN_POINT ( 'NONE',  ( 86.00510000878230699, -61.04220111983610053, 194.3129011386755849 ) ) ;
#14332 = CARTESIAN_POINT ( 'NONE',  ( 0.000000000000000000, 0.000000000000000000, -9.274828571428571422 ) ) ;
#14333 = CARTESIAN_POINT ( 'NONE',  ( -4.866346026169152239, 7.094448090634657866, 5.000000000000000000 ) ) ;
#14334 = AXIS2_PLACEMENT_3D ( 'NONE', #9550, #85060, #1992 ) ;
#14335 = FACE_OUTER_BOUND ( 'NONE', #82054, .T. ) ;
#14336 = VERTEX_POINT ( 'NONE', #8772 ) ;
#14337 =( LENGTH_UNIT ( ) NAMED_UNIT ( * ) SI_UNIT ( .MILLI., .METRE. ) );
#14338 = FACE_OUTER_BOUND ( 'NONE', #62072, .T. ) ;
#14339 = CARTESIAN_POINT ( 'NONE',  ( 21.61050315576346392, -60.00000000000001421, 40.45514523058442791 ) ) ;
#14340 = CIRCLE ( 'NONE', #74627, 5.000000000000001776 ) ;
#14341 = CARTESIAN_POINT ( 'NONE',  ( -99.15827349551238967, -30.00000000000000000, 146.2805621499050517 ) ) ;
#14342 = B_SPLINE_CURVE_WITH_KNOTS ( 'NONE', 3,
 ( #106704, #90534, #51658, #100215, #58158, #91085, #24762, #57609, #74339, #26381, #34466, #75405, #49533, #17193, #92655, #67337, #1502, #9069, #40918, #67855, #73809, #59244, #92120, #59780 ),
 .UNSPECIFIED., .F., .F.,
 ( 4, 2, 2, 2, 2, 2, 2, 2, 2, 2, 2, 4 ),
 ( 0.01655932398363392857, 0.01740833567538811050, 0.01825734736714228895, 0.01995537075065065280, 0.02080438244240483472, 0.02165339413415901665, 0.02335141751766738050, 0.02420042920942156242, 0.02504944090117574435, 0.02674746428468411513, 0.02844548766819248245, 0.03014351105170085324 ),
 .UNSPECIFIED. ) ;
#14343 = COLOUR_RGB ( '', 0.31764706, 0.68627451, 0.89019608) ;
#14344 = AXIS2_PLACEMENT_3D ( 'NONE', #8489, #25802, #88889 ) ;
#14345 = DIRECTION ( 'NONE',  ( -0.000000000000000000, 1.000000000000000000, 0.000000000000000000 ) ) ;
#14346 = CARTESIAN_POINT ( 'NONE',  ( 44.35530419813503755, -57.68391187086034932, 63.77888240609519244 ) ) ;
#14348 = CARTESIAN_POINT ( 'NONE',  ( 36.08349330513379982, -4.000000000000000000, 4.898587196589415787E-16 ) ) ;
#14347 = CARTESIAN_POINT ( 'NONE',  ( 9.657433074643469340, 43.43006688034495255, 15.25031001494009608 ) ) ;
#14349 = CARTESIAN_POINT ( 'NONE',  ( -17.53286307268036737, 50.00000000000001421, 63.07570132845683020 ) ) ;
#14350 = CARTESIAN_POINT ( 'NONE',  ( 29.68315524076926337, -1.200000000000000030E-05, -40.85535821593530414 ) ) ;
#14351 = CARTESIAN_POINT ( 'NONE',  ( -46.00000000000000000, 438.0646818829403060, 14.80758164879957661 ) ) ;
#14352 = CARTESIAN_POINT ( 'NONE',  ( -4.157015784815857984, -59.99999999999999289, 39.63100293437526034 ) ) ;
#14353 = SURFACE_STYLE_FILL_AREA ( #104439 ) ;
#14354 = ORIENTED_EDGE ( 'NONE', *, *, #39263, .T. ) ;
#14355 = CARTESIAN_POINT ( 'NONE',  ( 41.90764844430457003, 435.8631799414824854, 20.33131504462095762 ) ) ;
#14356 = CARTESIAN_POINT ( 'NONE',  ( -13.76569456190042118, -60.36563448930260734, 34.04465315501506240 ) ) ;
#14358 = CARTESIAN_POINT ( 'NONE',  ( 6.125000000000000000, -60.71953810597977252, 14.41094225130410855 ) ) ;
#14357 = CARTESIAN_POINT ( 'NONE',  ( -86.44151251292561255, -59.99999999999997868, 22.52580379535574906 ) ) ;
#14359 = EDGE_CURVE ( 'NONE', #71900, #105451, #92491, .T. ) ;
#14360 = VERTEX_POINT ( 'NONE', #29780 ) ;
#14361 = CARTESIAN_POINT ( 'NONE',  ( -11.46409645960823021, 12.99999999999756994, 10.00000000000000178 ) ) ;
#14362 = EDGE_CURVE ( 'NONE', #98844, #29601, #104318, .T. ) ;
#14363 = CARTESIAN_POINT ( 'NONE',  ( 15.85122647056153333, 4.114663126756317624, -4.288211754877312210 ) ) ;
#14364 = CARTESIAN_POINT ( 'NONE',  ( 0.000000000000000000, -80.00000000000000000, 37.00000000000000000 ) ) ;
#14365 = CARTESIAN_POINT ( 'NONE',  ( 11.89131030317610183, 1.482358050883964840E-15, 0.000000000000000000 ) ) ;
#14366 = EDGE_CURVE ( 'NONE', #89992, #15547, #20549, .T. ) ;
#14367 = CARTESIAN_POINT ( 'NONE',  ( 15.35975064870966911, 2.980508189489460946, -2.732879807888741741 ) ) ;
#14368 = CARTESIAN_POINT ( 'NONE',  ( 61.50711823914146947, -59.99999999999999289, 105.5777055690388977 ) ) ;
#14369 = CARTESIAN_POINT ( 'NONE',  ( -0.6456277288726508523, 53.45124240752763001, -10.08335398010373574 ) ) ;
#14370 = ORIENTED_EDGE ( 'NONE', *, *, #66560, .T. ) ;
#14371 = CARTESIAN_POINT ( 'NONE',  ( 0.9654893961777153422, -30.00000000000000355, 7.122964895856731538 ) ) ;
#14372 = FACE_OUTER_BOUND ( 'NONE', #78226, .T. ) ;
#14373 = AXIS2_PLACEMENT_3D ( 'NONE', #69185, #9847, #51373 ) ;
#14375 = CARTESIAN_POINT ( 'NONE',  ( 18.58349330513380693, 4.000000000000003553, 0.000000000000000000 ) ) ;
#14374 = CARTESIAN_POINT ( 'NONE',  ( 4.090242245409069888, -14.21045842199428932, 34.36068907045891763 ) ) ;
#14376 = CARTESIAN_POINT ( 'NONE',  ( -4.464768147782833374, -1.996984918325826586, 102.6740199126133888 ) ) ;
#14377 = EDGE_LOOP ( 'NONE', ( #5710, #28242, #95556, #102634, #101034, #93924 ) ) ;
#14378 = CIRCLE ( 'NONE', #100556, 4.000000000000000888 ) ;
#14379 = EDGE_CURVE ( 'NONE', #11843, #1378, #6149, .T. ) ;
#14380 = ORIENTED_EDGE ( 'NONE', *, *, #28397, .T. ) ;
#14381 = CARTESIAN_POINT ( 'NONE',  ( -29.19004656361920880, 323.8257188522660499, 14.61744461631383807 ) ) ;
#14382 = PRESENTATION_LAYER_ASSIGNMENT (  '', '', ( #69550 ) ) ;
#14383 = EDGE_LOOP ( 'NONE', ( #93587, #102914, #47852, #29680 ) ) ;
#14384 = CARTESIAN_POINT ( 'NONE',  ( 21.26797753924777012, 304.0416359807921935, 9.977564030807537065 ) ) ;
#14385 = DIRECTION ( 'NONE',  ( 0.000000000000000000, 1.000000000000000000, 0.000000000000000000 ) ) ;
#14386 = DIRECTION ( 'NONE',  ( 1.000000000000000000, 0.000000000000000000, 0.000000000000000000 ) ) ;
#14387 = EDGE_LOOP ( 'NONE', ( #23283, #48214, #99153, #86269 ) ) ;
#14388 = CARTESIAN_POINT ( 'NONE',  ( -105.4638592052966146, -59.99999999998518518, 201.8892716500855045 ) ) ;
#14389 = CARTESIAN_POINT ( 'NONE',  ( 46.00000000002251710, 485.7203612215654971, -0.7239266944879970689 ) ) ;
#14390 = CARTESIAN_POINT ( 'NONE',  ( 79.59154323555446808, -60.00000000000002132, 195.4646099998837769 ) ) ;
#14391 = CARTESIAN_POINT ( 'NONE',  ( 1.012061803676453042, 25.89207449483374290, -38.74815287735676606 ) ) ;
#14393 = CARTESIAN_POINT ( 'NONE',  ( 12.22020185172853601, -25.54866882569812603, 28.19719061603959176 ) ) ;
#14392 = CARTESIAN_POINT ( 'NONE',  ( -106.1779193982466580, -14.21045842199435860, 156.9944278011976451 ) ) ;
#14394 = CARTESIAN_POINT ( 'NONE',  ( 83.69899461553025333, -37.99999999999997158, 34.12667946149305465 ) ) ;
#14395 = CARTESIAN_POINT ( 'NONE',  ( -7.799243123709609371, 52.08920511281555576, 1.774792398066115107 ) ) ;
#14396 = CARTESIAN_POINT ( 'NONE',  ( -45.44394288432073381, -32.61731379389950547, 42.31964681332677003 ) ) ;
#14397 = CARTESIAN_POINT ( 'NONE',  ( 5.823303048885946964, -64.88595876702598275, 14.26806532518525472 ) ) ;
#14398 = ORIENTED_EDGE ( 'NONE', *, *, #84003, .F. ) ;
#14399 = CARTESIAN_POINT ( 'NONE',  ( 19.83349330513380693, 1.593028355512270962E-15, 0.000000000000000000 ) ) ;
#14400 = DIRECTION ( 'NONE',  ( 0.000000000000000000, -0.8660254037844381525, -0.5000000000000008882 ) ) ;
#14401 =( LENGTH_UNIT ( ) NAMED_UNIT ( * ) SI_UNIT ( .MILLI., .METRE. ) );
#14402 = FACE_OUTER_BOUND ( 'NONE', #64714, .T. ) ;
#14403 = DIRECTION ( 'NONE',  ( -1.000000000000000000, -0.000000000000000000, -0.000000000000000000 ) ) ;
#14404 = ORIENTED_EDGE ( 'NONE', *, *, #74546, .F. ) ;
#14405 = CARTESIAN_POINT ( 'NONE',  ( -8.654235699476732435, -14.00093397087661629, 15.99236324148348487 ) ) ;
#14406 = VERTEX_POINT ( 'NONE', #36816 ) ;
#14407 = B_SPLINE_CURVE_WITH_KNOTS ( 'NONE', 3,
 ( #53699, #62344, #21368, #77451 ),
 .UNSPECIFIED., .F., .F.,
 ( 4, 4 ),
 ( 0.3748654421220272703, 0.3763434592322586481 ),
 .UNSPECIFIED. ) ;
#14408 = CARTESIAN_POINT ( 'NONE',  ( 109.3806035902058795, -29.99999999998653166, 179.6279394377761776 ) ) ;
#14409 = CARTESIAN_POINT ( 'NONE',  ( 83.86866073052654258, 5.000000000000021316, 0.000000000000000000 ) ) ;
#14410 = STYLED_ITEM ( 'NONE', ( #46970 ), #17821 ) ;
#14411 = CARTESIAN_POINT ( 'NONE',  ( 6.700948648136186847, 41.88761797260490738, -59.59787299616537837 ) ) ;
#14412 = CARTESIAN_POINT ( 'NONE',  ( -24.33159596665262470, 34.19642918197134662, -12.16579798332630880 ) ) ;
#14413 = CARTESIAN_POINT ( 'NONE',  ( 89.66112378212690714, -30.00000000000000355, 86.53036795368753076 ) ) ;
#14414 = AXIS2_PLACEMENT_3D ( 'NONE', #47352, #13381, #29113 ) ;
#14415 = CARTESIAN_POINT ( 'NONE',  ( -27.99999999999999645, 0.000000000000000000, 0.000000000000000000 ) ) ;
#14416 = ORIENTED_EDGE ( 'NONE', *, *, #6781, .T. ) ;
#14417 = EDGE_CURVE ( 'NONE', #85237, #49798, #100326, .T. ) ;
#14418 = CIRCLE ( 'NONE', #66096, 4.000000000000001776 ) ;
#14419 = VERTEX_POINT ( 'NONE', #57858 ) ;
#14420 = ORIENTED_EDGE ( 'NONE', *, *, #13109, .F. ) ;
#14422 = DIRECTION ( 'NONE',  ( -1.000000000000000000, -1.224606353822377258E-16, -0.000000000000000000 ) ) ;
#14421 = STYLED_ITEM ( 'NONE', ( #9282 ), #95420 ) ;
#14423 = CARTESIAN_POINT ( 'NONE',  ( -10.00000000000000355, 0.000000000000000000, -10.00000000000000000 ) ) ;
#14424 = CARTESIAN_POINT ( 'NONE',  ( 17.24303157407923237, 294.5700599009814482, 9.877113118490870036 ) ) ;
#14425 = EDGE_CURVE ( 'NONE', #13798, #19325, #100854, .T. ) ;
#14426 = ADVANCED_FACE ( 'NONE', ( #98848 ), #88862, .T. ) ;
#14427 = EDGE_LOOP ( 'NONE', ( #98575, #40594, #41584, #99596, #40924 ) ) ;
#14428 = CARTESIAN_POINT ( 'NONE',  ( -16.01428880459204862, 3.811183212007244414, 1.301242280795995354 ) ) ;
#14429 = ORIENTED_EDGE ( 'NONE', *, *, #43854, .T. ) ;
#14430 = DIRECTION ( 'NONE',  ( 0.000000000000000000, 1.000000000000000000, 0.000000000000000000 ) ) ;
#14431 = CARTESIAN_POINT ( 'NONE',  ( 88.61011283327033539, -38.54255348427882666, 200.1637712349269975 ) ) ;
#14432 = DIRECTION ( 'NONE',  ( 0.000000000000000000, 1.000000000000000000, 0.000000000000000000 ) ) ;
#14433 = CARTESIAN_POINT ( 'NONE',  ( 85.70353180741470567, -52.75305998193952917, -8.674284238902059130 ) ) ;
#14434 = CARTESIAN_POINT ( 'NONE',  ( 82.85623877874613186, -38.00000000000004974, 166.0433923026292007 ) ) ;
#14435 = CARTESIAN_POINT ( 'NONE',  ( 39.62846356518264201, 316.6287052912528566, 7.214087219703729126 ) ) ;
#14436 = CARTESIAN_POINT ( 'NONE',  ( 43.99980723760478440, 434.6400489724846921, 17.20555692211239673 ) ) ;
#14437 = CARTESIAN_POINT ( 'NONE',  ( 0.000000000000000000, 0.000000000000000000, -5.710657142857142432 ) ) ;
#14438 = CARTESIAN_POINT ( 'NONE',  ( 4.561387878963821585, 143.2234794286142403, 5.000000000000000000 ) ) ;
#14439 = ORIENTED_EDGE ( 'NONE', *, *, #42504, .T. ) ;
#14440 = DIRECTION ( 'NONE',  ( 0.000000000000000000, 1.000000000000000000, 0.000000000000000000 ) ) ;
#14441 = EDGE_CURVE ( 'NONE', #90738, #4517, #99146, .T. ) ;
#14442 = CARTESIAN_POINT ( 'NONE',  ( -34.64744136446724099, 462.0025097428029426, 4.201592667583327945 ) ) ;
#14443 = COLOUR_RGB ( '', 0.72549020, 0.75294118, 0.79215686) ;
#14444 = CARTESIAN_POINT ( 'NONE',  ( -2.854624676502999669, 68.28528602110660017, 4.999999999999998224 ) ) ;
#14445 = VERTEX_POINT ( 'NONE', #74579 ) ;
#14446 = CARTESIAN_POINT ( 'NONE',  ( -43.38684324080074362, 436.1115529209241686, 18.84450155852746889 ) ) ;
#14447 = CARTESIAN_POINT ( 'NONE',  ( -33.70188103806000157, 302.7179012586964859, 11.74889379020421920 ) ) ;
#14448 = DIRECTION ( 'NONE',  ( 0.000000000000000000, 0.000000000000000000, 1.000000000000000000 ) ) ;
#14449 = DIRECTION ( 'NONE',  ( -1.000000000000000000, 0.000000000000000000, 0.000000000000000000 ) ) ;
#14450 = CARTESIAN_POINT ( 'NONE',  ( -5.656854249492379694, -17.93749999999999645, -5.656854249492380582 ) ) ;
#14451 = CARTESIAN_POINT ( 'NONE',  ( 44.63371705108917809, -29.90653276422889917, 54.31444785595910929 ) ) ;
#14452 = EDGE_CURVE ( 'NONE', #17876, #23615, #23439, .T. ) ;
#14453 = MECHANICAL_DESIGN_GEOMETRIC_PRESENTATION_REPRESENTATION (  '', ( #52346 ), #47188 ) ;
#14454 = ORIENTED_EDGE ( 'NONE', *, *, #100634, .F. ) ;
#14455 = CARTESIAN_POINT ( 'NONE',  ( 83.28920025294588925, -60.95966722623995793, 191.1640505686548295 ) ) ;
#14456 = EDGE_CURVE ( 'NONE', #33852, #99968, #97462, .T. ) ;
#14457 = CARTESIAN_POINT ( 'NONE',  ( -48.91361122442935283, 8.059984797525034494, 16.48958644079295155 ) ) ;
#14458 = ORIENTED_EDGE ( 'NONE', *, *, #73235, .F. ) ;
#14459 = CARTESIAN_POINT ( 'NONE',  ( 95.56805927552339597, -57.67170252440953959, 37.76800136122525231 ) ) ;
#14460 = CARTESIAN_POINT ( 'NONE',  ( 35.47684105139852306, 436.4843629120485389, 5.043999258398844887 ) ) ;
#14461 = CARTESIAN_POINT ( 'NONE',  ( 11.39884040753850947, -4.333298119783793645, 13.82668420656116837 ) ) ;
#14462 = CARTESIAN_POINT ( 'NONE',  ( 29.14573983020287784, 13.65694994997195444, 39.72476874530803315 ) ) ;
#14463 = CARTESIAN_POINT ( 'NONE',  ( -63.29526267904824266, -38.00000000000001421, 80.45729844939860698 ) ) ;
#14464 = CARTESIAN_POINT ( 'NONE',  ( 2.617993873628172263, -5.000000000000000000, -10.00000000000000000 ) ) ;
#14465 = CARTESIAN_POINT ( 'NONE',  ( 14.34999999999999787, 1.533819458162526451E-15, 0.000000000000000000 ) ) ;
#14467 = CARTESIAN_POINT ( 'NONE',  ( -10.93976548513864167, 11.14550375312795438, 9.847392385548467075 ) ) ;
#14466 = CARTESIAN_POINT ( 'NONE',  ( 3.750000000000004885, -6.495190528383287365, 1.734723475976807094E-15 ) ) ;
#14468 = ADVANCED_FACE ( 'NONE', ( #656 ), #64675, .F. ) ;
#14469 = DIRECTION ( 'NONE',  ( 0.000000000000000000, -0.000000000000000000, 1.000000000000000000 ) ) ;
#14470 = FACE_OUTER_BOUND ( 'NONE', #38626, .T. ) ;
#14471 = CARTESIAN_POINT ( 'NONE',  ( -32.80207110003820503, 464.7310103173836069, 6.970203097363641298 ) ) ;
#14472 = CARTESIAN_POINT ( 'NONE',  ( 28.99999999999999645, 0.000000000000000000, 0.000000000000000000 ) ) ;
#14473 = CYLINDRICAL_SURFACE ( 'NONE', #85554, 15.00000000000000000 ) ;
#14474 = CARTESIAN_POINT ( 'NONE',  ( 43.50721599125539285, 484.7945671711811428, 4.126833950650420135 ) ) ;
#14475 = AXIS2_PLACEMENT_3D ( 'NONE', #101898, #43143, #44209 ) ;
#14476 = EDGE_LOOP ( 'NONE', ( #21508, #35453, #44270, #38876, #26831 ) ) ;
#14477 = LINE ( 'NONE', #15021, #70312 ) ;
#14478 = FILL_AREA_STYLE ('',( #15559 ) ) ;
#14479 = CARTESIAN_POINT ( 'NONE',  ( -37.04855517154567224, -23.96599618594476766, -30.89117867367345127 ) ) ;
#14481 = CARTESIAN_POINT ( 'NONE',  ( -62.88590845438242383, -47.40890540049978341, -26.65507182869829350 ) ) ;
#14480 = CARTESIAN_POINT ( 'NONE',  ( 1.288479777019285939E-15, 37.86482112153537116, 10.52123582012687919 ) ) ;
#14482 = EDGE_CURVE ( 'NONE', #81100, #26896, #83511, .T. ) ;
#14483 = VERTEX_POINT ( 'NONE', #32032 ) ;
#14484 = CARTESIAN_POINT ( 'NONE',  ( 6.658902113223476249, 5.287118297638405018, -7.776713651266118354 ) ) ;
#14485 = ORIENTED_EDGE ( 'NONE', *, *, #17646, .T. ) ;
#14486 = EDGE_CURVE ( 'NONE', #96401, #94380, #50880, .T. ) ;
#14487 = EDGE_CURVE ( 'NONE', #41603, #29093, #104400, .T. ) ;
#14488 = DIRECTION ( 'NONE',  ( 0.5735764363510468256, 0.8191520442889913545, 0.000000000000000000 ) ) ;
#14489 = DIRECTION ( 'NONE',  ( -0.8191520442889974607, 0.000000000000000000, -0.5735764363510379438 ) ) ;
#14490 = CARTESIAN_POINT ( 'NONE',  ( -92.73154865952776049, -60.00000000000000000, -5.894050899535240085 ) ) ;
#14491 = ORIENTED_EDGE ( 'NONE', *, *, #31727, .T. ) ;
#14492 = CARTESIAN_POINT ( 'NONE',  ( 6.298933871243065141, 41.33266196706044582, -58.30935828777717234 ) ) ;
#14493 = CARTESIAN_POINT ( 'NONE',  ( 98.75509859307410920, -60.33206540521932482, 196.3354318149040409 ) ) ;
#14495 = FACE_OUTER_BOUND ( 'NONE', #81348, .T. ) ;
#14494 = SURFACE_STYLE_FILL_AREA ( #23703 ) ;
#14496 = ADVANCED_FACE ( 'NONE', ( #106411 ), #66521, .T. ) ;
#14497 = CARTESIAN_POINT ( 'NONE',  ( -79.80068360959039353, -60.35772941472219344, 173.0473014186353851 ) ) ;
#14498 = ORIENTED_EDGE ( 'NONE', *, *, #68757, .F. ) ;
#14499 = ADVANCED_FACE ( 'NONE', ( #39594 ), #32572, .T. ) ;
#14500 = ADVANCED_FACE ( 'NONE', ( #24491 ), #82961, .T. ) ;
#14501 = VERTEX_POINT ( 'NONE', #56665 ) ;
#14502 = EDGE_CURVE ( 'NONE', #214, #82136, #21754, .T. ) ;
#14503 = ORIENTED_EDGE ( 'NONE', *, *, #28365, .F. ) ;
#14504 = CARTESIAN_POINT ( 'NONE',  ( 31.36907200230133697, 433.8648511944086295, 23.03418318384254349 ) ) ;
#14505 = CARTESIAN_POINT ( 'NONE',  ( -5.000000000000000000, -14.24437098773013055, 11.98245615812826870 ) ) ;
#14506 = CARTESIAN_POINT ( 'NONE',  ( 53.29999999999999716, 3.309500000000014541, 4.052968581778174646E-16 ) ) ;
#14507 = ORIENTED_EDGE ( 'NONE', *, *, #4946, .F. ) ;
#14508 = CIRCLE ( 'NONE', #78287, 4.000000000000000888 ) ;
#14509 = PLANE ( 'NONE',  #3140 ) ;
#14510 = FACE_OUTER_BOUND ( 'NONE', #16731, .T. ) ;
#14511 = CARTESIAN_POINT ( 'NONE',  ( -89.37884834614470719, -57.60609784898206698, 203.8391154356046115 ) ) ;
#14512 = CARTESIAN_POINT ( 'NONE',  ( 0.06730325657375016424, -1.557442666578367829, 8.000000000000000000 ) ) ;
#14513 = DIRECTION ( 'NONE',  ( -1.000000000000000000, -1.224606353822377258E-16, -0.000000000000000000 ) ) ;
#14514 = DIRECTION ( 'NONE',  ( -0.8308658609248562588, -0.5564727496918402405, 0.000000000000000000 ) ) ;
#14515 = CARTESIAN_POINT ( 'NONE',  ( 2.455962139888945739, 15.75268258782372754, -9.700350089084166072 ) ) ;
#14516 = CARTESIAN_POINT ( 'NONE',  ( 86.49463782384169974, -14.21045842199436215, 11.84774393978288742 ) ) ;
#14517 = CARTESIAN_POINT ( 'NONE',  ( -66.64776185298879341, -30.00000000000000711, 114.0837597745640721 ) ) ;
#14518 = B_SPLINE_CURVE_WITH_KNOTS ( 'NONE', 3,
 ( #18010, #50876, #8302, #81639, #57906, #1793, #58459, #74093, #34214, #67086, #50344, #178, #66011, #67622, #98889, #59537, #42259, #48745, #75150, #83779 ),
 .UNSPECIFIED., .F., .F.,
 ( 4, 2, 2, 2, 2, 2, 2, 2, 2, 4 ),
 ( 0.006400020579250047421, 0.007199736318437515055, 0.007999452057624981821, 0.008799167796812449455, 0.009598883535999917088, 0.01039859927518738472, 0.01119831501437485236, 0.01159817288396858617, 0.01199803075356231825, 0.01279774649274978589 ),
 .UNSPECIFIED. ) ;
#14519 = CARTESIAN_POINT ( 'NONE',  ( -53.38980839664982625, -25.63582924091855375, 51.76195856533456663 ) ) ;
#14520 = VERTEX_POINT ( 'NONE', #32963 ) ;
#14521 = CARTESIAN_POINT ( 'NONE',  ( 1.313512443508423777, 21.63996318350142545, -6.880116371441049594 ) ) ;
#14522 = CIRCLE ( 'NONE', #81728, 4.000000000000000888 ) ;
#14523 = ORIENTED_EDGE ( 'NONE', *, *, #97591, .F. ) ;
#14524 = AXIS2_PLACEMENT_3D ( 'NONE', #30778, #54998, #5924 ) ;
#14525 = CARTESIAN_POINT ( 'NONE',  ( -100.1530219422562453, -45.25741937776533774, 192.4508485111738310 ) ) ;
#14526 = AXIS2_PLACEMENT_3D ( 'NONE', #100331, #34045, #35107 ) ;
#14527 = DIRECTION ( 'NONE',  ( -1.000000000000000000, -1.224606353822377258E-16, -0.000000000000000000 ) ) ;
#14528 = ORIENTED_EDGE ( 'NONE', *, *, #86666, .T. ) ;
#14529 = CARTESIAN_POINT ( 'NONE',  ( 19.19786010934679865, 49.77473709286820736, 61.56662838479388000 ) ) ;
#14530 = AXIS2_PLACEMENT_3D ( 'NONE', #54073, #63796, #96682 ) ;
#14531 = CARTESIAN_POINT ( 'NONE',  ( 107.4777185979739045, -38.36096664182583993, 193.9906563548574070 ) ) ;
#14532 = DIRECTION ( 'NONE',  ( 0.000000000000000000, -1.000000000000000000, 0.000000000000000000 ) ) ;
#14533 = DIRECTION ( 'NONE',  ( 0.000000000000000000, -1.000000000000000000, 0.000000000000000000 ) ) ;
#14534 = DIRECTION ( 'NONE',  ( 0.000000000000000000, 1.000000000000000000, 0.000000000000000000 ) ) ;
#14535 = CARTESIAN_POINT ( 'NONE',  ( -41.96737725787951945, 484.5368175928758774, -2.772775517605185147 ) ) ;
#14536 = CARTESIAN_POINT ( 'NONE',  ( 63.94887954703639110, -30.00000000000000711, 77.26283590874240303 ) ) ;
#14537 = CARTESIAN_POINT ( 'NONE',  ( 16.13875682045383542, 303.5610363769735045, -10.06180378987414592 ) ) ;
#14538 = CARTESIAN_POINT ( 'NONE',  ( 0.000000000000000000, 0.000000000000000000, 0.000000000000000000 ) ) ;
#14539 = CARTESIAN_POINT ( 'NONE',  ( -0.1696257032302785628, 34.17492106715072708, 29.74129072143946928 ) ) ;
#14540 = CARTESIAN_POINT ( 'NONE',  ( -35.40902385155463605, 484.3229957183393708, -1.494454771033894902 ) ) ;
#14541 = UNCERTAINTY_MEASURE_WITH_UNIT (LENGTH_MEASURE( 1.000000000000000082E-05 ), #65980, 'distance_accuracy_value', 'NONE');
#14542 = ORIENTED_EDGE ( 'NONE', *, *, #87679, .F. ) ;
#14543 = EDGE_LOOP ( 'NONE', ( #16545, #47221, #38740, #8649 ) ) ;
#14544 = CARTESIAN_POINT ( 'NONE',  ( 49.20350849749573996, -25.67110830728586635, 45.04464490564094348 ) ) ;
#14545 = FACE_OUTER_BOUND ( 'NONE', #62338, .T. ) ;
#14546 = DIRECTION ( 'NONE',  ( 0.000000000000000000, -1.000000000000000000, 0.000000000000000000 ) ) ;
#14547 = ADVANCED_FACE ( 'NONE', ( #8119 ), #100908, .F. ) ;
#14548 = CARTESIAN_POINT ( 'NONE',  ( -108.8331786921338704, -38.35659805241468945, 190.6592588805922901 ) ) ;
#14549 = VERTEX_POINT ( 'NONE', #76572 ) ;
#14550 = CARTESIAN_POINT ( 'NONE',  ( 84.61307093322078288, -38.35852348009560586, -23.18649592206343257 ) ) ;
#14551 = CARTESIAN_POINT ( 'NONE',  ( 13.04586309976887470, 19.29735459000327324, -7.772842735983566342 ) ) ;
#14552 = FACE_OUTER_BOUND ( 'NONE', #76118, .T. ) ;
#14553 = CARTESIAN_POINT ( 'NONE',  ( 32.15047201613552375, 464.7337454272250739, 11.12330847294782821 ) ) ;
#14554 = CARTESIAN_POINT ( 'NONE',  ( 99.13832651037952814, -45.28277757653744118, 125.4540675598559432 ) ) ;
#14555 = SURFACE_STYLE_USAGE ( .BOTH. , #23226 ) ;
#14556 = DIRECTION ( 'NONE',  ( -1.000000000000000000, -0.000000000000000000, -0.000000000000000000 ) ) ;
#14557 = CARTESIAN_POINT ( 'NONE',  ( 33.20892452566059205, 484.6201576160617606, 4.300277591678492328 ) ) ;
#14558 = SURFACE_STYLE_FILL_AREA ( #55546 ) ;
#14559 = CARTESIAN_POINT ( 'NONE',  ( 99.48401045806168952, -60.00000000000000711, 202.0262045926570806 ) ) ;
#14560 =( GEOMETRIC_REPRESENTATION_CONTEXT ( 3 ) GLOBAL_UNCERTAINTY_ASSIGNED_CONTEXT ( ( #42968 ) ) GLOBAL_UNIT_ASSIGNED_CONTEXT ( ( #6246, #65027, #106003 ) ) REPRESENTATION_CONTEXT ( 'NONE', 'WORKASPACE' ) );
#14561 =( BOUNDED_CURVE ( )  B_SPLINE_CURVE ( 2, ( #17934, #51865, #10344, #51334, #58919, #91813, #60526, #44322, #2242 ),
 .UNSPECIFIED., .F., .F. ) 
 B_SPLINE_CURVE_WITH_KNOTS ( ( 3, 2, 2, 2, 3 ),
 ( 0.8382352941176471894, 0.8455882352941177516, 0.8529411764705882026, 0.8602941176470588758, 0.8676470588235293269 ),
 .UNSPECIFIED. ) 
 CURVE ( )  GEOMETRIC_REPRESENTATION_ITEM ( )  RATIONAL_B_SPLINE_CURVE ( ( 0.9999999999999988898, 0.9238795325112878487, 1.000000000000000000, 0.9238795325112867385, 1.000000000000000000, 0.9238795325112867385, 1.000000000000000000, 0.9238795325112878487, 0.9999999999999988898 ) ) 
 REPRESENTATION_ITEM ( '' )  );
#14562 = CONICAL_SURFACE ( 'NONE', #73077, 4.000000000000000000, 0.9599310885968912466 ) ;
#14563 = EDGE_CURVE ( 'NONE', #73065, #58935, #78361, .T. ) ;
#14564 = EDGE_LOOP ( 'NONE', ( #88890, #95619, #23379, #52815, #47729 ) ) ;
#14565 = CARTESIAN_POINT ( 'NONE',  ( 56.24403759451723772, -46.43678935591641022, 65.97268512243753946 ) ) ;
#14566 = CARTESIAN_POINT ( 'NONE',  ( -34.62026995421213371, 301.0276281301425456, -8.612034659465027886 ) ) ;
#14567 = DIRECTION ( 'NONE',  ( 0.000000000000000000, -1.000000000000000000, 0.000000000000000000 ) ) ;
#14568 = AXIS2_PLACEMENT_3D ( 'NONE', #25679, #2409, #11024 ) ;
#14569 = STYLED_ITEM ( 'NONE', ( #53223 ), #17340 ) ;
#14570 = CARTESIAN_POINT ( 'NONE',  ( -7.744329845603316720, 26.53711769846545110, -2.018701143083231120 ) ) ;
#14571 = ORIENTED_EDGE ( 'NONE', *, *, #21150, .F. ) ;
#14573 = CARTESIAN_POINT ( 'NONE',  ( -9.668268460383899310, -50.82497190099731199, 29.56382476086920974 ) ) ;
#14572 = CARTESIAN_POINT ( 'NONE',  ( -98.79614853170117783, -38.47643861779322805, 200.8458920591413914 ) ) ;
#14574 = DIRECTION ( 'NONE',  ( -0.000000000000000000, -1.000000000000000000, -0.000000000000000000 ) ) ;
#14575 = CARTESIAN_POINT ( 'NONE',  ( 31.44899505358197800, 391.8681076219244801, 24.19046092930541292 ) ) ;
#14576 = CARTESIAN_POINT ( 'NONE',  ( -42.41881992943708468, 464.7100687009927924, 16.14946504447264175 ) ) ;
#14577 = CARTESIAN_POINT ( 'NONE',  ( -3.313708498984765161, -30.96874999999999645, 7.999999999999998224 ) ) ;
#14578 = CARTESIAN_POINT ( 'NONE',  ( -6.145467200819251019, -5.000000000000002665, -77.00333157709852117 ) ) ;
#14579 = LINE ( 'NONE', #81970, #51759 ) ;
#14580 = ORIENTED_EDGE ( 'NONE', *, *, #82398, .T. ) ;
#14581 = CARTESIAN_POINT ( 'NONE',  ( 81.85826472627840644, -53.49893263140352673, 180.4516800555814484 ) ) ;
#14582 = EDGE_CURVE ( 'NONE', #95530, #42925, #82552, .T. ) ;
#14583 = FACE_OUTER_BOUND ( 'NONE', #10986, .T. ) ;
#14584 = CARTESIAN_POINT ( 'NONE',  ( 36.49133541866372354, 28.04549298931340928, 12.86447375659304804 ) ) ;
#14585 = ORIENTED_EDGE ( 'NONE', *, *, #32180, .F. ) ;
#14586 = CARTESIAN_POINT ( 'NONE',  ( -36.55196016430014083, 336.7123902869778362, -1.787123880112916341 ) ) ;
#14587 = CARTESIAN_POINT ( 'NONE',  ( 7.084012698783952011, -4.012402067428147312, -17.39015006380907380 ) ) ;
#14588 = CARTESIAN_POINT ( 'NONE',  ( 23.58349330513380337, 1.593028355512270567E-15, 0.000000000000000000 ) ) ;
#14589 = CARTESIAN_POINT ( 'NONE',  ( -10.47796581436091579, 50.00000000000001421, -91.06180813479443259 ) ) ;
#14590 = FACE_OUTER_BOUND ( 'NONE', #51249, .T. ) ;
#14591 = FACE_OUTER_BOUND ( 'NONE', #90066, .T. ) ;
#14592 = PRODUCT ( 'hex nut high strength_din_Hexagon Nut DIN 6915 - M16 - S', 'hex nut high strength_din_Hexagon Nut DIN 6915 - M16 - S', '', ( #29391 ) ) ;
#14593 = ORIENTED_EDGE ( 'NONE', *, *, #58413, .T. ) ;
#14594 = CARTESIAN_POINT ( 'NONE',  ( 6.826575449902166248, 2.663085462279167093, -6.347418139105194257 ) ) ;
#14595 = CARTESIAN_POINT ( 'NONE',  ( -4.970849588242775674, -46.55209929711412542, 102.2755693391596594 ) ) ;
#14597 = CARTESIAN_POINT ( 'NONE',  ( -10.04210299847170518, 14.33706770242568851, -10.47444268205537199 ) ) ;
#14596 = CARTESIAN_POINT ( 'NONE',  ( 7.150000000000005684, 41.64999999999999147, -68.91429206202190016 ) ) ;
#14599 = MECHANICAL_DESIGN_GEOMETRIC_PRESENTATION_REPRESENTATION (  '', ( #790 ), #50788 ) ;
#14598 = PRODUCT_RELATED_PRODUCT_CATEGORY ( 'part', '', ( #11294 ) ) ;
#14600 = CARTESIAN_POINT ( 'NONE',  ( -2.977408999572654480, -18.12500000204838457, 7.188101187499999156 ) ) ;
#14601 = CARTESIAN_POINT ( 'NONE',  ( -28.77636872657267730, 18.82904586931651636, -39.99174360897771408 ) ) ;
#14602 = AXIS2_PLACEMENT_3D ( 'NONE', #6193, #72531, #80086 ) ;
#14603 = SURFACE_STYLE_FILL_AREA ( #22751 ) ;
#14604 = CIRCLE ( 'NONE', #18038, 4.000000000000001776 ) ;
#14605 = AXIS2_PLACEMENT_3D ( 'NONE', #40301, #14949, #88336 ) ;
#14606 = EDGE_LOOP ( 'NONE', ( #18212, #66803, #10687, #87043 ) ) ;
#14607 = PLANE ( 'NONE',  #66487 ) ;
#14608 = CARTESIAN_POINT ( 'NONE',  ( 0.000000000000000000, 0.000000000000000000, -0.7256075382097185722 ) ) ;
#14609 = AXIS2_PLACEMENT_3D ( 'NONE', #79587, #14304, #5696 ) ;
#14610 = DIRECTION ( 'NONE',  ( 0.000000000000000000, 0.000000000000000000, 1.000000000000000000 ) ) ;
#14611 = CARTESIAN_POINT ( 'NONE',  ( -43.00000000000000000, 436.5989882784185170, 19.94133085611150591 ) ) ;
#14612 = CARTESIAN_POINT ( 'NONE',  ( 1.083333333333333259, 6.880090707843052655, -5.848636054922040195 ) ) ;
#14613 = ORIENTED_EDGE ( 'NONE', *, *, #74414, .F. ) ;
#14614 = FACE_OUTER_BOUND ( 'NONE', #2484, .T. ) ;
#14615 = CARTESIAN_POINT ( 'NONE',  ( -1.734723475976807094E-15, 15.58845726811991383, 0.000000000000000000 ) ) ;
#14616 = ORIENTED_EDGE ( 'NONE', *, *, #98751, .F. ) ;
#14617 = EDGE_CURVE ( 'NONE', #15530, #25050, #76044, .T. ) ;
#14618 = CARTESIAN_POINT ( 'NONE',  ( -2.499999999999963141, -18.83381654053417620, 27.02533567785737034 ) ) ;
#14619 = CARTESIAN_POINT ( 'NONE',  ( -2.807206530941650957, -0.4217707022279503781, 102.9378052260346834 ) ) ;
#14620 = DIRECTION ( 'NONE',  ( -1.000000000000000000, -1.224606353822377258E-16, -0.000000000000000000 ) ) ;
#14621 = UNCERTAINTY_MEASURE_WITH_UNIT (LENGTH_MEASURE( 1.000000000000000082E-05 ), #9866, 'distance_accuracy_value', 'NONE');
#14622 = CARTESIAN_POINT ( 'NONE',  ( -106.5148633137519738, -60.00000000000000000, 119.6060780682273474 ) ) ;
#14623 = DIRECTION ( 'NONE',  ( 0.000000000000000000, 0.000000000000000000, -1.000000000000000000 ) ) ;
#14624 = CARTESIAN_POINT ( 'NONE',  ( -13.64050477809429829, 1.160452971590898885, 14.95551770859069585 ) ) ;
#14625 = CARTESIAN_POINT ( 'NONE',  ( -9.999999999999996447, -5.000000000000002665, -86.30899693747676338 ) ) ;
#14626 = CARTESIAN_POINT ( 'NONE',  ( -85.42087258937787908, -25.35191051116863648, 171.5620230697320778 ) ) ;
#14627 = ORIENTED_EDGE ( 'NONE', *, *, #98199, .F. ) ;
#14628 = DIRECTION ( 'NONE',  ( 0.000000000000000000, 0.000000000000000000, 1.000000000000000000 ) ) ;
#14629 = EDGE_CURVE ( 'NONE', #45991, #64739, #106082, .T. ) ;
#14630 = CONICAL_SURFACE ( 'NONE', #62882, 4.172000000000001485, 0.9599310885968750373 ) ;
#14631 = ORIENTED_EDGE ( 'NONE', *, *, #29544, .F. ) ;
#14632 = EDGE_CURVE ( 'NONE', #6036, #23078, #40648, .T. ) ;
#14633 = CARTESIAN_POINT ( 'NONE',  ( 5.477578620271509990, -68.16501439016104769, -2.459398706554655867 ) ) ;
#14634 = ADVANCED_FACE ( 'NONE', ( #13870 ), #106651, .F. ) ;
#14635 = CARTESIAN_POINT ( 'NONE',  ( -85.39439480315969888, -52.70747882121834493, 25.13064204089321052 ) ) ;
#14636 = DIRECTION ( 'NONE',  ( -1.000000000000000000, -1.224606353822377258E-16, -0.000000000000000000 ) ) ;
#14637 = EDGE_CURVE ( 'NONE', #78219, #59152, #27553, .T. ) ;
#14638 = CARTESIAN_POINT ( 'NONE',  ( -16.14595037822608958, 7.274337365584599091, -6.616591826375521457 ) ) ;
#14639 = CARTESIAN_POINT ( 'NONE',  ( 7.869432500667118191, 64.69453614009768216, -2.456524630699382222E-12 ) ) ;
#14640 = FILL_AREA_STYLE_COLOUR ( '', #64822 ) ;
#14641 = CARTESIAN_POINT ( 'NONE',  ( 0.7145311798163219708, 4.618802153517003184, -8.000000000000000000 ) ) ;
#14642 = CARTESIAN_POINT ( 'NONE',  ( 105.0775402602081954, -59.99999999999994316, 202.2121962084956976 ) ) ;
#14643 = CARTESIAN_POINT ( 'NONE',  ( -98.01432676219248208, -59.99999999999999289, 53.56972733528865405 ) ) ;
#14644 = CARTESIAN_POINT ( 'NONE',  ( -61.71058082456869442, -60.34646374257998502, 87.28499776601393023 ) ) ;
#14645 = VERTEX_POINT ( 'NONE', #59894 ) ;
#14646 = CARTESIAN_POINT ( 'NONE',  ( -43.66100747388606607, 39.42406093352394691, 48.52432126285668090 ) ) ;
#14647 = CARTESIAN_POINT ( 'NONE',  ( 93.59144555981008295, -60.00000000002452794, 204.9629604458358187 ) ) ;
#14648 = ORIENTED_EDGE ( 'NONE', *, *, #5591, .T. ) ;
#14649 = CARTESIAN_POINT ( 'NONE',  ( 3.040510621938483649, -42.95355241522654666, 31.04364016054148934 ) ) ;
#14650 = CARTESIAN_POINT ( 'NONE',  ( 4.401442555609581635E-16, -22.15625000204838457, -7.188101187500000044 ) ) ;
#14651 = SURFACE_SIDE_STYLE ('',( #55634 ) ) ;
#14652 = ORIENTED_EDGE ( 'NONE', *, *, #22711, .T. ) ;
#14653 = DIRECTION ( 'NONE',  ( -1.000000000000000000, -1.224606353822377258E-16, -0.000000000000000000 ) ) ;
#14654 = ORIENTED_EDGE ( 'NONE', *, *, #62858, .T. ) ;
#14655 = CARTESIAN_POINT ( 'NONE',  ( -46.00000000000000000, 450.0000000000002274, 13.20242257375370976 ) ) ;
#14656 = CIRCLE ( 'NONE', #856, 4.172000000000001485 ) ;
#14657 = CARTESIAN_POINT ( 'NONE',  ( 7.122964895856751077, -30.00000000000000355, -0.9654893961775683486 ) ) ;
#14658 = CARTESIAN_POINT ( 'NONE',  ( -104.3750103821752191, -60.00000000000000000, 199.7222116143482538 ) ) ;
#14659 = CARTESIAN_POINT ( 'NONE',  ( 9.125156274357966169, -54.52949388323710878, 31.09081505442903648 ) ) ;
#14660 = CARTESIAN_POINT ( 'NONE',  ( 5.082755093536325930, -23.84375000204838457, -5.082755093536325042 ) ) ;
#14661 = CARTESIAN_POINT ( 'NONE',  ( 6.125000000000095923, -15.62228920881129390, 14.41094225130415651 ) ) ;
#14662 = CARTESIAN_POINT ( 'NONE',  ( -12.61670886434728267, 18.48906243878285238, 8.368148073796660924 ) ) ;
#14663 = CARTESIAN_POINT ( 'NONE',  ( 5.000000000000000000, -66.75027687118438280, 15.74257363030519663 ) ) ;
#14664 = CARTESIAN_POINT ( 'NONE',  ( -7.996668422906947349, 48.00000000000000000, -78.85453279917602742 ) ) ;
#14665 = CARTESIAN_POINT ( 'NONE',  ( 7.554474191401430616, -6.015471045889135837, 14.04826599594835557 ) ) ;
#14666 = FACE_OUTER_BOUND ( 'NONE', #53405, .T. ) ;
#14667 = AXIS2_PLACEMENT_3D ( 'NONE', #82638, #90199, #49190 ) ;
#14668 = CARTESIAN_POINT ( 'NONE',  ( 22.35256411763875661, 303.1536920125136589, -9.935383756229917651 ) ) ;
#14669 = CARTESIAN_POINT ( 'NONE',  ( -38.30955110355977666, -22.21941382654016905, 33.68855472650722049 ) ) ;
#14670 = ORIENTED_EDGE ( 'NONE', *, *, #92109, .T. ) ;
#14671 = SURFACE_SIDE_STYLE ('',( #96157 ) ) ;
#14672 = CARTESIAN_POINT ( 'NONE',  ( 38.28027864600694130, -42.97064924050712165, 38.10376371723102551 ) ) ;
#14673 =( GEOMETRIC_REPRESENTATION_CONTEXT ( 3 ) GLOBAL_UNCERTAINTY_ASSIGNED_CONTEXT ( ( #42686 ) ) GLOBAL_UNIT_ASSIGNED_CONTEXT ( ( #58899, #34115, #66986 ) ) REPRESENTATION_CONTEXT ( 'NONE', 'WORKASPACE' ) );
#14674 = CARTESIAN_POINT ( 'NONE',  ( 14.86825985028009711, -3.469446951953614189E-15, -8.569529079650944681 ) ) ;
#14675 = ORIENTED_EDGE ( 'NONE', *, *, #21063, .F. ) ;
#14676 = CARTESIAN_POINT ( 'NONE',  ( 33.68177706158876106, 464.5004658938952957, 17.05886715805488407 ) ) ;
#14677 = EDGE_CURVE ( 'NONE', #77056, #45751, #35531, .T. ) ;
#14678 = CARTESIAN_POINT ( 'NONE',  ( -74.34775434501226243, -38.32892518166006823, 163.3919322230082969 ) ) ;
#14679 = STYLED_ITEM ( 'NONE', ( #13575 ), #87845 ) ;
#14680 = ORIENTED_EDGE ( 'NONE', *, *, #67180, .T. ) ;
#14682 = LINE ( 'NONE', #81528, #16462 ) ;
#14681 = DIRECTION ( 'NONE',  ( -1.000000000000000000, -0.000000000000000000, -0.000000000000000000 ) ) ;
#14683 = DIRECTION ( 'NONE',  ( -1.000000000000000000, 0.000000000000000000, 0.000000000000000000 ) ) ;
#14684 = CARTESIAN_POINT ( 'NONE',  ( 22.33349330513380337, 4.898587196589405926E-16, -4.000000000000001776 ) ) ;
#14685 = CIRCLE ( 'NONE', #38894, 5.000000000000001776 ) ;
#14686 =( GEOMETRIC_REPRESENTATION_CONTEXT ( 3 ) GLOBAL_UNCERTAINTY_ASSIGNED_CONTEXT ( ( #85909 ) ) GLOBAL_UNIT_ASSIGNED_CONTEXT ( ( #28104, #85241, #58851 ) ) REPRESENTATION_CONTEXT ( 'NONE', 'WORKASPACE' ) );
#14687 = CARTESIAN_POINT ( 'NONE',  ( 0.000000000000000000, 0.000000000000000000, -1.161000000000000032 ) ) ;
#14688 = CARTESIAN_POINT ( 'NONE',  ( -38.39281685574185587, 437.9237591976292947, 4.303444208756491030 ) ) ;
#14689 = CIRCLE ( 'NONE', #74967, 3.400000000000000355 ) ;
#14690 = CARTESIAN_POINT ( 'NONE',  ( -48.69590189480585707, 13.58600142653171972, -16.66526863408559578 ) ) ;
#14691 = CARTESIAN_POINT ( 'NONE',  ( 0.000000000000000000, 0.000000000000000000, 0.000000000000000000 ) ) ;
#14692 = CARTESIAN_POINT ( 'NONE',  ( 93.72088428965379592, -60.00000000000000711, 39.00990964174581421 ) ) ;
#14693 = AXIS2_PLACEMENT_3D ( 'NONE', #55423, #47340, #80234 ) ;
#14694 = CARTESIAN_POINT ( 'NONE',  ( -43.47770857297125957, 484.8227827122622102, 4.253339224813452724 ) ) ;
#14695 = CIRCLE ( 'NONE', #81824, 5.000000000000002665 ) ;
#14696 = CARTESIAN_POINT ( 'NONE',  ( 0.000000000000000000, 34.08768991669519721, 0.000000000000000000 ) ) ;
#14697 = CARTESIAN_POINT ( 'NONE',  ( 12.33349330513380337, 4.898587196589405926E-16, -4.000000000000001776 ) ) ;
#14698 = ADVANCED_FACE ( 'NONE', ( #18925 ), #37310, .T. ) ;
#14699 = ORIENTED_EDGE ( 'NONE', *, *, #94152, .F. ) ;
#14700 = EDGE_CURVE ( 'NONE', #60873, #3475, #90631, .T. ) ;
#14701 = CARTESIAN_POINT ( 'NONE',  ( -89.32516398097905608, -29.99999999998676259, 6.631855125688738362 ) ) ;
#14702 = VERTEX_POINT ( 'NONE', #58824 ) ;
#14703 = CARTESIAN_POINT ( 'NONE',  ( -9.819569948016248162, -57.58692256219968897, 28.90708029074982477 ) ) ;
#14704 = CARTESIAN_POINT ( 'NONE',  ( -15.20015366321276495, 3.406002745437296753, 3.875710626047840446 ) ) ;
#14705 = CARTESIAN_POINT ( 'NONE',  ( 9.075061004355044147, 14.05394893828536063, -6.138968940038654494E-13 ) ) ;
#14706 = LINE ( 'NONE', #72426, #34627 ) ;
#14707 = CARTESIAN_POINT ( 'NONE',  ( 82.13300407177993634, -37.81708028406786326, -13.51745076886380659 ) ) ;
#14708 = CARTESIAN_POINT ( 'NONE',  ( -7.188101187500002709, -24.68750000204838457, 2.977408999572648707 ) ) ;
#14709 = DIRECTION ( 'NONE',  ( -1.000000000000000000, -1.224606353822377258E-16, -0.000000000000000000 ) ) ;
#14710 = FACE_OUTER_BOUND ( 'NONE', #42710, .T. ) ;
#14711 = CARTESIAN_POINT ( 'NONE',  ( 6.819782173531151237, 41.52802923938777013, -70.37695045978405517 ) ) ;
#14712 = ORIENTED_EDGE ( 'NONE', *, *, #30508, .F. ) ;
#14714 = EDGE_LOOP ( 'NONE', ( #29885, #38289, #77312, #3784 ) ) ;
#14713 = CARTESIAN_POINT ( 'NONE',  ( 4.382959417677087188, -1.862050784382271562, 102.7400018439556391 ) ) ;
#14715 = CARTESIAN_POINT ( 'NONE',  ( 80.37524443596792878, -46.43599209193401123, 156.8239579507224448 ) ) ;
#14716 = ADVANCED_FACE ( 'NONE', ( #93311 ), #33838, .T. ) ;
#14717 = CARTESIAN_POINT ( 'NONE',  ( -38.32973030926034141, 27.37225254236124528, -13.21033226210355416 ) ) ;
#14718 = EDGE_LOOP ( 'NONE', ( #71760, #84124, #22315, #58632 ) ) ;
#14719 = CARTESIAN_POINT ( 'NONE',  ( -12.50000000000000711, 41.24423117302004727, -72.11661107032048790 ) ) ;
#14720 = CARTESIAN_POINT ( 'NONE',  ( -1.235501149773866825, 15.31955389872309858, -50.72623786250530742 ) ) ;
#14721 = CARTESIAN_POINT ( 'NONE',  ( -7.188101187500000044, -10.90625000204838457, -8.802885111219163269E-16 ) ) ;
#14722 = DIRECTION ( 'NONE',  ( 0.000000000000000000, 0.000000000000000000, 1.000000000000000000 ) ) ;
#14723 = VECTOR ( 'NONE', #67033, 1000.000000000000000 ) ;
#14724 = CARTESIAN_POINT ( 'NONE',  ( -44.31189620312834876, -57.68384900168454976, 63.67342368891909388 ) ) ;
#14725 = EDGE_CURVE ( 'NONE', #69385, #36626, #97640, .T. ) ;
#14726 = CARTESIAN_POINT ( 'NONE',  ( 6.463344223170843783, -7.245769408789100474, -1.129975644293425230 ) ) ;
#14727 = ORIENTED_EDGE ( 'NONE', *, *, #80554, .F. ) ;
#14728 =( NAMED_UNIT ( * ) PLANE_ANGLE_UNIT ( ) SI_UNIT ( $, .RADIAN. ) );
#14729 = DIRECTION ( 'NONE',  ( 0.000000000000000000, 0.000000000000000000, 1.000000000000000000 ) ) ;
#14730 = DIRECTION ( 'NONE',  ( 0.000000000000000000, 1.000000000000000000, 0.000000000000000000 ) ) ;
#14731 = CARTESIAN_POINT ( 'NONE',  ( 4.898587196589412829E-16, -19.62499999999999289, -8.000000000000000000 ) ) ;
#14732 = CARTESIAN_POINT ( 'NONE',  ( 48.15175547875055173, 14.66334354488943426, -16.85535821593556349 ) ) ;
#14733 = EDGE_LOOP ( 'NONE', ( #106732, #79210, #63158, #7266, #10188, #46390 ) ) ;
#14734 = CARTESIAN_POINT ( 'NONE',  ( -8.000000000000001776, -10.34375000409676915, 3.313708498984758943 ) ) ;
#14735 = CARTESIAN_POINT ( 'NONE',  ( 0.7145311798163234140, -9.237604307034013473, 6.198474679904167468E-16 ) ) ;
#14736 = SURFACE_SIDE_STYLE ('',( #55714 ) ) ;
#14737 = CARTESIAN_POINT ( 'NONE',  ( -1.000000000000000222, -5.000000000000000000, -14.14213562373095101 ) ) ;
#14738 = B_SPLINE_CURVE_WITH_KNOTS ( 'NONE', 3,
 ( #46909, #31298, #64184, #20592, #21102, #70671, #86350, #95472, #12415, #5406, #4340, #37811, #62588, #54447, #87400, #13472, #90029, #73294, #57115, #25327 ),
 .UNSPECIFIED., .F., .F.,
 ( 4, 2, 2, 2, 2, 2, 2, 2, 2, 4 ),
 ( 0.007172846040326944991, 0.007676791773118825553, 0.008180737505910706114, 0.008684683238702585809, 0.009188628971494467237, 0.009692574704286346932, 0.01019652043707822836, 0.01070046616987010805, 0.01095243903626605050, 0.01120441190266199122 ),
 .UNSPECIFIED. ) ;
#14739 = CARTESIAN_POINT ( 'NONE',  ( -9.797537890442933772, 88.46557797666194745, 2.014215961808879296 ) ) ;
#14740 = CARTESIAN_POINT ( 'NONE',  ( 7.999999999999998224, -20.09374999999999289, 3.313708498984766049 ) ) ;
#14742 = ADVANCED_FACE ( 'NONE', ( #74443 ), #1043, .T. ) ;
#14741 = SHAPE_DEFINITION_REPRESENTATION ( #61402, #81203 ) ;
#14743 = CARTESIAN_POINT ( 'NONE',  ( -6.662856812433364695, -15.38938976169041695, 14.67262768018345298 ) ) ;
#14744 = ORIENTED_EDGE ( 'NONE', *, *, #82117, .F. ) ;
#14745 = DIRECTION ( 'NONE',  ( 0.000000000000000000, -1.000000000000000000, 0.000000000000000000 ) ) ;
#14746 =( NAMED_UNIT ( * ) PLANE_ANGLE_UNIT ( ) SI_UNIT ( $, .RADIAN. ) );
#14747 = DIRECTION ( 'NONE',  ( 0.000000000000000000, -1.000000000000000000, 0.000000000000000000 ) ) ;
#14748 = CARTESIAN_POINT ( 'NONE',  ( 53.11664595332064209, -36.25651953744597478, -35.66653243501286852 ) ) ;
#14749 = DIRECTION ( 'NONE',  ( -1.000000000000000000, 0.000000000000000000, 0.000000000000000000 ) ) ;
#14750 = AXIS2_PLACEMENT_3D ( 'NONE', #31729, #64616, #97483 ) ;
#14751 = EDGE_LOOP ( 'NONE', ( #94010, #37126, #54611, #59031 ) ) ;
#14752 = DIRECTION ( 'NONE',  ( 0.5735764363510490460, 0.8191520442889896891, 0.000000000000000000 ) ) ;
#14753 = CARTESIAN_POINT ( 'NONE',  ( 95.17612642465779516, -57.62056889977026941, 204.5393882615723271 ) ) ;
#14754 = CARTESIAN_POINT ( 'NONE',  ( -4.205882352941162416, -5.000000000000000000, -72.69916451482997388 ) ) ;
#14755 = CARTESIAN_POINT ( 'NONE',  ( -5.619193549420737455, -4.261310591078485643, -5.875704392893697836 ) ) ;
#14756 = DIRECTION ( 'NONE',  ( -1.000000000000000000, -1.224606353822377258E-16, -0.000000000000000000 ) ) ;
#14757 = VECTOR ( 'NONE', #47706, 1000.000000000000000 ) ;
#14758 = CARTESIAN_POINT ( 'NONE',  ( -37.54559764570181812, 464.1143081516144662, 19.43664670202813838 ) ) ;
#14759 = CARTESIAN_POINT ( 'NONE',  ( -72.22471733123828130, -60.00000000000000000, 155.9617568056963819 ) ) ;
#14760 = AXIS2_PLACEMENT_3D ( 'NONE', #89664, #31454, #72919 ) ;
#14761 = AXIS2_PLACEMENT_3D ( 'NONE', #62692, #54563, #89615 ) ;
#14762 = CARTESIAN_POINT ( 'NONE',  ( -44.43774958859658142, 337.2802145563449017, 0.2445019049555710311 ) ) ;
#14763 = CARTESIAN_POINT ( 'NONE',  ( 100.0424503805845831, 6.123233995736582872E-16, -5.000000000000011546 ) ) ;
#14764 = CARTESIAN_POINT ( 'NONE',  ( 63.25915952246698026, 50.00000000000000000, 0.7870165385177050332 ) ) ;
#14765 = CARTESIAN_POINT ( 'NONE',  ( -86.30709385375372733, -21.08530101006160606, 179.9897705061360682 ) ) ;
#14766 = ORIENTED_EDGE ( 'NONE', *, *, #96195, .F. ) ;
#14767 = CARTESIAN_POINT ( 'NONE',  ( 34.68718586615926824, 326.8403318033771825, -4.364199029797471319 ) ) ;
#14768 = CIRCLE ( 'NONE', #66450, 5.000000000000010658 ) ;
#14769 = AXIS2_PLACEMENT_3D ( 'NONE', #71921, #89173, #55707 ) ;
#14770 = ADVANCED_FACE ( 'NONE', ( #93839 ), #92307, .T. ) ;
#14771 = ADVANCED_FACE ( 'NONE', ( #28079 ), #71147, .T. ) ;
#14772 = ORIENTED_EDGE ( 'NONE', *, *, #86024, .T. ) ;
#14773 = CARTESIAN_POINT ( 'NONE',  ( 12.49986889690059222, -3.000000000000002665, -76.70852482682694529 ) ) ;
#14774 = EDGE_CURVE ( 'NONE', #75040, #103547, #102718, .T. ) ;
#14775 = CARTESIAN_POINT ( 'NONE',  ( -20.46799911788806625, 303.8501572683899781, -10.00035002725203448 ) ) ;
#14776 = CARTESIAN_POINT ( 'NONE',  ( 42.08762648273143014, 487.0030674539048618, 9.106351919857845090 ) ) ;
#14777 = CARTESIAN_POINT ( 'NONE',  ( -32.22120753352784561, 464.6691781026584636, 10.60621122532581140 ) ) ;
#14779 = CIRCLE ( 'NONE', #2780, 11.27631144943088337 ) ;
#14778 = DIRECTION ( 'NONE',  ( 0.000000000000000000, 0.1323839925376418813, 0.9911985061125716534 ) ) ;
#14780 = ORIENTED_EDGE ( 'NONE', *, *, #46849, .T. ) ;
#14781 = CARTESIAN_POINT ( 'NONE',  ( 19.16335059359749593, 50.00000000000000000, 60.36429063721810451 ) ) ;
#14782 = EDGE_CURVE ( 'NONE', #21618, #49400, #83752, .T. ) ;
#14783 = CARTESIAN_POINT ( 'NONE',  ( 11.69764001847466339, 21.03308801239159109, -7.673093909533472257 ) ) ;
#14784 = CARTESIAN_POINT ( 'NONE',  ( 2.227375807148842313, -1.734723475976807094E-15, -17.01589776168603407 ) ) ;
#14785 = CARTESIAN_POINT ( 'NONE',  ( 0.000000000000000000, 5.629165124598848102, -3.250000000000007105 ) ) ;
#14786 = CARTESIAN_POINT ( 'NONE',  ( 78.96299857857128757, -14.21045842199439946, -22.44940295094700033 ) ) ;
#14787 = CARTESIAN_POINT ( 'NONE',  ( -81.05843653766993384, -32.56278768442193439, 144.8551522210765370 ) ) ;
#14788 = ORIENTED_EDGE ( 'NONE', *, *, #8211, .F. ) ;
#14789 = CARTESIAN_POINT ( 'NONE',  ( 4.154910845142357978, -29.99999999999994316, 36.99135396797706932 ) ) ;
#14790 =( LENGTH_UNIT ( ) NAMED_UNIT ( * ) SI_UNIT ( .MILLI., .METRE. ) );
#14791 = CARTESIAN_POINT ( 'NONE',  ( 78.27301562901895693, -57.50947999237905606, 196.9356207485391224 ) ) ;
#14792 = B_SPLINE_CURVE_WITH_KNOTS ( 'NONE', 3,
 ( #91352, #16931, #9332, #65473, #23450, #97830, #98872, #90276, #15320, #65997 ),
 .UNSPECIFIED., .F., .F.,
 ( 4, 2, 2, 2, 4 ),
 ( 0.000000000000000000, 0.001993803085173305196, 0.003987606170346610392, 0.005981409255519916021, 0.007975212340693220783 ),
 .UNSPECIFIED. ) ;
#14793 = DIRECTION ( 'NONE',  ( 0.000000000000000000, 0.000000000000000000, 1.000000000000000000 ) ) ;
#14794 = CARTESIAN_POINT ( 'NONE',  ( 30.59828542553725583, 308.7413687888409299, -8.648601138669905097 ) ) ;
#14795 = CARTESIAN_POINT ( 'NONE',  ( -30.00000000000000000, 461.8887775513397855, 11.55279652844097171 ) ) ;
#14796 = VERTEX_POINT ( 'NONE', #37762 ) ;
#14797 = B_SPLINE_CURVE_WITH_KNOTS ( 'NONE', 3,
 ( #15283, #55716, #81069, #35217 ),
 .UNSPECIFIED., .F., .F.,
 ( 4, 4 ),
 ( 1.497901326927488094E-16, 0.0002642584603499430781 ),
 .UNSPECIFIED. ) ;
#14798 = CARTESIAN_POINT ( 'NONE',  ( 7.500000000000000000, 2.575910028905302074, -0.3641256808890085961 ) ) ;
#14799 = LINE ( 'NONE', #66013, #1424 ) ;
#14801 = CARTESIAN_POINT ( 'NONE',  ( -105.4329160415097562, -60.15501871978297288, 153.9737639351797327 ) ) ;
#14800 = CARTESIAN_POINT ( 'NONE',  ( -15.50702112914504838, 36.95515616017750204, 23.25462944313558111 ) ) ;
#14802 = CARTESIAN_POINT ( 'NONE',  ( 7.188101187500000044, -17.65625000204838457, 0.000000000000000000 ) ) ;
#14803 = PRESENTATION_LAYER_ASSIGNMENT (  '', '', ( #981 ) ) ;
#14804 = CARTESIAN_POINT ( 'NONE',  ( 9.165151389911677882, 84.73264844392886630, -4.000000000000000000 ) ) ;
#14805 = CARTESIAN_POINT ( 'NONE',  ( 6.849721346867525540, 41.84384207023756375, -59.83401400531045056 ) ) ;
#14806 = CARTESIAN_POINT ( 'NONE',  ( -17.71951158999537057, 45.45134770963998960, -4.750929343604651578 ) ) ;
#14807 = DIRECTION ( 'NONE',  ( 0.000000000000000000, -0.8660254037844375974, 0.5000000000000019984 ) ) ;
#14808 = VERTEX_POINT ( 'NONE', #85766 ) ;
#14809 = DIRECTION ( 'NONE',  ( 0.000000000000000000, -1.000000000000000000, 0.000000000000000000 ) ) ;
#14811 = CARTESIAN_POINT ( 'NONE',  ( 31.71700056584302629, -53.37470450013292123, 36.28623570309412116 ) ) ;
#14810 = CARTESIAN_POINT ( 'NONE',  ( -6.891666673413887896E-15, -70.53271932724189242, 13.00000000000000000 ) ) ;
#14812 = CARTESIAN_POINT ( 'NONE',  ( 23.61948937802333504, 28.00997096501933825, -30.76980700055193552 ) ) ;
#14813 = ORIENTED_EDGE ( 'NONE', *, *, #19938, .F. ) ;
#14814 = EDGE_CURVE ( 'NONE', #16299, #99968, #11840, .T. ) ;
#14815 = ORIENTED_EDGE ( 'NONE', *, *, #43138, .T. ) ;
#14817 = FACE_BOUND ( 'NONE', #103894, .T. ) ;
#14816 = SURFACE_STYLE_FILL_AREA ( #30512 ) ;
#14818 = FACE_OUTER_BOUND ( 'NONE', #20256, .T. ) ;
#14819 = DIRECTION ( 'NONE',  ( 0.000000000000000000, -1.000000000000000000, 0.000000000000000000 ) ) ;
#14820 = CARTESIAN_POINT ( 'NONE',  ( 14.31968076504620946, 0.6252655212105243665, 14.98772011519035630 ) ) ;
#14821 = CARTESIAN_POINT ( 'NONE',  ( 0.000000000000000000, 0.000000000000000000, -13.00000000000000000 ) ) ;
#14822 = ORIENTED_EDGE ( 'NONE', *, *, #73922, .F. ) ;
#14823 = EDGE_CURVE ( 'NONE', #2515, #54844, #69989, .T. ) ;
#14824 = CARTESIAN_POINT ( 'NONE',  ( 32.68672512615790993, -60.00000000000000711, -40.59438170049026695 ) ) ;
#14825 = AXIS2_PLACEMENT_3D ( 'NONE', #96910, #30605, #13846 ) ;
#14826 = CARTESIAN_POINT ( 'NONE',  ( 22.45260625274932664, 25.48533499626559262, -32.95744641864007463 ) ) ;
#14827 = CARTESIAN_POINT ( 'NONE',  ( 2.936182742933428427E-09, -59.99999999999998579, 41.99999999999667466 ) ) ;
#14828 = DIRECTION ( 'NONE',  ( 0.000000000000000000, 0.000000000000000000, 1.000000000000000000 ) ) ;
#14829 = CARTESIAN_POINT ( 'NONE',  ( -47.77471032523668981, 17.34854710534463251, -14.37330285161499255 ) ) ;
#14830 = EDGE_CURVE ( 'NONE', #88025, #40649, #4476, .T. ) ;
#14831 = ORIENTED_EDGE ( 'NONE', *, *, #72563, .F. ) ;
#14832 = VECTOR ( 'NONE', #94207, 1000.000000000000000 ) ;
#14833 = VERTEX_POINT ( 'NONE', #44770 ) ;
#14834 = ORIENTED_EDGE ( 'NONE', *, *, #19819, .T. ) ;
#14835 = CARTESIAN_POINT ( 'NONE',  ( 29.98176661990081371, 0.000000000000000000, 5.000000000000002665 ) ) ;
#14836 = CARTESIAN_POINT ( 'NONE',  ( -38.16423750294135431, 438.4460316866491212, 23.47818834081018124 ) ) ;
#14837 = CARTESIAN_POINT ( 'NONE',  ( 33.14180294099352864, 415.2512948571491620, 25.78082742257582893 ) ) ;
#14838 = CARTESIAN_POINT ( 'NONE',  ( -44.78715759568187593, 344.4533273986938298, 1.769479026230448504 ) ) ;
#14839 = CARTESIAN_POINT ( 'NONE',  ( 69.67238219402268840, -4.000000000000000000, 4.898587196589421703E-16 ) ) ;
#14840 = CARTESIAN_POINT ( 'NONE',  ( -46.00000000000000711, 486.1375394786616084, 2.115994497953515019 ) ) ;
#14841 = CARTESIAN_POINT ( 'NONE',  ( 6.463481858019720860, -7.246446802359431949, 1.128819432756288599 ) ) ;
#14842 = ORIENTED_EDGE ( 'NONE', *, *, #96907, .T. ) ;
#14843 = DIRECTION ( 'NONE',  ( -0.000000000000000000, -1.000000000000000000, -0.000000000000000000 ) ) ;
#14844 = B_SPLINE_CURVE_WITH_KNOTS ( 'NONE', 3,
 ( #18235, #52165, #34961, #50553, #68910, #36568, #100188, #67828, #59215, #75374, #19859, #76975, #26355, #76434, #85077, #35492, #51089, #10115, #100715, #59751, #11161, #84550, #3091, #27416, #93169, #36038, #72068, #69958, #37628, #86166, #104429, #29533, #6255, #5741 ),
 .UNSPECIFIED., .F., .F.,
 ( 4, 2, 2, 2, 2, 2, 2, 2, 2, 2, 2, 2, 2, 2, 2, 2, 4 ),
 ( 2.814585498623475875E-17, 0.0007899309203816313628, 0.001579861840763234536, 0.002369792761144837601, 0.003159723681526440883, 0.003949654601908043731, 0.004739585522289646580, 0.005529516442671250295, 0.006319447363052853144, 0.007109378283434455992, 0.007899309203816059707, 0.008689240124197663423, 0.009479171044579265404, 0.01026910196496086912, 0.01105903288534247284, 0.01184896380572407482, 0.01263889472610567853 ),
 .UNSPECIFIED. ) ;
#14845 = ORIENTED_EDGE ( 'NONE', *, *, #11529, .F. ) ;
#14846 = CARTESIAN_POINT ( 'NONE',  ( -6.125000000000000000, -60.71953810597580059, 14.41094225130411033 ) ) ;
#14847 = CARTESIAN_POINT ( 'NONE',  ( -37.46929538836621276, 50.00000000000000000, -55.58823529426164356 ) ) ;
#14848 = DIRECTION ( 'NONE',  ( -1.000000000000000000, -1.224606353822377258E-16, -0.000000000000000000 ) ) ;
#14849 = AXIS2_PLACEMENT_3D ( 'NONE', #8585, #56597, #48502 ) ;
#14850 = COLOUR_RGB ( '', 0.72549020, 0.75294118, 0.79215686) ;
#14851 = CIRCLE ( 'NONE', #23429, 4.250000000000000000 ) ;
#14852 = AXIS2_PLACEMENT_3D ( 'NONE', #7884, #89361, #54842 ) ;
#14853 = CARTESIAN_POINT ( 'NONE',  ( 22.33349330513380693, 4.000000000000002665, 0.000000000000000000 ) ) ;
#14854 = CARTESIAN_POINT ( 'NONE',  ( 65.57816012826067720, -46.43382891351115660, 91.59682735943974308 ) ) ;
#14855 = ORIENTED_EDGE ( 'NONE', *, *, #32565, .T. ) ;
#14856 = CARTESIAN_POINT ( 'NONE',  ( 42.09158233638500235, 465.7816406625409513, 14.79318349170029734 ) ) ;
#14857 = AXIS2_PLACEMENT_3D ( 'NONE', #15682, #7721, #14610 ) ;
#14858 = CARTESIAN_POINT ( 'NONE',  ( -5.744562646538028616, 12.72950497522988300, 4.000000000000000000 ) ) ;
#14859 = CARTESIAN_POINT ( 'NONE',  ( -22.45002021702217121, -57.67118433041228798, -43.66150106997372404 ) ) ;
#14860 = EDGE_CURVE ( 'NONE', #19102, #94625, #32154, .T. ) ;
#14861 = ORIENTED_EDGE ( 'NONE', *, *, #5983, .F. ) ;
#14862 = CARTESIAN_POINT ( 'NONE',  ( 47.07350275986915733, 18.64911821952824056, 14.79681583022511404 ) ) ;
#14863 = CIRCLE ( 'NONE', #75128, 4.172000000000009479 ) ;
#14864 = CONICAL_SURFACE ( 'NONE', #42436, 7.500000000000000888, 0.8594454914424817238 ) ;
#14865 = DIRECTION ( 'NONE',  ( -1.000000000000000000, -1.224606353822377258E-16, -0.000000000000000000 ) ) ;
#14866 = CARTESIAN_POINT ( 'NONE',  ( 5.656854249492380582, -30.50000000409677270, -5.656854249492379694 ) ) ;
#14867 =( NAMED_UNIT ( * ) SI_UNIT ( $, .STERADIAN. ) SOLID_ANGLE_UNIT ( ) );
#14868 = CARTESIAN_POINT ( 'NONE',  ( 86.09607050833426456, -57.43433071910509113, 193.2105974690565802 ) ) ;
#14869 = CARTESIAN_POINT ( 'NONE',  ( -5.863284779130247593, 4.691109759206348429, 4.999999999999999112 ) ) ;
#14870 = SURFACE_STYLE_USAGE ( .BOTH. , #21948 ) ;
#14871 = EDGE_CURVE ( 'NONE', #76918, #33707, #78538, .T. ) ;
#14872 = CARTESIAN_POINT ( 'NONE',  ( -42.18756898894582719, 484.4522853017719513, -2.425645685620454906 ) ) ;
#14873 = EDGE_LOOP ( 'NONE', ( #70025, #97365 ) ) ;
#14874 = CARTESIAN_POINT ( 'NONE',  ( 26.69900261086841198, 1.482358050883964840E-15, 0.000000000000000000 ) ) ;
#14875 = DIRECTION ( 'NONE',  ( 1.000000000000000000, 0.000000000000000000, -0.000000000000000000 ) ) ;
#14876 = AXIS2_PLACEMENT_3D ( 'NONE', #36356, #27734, #77300 ) ;
#14877 = CARTESIAN_POINT ( 'NONE',  ( 34.08754861723457452, -59.99999999999998579, 45.65693729473046147 ) ) ;
#14878 = CARTESIAN_POINT ( 'NONE',  ( -100.1431153105590823, -30.00000000000001066, 184.9454591299870856 ) ) ;
#14879 = DIRECTION ( 'NONE',  ( 1.000000000000000000, 0.000000000000000000, 0.000000000000000000 ) ) ;
#14880 = CARTESIAN_POINT ( 'NONE',  ( 40.40776752368557112, -57.69128819681711917, 56.34745769540169391 ) ) ;
#14881 = CARTESIAN_POINT ( 'NONE',  ( 15.66820627147619582, -1.212563469572859987, 14.95337489854003898 ) ) ;
#14882 = CARTESIAN_POINT ( 'NONE',  ( -19.53695861423244651, 43.95068861312910258, -83.64112249031806812 ) ) ;
#14883 = DIRECTION ( 'NONE',  ( 0.000000000000000000, 0.000000000000000000, 1.000000000000000000 ) ) ;
#14884 = CARTESIAN_POINT ( 'NONE',  ( -9.999999999997886135, 15.11700796860587381, 0.7408669144214915514 ) ) ;
#14885 = CYLINDRICAL_SURFACE ( 'NONE', #97755, 4.000000000000000000 ) ;
#14886 = CARTESIAN_POINT ( 'NONE',  ( -25.02205373457694648, -60.00000000000000711, 41.17636800131604247 ) ) ;
#14887 = SURFACE_STYLE_USAGE ( .BOTH. , #106557 ) ;
#14888 = AXIS2_PLACEMENT_3D ( 'NONE', #32795, #49471, #9009 ) ;
#14889 = CARTESIAN_POINT ( 'NONE',  ( -86.74851537548293834, -20.66079247287741794, 185.3133297257026015 ) ) ;
#14890 = ORIENTED_EDGE ( 'NONE', *, *, #8473, .T. ) ;
#14891 = CARTESIAN_POINT ( 'NONE',  ( 17.50000000000007461, 48.00000000000153477, 62.61753806507840636 ) ) ;
#14892 = CARTESIAN_POINT ( 'NONE',  ( 33.85195725564128821, 465.2464970902066739, 17.18122764674265568 ) ) ;
#14893 = CARTESIAN_POINT ( 'NONE',  ( -11.24664110559554153, -32.51291048916622373, 29.33424993359241739 ) ) ;
#14894 =( BOUNDED_SURFACE ( )  B_SPLINE_SURFACE ( 2, 3, ( 
 ( #55294, #11653, #12189, #36522, #45119, #77998, #102270, #61295, #102811, #37043 ),
 ( #28972, #64478, #82228, #23500, #81679, #56345, #98929, #15907, #105967, #97347 ),
 ( #90329, #31076, #41244, #66052, #64992, #89808, #22970, #16437, #40709, #96841 ) ),
 .UNSPECIFIED., .F., .F., .F. ) 
 B_SPLINE_SURFACE_WITH_KNOTS ( ( 3, 3 ),
 ( 4, 2, 2, 2, 4 ),
 ( 0.000000000000000000, 1.000000000000000000 ),
 ( 0.000000000000000000, 0.01533609919089652315, 0.03067219838179304631, 0.04600829757268956599, 0.06134439676358609261 ),
 .UNSPECIFIED. ) 
 GEOMETRIC_REPRESENTATION_ITEM ( )  RATIONAL_B_SPLINE_SURFACE ( (
 ( 1.000000000000000000, 1.000000000000000000, 1.000000000000000000, 1.000000000000000000, 1.000000000000000000, 1.000000000000000000, 1.000000000000000000, 1.000000000000000000, 1.000000000000000000, 1.000000000000000000),
 ( 1.857142857142858317, 1.857142857142858317, 1.857142857142858317, 1.857142857142858317, 1.857142857142858317, 1.857142857142858317, 1.857142857142858317, 1.857142857142858317, 1.857142857142858317, 1.857142857142858317),
 ( 1.000000000000000000, 1.000000000000000000, 1.000000000000000000, 1.000000000000000000, 1.000000000000000000, 1.000000000000000000, 1.000000000000000000, 1.000000000000000000, 1.000000000000000000, 1.000000000000000000) ) ) 
 REPRESENTATION_ITEM ( '' )  SURFACE ( )  );
#14895 = DIRECTION ( 'NONE',  ( -0.8191520442889911324, 1.003171929053523884E-16, 0.5735764363510470476 ) ) ;
#14896 = EDGE_CURVE ( 'NONE', #550, #67342, #45823, .T. ) ;
#14897 = AXIS2_PLACEMENT_3D ( 'NONE', #63466, #89317, #40749 ) ;
#14898 = ORIENTED_EDGE ( 'NONE', *, *, #1983, .T. ) ;
#14899 = CARTESIAN_POINT ( 'NONE',  ( 80.97977184163765685, -5.000000000000000000, 6.123233995736778115E-16 ) ) ;
#14900 = CARTESIAN_POINT ( 'NONE',  ( -9.085304181916990629, -4.999999999999727329, -17.32925045961839317 ) ) ;
#14901 = CARTESIAN_POINT ( 'NONE',  ( -12.13034742782427777, 41.99999999999999289, -93.82352941176471006 ) ) ;
#14902 = CIRCLE ( 'NONE', #92442, 4.000000000000000888 ) ;
#14903 = AXIS2_PLACEMENT_3D ( 'NONE', #67202, #101684, #101148 ) ;
#14904 = EDGE_CURVE ( 'NONE', #56970, #53610, #54403, .T. ) ;
#14905 = PRESENTATION_STYLE_ASSIGNMENT (( #27569 ) ) ;
#14906 = CARTESIAN_POINT ( 'NONE',  ( 62.83177751537848366, -60.00000000000000000, 110.1979811477270204 ) ) ;
#14907 = DIRECTION ( 'NONE',  ( 0.000000000000000000, -1.000000000000000000, 0.000000000000000000 ) ) ;
#14908 = ORIENTED_EDGE ( 'NONE', *, *, #81112, .T. ) ;
#14909 = FACE_OUTER_BOUND ( 'NONE', #4750, .T. ) ;
#14910 = CARTESIAN_POINT ( 'NONE',  ( 0.000000000000000000, 0.000000000000000000, 4.000000000000000000 ) ) ;
#14911 = AXIS2_PLACEMENT_3D ( 'NONE', #2193, #9755, #68011 ) ;
#14912 = CIRCLE ( 'NONE', #94168, 5.000000000000011546 ) ;
#14913 = CARTESIAN_POINT ( 'NONE',  ( 5.371950044183567030, -2.205168805904308194, 104.0625755208173331 ) ) ;
#14914 = FILL_AREA_STYLE ('',( #7354 ) ) ;
#14915 = CARTESIAN_POINT ( 'NONE',  ( -4.980618096941614503, -3.539029780453323948, 103.2912570477108716 ) ) ;
#14916 = ORIENTED_EDGE ( 'NONE', *, *, #26052, .F. ) ;
#14917 = AXIS2_PLACEMENT_3D ( 'NONE', #12791, #38691, #21457 ) ;
#14919 = VECTOR ( 'NONE', #95707, 1000.000000000000000 ) ;
#14918 = CARTESIAN_POINT ( 'NONE',  ( -27.89321753534029824, 311.6752679970134068, 11.81702633892450471 ) ) ;
#14920 = ORIENTED_EDGE ( 'NONE', *, *, #48323, .T. ) ;
#14921 = DIRECTION ( 'NONE',  ( 0.000000000000000000, 1.000000000000000000, 0.000000000000000000 ) ) ;
#14922 = DIRECTION ( 'NONE',  ( 1.000000000000000000, 1.224606353822377258E-16, 0.000000000000000000 ) ) ;
#14923 = LINE ( 'NONE', #48353, #14021 ) ;
#14924 = VERTEX_POINT ( 'NONE', #55992 ) ;
#14925 = EDGE_CURVE ( 'NONE', #85025, #8093, #13958, .T. ) ;
#14926 = CARTESIAN_POINT ( 'NONE',  ( -9.172731267813459155, 6.899963662535627762, -3.046434832396871961 ) ) ;
#14927 = CARTESIAN_POINT ( 'NONE',  ( -80.99729387517955104, -59.99999999999265299, 200.5325947112515337 ) ) ;
#14928 = DIRECTION ( 'NONE',  ( 0.000000000000000000, -1.000000000000000000, 0.000000000000000000 ) ) ;
#14929 = CARTESIAN_POINT ( 'NONE',  ( 86.19853216617802616, -60.00000000000000000, 200.6758986416989785 ) ) ;
#14930 = CARTESIAN_POINT ( 'NONE',  ( 44.08840282922849241, 485.7747746244180007, 4.178803824087734320 ) ) ;
#14931 = DIRECTION ( 'NONE',  ( 0.000000000000000000, -1.000000000000000000, 0.000000000000000000 ) ) ;
#14933 = CARTESIAN_POINT ( 'NONE',  ( 9.314459442565317104, -49.91580766175264472, 32.21235667255560031 ) ) ;
#14932 = CARTESIAN_POINT ( 'NONE',  ( -114.2389886898993581, -60.00000000000000000, 181.3578213617837491 ) ) ;
#14934 = CARTESIAN_POINT ( 'NONE',  ( 102.0814292656478983, -38.00000000000000000, 157.7111269564730094 ) ) ;
#14935 = CARTESIAN_POINT ( 'NONE',  ( 5.708216051535447754E-15, 25.16329480281783759, 46.61112130868859538 ) ) ;
#14936 = CARTESIAN_POINT ( 'NONE',  ( -45.31002847039886916, -22.24445591861224258, 39.34227033862079992 ) ) ;
#14937 = EDGE_CURVE ( 'NONE', #105449, #85237, #21855, .T. ) ;
#14938 = CARTESIAN_POINT ( 'NONE',  ( -0.3343981592458916130, 35.06559523944065404, -27.29262800599611438 ) ) ;
#14939 = VERTEX_POINT ( 'NONE', #25840 ) ;
#14940 = CARTESIAN_POINT ( 'NONE',  ( -43.81051912592810282, 434.3294622498371496, 12.62549197245937549 ) ) ;
#14941 = CYLINDRICAL_SURFACE ( 'NONE', #71575, 8.000000000000000000 ) ;
#14942 = CARTESIAN_POINT ( 'NONE',  ( 11.90234461615518491, 304.5915712872084669, -9.055312070383802592 ) ) ;
#14943 = CARTESIAN_POINT ( 'NONE',  ( 35.11650669486618170, 1.474610560812782335E-15, 0.000000000000000000 ) ) ;
#14945 = ORIENTED_EDGE ( 'NONE', *, *, #34956, .T. ) ;
#14944 = CONICAL_SURFACE ( 'NONE', #32223, 3.400000000000000355, 0.9599310885968748153 ) ;
#14946 = CARTESIAN_POINT ( 'NONE',  ( 4.348929473936380852, -48.21591736632261416, 103.6864098602935655 ) ) ;
#14947 = VERTEX_POINT ( 'NONE', #98599 ) ;
#14948 = CARTESIAN_POINT ( 'NONE',  ( 84.40333236755373036, -29.99999999999844746, 196.7259491443398929 ) ) ;
#14949 = DIRECTION ( 'NONE',  ( -1.000000000000000000, -1.224606353822377258E-16, -0.000000000000000000 ) ) ;
#14950 = CARTESIAN_POINT ( 'NONE',  ( 5.916007316295453400, 41.94280310092248243, -59.21688529221268738 ) ) ;
#14951 = COLOUR_RGB ( '', 0.31764706, 0.68627451, 0.89019608) ;
#14952 = FACE_OUTER_BOUND ( 'NONE', #46392, .T. ) ;
#14953 = CARTESIAN_POINT ( 'NONE',  ( 94.31238871030012660, -30.00000000000000711, 113.8407967138806924 ) ) ;
#14954 = DIRECTION ( 'NONE',  ( -1.000000000000000000, -1.224606353822377258E-16, -0.000000000000000000 ) ) ;
#14955 = ADVANCED_FACE ( 'NONE', ( #24748 ), #82429, .T. ) ;
#14956 = ORIENTED_EDGE ( 'NONE', *, *, #80253, .F. ) ;
#14957 = ORIENTED_EDGE ( 'NONE', *, *, #66370, .T. ) ;
#14958 = EDGE_LOOP ( 'NONE', ( #76945, #15199, #11476, #71700 ) ) ;
#14959 = CARTESIAN_POINT ( 'NONE',  ( -33.00496812084323750, 465.6658704666174913, 15.15901827095430576 ) ) ;
#14960 = CARTESIAN_POINT ( 'NONE',  ( -5.140510257140494588, -10.64770037776033185, -10.57912409963173772 ) ) ;
#14961 = CARTESIAN_POINT ( 'NONE',  ( -37.54559764570092995, 464.1143081516180473, 19.43664670202776179 ) ) ;
#14962 = ORIENTED_EDGE ( 'NONE', *, *, #97659, .T. ) ;
#14963 = CARTESIAN_POINT ( 'NONE',  ( 74.07777777777778283, -3.309500000000000774, 4.475777889183797681E-16 ) ) ;
#14964 = VERTEX_POINT ( 'NONE', #49519 ) ;
#14965 = CARTESIAN_POINT ( 'NONE',  ( 4.250000000000000000, 0.000000000000000000, -9.078441367943003826 ) ) ;
#14966 = CARTESIAN_POINT ( 'NONE',  ( 85.15627926326807540, -38.69159677318751989, 198.5762613391925413 ) ) ;
#14967 = CARTESIAN_POINT ( 'NONE',  ( 13.03375404248404834, 6.122153719266105298, 7.298667805333264980 ) ) ;
#14968 = CARTESIAN_POINT ( 'NONE',  ( 85.73051029312144067, -52.75124695241775896, -8.197939295095531875 ) ) ;
#14969 = CARTESIAN_POINT ( 'NONE',  ( 83.15040716801659926, -38.00000000000005684, 168.9672039349142949 ) ) ;
#14970 = CARTESIAN_POINT ( 'NONE',  ( 31.53898829120952030, 327.6230605552352699, 16.00730009383292440 ) ) ;
#14971 = DIRECTION ( 'NONE',  ( -1.000000000000000000, -0.000000000000000000, -0.000000000000000000 ) ) ;
#14972 = CIRCLE ( 'NONE', #99416, 4.000000000000001776 ) ;
#14973 = CARTESIAN_POINT ( 'NONE',  ( 27.99999999999999645, 1.836970198721029589E-15, -15.00000000000000000 ) ) ;
#14974 = AXIS2_PLACEMENT_3D ( 'NONE', #73477, #90213, #23381 ) ;
#14975 =( NAMED_UNIT ( * ) PLANE_ANGLE_UNIT ( ) SI_UNIT ( $, .RADIAN. ) );
#14976 = CARTESIAN_POINT ( 'NONE',  ( 41.21073348271418979, 328.7814315827667428, 10.19983387948521170 ) ) ;
#14977 = EDGE_LOOP ( 'NONE', ( #52526, #36663, #9323, #96752, #105690 ) ) ;
#14978 = ADVANCED_FACE ( 'NONE', ( #88673 ), #26995, .T. ) ;
#14979 = CARTESIAN_POINT ( 'NONE',  ( -37.55700377048162153, 460.8426286395056195, 2.817645980328392863 ) ) ;
#14980 =( NAMED_UNIT ( * ) SI_UNIT ( $, .STERADIAN. ) SOLID_ANGLE_UNIT ( ) );
#14981 = ORIENTED_EDGE ( 'NONE', *, *, #26774, .T. ) ;
#14982 = CARTESIAN_POINT ( 'NONE',  ( 0.5805565836007650082, -3.752776749732574135, -6.500000000000001776 ) ) ;
#14984 = CARTESIAN_POINT ( 'NONE',  ( -31.08895332998342198, 299.3338306225929273, 10.94102856163953952 ) ) ;
#14983 = CARTESIAN_POINT ( 'NONE',  ( 0.000000000000000000, 0.000000000000000000, 0.000000000000000000 ) ) ;
#14985 = DIRECTION ( 'NONE',  ( -1.000000000000000000, -1.224606353822377258E-16, -0.000000000000000000 ) ) ;
#14986 = UNCERTAINTY_MEASURE_WITH_UNIT (LENGTH_MEASURE( 1.000000000000000082E-05 ), #40075, 'distance_accuracy_value', 'NONE');
#14987 = SURFACE_SIDE_STYLE ('',( #8495 ) ) ;
#14988 = CARTESIAN_POINT ( 'NONE',  ( -3.313708498984765161, -14.46874999999999289, 7.999999999999998224 ) ) ;
#14989 = MECHANICAL_DESIGN_GEOMETRIC_PRESENTATION_REPRESENTATION (  '', ( #8127 ), #35754 ) ;
#14991 = CARTESIAN_POINT ( 'NONE',  ( -1.943011881543717845, -18.06865899137350340, 35.01031080251575389 ) ) ;
#14990 = CONICAL_SURFACE ( 'NONE', #64964, 3.309500000000001663, 0.9599310885968770357 ) ;
#14992 = EDGE_CURVE ( 'NONE', #31239, #2579, #63150, .T. ) ;
#14993 = CIRCLE ( 'NONE', #66750, 4.999999999999999112 ) ;
#14994 = COLOUR_RGB ( '', 0.66274510, 0.83137255, 0.94901961) ;
#14995 = VECTOR ( 'NONE', #73285, 1000.000000000000000 ) ;
#14996 = VERTEX_POINT ( 'NONE', #46616 ) ;
#14997 = CARTESIAN_POINT ( 'NONE',  ( 86.40712283630125512, -17.65985353466466279, 176.8060135199089018 ) ) ;
#14998 = CARTESIAN_POINT ( 'NONE',  ( 0.000000000000000000, 67.05096163904791240, -10.02537308446410691 ) ) ;
#14999 = SURFACE_SIDE_STYLE ('',( #96994 ) ) ;
#15000 = EDGE_LOOP ( 'NONE', ( #68305, #69639, #88597, #72238 ) ) ;
#15001 = CARTESIAN_POINT ( 'NONE',  ( 93.83458408931859651, -57.67449834134204423, 11.79857076260040216 ) ) ;
#15002 = EDGE_CURVE ( 'NONE', #717, #71103, #16629, .T. ) ;
#15003 = CARTESIAN_POINT ( 'NONE',  ( 36.22735294587279498, 437.9860357368701784, 4.211724321154513007 ) ) ;
#15004 = CARTESIAN_POINT ( 'NONE',  ( -7.000000000000000000, 8.572527594031473190E-16, -0.7256075382097185722 ) ) ;
#15005 = MECHANICAL_DESIGN_GEOMETRIC_PRESENTATION_REPRESENTATION (  '', ( #30525 ), #71820 ) ;
#15006 = CARTESIAN_POINT ( 'NONE',  ( -84.35947751489756286, -37.99999999999994316, 179.2493818773862131 ) ) ;
#15007 = CARTESIAN_POINT ( 'NONE',  ( 8.922269033010996608, -5.000000000000000000, -5.219866590717683330 ) ) ;
#15008 = DIRECTION ( 'NONE',  ( 0.000000000000000000, -1.000000000000000000, 0.000000000000000000 ) ) ;
#15010 = CARTESIAN_POINT ( 'NONE',  ( -10.36378764587132117, 10.91134418945301832, 10.43617239968854982 ) ) ;
#15009 = CARTESIAN_POINT ( 'NONE',  ( 12.61650669486618881, 4.898587196589413815E-16, -4.000000000000000888 ) ) ;
#15011 = VERTEX_POINT ( 'NONE', #63354 ) ;
#15012 = CIRCLE ( 'NONE', #101189, 4.172000000000001485 ) ;
#15013 = CARTESIAN_POINT ( 'NONE',  ( 9.609724578338589396, 294.6537309100400535, -2.768030809509012258 ) ) ;
#15014 = CARTESIAN_POINT ( 'NONE',  ( -12.49999999999999822, -4.999999999999999112, -8.595933841506989026 ) ) ;
#15015 = CARTESIAN_POINT ( 'NONE',  ( 9.609938133566929608, -5.000000000000000000, -92.36043836069937640 ) ) ;
#15016 = CARTESIAN_POINT ( 'NONE',  ( -3.976861647037802427, -22.09778810902588830, -30.53710112390729137 ) ) ;
#15017 = CARTESIAN_POINT ( 'NONE',  ( 45.11650669486618881, -3.999999999999998224, 0.000000000000000000 ) ) ;
#15018 = CARTESIAN_POINT ( 'NONE',  ( -82.24209943865865569, -37.99999999999997158, -13.36826342095787368 ) ) ;
#15019 = AXIS2_PLACEMENT_3D ( 'NONE', #87920, #14527, #29713 ) ;
#15020 = ORIENTED_EDGE ( 'NONE', *, *, #8758, .T. ) ;
#15021 = CARTESIAN_POINT ( 'NONE',  ( 13.58349330513380515, 4.000000000000003553, 0.000000000000000000 ) ) ;
#15022 = DIRECTION ( 'NONE',  ( -0.000000000000000000, 1.000000000000000000, -0.000000000000000000 ) ) ;
#15023 = COLOUR_RGB ( '', 0.08235294, 0.09019608, 0.10196078) ;
#15024 = CARTESIAN_POINT ( 'NONE',  ( 5.858881034796412202, -61.21413675997018800, 1.317748741875967022 ) ) ;
#15026 = CARTESIAN_POINT ( 'NONE',  ( -59.18075469557353330, -34.58949886300455745, -25.51696680825630992 ) ) ;
#15025 = CARTESIAN_POINT ( 'NONE',  ( 1.102182119232618897E-15, -20.00000000000001776, 9.000000000000007105 ) ) ;
#15027 = EDGE_CURVE ( 'NONE', #87378, #14445, #94182, .T. ) ;
#15028 = VERTEX_POINT ( 'NONE', #14763 ) ;
#15029 = VERTEX_POINT ( 'NONE', #21846 ) ;
#15030 = EDGE_CURVE ( 'NONE', #84815, #10145, #47646, .T. ) ;
#15031 = ADVANCED_FACE ( 'NONE', ( #70372 ), #76923, .T. ) ;
#15032 = CIRCLE ( 'NONE', #40912, 4.000000000000001776 ) ;
#15033 = CARTESIAN_POINT ( 'NONE',  ( 10.45208520439346422, 43.95501981190459162, -12.90779740156171584 ) ) ;
#15034 = CARTESIAN_POINT ( 'NONE',  ( 30.00000000000000000, 1.102182119232617714E-15, -9.000000000000000000 ) ) ;
#15035 = CARTESIAN_POINT ( 'NONE',  ( -92.70286745887267443, -59.99999999999997868, -4.853674443702933772 ) ) ;
#15036 = ORIENTED_EDGE ( 'NONE', *, *, #105196, .F. ) ;
#15037 = CARTESIAN_POINT ( 'NONE',  ( -7.232205791931226813, 41.33266196707086237, -58.20097105120220249 ) ) ;
#15038 = DIRECTION ( 'NONE',  ( 0.000000000000000000, 0.000000000000000000, 1.000000000000000000 ) ) ;
#15039 = CARTESIAN_POINT ( 'NONE',  ( 95.20707830180857911, -45.27064899011855914, 194.1781096548304788 ) ) ;
#15041 = CARTESIAN_POINT ( 'NONE',  ( 36.84999999999999432, 1.533819458162526451E-15, 0.000000000000000000 ) ) ;
#15040 = DIRECTION ( 'NONE',  ( 0.000000000000000000, 0.000000000000000000, -1.000000000000000000 ) ) ;
#15042 = EDGE_CURVE ( 'NONE', #71251, #69309, #26827, .T. ) ;
#15043 = CARTESIAN_POINT ( 'NONE',  ( -83.48750810316161619, -32.53526638036854024, 163.2801944554805118 ) ) ;
#15044 =( GEOMETRIC_REPRESENTATION_CONTEXT ( 3 ) GLOBAL_UNCERTAINTY_ASSIGNED_CONTEXT ( ( #106590 ) ) GLOBAL_UNIT_ASSIGNED_CONTEXT ( ( #18472, #100954, #43784 ) ) REPRESENTATION_CONTEXT ( 'NONE', 'WORKASPACE' ) );
#15045 = VERTEX_POINT ( 'NONE', #96254 ) ;
#15046 = ORIENTED_EDGE ( 'NONE', *, *, #45609, .F. ) ;
#15047 = VERTEX_POINT ( 'NONE', #103266 ) ;
#15048 = DIRECTION ( 'NONE',  ( 0.000000000000000000, -1.000000000000000000, 0.000000000000000000 ) ) ;
#15049 = CARTESIAN_POINT ( 'NONE',  ( -6.038222094116281191, -12.57840291894124363, 12.65816746961276706 ) ) ;
#15050 = PRESENTATION_STYLE_ASSIGNMENT (( #23712 ) ) ;
#15051 = ORIENTED_EDGE ( 'NONE', *, *, #3327, .F. ) ;
#15052 = ADVANCED_FACE ( 'NONE', ( #62815 ), #103786, .F. ) ;
#15053 = FILL_AREA_STYLE ('',( #38826 ) ) ;
#15054 = CARTESIAN_POINT ( 'NONE',  ( 6.500000000000000000, -2.501851166488394451, -5.848636054922037530 ) ) ;
#15055 = CARTESIAN_POINT ( 'NONE',  ( -10.00000000000004086, 14.99999999999998934, -4.210530276627957313 ) ) ;
#15056 = CARTESIAN_POINT ( 'NONE',  ( -78.78539465073522763, -57.50642106797575082, 197.5849804933186817 ) ) ;
#15057 = CARTESIAN_POINT ( 'NONE',  ( 1.450851314122095559, -49.97609955501174284, 101.4859915538870609 ) ) ;
#15058 = CARTESIAN_POINT ( 'NONE',  ( 4.555094537983155334, 5.243183837310242623, -6.208110906918259175 ) ) ;
#15059 = AXIS2_PLACEMENT_3D ( 'NONE', #92522, #75269, #17596 ) ;
#15060 = DIRECTION ( 'NONE',  ( -1.000000000000000000, -0.000000000000000000, -0.000000000000000000 ) ) ;
#15061 = VECTOR ( 'NONE', #50083, 1000.000000000000000 ) ;
#15062 = CARTESIAN_POINT ( 'NONE',  ( 1.404490565847964501, 15.46725112412266334, -9.926810856659662008 ) ) ;
#15063 = CARTESIAN_POINT ( 'NONE',  ( -33.15890210479862787, -30.00000000000000711, -37.92163678030271967 ) ) ;
#15064 = EDGE_CURVE ( 'NONE', #90250, #78219, #87245, .T. ) ;
#15065 = CARTESIAN_POINT ( 'NONE',  ( -1.385021579957316007, -30.00000000000000000, 37.00000000000000711 ) ) ;
#15066 = CARTESIAN_POINT ( 'NONE',  ( -53.79344265758010124, -29.09963908877845284, 53.78559824726266925 ) ) ;
#15067 = CARTESIAN_POINT ( 'NONE',  ( 29.66054107240687543, -5.000000000000000000, 6.123233995736768255E-16 ) ) ;
#15068 = PRESENTATION_LAYER_ASSIGNMENT (  '', '', ( #75106 ) ) ;
#15070 = ORIENTED_EDGE ( 'NONE', *, *, #90174, .T. ) ;
#15069 = MECHANICAL_DESIGN_GEOMETRIC_PRESENTATION_REPRESENTATION (  '', ( #61615 ), #42633 ) ;
#15071 = STYLED_ITEM ( 'NONE', ( #51245 ), #3886 ) ;
#15072 = CARTESIAN_POINT ( 'NONE',  ( -97.79127707065502761, -52.80354280853628524, 195.1513629227311242 ) ) ;
#15073 = PRESENTATION_LAYER_ASSIGNMENT (  '', '', ( #47782 ) ) ;
#15074 = DIRECTION ( 'NONE',  ( 0.000000000000000000, 0.000000000000000000, 1.000000000000000000 ) ) ;
#15075 = ORIENTED_EDGE ( 'NONE', *, *, #75200, .F. ) ;
#15076 = CARTESIAN_POINT ( 'NONE',  ( 19.40536060365760207, 49.94405995648938301, 60.94144269849599738 ) ) ;
#15077 = CARTESIAN_POINT ( 'NONE',  ( 106.7250614457355198, -38.36694503808185175, 195.3045705398520511 ) ) ;
#15078 = CARTESIAN_POINT ( 'NONE',  ( -80.00000000000000000, -52.00000000000000000, -19.09707704303353282 ) ) ;
#15079 = CARTESIAN_POINT ( 'NONE',  ( 6.815830331203685866, 0.6619522098568458857, -6.171384342982615401 ) ) ;
#15080 = DIRECTION ( 'NONE',  ( -1.000000000000000000, 0.000000000000000000, 0.000000000000000000 ) ) ;
#15081 = CARTESIAN_POINT ( 'NONE',  ( 80.77650999055178715, -30.00000000000000711, 138.7427449783301370 ) ) ;
#15082 = CONICAL_SURFACE ( 'NONE', #87408, 3.309500000000001663, 0.9599310885968770357 ) ;
#15083 = CARTESIAN_POINT ( 'NONE',  ( 0.4042117618284674085, -3.141900367810040784, 6.500000000000000000 ) ) ;
#15084 = CARTESIAN_POINT ( 'NONE',  ( 36.13333162057519843, 491.8038228668837064, 12.56276695384558550 ) ) ;
#15085 = CARTESIAN_POINT ( 'NONE',  ( -1.126885523087953089, 34.38870459337674390, 29.13346846296686721 ) ) ;
#15086 = CARTESIAN_POINT ( 'NONE',  ( 0.000000000000000000, 0.000000000000000000, -0.4621369752184079083 ) ) ;
#15087 = AXIS2_PLACEMENT_3D ( 'NONE', #44900, #53507, #86432 ) ;
#15088 = ORIENTED_EDGE ( 'NONE', *, *, #285, .F. ) ;
#15089 = ORIENTED_EDGE ( 'NONE', *, *, #66692, .F. ) ;
#15090 = CARTESIAN_POINT ( 'NONE',  ( 49.54155134396112459, -25.66740930363953410, 45.52487917608116419 ) ) ;
#15091 = DIRECTION ( 'NONE',  ( -0.5735764363510497121, 0.8191520442889892450, 1.003171929053521665E-16 ) ) ;
#15092 = DIRECTION ( 'NONE',  ( -1.000000000000000000, -1.224606353822377258E-16, -0.000000000000000000 ) ) ;
#15093 = CARTESIAN_POINT ( 'NONE',  ( -107.4879495132023095, -38.36268515545186375, 194.0533311958894842 ) ) ;
#15094 = AXIS2_PLACEMENT_3D ( 'NONE', #48101, #47046, #23882 ) ;
#15095 = ORIENTED_EDGE ( 'NONE', *, *, #55747, .F. ) ;
#15096 = CARTESIAN_POINT ( 'NONE',  ( 110.2348944668668622, -38.35604625147674085, 157.2622168874477779 ) ) ;
#15097 = CARTESIAN_POINT ( 'NONE',  ( 10.36233036400907004, 16.98659626113961352, -9.892282517339653580 ) ) ;
#15098 = CARTESIAN_POINT ( 'NONE',  ( -6.645598051714149967, 41.91296950070219651, -68.91429205809731684 ) ) ;
#15099 = CARTESIAN_POINT ( 'NONE',  ( 0.000000000000000000, 0.000000000000000000, -8.125150395352576993 ) ) ;
#15100 = CARTESIAN_POINT ( 'NONE',  ( 93.99242027173671943, -37.84847618451019002, 101.9190371959758181 ) ) ;
#15101 =( NAMED_UNIT ( * ) PLANE_ANGLE_UNIT ( ) SI_UNIT ( $, .RADIAN. ) );
#15102 = SURFACE_STYLE_USAGE ( .BOTH. , #96572 ) ;
#15103 = CARTESIAN_POINT ( 'NONE',  ( -36.01958551496955607, 344.3887468264661607, -0.3208639796993665860 ) ) ;
#15104 = CARTESIAN_POINT ( 'NONE',  ( 0.000000000000000000, -1.200000000000000030E-05, 17.50000000000000000 ) ) ;
#15105 = CARTESIAN_POINT ( 'NONE',  ( 10.50000000000000711, -5.000000000000000000, -80.60844091781802945 ) ) ;
#15106 = CARTESIAN_POINT ( 'NONE',  ( 88.01504803064270277, -59.99999999999999289, 201.3865903595551572 ) ) ;
#15107 = AXIS2_PLACEMENT_3D ( 'NONE', #92250, #49674, #51260 ) ;
#15108 = CARTESIAN_POINT ( 'NONE',  ( -16.75187969033532553, 34.25544727262118982, 24.30698433968612449 ) ) ;
#15109 = ORIENTED_EDGE ( 'NONE', *, *, #11356, .T. ) ;
#15110 = CARTESIAN_POINT ( 'NONE',  ( 58.58608388584831062, -32.54594335739298572, 65.51434834299064391 ) ) ;
#15111 = CARTESIAN_POINT ( 'NONE',  ( -27.46538772309321530, 305.3421805592328724, -9.449778543000565634 ) ) ;
#15112 = CARTESIAN_POINT ( 'NONE',  ( 6.928203230275506996, 30.26883324508997575, -3.999999999999999112 ) ) ;
#15113 = EDGE_CURVE ( 'NONE', #45889, #3051, #79513, .T. ) ;
#15114 = CARTESIAN_POINT ( 'NONE',  ( -7.150931910075644105, 28.21374201477736676, -3.588457848165353958 ) ) ;
#15115 = ORIENTED_EDGE ( 'NONE', *, *, #86694, .F. ) ;
#15117 = CARTESIAN_POINT ( 'NONE',  ( -14.87367913736586900, 23.06835470864390558, 1.002906751349593506 ) ) ;
#15116 = CARTESIAN_POINT ( 'NONE',  ( -93.90547544503390043, -38.35568117715248349, 50.59712527411566896 ) ) ;
#15118 = AXIS2_PLACEMENT_3D ( 'NONE', #14615, #105246, #80417 ) ;
#15119 = DIRECTION ( 'NONE',  ( -0.9915366780650390899, -0.1269898409407501094, -0.02699252395739001886 ) ) ;
#15120 = CARTESIAN_POINT ( 'NONE',  ( 31.39951845036370059, 423.6537597265949557, 23.88519890770611553 ) ) ;
#15121 = CARTESIAN_POINT ( 'NONE',  ( 42.40769230769231513, 4.172000000000003261, 0.000000000000000000 ) ) ;
#15122 = CARTESIAN_POINT ( 'NONE',  ( -7.188101187500002709, -9.687500002048384573, 2.977408999572648707 ) ) ;
#15123 = CARTESIAN_POINT ( 'NONE',  ( -17.49999999999996803, 44.85000000000000853, 64.09953197957064219 ) ) ;
#15124 = EDGE_CURVE ( 'NONE', #55161, #63565, #45572, .T. ) ;
#15125 = CIRCLE ( 'NONE', #23788, 5.000000000000001776 ) ;
#15126 = EDGE_CURVE ( 'NONE', #96664, #67017, #47664, .T. ) ;
#15127 = CARTESIAN_POINT ( 'NONE',  ( -33.85195725564127400, 465.2464970902067307, 17.18122764674263436 ) ) ;
#15128 = VERTEX_POINT ( 'NONE', #31000 ) ;
#15129 = CARTESIAN_POINT ( 'NONE',  ( 80.94188275191889659, -60.49855713378364186, 182.8649140336319761 ) ) ;
#15130 = CARTESIAN_POINT ( 'NONE',  ( 40.02592568779148507, 6.123233995736772199E-16, -5.000000000000001776 ) ) ;
#15131 = CIRCLE ( 'NONE', #68505, 4.000000000000001776 ) ;
#15132 = CARTESIAN_POINT ( 'NONE',  ( -33.12944332324994434, 439.4248878830263152, 23.85028906779292868 ) ) ;
#15133 = EDGE_LOOP ( 'NONE', ( #78593, #47327, #32942, #68063 ) ) ;
#15134 = CARTESIAN_POINT ( 'NONE',  ( 6.463647488011505793, -2.646730816809989228, 6.840026438643557860 ) ) ;
#15135 = EDGE_CURVE ( 'NONE', #79036, #54576, #21830, .T. ) ;
#15136 = CARTESIAN_POINT ( 'NONE',  ( 7.499994653025345848, -2.925861026135234244, -20.99866594783414797 ) ) ;
#15137 = CARTESIAN_POINT ( 'NONE',  ( 26.78714902951895382, 34.58969031657304072, -10.02637816120943270 ) ) ;
#15138 = CARTESIAN_POINT ( 'NONE',  ( 14.24890542153238471, 2.189729425896414838, -4.659254829976903878 ) ) ;
#15139 = DIRECTION ( 'NONE',  ( -0.000000000000000000, -1.000000000000000000, -0.000000000000000000 ) ) ;
#15140 = CARTESIAN_POINT ( 'NONE',  ( -28.72976249129343884, 13.62251309882729267, -40.04442010369706395 ) ) ;
#15141 = ORIENTED_EDGE ( 'NONE', *, *, #9492, .F. ) ;
#15142 = AXIS2_PLACEMENT_3D ( 'NONE', #100753, #102357, #44135 ) ;
#15143 = VECTOR ( 'NONE', #71174, 1000.000000000000000 ) ;
#15144 = VECTOR ( 'NONE', #28614, 1000.000000000000000 ) ;
#15145 = CARTESIAN_POINT ( 'NONE',  ( 6.818262094731102785, 1.323628772216710603, -6.207787212118526909 ) ) ;
#15146 = CARTESIAN_POINT ( 'NONE',  ( 0.6414297221551786832, 26.01290138943593888, 38.42394282347074608 ) ) ;
#15148 = CARTESIAN_POINT ( 'NONE',  ( -11.66708038261545965, 8.918174348190984091, -9.153312531148994680 ) ) ;
#15147 = CARTESIAN_POINT ( 'NONE',  ( 34.85398709568261921, 481.6347222374536727, 14.59797584736199205 ) ) ;
#15149 = CARTESIAN_POINT ( 'NONE',  ( 2.977408999572651815, -17.93750000204838457, 7.188101187500000933 ) ) ;
#15150 = CARTESIAN_POINT ( 'NONE',  ( -28.46814188645407739, 18.16755603797500029, -40.55128649371884109 ) ) ;
#15151 = CIRCLE ( 'NONE', #66825, 4.000000000000007105 ) ;
#15152 = CYLINDRICAL_SURFACE ( 'NONE', #6969, 1.250000000000001110 ) ;
#15153 = ORIENTED_EDGE ( 'NONE', *, *, #97685, .T. ) ;
#15154 = CARTESIAN_POINT ( 'NONE',  ( 23.76770941297787587, 25.83109853082994789, 30.83089620004140130 ) ) ;
#15155 = CARTESIAN_POINT ( 'NONE',  ( -3.342518420180325300, 120.5426393934660609, -4.999999999999999112 ) ) ;
#15156 = DIRECTION ( 'NONE',  ( 1.000000000000000000, -0.000000000000000000, -0.000000000000000000 ) ) ;
#15157 = CARTESIAN_POINT ( 'NONE',  ( -14.24976063294461781, 2.188309765144745178, 4.656908667384352718 ) ) ;
#15158 = EDGE_CURVE ( 'NONE', #75560, #51764, #49343, .T. ) ;
#15159 = VERTEX_POINT ( 'NONE', #13169 ) ;
#15160 = AXIS2_PLACEMENT_3D ( 'NONE', #82957, #25838, #68383 ) ;
#15161 = FACE_OUTER_BOUND ( 'NONE', #78617, .T. ) ;
#15162 = DIRECTION ( 'NONE',  ( -1.000000000000000000, -1.224606353822377258E-16, -0.000000000000000000 ) ) ;
#15163 = ORIENTED_EDGE ( 'NONE', *, *, #67207, .T. ) ;
#15164 = EDGE_CURVE ( 'NONE', #16434, #73038, #90707, .T. ) ;
#15165 = PLANE ( 'NONE',  #26608 ) ;
#15166 = CARTESIAN_POINT ( 'NONE',  ( -17.49999999999999645, -2.499999999999999556, 25.00000000000000000 ) ) ;
#15167 = CARTESIAN_POINT ( 'NONE',  ( 16.13647630347072948, 6.334953579828321857, -5.738861489052264453 ) ) ;
#15168 = CARTESIAN_POINT ( 'NONE',  ( -106.4896240607370572, -60.00000000000000000, 119.4492507493957305 ) ) ;
#15169 = CARTESIAN_POINT ( 'NONE',  ( 28.71513376685288321, 15.67191133428134542, -41.65496614056306868 ) ) ;
#15170 = LINE ( 'NONE', #64790, #22986 ) ;
#15171 = DIRECTION ( 'NONE',  ( -0.1269898409407502204, -0.9919025243773941236, 0.001721171576547747550 ) ) ;
#15172 = DIRECTION ( 'NONE',  ( 0.000000000000000000, -1.000000000000000000, 0.000000000000000000 ) ) ;
#15174 = CARTESIAN_POINT ( 'NONE',  ( 6.575925811255156184, 3.850887307289501571, 6.669932470447524686 ) ) ;
#15173 = CARTESIAN_POINT ( 'NONE',  ( 9.739726766102963396, -5.000000000000000888, -82.38252115499879835 ) ) ;
#15175 = CIRCLE ( 'NONE', #75468, 4.000000000000001776 ) ;
#15176 = CARTESIAN_POINT ( 'NONE',  ( -85.66159904005490944, -21.90579002698637723, 168.1005346913126743 ) ) ;
#15177 = ORIENTED_EDGE ( 'NONE', *, *, #1284, .F. ) ;
#15178 = DIRECTION ( 'NONE',  ( 0.000000000000000000, 1.000000000000000000, -0.000000000000000000 ) ) ;
#15179 = ORIENTED_EDGE ( 'NONE', *, *, #38730, .F. ) ;
#15180 = CARTESIAN_POINT ( 'NONE',  ( 43.02621584241283870, 434.6128289108255558, 16.97888786058996402 ) ) ;
#15181 = B_SPLINE_CURVE_WITH_KNOTS ( 'NONE', 3,
 ( #85669, #77567, #36614, #102364 ),
 .UNSPECIFIED., .F., .F.,
 ( 4, 4 ),
 ( 0.000000000000000000, 1.000000000000000000 ),
 .UNSPECIFIED. ) ;
#15182 = CARTESIAN_POINT ( 'NONE',  ( 14.83349330513380693, 1.593028355512270962E-15, 0.000000000000000000 ) ) ;
#15183 = CARTESIAN_POINT ( 'NONE',  ( 8.167412539202029365, 39.27912669871973605, -5.000000000000000888 ) ) ;
#15184 = CARTESIAN_POINT ( 'NONE',  ( -12.60465631124217900, -5.000000000000000000, -81.60874940243330400 ) ) ;
#15185 = CARTESIAN_POINT ( 'NONE',  ( -43.97702309830648915, 485.9235625653078046, 4.765750180334560326 ) ) ;
#15186 = AXIS2_PLACEMENT_3D ( 'NONE', #15771, #81024, #7141 ) ;
#15187 = CARTESIAN_POINT ( 'NONE',  ( 114.5718218735923131, -60.00000000000004974, 174.9501719601325078 ) ) ;
#15188 = CARTESIAN_POINT ( 'NONE',  ( -99.89444227931625164, -30.00000000000003197, 96.08249125629401988 ) ) ;
#15189 = CARTESIAN_POINT ( 'NONE',  ( -62.17707188868673285, -36.01208718166724765, 76.36316336690838114 ) ) ;
#15190 = VERTEX_POINT ( 'NONE', #22902 ) ;
#15191 = CARTESIAN_POINT ( 'NONE',  ( -30.78465349003366214, 38.95360288174918395, 55.80746841105920453 ) ) ;
#15192 = CARTESIAN_POINT ( 'NONE',  ( 94.51406953657293286, -59.99999999999998579, 3.554358192505464586 ) ) ;
#15193 = EDGE_LOOP ( 'NONE', ( #60769, #36893, #36137 ) ) ;
#15194 = CARTESIAN_POINT ( 'NONE',  ( 13.69909788704105935, -56.64682055396593796, 24.10694589033532154 ) ) ;
#15195 = CARTESIAN_POINT ( 'NONE',  ( 7.188101187500000933, -13.43750000204838457, -2.977408999572650483 ) ) ;
#15196 = AXIS2_PLACEMENT_3D ( 'NONE', #47545, #63759, #96121 ) ;
#15197 = EDGE_CURVE ( 'NONE', #89220, #74466, #55739, .T. ) ;
#15198 = SURFACE_STYLE_USAGE ( .BOTH. , #14651 ) ;
#15199 = ORIENTED_EDGE ( 'NONE', *, *, #66432, .F. ) ;
#15201 = CARTESIAN_POINT ( 'NONE',  ( 7.203362828890048419, -30.00000000000004263, -0.01858974796685433292 ) ) ;
#15200 = MECHANICAL_DESIGN_GEOMETRIC_PRESENTATION_REPRESENTATION (  '', ( #103078 ), #56533 ) ;
#15202 = ORIENTED_EDGE ( 'NONE', *, *, #70416, .T. ) ;
#15203 = CARTESIAN_POINT ( 'NONE',  ( -7.500000000000000888, 0.000000000000000000, 0.000000000000000000 ) ) ;
#15204 = CARTESIAN_POINT ( 'NONE',  ( 0.000000000000000000, 0.000000000000000000, 4.000000000000000000 ) ) ;
#15205 = CARTESIAN_POINT ( 'NONE',  ( -110.3478029491143104, -60.00000000000001421, 189.9910190477876597 ) ) ;
#15206 = CARTESIAN_POINT ( 'NONE',  ( -3.685905252136130184, -1.041089327947677834, 104.2837900504744510 ) ) ;
#15207 = CARTESIAN_POINT ( 'NONE',  ( 4.401442555609581635E-16, -29.65625000204838813, -7.188101187500000044 ) ) ;
#15208 = CARTESIAN_POINT ( 'NONE',  ( 37.24486667819500241, 485.5941914037273932, -4.198424488985136982 ) ) ;
#15209 =( BOUNDED_SURFACE ( )  B_SPLINE_SURFACE ( 3, 2, ( 
 ( #45186, #14363, #80170 ),
 ( #5760, #62424, #104451 ),
 ( #96388, #87227, #71029 ),
 ( #46233, #21449, #87759 ),
 ( #53263, #13310, #78061 ),
 ( #46754, #29040, #30068 ) ),
 .UNSPECIFIED., .F., .F., .F. ) 
 B_SPLINE_SURFACE_WITH_KNOTS ( ( 4, 2, 4 ),
 ( 3, 3 ),
 ( -8.868773770931426270E-17, 0.001801542390204190734, 0.003603084780408470373 ),
 ( 0.000000000000000000, 1.000000000000000000 ),
 .UNSPECIFIED. ) 
 GEOMETRIC_REPRESENTATION_ITEM ( )  RATIONAL_B_SPLINE_SURFACE ( (
 ( 1.000000000000000000, 0.9115707425106689410, 1.000000000000000000),
 ( 1.000000000000000000, 0.9032011672212912901, 1.000000000000000000),
 ( 1.000000000000000000, 0.8933560653589430745, 1.000000000000000000),
 ( 1.000000000000000000, 0.8671388017652420510, 1.000000000000000000),
 ( 1.000000000000000000, 0.8506934603551941088, 1.000000000000000000),
 ( 1.000000000000000000, 0.8291561975888570579, 1.000000000000000000) ) ) 
 REPRESENTATION_ITEM ( '' )  SURFACE ( )  );
#15210 = CARTESIAN_POINT ( 'NONE',  ( -11.50426943841285876, 15.12044061251818938, 9.781685010125752200 ) ) ;
#15211 = CARTESIAN_POINT ( 'NONE',  ( -15.00099999999999767, 12.99999999999999289, 0.000000000000000000 ) ) ;
#15212 = CARTESIAN_POINT ( 'NONE',  ( 0.000000000000000000, 49.50000000000000000, 0.000000000000000000 ) ) ;
#15213 = CARTESIAN_POINT ( 'NONE',  ( 14.85285428659677720, -6.992436857781551218, 13.28281651405465702 ) ) ;
#15214 = CARTESIAN_POINT ( 'NONE',  ( -43.66634721479189807, 409.2520837962942437, 16.13407036732532518 ) ) ;
#15215 = CARTESIAN_POINT ( 'NONE',  ( 100.8709588495254508, -60.00000000000001421, 195.1801793387124633 ) ) ;
#15216 = CARTESIAN_POINT ( 'NONE',  ( -31.61288136673854510, -22.14119122292571618, 30.54124083663120004 ) ) ;
#15217 = ORIENTED_EDGE ( 'NONE', *, *, #61643, .T. ) ;
#15218 = CARTESIAN_POINT ( 'NONE',  ( -36.71273542727830375, 461.9574973007366339, 3.152060736416770759 ) ) ;
#15219 = COLOUR_RGB ( '', 0.09019608, 0.27058824, 0.51372549) ;
#15220 = TOROIDAL_SURFACE ( 'NONE', #29000, 12.00000000000001066, 3.000000000000000000 ) ;
#15221 = CARTESIAN_POINT ( 'NONE',  ( 38.30783514898087816, -22.21897967646507865, 33.68727933474853842 ) ) ;
#15223 = AXIS2_PLACEMENT_3D ( 'NONE', #101690, #36470, #61791 ) ;
#15222 = CARTESIAN_POINT ( 'NONE',  ( 11.19959342721965179, -3.864748466433897305E-12, 19.43146043915186993 ) ) ;
#15224 = EDGE_LOOP ( 'NONE', ( #53625, #7811, #2194, #44009, #35035 ) ) ;
#15225 = CIRCLE ( 'NONE', #44738, 4.000000000000001776 ) ;
#15226 = DIRECTION ( 'NONE',  ( -0.000000000000000000, -1.000000000000000000, -0.000000000000000000 ) ) ;
#15227 = CARTESIAN_POINT ( 'NONE',  ( -57.42639478918781037, -38.34440198517998510, 88.53404947109167722 ) ) ;
#15228 = ORIENTED_EDGE ( 'NONE', *, *, #22492, .T. ) ;
#15230 = CARTESIAN_POINT ( 'NONE',  ( 24.37088254901632567, 295.3567874699774620, -9.892597027136796228 ) ) ;
#15229 = CARTESIAN_POINT ( 'NONE',  ( 7.409209413120518839, -5.000000000000000888, -15.54546483169703563 ) ) ;
#15231 = CARTESIAN_POINT ( 'NONE',  ( 85.59800593614014019, 6.123233995736582872E-16, -5.000000000000011546 ) ) ;
#15232 = CARTESIAN_POINT ( 'NONE',  ( 6.458251213448418682, 3.357560920637083779, 6.499999999999997335 ) ) ;
#15233 = CONICAL_SURFACE ( 'NONE', #99616, 4.000000000000007105, 0.9599310885968835860 ) ;
#15234 = CARTESIAN_POINT ( 'NONE',  ( 0.5677053942435199563, 44.03347157068819939, -16.38324328692960563 ) ) ;
#15235 = CARTESIAN_POINT ( 'NONE',  ( -38.81019369337919045, 25.23140533547475073, 11.84541638487588067 ) ) ;
#15236 = CYLINDRICAL_SURFACE ( 'NONE', #99942, 5.000000000000000888 ) ;
#15237 = DIRECTION ( 'NONE',  ( -1.000000000000000000, -0.000000000000000000, -0.000000000000000000 ) ) ;
#15238 = CARTESIAN_POINT ( 'NONE',  ( 93.20221228412790992, -60.00000000000000711, 34.27167064687595399 ) ) ;
#15239 = CARTESIAN_POINT ( 'NONE',  ( -43.46689911038884446, 485.4921130117998018, 4.095024577344805294 ) ) ;
#15240 = CYLINDRICAL_SURFACE ( 'NONE', #73095, 4.000000000000000000 ) ;
#15241 = CARTESIAN_POINT ( 'NONE',  ( 5.096247963225427391, -4.999999999999998224, -73.00359695309825270 ) ) ;
#15242 = ORIENTED_EDGE ( 'NONE', *, *, #44877, .T. ) ;
#15243 = ADVANCED_FACE ( 'NONE', ( #94666 ), #44210, .T. ) ;
#15244 = CIRCLE ( 'NONE', #6617, 0.9999999999999811262 ) ;
#15245 = CARTESIAN_POINT ( 'NONE',  ( -79.69840623192676787, -30.00000000000000711, 132.5680624720444314 ) ) ;
#15246 = ORIENTED_EDGE ( 'NONE', *, *, #78931, .T. ) ;
#15247 = CARTESIAN_POINT ( 'NONE',  ( -9.171181789971550202, -55.04814173952514977, 30.98656384792473162 ) ) ;
#15248 = CARTESIAN_POINT ( 'NONE',  ( -15.91318055706418200, 3.411564560433507420, -2.528039842340506382 ) ) ;
#15249 = CARTESIAN_POINT ( 'NONE',  ( 3.996239228619476336, 15.12369778636299777, 4.999999999999999112 ) ) ;
#15250 = DIRECTION ( 'NONE',  ( 0.000000000000000000, -1.000000000000000000, 0.000000000000000000 ) ) ;
#15251 = CARTESIAN_POINT ( 'NONE',  ( 9.989285784994811124, 26.02657572554299747, 0.5301777604595849791 ) ) ;
#15252 = CARTESIAN_POINT ( 'NONE',  ( 7.188101187499999156, -25.62500000204838813, 2.977408999572654924 ) ) ;
#15253 = CARTESIAN_POINT ( 'NONE',  ( 70.89460441624491693, 4.000000000000014211, 0.000000000000000000 ) ) ;
#15254 = SURFACE_SIDE_STYLE ('',( #23377 ) ) ;
#15255 = CARTESIAN_POINT ( 'NONE',  ( 7.200568560992048006, 40.92548620364146927, -70.61799382922531265 ) ) ;
#15256 = ADVANCED_FACE ( 'NONE', ( #15306 ), #72992, .T. ) ;
#15257 = AXIS2_PLACEMENT_3D ( 'NONE', #104626, #14009, #31822 ) ;
#15258 = ORIENTED_EDGE ( 'NONE', *, *, #65031, .T. ) ;
#15259 = ADVANCED_FACE ( 'NONE', ( #16363 ), #57339, .T. ) ;
#15260 = COLOUR_RGB ( '', 0.08235294, 0.09019608, 0.10196078) ;
#15262 = ORIENTED_EDGE ( 'NONE', *, *, #57076, .T. ) ;
#15261 = DIRECTION ( 'NONE',  ( 0.8191520442889884679, 0.000000000000000000, 0.5735764363510509334 ) ) ;
#15263 = CARTESIAN_POINT ( 'NONE',  ( 82.26387345944664276, -32.55838572498345940, 153.0448389433394993 ) ) ;
#15264 = CARTESIAN_POINT ( 'NONE',  ( 0.000000000000000000, 4.898587196589412829E-16, -4.000000000000000000 ) ) ;
#15265 = ORIENTED_EDGE ( 'NONE', *, *, #71479, .F. ) ;
#15266 = CARTESIAN_POINT ( 'NONE',  ( -62.27995536352283779, 50.00000000000000000, 9.818553861624332413 ) ) ;
#15267 = ADVANCED_FACE ( 'NONE', ( #49253 ), #68311, .T. ) ;
#15268 = CARTESIAN_POINT ( 'NONE',  ( 7.413471587080152858, -87.64352159168326750, -3.013058070223548324 ) ) ;
#15269 = CARTESIAN_POINT ( 'NONE',  ( -2.977408999572654480, -12.12500000204838635, 7.188101187499999156 ) ) ;
#15270 = CARTESIAN_POINT ( 'NONE',  ( 0.000000000000000000, 4.000000000000000000, 0.000000000000000000 ) ) ;
#15271 = CARTESIAN_POINT ( 'NONE',  ( -47.68231610104891871, -57.68007204195236426, 71.30078553503261674 ) ) ;
#15272 = B_SPLINE_SURFACE_WITH_KNOTS ( 'NONE', 3, 3, ( 
 ( #39913, #16152, #98658, #73858, #9116, #42025, #106752, #33971, #89527, #65244 ),
 ( #74908, #40970, #41494, #992, #24808, #99734, #58760, #57660, #98135, #56604 ),
 ( #48510, #81404, #16692, #91655, #31833, #47978, #90047, #8591, #80884, #6995 ),
 ( #97587, #49040, #81937, #49582, #8057, #82491, #7515, #72787, #105692, #64716 ),
 ( #40433, #43623, #36641, #19936, #60367, #9643, #67381, #93242, #69508, #83542 ),
 ( #28544, #10707, #51165, #35038, #68984, #102394, #3714, #52240, #17772, #60889 ),
 ( #52778, #19406, #42552, #67901, #85147, #35571, #61424, #11775, #93777, #76515 ),
 ( #50625, #85698, #68445, #11239, #44707, #27492, #2623, #101859, #84084, #34513 ) ),
 .UNSPECIFIED., .F., .F., .F.,
 ( 4, 2, 2, 4 ),
 ( 4, 2, 2, 2, 4 ),
 ( 0.000000000000000000, 0.2500000000000000000, 0.5000000000000000000, 1.000000000000000000 ),
 ( 0.000000000000000000, 0.1250000000000000000, 0.2500000000000000000, 0.5000000000000000000, 1.000000000000000000 ),
 .UNSPECIFIED. ) ;
#15273 = CARTESIAN_POINT ( 'NONE',  ( 9.614447121721056533, 294.6546896927073931, 9.895101723320543385 ) ) ;
#15274 = EDGE_LOOP ( 'NONE', ( #37589, #73123, #97533, #57658, #43358, #93947 ) ) ;
#15275 =( NAMED_UNIT ( * ) SI_UNIT ( $, .STERADIAN. ) SOLID_ANGLE_UNIT ( ) );
#15276 = CARTESIAN_POINT ( 'NONE',  ( 4.258999010316452782, 140.4059127768352653, 5.000000000000000000 ) ) ;
#15277 = DIRECTION ( 'NONE',  ( -1.000000000000000000, -1.224606353822377258E-16, -0.000000000000000000 ) ) ;
#15278 = LINE ( 'NONE', #71924, #43071 ) ;
#15279 = VERTEX_POINT ( 'NONE', #58429 ) ;
#15280 = CARTESIAN_POINT ( 'NONE',  ( -5.656854249492379694, -12.12500000409676915, -5.656854249492380582 ) ) ;
#15281 = CARTESIAN_POINT ( 'NONE',  ( -27.20181548915192948, -20.34077866823755798, 31.75751083479892856 ) ) ;
#15282 = CARTESIAN_POINT ( 'NONE',  ( 9.999999999999998224, 15.00000000000000000, -2.283746462400398747E-15 ) ) ;
#15283 = CARTESIAN_POINT ( 'NONE',  ( 32.87547266101556431, 465.6993878536748070, 10.91512469976365551 ) ) ;
#15284 = AXIS2_PLACEMENT_3D ( 'NONE', #66220, #67305, #12105 ) ;
#15285 = CARTESIAN_POINT ( 'NONE',  ( -9.842473135306409660, 88.58931817113585794, 1.785129593756285660 ) ) ;
#15286 = FACE_OUTER_BOUND ( 'NONE', #6634, .T. ) ;
#15287 = PRODUCT_CONTEXT ( 'NONE', #49301, 'mechanical' ) ;
#15288 = CARTESIAN_POINT ( 'NONE',  ( -9.333892298909264085, 31.78275731625031852, -3.590295303293458140 ) ) ;
#15289 = ORIENTED_EDGE ( 'NONE', *, *, #16638, .F. ) ;
#15290 = CARTESIAN_POINT ( 'NONE',  ( -4.587653515170670104, -47.78786149309958375, 43.03795885842958313 ) ) ;
#15291 = LINE ( 'NONE', #32029, #102540 ) ;
#15292 = DIRECTION ( 'NONE',  ( 1.000000000000000000, 0.000000000000000000, 0.000000000000000000 ) ) ;
#15293 = CARTESIAN_POINT ( 'NONE',  ( -67.60950767405599038, -38.09528385293550201, -32.01701373524668526 ) ) ;
#15294 = DIRECTION ( 'NONE',  ( -1.000000000000000000, -1.224606353822377258E-16, -0.000000000000000000 ) ) ;
#15295 = VERTEX_POINT ( 'NONE', #23976 ) ;
#15296 = CARTESIAN_POINT ( 'NONE',  ( 5.656854249492380582, -9.500000004096769146, -5.656854249492379694 ) ) ;
#15297 = CARTESIAN_POINT ( 'NONE',  ( 91.26148061703614189, -57.61363950115104160, 204.2176009484390136 ) ) ;
#15298 = CIRCLE ( 'NONE', #35996, 0.5000000000000004441 ) ;
#15299 = EDGE_CURVE ( 'NONE', #56333, #54099, #40642, .T. ) ;
#15300 = CARTESIAN_POINT ( 'NONE',  ( 35.67416790563076034, 463.3851398029195252, 19.97299141547252077 ) ) ;
#15301 = CARTESIAN_POINT ( 'NONE',  ( 3.787353845334695546, 16.54002813235528535, 5.888118072323124785 ) ) ;
#15302 = CARTESIAN_POINT ( 'NONE',  ( 62.59524157938817268, 40.83906611471955728, 18.50207713792757147 ) ) ;
#15303 = CARTESIAN_POINT ( 'NONE',  ( -73.49543186908600489, -60.00000000000001421, 167.1451735809920081 ) ) ;
#15304 = CONICAL_SURFACE ( 'NONE', #65276, 13.50000000000000178, 1.047197551196596077 ) ;
#15305 = CARTESIAN_POINT ( 'NONE',  ( -40.73878142687892279, 503.7113041876743864, 10.19672445236252045 ) ) ;
#15306 = FACE_OUTER_BOUND ( 'NONE', #65775, .T. ) ;
#15307 = CARTESIAN_POINT ( 'NONE',  ( -21.51569398614858031, 294.9107018935607130, -9.987480606144490736 ) ) ;
#15308 = CARTESIAN_POINT ( 'NONE',  ( -85.96492870306816769, -28.40779642704074348, 181.6674700888168275 ) ) ;
#15309 = EDGE_LOOP ( 'NONE', ( #47730, #74019, #20688, #95280, #103975 ) ) ;
#15310 = CARTESIAN_POINT ( 'NONE',  ( 32.02727017616632565, 314.0444030994631248, -7.577622885421612331 ) ) ;
#15311 = EDGE_LOOP ( 'NONE', ( #31852, #86351, #49524, #43879 ) ) ;
#15313 = EDGE_CURVE ( 'NONE', #96379, #70568, #95003, .T. ) ;
#15312 = CARTESIAN_POINT ( 'NONE',  ( 62.33904886068935980, -4.000000000000000888, 4.898587196589422689E-16 ) ) ;
#15314 = CARTESIAN_POINT ( 'NONE',  ( -5.833333333333327708, -3.728231135448884181, 103.8776713793258750 ) ) ;
#15315 = CARTESIAN_POINT ( 'NONE',  ( -84.58417382167392873, -60.18425325025634720, -16.69743988867924500 ) ) ;
#15316 = CIRCLE ( 'NONE', #75606, 4.000000000000007105 ) ;
#15317 = CARTESIAN_POINT ( 'NONE',  ( 6.326622418652846136, 1.327077765692999733, -6.831545684615175418 ) ) ;
#15318 = VECTOR ( 'NONE', #73776, 1000.000000000000000 ) ;
#15319 = VERTEX_POINT ( 'NONE', #7208 ) ;
#15320 = CARTESIAN_POINT ( 'NONE',  ( 6.562934840145643101, 7.579717272840337472, -0.5631738335430729325 ) ) ;
#15321 = CARTESIAN_POINT ( 'NONE',  ( 10.56215772281497323, 17.85407101821802556, -9.582426342768091132 ) ) ;
#15322 = CARTESIAN_POINT ( 'NONE',  ( 2.083846472846741813E-15, -1.734723475976807094E-15, 17.01589776168603407 ) ) ;
#15323 = MECHANICAL_DESIGN_GEOMETRIC_PRESENTATION_REPRESENTATION (  '', ( #56657 ), #44614 ) ;
#15324 = CARTESIAN_POINT ( 'NONE',  ( -35.20576575318266066, 464.3971859289012514, 19.03676487905852710 ) ) ;
#15325 = CONICAL_SURFACE ( 'NONE', #60103, 8.000000000000000000, 0.9599310885968911355 ) ;
#15326 = CARTESIAN_POINT ( 'NONE',  ( 77.20805073229469428, -29.99999999999999289, -26.53535389768476449 ) ) ;
#15327 = CARTESIAN_POINT ( 'NONE',  ( -78.91132512760897555, -36.02857813642251728, 136.0548663355014867 ) ) ;
#15328 = ORIENTED_EDGE ( 'NONE', *, *, #4440, .F. ) ;
#15329 = CARTESIAN_POINT ( 'NONE',  ( 102.9313392694734688, 1.016364837396684119E-14, 0.000000000000000000 ) ) ;
#15330 = CARTESIAN_POINT ( 'NONE',  ( 105.7047805233263063, -57.64761371320827266, 201.1859495630244226 ) ) ;
#15331 = CARTESIAN_POINT ( 'NONE',  ( 0.000000000000000000, -48.79941684889506348, 112.0000000000000000 ) ) ;
#15333 = CIRCLE ( 'NONE', #101498, 2.000000000000001776 ) ;
#15332 = CARTESIAN_POINT ( 'NONE',  ( 39.06108710778507032, 311.1868365531275913, 1.892069196330523839 ) ) ;
#15334 = ADVANCED_FACE ( 'NONE', ( #27160 ), #45902, .T. ) ;
#15335 = CARTESIAN_POINT ( 'NONE',  ( 0.05458999538792581874, -1.264741368075138706, -6.499999999999999112 ) ) ;
#15336 = ORIENTED_EDGE ( 'NONE', *, *, #88401, .F. ) ;
#15337 = AXIS2_PLACEMENT_3D ( 'NONE', #91793, #50258, #66443 ) ;
#15338 = DIRECTION ( 'NONE',  ( 0.000000000000000000, 0.000000000000000000, -1.000000000000000000 ) ) ;
#15339 = FACE_OUTER_BOUND ( 'NONE', #23385, .T. ) ;
#15340 = CARTESIAN_POINT ( 'NONE',  ( -16.42257055868371651, 36.46149248629888007, 24.27355254955521247 ) ) ;
#15341 = CARTESIAN_POINT ( 'NONE',  ( -1.320432766682874540E-15, -16.53125000204838813, 7.188101187500000044 ) ) ;
#15342 = CARTESIAN_POINT ( 'NONE',  ( 7.970070017554211184, -4.546953124339766283, -8.057670357645358550 ) ) ;
#15343 = CYLINDRICAL_SURFACE ( 'NONE', #91116, 1.250000000000001110 ) ;
#15344 = CARTESIAN_POINT ( 'NONE',  ( 1.249506209833404657, 34.67599045332981689, 28.33744947526314206 ) ) ;
#15345 = CARTESIAN_POINT ( 'NONE',  ( 0.000000000000000000, 0.000000000000000000, -7.554475477074167777 ) ) ;
#15346 = AXIS2_PLACEMENT_3D ( 'NONE', #2246, #52943, #2791 ) ;
#15347 = EDGE_LOOP ( 'NONE', ( #83293, #76470, #25726, #74518, #92935 ) ) ;
#15348 = LINE ( 'NONE', #97323, #650 ) ;
#15350 = CARTESIAN_POINT ( 'NONE',  ( 29.01731335256807398, -49.90763980309816361, 34.62778969272466156 ) ) ;
#15349 = CARTESIAN_POINT ( 'NONE',  ( -34.17891763260271887, -14.21045842199440301, 38.95228509905292924 ) ) ;
#15351 = CARTESIAN_POINT ( 'NONE',  ( -24.22978927791485404, 25.18864859774202714, 32.69423595551459982 ) ) ;
#15352 = MECHANICAL_DESIGN_GEOMETRIC_PRESENTATION_REPRESENTATION (  '', ( #53244 ), #80644 ) ;
#15353 = ORIENTED_EDGE ( 'NONE', *, *, #2460, .F. ) ;
#15354 = ORIENTED_EDGE ( 'NONE', *, *, #98244, .F. ) ;
#15356 = FACE_BOUND ( 'NONE', #70114, .T. ) ;
#15355 = DIRECTION ( 'NONE',  ( -1.000000000000000000, -0.000000000000000000, -0.000000000000000000 ) ) ;
#15357 = CARTESIAN_POINT ( 'NONE',  ( -43.00000000000000000, 500.0000000000002274, 0.000000000000000000 ) ) ;
#15358 = DIRECTION ( 'NONE',  ( -0.5735764363510497121, 0.8191520442889892450, 1.003171929053521665E-16 ) ) ;
#15359 = CARTESIAN_POINT ( 'NONE',  ( 42.23079339798727716, 460.7352525929352964, 2.726051457480584972 ) ) ;
#15360 = CARTESIAN_POINT ( 'NONE',  ( -30.00000000000000000, 490.5636507776930557, 7.413185101875094496 ) ) ;
#15361 =( NAMED_UNIT ( * ) SI_UNIT ( $, .STERADIAN. ) SOLID_ANGLE_UNIT ( ) );
#15362 = ORIENTED_EDGE ( 'NONE', *, *, #78370, .T. ) ;
#15363 = CARTESIAN_POINT ( 'NONE',  ( 15.96501273729558257, -60.00000000000000000, -42.10368348739202560 ) ) ;
#15364 = B_SPLINE_CURVE_WITH_KNOTS ( 'NONE', 3,
 ( #41706, #66507, #1755, #82151, #49788, #57334 ),
 .UNSPECIFIED., .F., .F.,
 ( 4, 2, 4 ),
 ( 0.000000000000000000, 0.5000000000000000000, 1.000000000000000000 ),
 .UNSPECIFIED. ) ;
#15365 = CARTESIAN_POINT ( 'NONE',  ( 89.67317295579802305, -30.00000000000008882, 189.5710670903794721 ) ) ;
#15366 = LINE ( 'NONE', #23493, #70340 ) ;
#15367 = CARTESIAN_POINT ( 'NONE',  ( 30.00000000000000000, 1.714505518806294441E-15, 13.00000000000000000 ) ) ;
#15368 = DIRECTION ( 'NONE',  ( -0.000000000000000000, 0.000000000000000000, -1.000000000000000000 ) ) ;
#15369 = ORIENTED_EDGE ( 'NONE', *, *, #78781, .F. ) ;
#15370 = B_SPLINE_CURVE_WITH_KNOTS ( 'NONE', 3,
 ( #103810, #29955, #62839, #95730, #38571, #97838 ),
 .UNSPECIFIED., .F., .F.,
 ( 4, 2, 4 ),
 ( 2.380729205335813291E-07, 0.003943479449179693175, 0.007886720825438852528 ),
 .UNSPECIFIED. ) ;
#15371 = ORIENTED_EDGE ( 'NONE', *, *, #56373, .T. ) ;
#15372 = VERTEX_POINT ( 'NONE', #9318 ) ;
#15373 = DIRECTION ( 'NONE',  ( 1.000000000000000000, -0.000000000000000000, -0.000000000000000000 ) ) ;
#15374 = CARTESIAN_POINT ( 'NONE',  ( -32.28552837373656814, 464.7648866755938570, 15.30384310834764428 ) ) ;
#15375 = CARTESIAN_POINT ( 'NONE',  ( -39.30528374322037877, 437.8648113156952490, 22.91822685283586125 ) ) ;
#15376 = CARTESIAN_POINT ( 'NONE',  ( 24.53406555947808343, 304.2472816665747359, 10.24320745312229164 ) ) ;
#15377 = CARTESIAN_POINT ( 'NONE',  ( -41.00068889408650108, 320.1545059241889248, 4.151165785700200672 ) ) ;
#15378 = CARTESIAN_POINT ( 'NONE',  ( -5.005299804888146298, -64.88413123474070687, 13.89682420523173079 ) ) ;
#15380 = CARTESIAN_POINT ( 'NONE',  ( -46.00000000000000000, 488.1813821183741879, 2.479370420756893623 ) ) ;
#15379 = COLOUR_RGB ( '', 0.08235294, 0.09019608, 0.10196078) ;
#15381 = CARTESIAN_POINT ( 'NONE',  ( 31.08349330513380337, 1.593028355512270567E-15, 0.000000000000000000 ) ) ;
#15382 = ORIENTED_EDGE ( 'NONE', *, *, #52147, .T. ) ;
#15383 = CARTESIAN_POINT ( 'NONE',  ( -9.643763425038864412, 44.08769799646883314, 13.07246033778566918 ) ) ;
#15384 = ORIENTED_EDGE ( 'NONE', *, *, #19855, .F. ) ;
#15385 = FACE_OUTER_BOUND ( 'NONE', #31760, .T. ) ;
#15386 = DIRECTION ( 'NONE',  ( 0.000000000000000000, 0.000000000000000000, 1.000000000000000000 ) ) ;
#15387 = CARTESIAN_POINT ( 'NONE',  ( -41.72175139495112717, 485.6241823541930103, -4.286260377904754115 ) ) ;
#15388 = AXIS2_PLACEMENT_3D ( 'NONE', #105245, #71276, #104170 ) ;
#15389 = CIRCLE ( 'NONE', #5078, 3.309500000000001663 ) ;
#15390 = CARTESIAN_POINT ( 'NONE',  ( -62.94953480991654970, -59.99999999999994316, 90.76860819568858574 ) ) ;
#15391 = CARTESIAN_POINT ( 'NONE',  ( 68.52817887026473898, -39.48419332027852846, 97.13330144592191573 ) ) ;
#15392 = ORIENTED_EDGE ( 'NONE', *, *, #45945, .T. ) ;
#15393 = CARTESIAN_POINT ( 'NONE',  ( 42.00353007817209061, 464.8744261507625311, 15.23981939152684184 ) ) ;
#15394 = EDGE_CURVE ( 'NONE', #28630, #70272, #33304, .T. ) ;
#15395 = CARTESIAN_POINT ( 'NONE',  ( -6.705175466950450414, 9.539476085123771654, 2.022930269817423188 ) ) ;
#15396 = EDGE_CURVE ( 'NONE', #71668, #58013, #32134, .T. ) ;
#15397 = CARTESIAN_POINT ( 'NONE',  ( -51.62523913740291448, -57.67116585372185966, -39.59675499642695939 ) ) ;
#15398 = ORIENTED_EDGE ( 'NONE', *, *, #71955, .F. ) ;
#15399 = VECTOR ( 'NONE', #15987, 1000.000000000000000 ) ;
#15400 = DIRECTION ( 'NONE',  ( -0.5735764363510494901, -0.8191520442889894671, 0.000000000000000000 ) ) ;
#15401 = CONICAL_SURFACE ( 'NONE', #24063, 4.000000000000007105, 0.9599310885968835860 ) ;
#15402 = CARTESIAN_POINT ( 'NONE',  ( -37.36240688365094798, 491.3429102029593309, 12.25869953513271682 ) ) ;
#15403 = CARTESIAN_POINT ( 'NONE',  ( 8.000000000000000000, -27.59375000409676915, -3.313708498984761608 ) ) ;
#15404 = CARTESIAN_POINT ( 'NONE',  ( 7.137815226408910974, -4.999999999999998224, 4.175893272575850190 ) ) ;
#15405 = CARTESIAN_POINT ( 'NONE',  ( 9.999952458099503616, 246.0001188547612685, 0.2653554233229091230 ) ) ;
#15406 = FACE_OUTER_BOUND ( 'NONE', #57825, .T. ) ;
#15407 = CARTESIAN_POINT ( 'NONE',  ( -10.31642403553700937, 7.048099644362468830, 0.000000000000000000 ) ) ;
#15408 = CARTESIAN_POINT ( 'NONE',  ( 13.50000000000000711, 5.257130651325589099, -0.5389759092231705129 ) ) ;
#15409 = DIRECTION ( 'NONE',  ( 0.9970137454669278920, 1.615587133892632177E-27, -0.07722429248628930043 ) ) ;
#15410 = CARTESIAN_POINT ( 'NONE',  ( 15.72335261638225035, 304.5560424773130990, 8.874135054364925779 ) ) ;
#15411 = ORIENTED_EDGE ( 'NONE', *, *, #65165, .F. ) ;
#15412 = DIRECTION ( 'NONE',  ( 0.5735764363510466035, -0.8191520442889914655, 1.003171929053524500E-16 ) ) ;
#15413 = CARTESIAN_POINT ( 'NONE',  ( -4.852941176470598528, -3.000000000000002665, -70.80672828634229177 ) ) ;
#15414 = CARTESIAN_POINT ( 'NONE',  ( 12.80896177052940388, -60.00000000000000711, 39.70888688113913645 ) ) ;
#15415 = CARTESIAN_POINT ( 'NONE',  ( -94.05504825925655155, -30.00000000000000000, 191.2807258966970210 ) ) ;
#15416 = AXIS2_PLACEMENT_3D ( 'NONE', #75488, #69018, #60923 ) ;
#15417 = LINE ( 'NONE', #48304, #103742 ) ;
#15418 = CARTESIAN_POINT ( 'NONE',  ( 45.11600752062921060, -57.68303782434002613, 65.41414365635188233 ) ) ;
#15420 = DIRECTION ( 'NONE',  ( 1.000000000000000000, 1.224606353822377258E-16, 0.000000000000000000 ) ) ;
#15419 = CARTESIAN_POINT ( 'NONE',  ( -0.8392880725949716236, 25.95834017491164403, -38.57005309225670686 ) ) ;
#15421 = ADVANCED_FACE ( 'NONE', ( #19611 ), #35695, .T. ) ;
#15422 = CARTESIAN_POINT ( 'NONE',  ( 11.11178199064544536, -22.91032599454487695, -38.54163065549817446 ) ) ;
#15423 = CARTESIAN_POINT ( 'NONE',  ( -9.700350089084256666, 15.75268258782372754, 2.455962139888509199 ) ) ;
#15424 = DIRECTION ( 'NONE',  ( -0.000000000000000000, 1.000000000000000000, -0.000000000000000000 ) ) ;
#15425 = CARTESIAN_POINT ( 'NONE',  ( -24.73795869524107616, -60.00000000000000000, 41.10165728384131967 ) ) ;
#15426 = CARTESIAN_POINT ( 'NONE',  ( 13.07948690922876089, 8.363364708107999590, 8.866367791206201332 ) ) ;
#15427 = AXIS2_PLACEMENT_3D ( 'NONE', #46823, #102947, #29618 ) ;
#15428 = CARTESIAN_POINT ( 'NONE',  ( 1.099023582544892408, 45.97038027629827184, -16.88323843016358694 ) ) ;
#15429 = CARTESIAN_POINT ( 'NONE',  ( -87.09031288375886959, -28.00572983669372107, 187.1676684957507177 ) ) ;
#15430 = ORIENTED_EDGE ( 'NONE', *, *, #100437, .T. ) ;
#15431 = CARTESIAN_POINT ( 'NONE',  ( 17.50000000000004619, 50.67917894245540822, 63.46126552127685727 ) ) ;
#15432 = CARTESIAN_POINT ( 'NONE',  ( 11.70799159436998593, -8.253155071789681330, 19.32017322931982051 ) ) ;
#15433 = CARTESIAN_POINT ( 'NONE',  ( -15.66209394986200287, -39.47634415140716868, 30.64911114313175133 ) ) ;
#15434 = CARTESIAN_POINT ( 'NONE',  ( 1.107919095008624844E-15, -5.309483803148806302, -3.803704290982252711 ) ) ;
#15436 = EDGE_CURVE ( 'NONE', #35268, #91137, #89081, .T. ) ;
#15435 = CARTESIAN_POINT ( 'NONE',  ( 21.36650669486618881, 0.000000000000000000, 4.000000000000000888 ) ) ;
#15437 = ORIENTED_EDGE ( 'NONE', *, *, #51035, .T. ) ;
#15438 = CARTESIAN_POINT ( 'NONE',  ( 35.11650669486618170, 1.474610560812782335E-15, 0.000000000000000000 ) ) ;
#15439 = CARTESIAN_POINT ( 'NONE',  ( -7.022229286278467875, -4.221542269106504541, -17.11103215587112913 ) ) ;
#15440 = CARTESIAN_POINT ( 'NONE',  ( -29.77450884433714151, 8.177050405881796991, -42.10535821593515493 ) ) ;
#15441 = AXIS2_PLACEMENT_3D ( 'NONE', #68220, #33745, #10501 ) ;
#15442 = CYLINDRICAL_SURFACE ( 'NONE', #12279, 4.000000000000000888 ) ;
#15443 = CARTESIAN_POINT ( 'NONE',  ( -7.744168461338430731, -81.53745938284842509, 2.019395720771552050 ) ) ;
#15444 = CARTESIAN_POINT ( 'NONE',  ( 73.52739441614612304, -60.00000000000000000, 167.4607074514827332 ) ) ;
#15445 = CARTESIAN_POINT ( 'NONE',  ( -45.50145573691759182, 405.2496736015978627, 8.430338687477670234 ) ) ;
#15446 = VERTEX_POINT ( 'NONE', #93464 ) ;
#15447 = CARTESIAN_POINT ( 'NONE',  ( -2.139906788305918628, -30.00000000000000355, 7.052091621315984327 ) ) ;
#15448 = LINE ( 'NONE', #14910, #47196 ) ;
#15449 = CONICAL_SURFACE ( 'NONE', #47922, 3.309500000000001663, 0.9599310885968770357 ) ;
#15450 = CARTESIAN_POINT ( 'NONE',  ( -0.6508621380849229920, -8.763657152406457485, -7.907633014911229274 ) ) ;
#15451 = CARTESIAN_POINT ( 'NONE',  ( 4.147930821993710993, -1.050632865739543620, 104.5115743862824615 ) ) ;
#15452 = EDGE_CURVE ( 'NONE', #75804, #54950, #20141, .T. ) ;
#15453 = ORIENTED_EDGE ( 'NONE', *, *, #15941, .F. ) ;
#15454 = CARTESIAN_POINT ( 'NONE',  ( -25.77297728949481126, 308.6353064608509840, 9.816699030083849919 ) ) ;
#15455 = ORIENTED_EDGE ( 'NONE', *, *, #44345, .F. ) ;
#15456 = DIRECTION ( 'NONE',  ( 0.000000000000000000, -1.000000000000000000, 0.000000000000000000 ) ) ;
#15458 = EDGE_CURVE ( 'NONE', #99968, #13469, #47724, .T. ) ;
#15457 = CARTESIAN_POINT ( 'NONE',  ( 31.09913253216321749, 439.4710977885268903, 22.91121712903616725 ) ) ;
#15459 = FACE_OUTER_BOUND ( 'NONE', #23982, .T. ) ;
#15460 = VERTEX_POINT ( 'NONE', #51378 ) ;
#15461 = CARTESIAN_POINT ( 'NONE',  ( 63.03617022297318329, 49.99999999997997691, -16.93907820452584545 ) ) ;
#15462 = FACE_OUTER_BOUND ( 'NONE', #80128, .T. ) ;
#15463 = AXIS2_PLACEMENT_3D ( 'NONE', #46789, #62983, #5791 ) ;
#15464 = CARTESIAN_POINT ( 'NONE',  ( -105.8057338367873399, -59.99999999999877076, 201.6387488181161700 ) ) ;
#15465 = CARTESIAN_POINT ( 'NONE',  ( 24.83349330513380693, 1.593028355512270962E-15, 0.000000000000000000 ) ) ;
#15466 = AXIS2_PLACEMENT_3D ( 'NONE', #81714, #25678, #58542 ) ;
#15467 = CARTESIAN_POINT ( 'NONE',  ( 85.55794531748325937, -60.00000000000000000, 200.3757775331295079 ) ) ;
#15468 = DIRECTION ( 'NONE',  ( 1.000000000000000000, 1.224606353822377258E-16, 0.000000000000000000 ) ) ;
#15469 = LINE ( 'NONE', #65087, #58952 ) ;
#15471 = CARTESIAN_POINT ( 'NONE',  ( 17.74185477829191981, -32.51177142622724148, 29.60969788138565661 ) ) ;
#15470 = CARTESIAN_POINT ( 'NONE',  ( -114.5289996431801853, -60.00000000000001421, 168.5344195898668715 ) ) ;
#15472 = ADVANCED_FACE ( 'NONE', ( #26110 ), #76993, .T. ) ;
#15474 = CARTESIAN_POINT ( 'NONE',  ( 97.09147383894379857, -38.00000000000009237, 192.8437217724261359 ) ) ;
#15473 = PRODUCT_DEFINITION_CONTEXT ( 'detailed design', #100980, 'design' ) ;
#15475 = CARTESIAN_POINT ( 'NONE',  ( 0.000000000000000000, -8.000000000000000000, 0.000000000000000000 ) ) ;
#15476 = CONICAL_SURFACE ( 'NONE', #53368, 5.000000000000010658, 0.9599310885968697082 ) ;
#15477 = CARTESIAN_POINT ( 'NONE',  ( -44.56587912721629152, -29.16193315628479610, 40.40586370753838708 ) ) ;
#15479 = DIRECTION ( 'NONE',  ( -1.000000000000000000, -0.000000000000000000, -0.000000000000000000 ) ) ;
#15478 = B_SPLINE_CURVE_WITH_KNOTS ( 'NONE', 3,
 ( #66098, #57995, #50960, #93037, #90916, #17568, #17030, #49906, #74706, #100587, #34835, #9984, #8914, #41818, #19198, #67705, #42888, #10512, #83873, #50428 ),
 .UNSPECIFIED., .F., .F.,
 ( 4, 2, 2, 2, 2, 2, 2, 2, 2, 4 ),
 ( 0.003775051291532607704, 0.004278405665375015383, 0.004781760039217423930, 0.005285114413059831609, 0.005788468786902239288, 0.006040145973823445730, 0.006291823160744653039, 0.006795177534587053779, 0.007298531908429453652, 0.007801886282271855259 ),
 .UNSPECIFIED. ) ;
#15480 = EDGE_LOOP ( 'NONE', ( #34083, #13388, #22135, #30857, #27596 ) ) ;
#15481 = EDGE_CURVE ( 'NONE', #45468, #95564, #18519, .T. ) ;
#15482 = CARTESIAN_POINT ( 'NONE',  ( -33.00000000000000000, 464.3970849722209664, 17.41240408234212111 ) ) ;
#15483 = DIRECTION ( 'NONE',  ( 0.000000000000000000, -1.000000000000000000, 0.000000000000000000 ) ) ;
#15484 = CARTESIAN_POINT ( 'NONE',  ( -4.999999999997973177, -61.61794147117323206, 12.73961838306073879 ) ) ;
#15485 = FACE_OUTER_BOUND ( 'NONE', #24863, .T. ) ;
#15486 = COLOUR_RGB ( '', 0.72549020, 0.75294118, 0.79215686) ;
#15487 = FILL_AREA_STYLE_COLOUR ( '', #1703 ) ;
#15488 = CARTESIAN_POINT ( 'NONE',  ( 35.74483125092430669, 413.6409941285803598, 6.029078300230034770 ) ) ;
#15489 = ORIENTED_EDGE ( 'NONE', *, *, #37600, .F. ) ;
#15490 = CARTESIAN_POINT ( 'NONE',  ( 4.680975426248633831, -47.58422982932144407, 103.4780497728483368 ) ) ;
#15491 = ORIENTED_EDGE ( 'NONE', *, *, #97547, .F. ) ;
#15492 = CARTESIAN_POINT ( 'NONE',  ( 95.01775444805275583, -29.99999999999331735, 199.9312514212468272 ) ) ;
#15493 = LINE ( 'NONE', #63535, #102485 ) ;
#15494 = CARTESIAN_POINT ( 'NONE',  ( 6.031322594622289479, 41.99459408341585487, -59.73016589819391697 ) ) ;
#15495 = FILL_AREA_STYLE_COLOUR ( '', #15486 ) ;
#15496 = CARTESIAN_POINT ( 'NONE',  ( 94.47209748978787047, -30.00000000000000000, 114.8027109744303687 ) ) ;
#15497 = CIRCLE ( 'NONE', #87809, 4.000000000000000000 ) ;
#15498 = LINE ( 'NONE', #41897, #105324 ) ;
#15499 = ORIENTED_EDGE ( 'NONE', *, *, #18587, .F. ) ;
#15500 = CIRCLE ( 'NONE', #94760, 4.000000000000007105 ) ;
#15501 = ORIENTED_EDGE ( 'NONE', *, *, #77459, .T. ) ;
#15502 = ORIENTED_EDGE ( 'NONE', *, *, #19619, .T. ) ;
#15503 = CARTESIAN_POINT ( 'NONE',  ( -32.81762910952392787, 465.7339109552316359, 14.50750636005640892 ) ) ;
#15504 = CARTESIAN_POINT ( 'NONE',  ( -6.392921701574284299, 41.54610357429506706, -70.64273452805430509 ) ) ;
#15505 = CARTESIAN_POINT ( 'NONE',  ( -38.46627235044618942, 463.5297074240463076, 19.68396873923987300 ) ) ;
#15506 = VERTEX_POINT ( 'NONE', #51913 ) ;
#15507 =( NAMED_UNIT ( * ) SI_UNIT ( $, .STERADIAN. ) SOLID_ANGLE_UNIT ( ) );
#15508 = ORIENTED_EDGE ( 'NONE', *, *, #33199, .F. ) ;
#15509 = DIRECTION ( 'NONE',  ( 0.000000000000000000, 0.000000000000000000, 1.000000000000000000 ) ) ;
#15510 = CARTESIAN_POINT ( 'NONE',  ( 81.59129191571777540, -38.84187913677770609, 195.3900936346319952 ) ) ;
#15511 = CARTESIAN_POINT ( 'NONE',  ( 11.44979815925891842, 7.555154868943327884, 9.462210209118575577 ) ) ;
#15512 = DIRECTION ( 'NONE',  ( 0.000000000000000000, -1.000000000000000000, 0.000000000000000000 ) ) ;
#15513 = CARTESIAN_POINT ( 'NONE',  ( 37.13996112556628759, 311.9295539373470092, 14.05047757564090460 ) ) ;
#15514 = CARTESIAN_POINT ( 'NONE',  ( -14.29190075645675861, 21.26710225494873185, 5.626279437267716510 ) ) ;
#15515 = CARTESIAN_POINT ( 'NONE',  ( -40.54048956546211713, 460.8805895396322398, 2.213361020665719270 ) ) ;
#15516 = CARTESIAN_POINT ( 'NONE',  ( 42.73661845073595345, 422.4026850698294311, 19.47781275723680849 ) ) ;
#15517 = ADVANCED_FACE ( 'NONE', ( #101543 ), #67591, .T. ) ;
#15518 = CARTESIAN_POINT ( 'NONE',  ( 18.09999999999999787, -3.309499999999999886, 4.475777889183790779E-16 ) ) ;
#15519 = ORIENTED_EDGE ( 'NONE', *, *, #38703, .F. ) ;
#15520 = CARTESIAN_POINT ( 'NONE',  ( -35.52970765843740963, 407.4888284783144741, 7.046337194675730053 ) ) ;
#15521 = CARTESIAN_POINT ( 'NONE',  ( -35.43347100846272468, 303.8941957845916590, 4.023230233832623348 ) ) ;
#15522 = DIRECTION ( 'NONE',  ( -0.2255559232117777535, 0.1250062448739086840, 0.9661769839147521521 ) ) ;
#15523 = CARTESIAN_POINT ( 'NONE',  ( 37.61650669486618881, 1.474610560812782335E-15, 0.000000000000000000 ) ) ;
#15524 = CARTESIAN_POINT ( 'NONE',  ( 3.313708498984762496, -15.78124999999999289, 7.999999999999998224 ) ) ;
#15525 = CARTESIAN_POINT ( 'NONE',  ( 44.47534377888506185, -38.31160956920666649, 57.00192013341545305 ) ) ;
#15526 = AXIS2_PLACEMENT_3D ( 'NONE', #29268, #93439, #4413 ) ;
#15527 = ADVANCED_FACE ( 'NONE', ( #60049 ), #85636, .T. ) ;
#15528 = DIRECTION ( 'NONE',  ( -0.8191520442889975717, 0.000000000000000000, -0.5735764363510378328 ) ) ;
#15529 = SURFACE_STYLE_FILL_AREA ( #98569 ) ;
#15530 = VERTEX_POINT ( 'NONE', #26628 ) ;
#15531 = CARTESIAN_POINT ( 'NONE',  ( 85.09804983725459238, -42.94247291440246528, 186.0227739267606637 ) ) ;
#15532 = DIRECTION ( 'NONE',  ( -1.000000000000000000, 0.000000000000000000, 0.000000000000000000 ) ) ;
#15533 = B_SPLINE_CURVE_WITH_KNOTS ( 'NONE', 3,
 ( #38381, #87453, #14059, #23252 ),
 .UNSPECIFIED., .F., .F.,
 ( 4, 4 ),
 ( 7.429119110621935446E-17, 0.001193002000561107449 ),
 .UNSPECIFIED. ) ;
#15534 = VERTEX_POINT ( 'NONE', #46490 ) ;
#15535 = CARTESIAN_POINT ( 'NONE',  ( 95.57137203408007053, -57.67170117783086880, 37.79708907818724128 ) ) ;
#15536 = CARTESIAN_POINT ( 'NONE',  ( 34.62305774441573192, 437.4305192986075213, 5.012907847576154374 ) ) ;
#15537 = DIRECTION ( 'NONE',  ( 0.000000000000000000, 0.000000000000000000, 1.000000000000000000 ) ) ;
#15538 = CARTESIAN_POINT ( 'NONE',  ( 8.099999999999999645, -3.752776749732565253, 6.499999999999999112 ) ) ;
#15539 = ADVANCED_FACE ( 'NONE', ( #29288 ), #70765, .F. ) ;
#15540 = VECTOR ( 'NONE', #86495, 1000.000000000000000 ) ;
#15541 = CARTESIAN_POINT ( 'NONE',  ( 29.07939586085803185, 18.85565742903570552, 39.75811902752973737 ) ) ;
#15542 = CARTESIAN_POINT ( 'NONE',  ( 7.137815226409024660, -5.000000000001136868, -4.175893272573466319 ) ) ;
#15543 = CARTESIAN_POINT ( 'NONE',  ( 0.3470952277635269700, 8.860649561028099086, -7.493596212620244224 ) ) ;
#15546 = CARTESIAN_POINT ( 'NONE',  ( -12.55742542063729417, 5.178327859976680436, 8.085065843704475341 ) ) ;
#15545 = AXIS2_PLACEMENT_3D ( 'NONE', #67709, #100590, #26750 ) ;
#15544 = DIRECTION ( 'NONE',  ( -1.000000000000000000, -1.224606353822377258E-16, -0.000000000000000000 ) ) ;
#15547 = VERTEX_POINT ( 'NONE', #29811 ) ;
#15548 = ADVANCED_FACE ( 'NONE', ( #71286 ), #75284, .T. ) ;
#15549 =( NAMED_UNIT ( * ) SI_UNIT ( $, .STERADIAN. ) SOLID_ANGLE_UNIT ( ) );
#15550 = FILL_AREA_STYLE_COLOUR ( '', #41836 ) ;
#15551 = CARTESIAN_POINT ( 'NONE',  ( -10.50000000000000711, -5.000000000000000000, -78.42624373368740009 ) ) ;
#15552 = CARTESIAN_POINT ( 'NONE',  ( 21.67692307692307452, 4.172000000000003261, 0.000000000000000000 ) ) ;
#15553 = CARTESIAN_POINT ( 'NONE',  ( 9.999999999999996447, 15.00000000000000000, -4.397168787612349306 ) ) ;
#15554 = CARTESIAN_POINT ( 'NONE',  ( -101.3870858685743173, -38.00000000000002132, 187.1511826377679881 ) ) ;
#15555 = B_SPLINE_CURVE_WITH_KNOTS ( 'NONE', 3,
 ( #82900, #64724, #88477, #22165, #15098, #29739, #80354, #14028 ),
 .UNSPECIFIED., .F., .F.,
 ( 4, 2, 2, 4 ),
 ( 0.000000000000000000, 0.5000000000000000000, 0.7500000000000000000, 1.000000000000000000 ),
 .UNSPECIFIED. ) ;
#15556 = VECTOR ( 'NONE', #5694, 1000.000000000000000 ) ;
#15557 = ORIENTED_EDGE ( 'NONE', *, *, #88011, .T. ) ;
#15558 = CARTESIAN_POINT ( 'NONE',  ( -5.385673916453012744, -3.469446951953614189E-15, 18.57417562100670949 ) ) ;
#15559 = FILL_AREA_STYLE_COLOUR ( '', #36562 ) ;
#15560 = CARTESIAN_POINT ( 'NONE',  ( -10.85172174320315541, -16.38067545052308915, -34.74268429604064323 ) ) ;
#15561 = AXIS2_PLACEMENT_3D ( 'NONE', #62617, #4368, #63687 ) ;
#15564 = EDGE_CURVE ( 'NONE', #29160, #26937, #11540, .T. ) ;
#15563 = CARTESIAN_POINT ( 'NONE',  ( -62.18019193066977124, -60.22836170466317185, -29.09066113803248044 ) ) ;
#15562 = CARTESIAN_POINT ( 'NONE',  ( 18.86650669486618881, 4.898587196589411843E-16, -4.000000000000000888 ) ) ;
#15565 = ORIENTED_EDGE ( 'NONE', *, *, #57855, .F. ) ;
#15566 = PRESENTATION_LAYER_ASSIGNMENT (  '', '', ( #31100 ) ) ;
#15567 = ORIENTED_EDGE ( 'NONE', *, *, #44424, .T. ) ;
#15568 = CARTESIAN_POINT ( 'NONE',  ( -26.35538756233841085, 34.76322194132067267, 9.819931615225865329 ) ) ;
#15569 = CARTESIAN_POINT ( 'NONE',  ( 11.27275010301936753, 43.63375202082728777, -13.37403123923981951 ) ) ;
#15570 = CIRCLE ( 'NONE', #84511, 4.000000000000000000 ) ;
#15571 = CARTESIAN_POINT ( 'NONE',  ( -7.500000000000000000, 4.330127018922188320, -10.00000000000000000 ) ) ;
#15572 = CARTESIAN_POINT ( 'NONE',  ( -92.72847056440254221, -59.99999999999998579, -5.749582770862643244 ) ) ;
#15573 = ORIENTED_EDGE ( 'NONE', *, *, #99359, .T. ) ;
#15574 = CARTESIAN_POINT ( 'NONE',  ( 42.42558281948700483, -34.00733088751519517, -29.05298797978474212 ) ) ;
#15575 = CARTESIAN_POINT ( 'NONE',  ( 82.42421628608209971, 1.030564683017419500E-14, 0.000000000000000000 ) ) ;
#15576 = CARTESIAN_POINT ( 'NONE',  ( 98.44225398900675827, -60.33831865521403870, 196.4443166631917563 ) ) ;
#15578 = CARTESIAN_POINT ( 'NONE',  ( -16.96468291457300026, 45.49948827470975488, 6.626685320826292802 ) ) ;
#15577 = LINE ( 'NONE', #8010, #56003 ) ;
#15579 = CARTESIAN_POINT ( 'NONE',  ( -84.74748497845986606, -18.65607540284239718, 153.2878044841931455 ) ) ;
#15580 = ORIENTED_EDGE ( 'NONE', *, *, #12428, .F. ) ;
#15581 = ORIENTED_EDGE ( 'NONE', *, *, #35753, .F. ) ;
#15582 = ORIENTED_EDGE ( 'NONE', *, *, #29535, .F. ) ;
#15583 = CARTESIAN_POINT ( 'NONE',  ( -8.786988139152953468E-15, 18.64300841652315910, 38.36521369532682257 ) ) ;
#15584 = ADVANCED_FACE ( 'NONE', ( #21713 ), #4433, .T. ) ;
#15585 = CARTESIAN_POINT ( 'NONE',  ( -4.999999999999997335, -12.50629439490131389, 11.30430831583516316 ) ) ;
#15586 = ORIENTED_EDGE ( 'NONE', *, *, #34881, .T. ) ;
#15587 = CARTESIAN_POINT ( 'NONE',  ( -42.29361012144100584, 486.6953289214003462, 8.720858923702914822 ) ) ;
#15588 = CARTESIAN_POINT ( 'NONE',  ( -0.000000000000000000, 34.25047185182970111, -44.13186320217320713 ) ) ;
#15589 = CARTESIAN_POINT ( 'NONE',  ( -10.00000000000000000, 15.00000000000000178, -3.082707893549292422 ) ) ;
#15590 = CARTESIAN_POINT ( 'NONE',  ( -99.73481241717010448, -57.62673548571369508, 203.9935789388791250 ) ) ;
#15591 = CARTESIAN_POINT ( 'NONE',  ( -4.658465013329191606, -66.32363879673093265, 3.783534922165390668 ) ) ;
#15592 = CARTESIAN_POINT ( 'NONE',  ( 0.000000000000000000, 0.000000000000000000, -13.00000000000000000 ) ) ;
#15593 = DIRECTION ( 'NONE',  ( 0.1108331996454379326, -0.9715652913456128692, -0.2092292678113387983 ) ) ;
#15594 = CARTESIAN_POINT ( 'NONE',  ( 0.7060372491531136108, 15.23416508906601230, -9.999999999999998224 ) ) ;
#15595 = CARTESIAN_POINT ( 'NONE',  ( -8.309739744518550353, -29.99999999999999289, -39.88085837097889197 ) ) ;
#15596 = ADVANCED_FACE ( 'NONE', ( #78845 ), #79903, .F. ) ;
#15597 = CARTESIAN_POINT ( 'NONE',  ( 6.800000000000000711, 6.123233995736767268E-16, -5.000000000000000888 ) ) ;
#15598 = CARTESIAN_POINT ( 'NONE',  ( -53.02381676432123214, -36.03889879312533395, 54.93151352944263266 ) ) ;
#15599 = DIRECTION ( 'NONE',  ( 0.5735764363510470476, -0.8191520442889911324, 1.003171929053524007E-16 ) ) ;
#15600 = ORIENTED_EDGE ( 'NONE', *, *, #87532, .T. ) ;
#15601 = CARTESIAN_POINT ( 'NONE',  ( -98.75596714119691910, -37.75931162163595900, 192.0729565296949772 ) ) ;
#15602 = CARTESIAN_POINT ( 'NONE',  ( -7.416584036551215675, 294.7171783682675255, -6.719350101469791170 ) ) ;
#15603 = ORIENTED_EDGE ( 'NONE', *, *, #710, .T. ) ;
#15604 = CARTESIAN_POINT ( 'NONE',  ( 42.48678019891497826, 465.9003906206858687, 13.75832259440545435 ) ) ;
#15605 = CARTESIAN_POINT ( 'NONE',  ( 85.34762539502915502, -38.35938083958861711, -22.54931118768901754 ) ) ;
#15606 = CARTESIAN_POINT ( 'NONE',  ( 0.000000000000000000, 43.50000000000000711, 0.000000000000000000 ) ) ;
#15607 = CARTESIAN_POINT ( 'NONE',  ( 25.21823338009918203, 1.482358050883964840E-15, 0.000000000000000000 ) ) ;
#15608 = EDGE_CURVE ( 'NONE', #12195, #83228, #5778, .T. ) ;
#15609 = EDGE_CURVE ( 'NONE', #19762, #104952, #12628, .T. ) ;
#15610 = FACE_OUTER_BOUND ( 'NONE', #14958, .T. ) ;
#15611 = CYLINDRICAL_SURFACE ( 'NONE', #29312, 3.400000000000000355 ) ;
#15612 = CARTESIAN_POINT ( 'NONE',  ( 85.25593731491920835, -30.00000000000000355, 172.6945922388917438 ) ) ;
#15613 = CARTESIAN_POINT ( 'NONE',  ( 37.02702338562992423, 490.9575081778457957, 12.45591594067282060 ) ) ;
#15614 = CARTESIAN_POINT ( 'NONE',  ( -29.33080127677455096, 13.52978328598925906, 39.65469037846435896 ) ) ;
#15615 = CARTESIAN_POINT ( 'NONE',  ( -6.818286579240214529, 1.325012739682868590, -6.208253321455268647 ) ) ;
#15616 = AXIS2_PLACEMENT_3D ( 'NONE', #50620, #81933, #106747 ) ;
#15617 = AXIS2_PLACEMENT_3D ( 'NONE', #57398, #73581, #90313 ) ;
#15618 = ORIENTED_EDGE ( 'NONE', *, *, #78564, .T. ) ;
#15619 = ORIENTED_EDGE ( 'NONE', *, *, #16038, .F. ) ;
#15620 = CARTESIAN_POINT ( 'NONE',  ( 50.44857603004569313, -29.12119561422500524, 47.99944827896294441 ) ) ;
#15621 = CARTESIAN_POINT ( 'NONE',  ( -3.397168681869905615, 299.9648137111082633, -10.00714490978890758 ) ) ;
#15622 = CARTESIAN_POINT ( 'NONE',  ( 36.45652548590511799, 28.06682613793154957, -12.78635007879563190 ) ) ;
#15623 = ORIENTED_EDGE ( 'NONE', *, *, #49682, .T. ) ;
#15624 = CARTESIAN_POINT ( 'NONE',  ( -108.1290187186095437, -38.35627294540438470, 138.7757913829071299 ) ) ;
#15625 = VERTEX_POINT ( 'NONE', #13574 ) ;
#15626 = CARTESIAN_POINT ( 'NONE',  ( 1.347111479062088207E-15, -1.734723475976807094E-15, 100.9999999999999858 ) ) ;
#15627 = CARTESIAN_POINT ( 'NONE',  ( 90.86461683327247840, -38.35179314048024679, 20.70149138315537840 ) ) ;
#15628 = CARTESIAN_POINT ( 'NONE',  ( 12.69532080757137926, 18.64199302928275159, -8.260889120040829425 ) ) ;
#15629 = CARTESIAN_POINT ( 'NONE',  ( 101.9339513551239378, -37.84836680173732759, 156.3405949689792749 ) ) ;
#15630 = CARTESIAN_POINT ( 'NONE',  ( -32.15310320217081141, 439.7024266304582625, 23.94087012106557566 ) ) ;
#15631 = CARTESIAN_POINT ( 'NONE',  ( 22.19982010036187603, 28.18804608458829719, 31.21118039878576411 ) ) ;
#15632 = CARTESIAN_POINT ( 'NONE',  ( -28.09654795190569132, 307.1907278677510931, -9.251968270002775441 ) ) ;
#15633 = CARTESIAN_POINT ( 'NONE',  ( 4.971339166421698152, -62.51181963379390538, 12.85213906502154835 ) ) ;
#15634 = CARTESIAN_POINT ( 'NONE',  ( 77.82654327636778646, -60.00000000000000000, 192.4673928146949891 ) ) ;
#15635 = CIRCLE ( 'NONE', #31234, 4.000000000000001776 ) ;
#15636 = CARTESIAN_POINT ( 'NONE',  ( -43.11534632275854761, 435.4435433140274654, 9.329549855370874667 ) ) ;
#15637 = ORIENTED_EDGE ( 'NONE', *, *, #67931, .F. ) ;
#15638 = CARTESIAN_POINT ( 'NONE',  ( 57.84234124985879788, -46.43614486156029386, 69.91354623974028470 ) ) ;
#15639 = CARTESIAN_POINT ( 'NONE',  ( -22.52158133765707149, 295.0395296717392739, -9.960097416559106520 ) ) ;
#15641 = ADVANCED_FACE ( 'NONE', ( #95061 ), #96107, .F. ) ;
#15640 = B_SPLINE_CURVE_WITH_KNOTS ( 'NONE', 3,
 ( #77882, #85443, #36921, #61173, #94059, #54106 ),
 .UNSPECIFIED., .F., .F.,
 ( 4, 2, 4 ),
 ( 0.02044294606936548214, 0.03157470899999220704, 0.04270647193061893887 ),
 .UNSPECIFIED. ) ;
#15642 = CARTESIAN_POINT ( 'NONE',  ( 9.996020202094923590, -50.00033894567218340, 27.38654800878193996 ) ) ;
#15643 = DIRECTION ( 'NONE',  ( 0.000000000000000000, -1.000000000000000000, 0.000000000000000000 ) ) ;
#15644 = ORIENTED_EDGE ( 'NONE', *, *, #55924, .T. ) ;
#15645 = AXIS2_PLACEMENT_3D ( 'NONE', #50685, #16216, #58272 ) ;
#15647 = CARTESIAN_POINT ( 'NONE',  ( -14.29190075645675861, 21.26710225494873185, 5.626279437267716510 ) ) ;
#15646 = CARTESIAN_POINT ( 'NONE',  ( -73.36661343314580108, -29.99999999991936761, 145.3711930596387845 ) ) ;
#15648 = DIRECTION ( 'NONE',  ( 0.000000000000000000, 0.000000000000000000, 1.000000000000000000 ) ) ;
#15649 = DIRECTION ( 'NONE',  ( 0.000000000000000000, 0.000000000000000000, 1.000000000000000000 ) ) ;
#15650 = DIRECTION ( 'NONE',  ( -1.000000000000000000, -1.224606353822377258E-16, -0.000000000000000000 ) ) ;
#15651 = CARTESIAN_POINT ( 'NONE',  ( 5.656854249492380582, -31.81249999999999289, -5.656854249492379694 ) ) ;
#15652 = EDGE_CURVE ( 'NONE', #73667, #22177, #36846, .T. ) ;
#15653 = AXIS2_PLACEMENT_3D ( 'NONE', #88503, #57691, #48547 ) ;
#15654 = DIRECTION ( 'NONE',  ( -1.000000000000000000, -1.224606353822377258E-16, -0.000000000000000000 ) ) ;
#15655 = VERTEX_POINT ( 'NONE', #86969 ) ;
#15656 = CARTESIAN_POINT ( 'NONE',  ( 84.42314394957541879, -32.44248152629501902, 172.3652158902926601 ) ) ;
#15657 = CARTESIAN_POINT ( 'NONE',  ( 30.00000000000000000, 488.8442721620239126, 4.433647275927487641 ) ) ;
#15658 = CARTESIAN_POINT ( 'NONE',  ( -5.656854249492381470, -8.750000004096769146, 5.656854249492379694 ) ) ;
#15659 = ORIENTED_EDGE ( 'NONE', *, *, #92637, .T. ) ;
#15660 = CARTESIAN_POINT ( 'NONE',  ( -4.165977904505308693, 16.00000000000000000, -9.090909090909089940 ) ) ;
#15661 = CARTESIAN_POINT ( 'NONE',  ( 7.417322861520009525, -4.999999999978371079, -16.62528780688618824 ) ) ;
#15662 = CARTESIAN_POINT ( 'NONE',  ( 25.89149878171548380, 35.08194043918889804, -8.495905954776644009 ) ) ;
#15663 = FACE_OUTER_BOUND ( 'NONE', #81796, .T. ) ;
#15664 = PRESENTATION_STYLE_ASSIGNMENT (( #16735 ) ) ;
#15665 = DIRECTION ( 'NONE',  ( -1.000000000000000000, -0.000000000000000000, -0.000000000000000000 ) ) ;
#15666 = EDGE_CURVE ( 'NONE', #104078, #41373, #19194, .T. ) ;
#15667 = ORIENTED_EDGE ( 'NONE', *, *, #44202, .T. ) ;
#15668 = SURFACE_SIDE_STYLE ('',( #48025 ) ) ;
#15669 = AXIS2_PLACEMENT_3D ( 'NONE', #98729, #24885, #72864 ) ;
#15670 = CIRCLE ( 'NONE', #44965, 4.172000000000001485 ) ;
#15671 = LINE ( 'NONE', #89041, #16917 ) ;
#15672 = FILL_AREA_STYLE ('',( #80400 ) ) ;
#15674 = CARTESIAN_POINT ( 'NONE',  ( -10.03715289824008750, 13.99183644020731343, -10.50945001292772929 ) ) ;
#15673 = CARTESIAN_POINT ( 'NONE',  ( -24.75015538639915746, -28.86932137373848661, 38.18840044054004323 ) ) ;
#15675 = AXIS2_PLACEMENT_3D ( 'NONE', #75334, #1976, #34923 ) ;
#15676 = CARTESIAN_POINT ( 'NONE',  ( 2.977408999572650927, -12.87500000204838280, -7.188101187500001821 ) ) ;
#15677 = CARTESIAN_POINT ( 'NONE',  ( 18.69662128202880069, 302.6591720840974062, -10.04079946497810383 ) ) ;
#15678 = DIRECTION ( 'NONE',  ( -0.000000000000000000, 1.000000000000000000, 0.000000000000000000 ) ) ;
#15679 = EDGE_LOOP ( 'NONE', ( #28655, #95189, #103443, #49460 ) ) ;
#15680 = CARTESIAN_POINT ( 'NONE',  ( -17.50000000000013500, 50.00117660290769805, 59.93398959461790554 ) ) ;
#15681 = CARTESIAN_POINT ( 'NONE',  ( 0.000000000000000000, 0.000000000000000000, -13.00000000000000000 ) ) ;
#15682 = CARTESIAN_POINT ( 'NONE',  ( 0.000000000000000000, -4.000000000000003553, 112.0000000000000000 ) ) ;
#15683 = CARTESIAN_POINT ( 'NONE',  ( 86.17777777777776294, 1.023464760207051730E-14, 0.000000000000000000 ) ) ;
#15684 = LINE ( 'NONE', #96622, #5269 ) ;
#15685 = AXIS2_PLACEMENT_3D ( 'NONE', #71601, #48386, #65111 ) ;
#15686 = ORIENTED_EDGE ( 'NONE', *, *, #100790, .T. ) ;
#15687 = B_SPLINE_CURVE_WITH_KNOTS ( 'NONE', 3,
 ( #99256, #27029, #82566, #8670, #59912, #84168 ),
 .UNSPECIFIED., .F., .F.,
 ( 4, 2, 4 ),
 ( 0.000000000000000000, 0.001995463903526787514, 0.003990927807053575027 ),
 .UNSPECIFIED. ) ;
#15688 = DIRECTION ( 'NONE',  ( 0.000000000000000000, 0.000000000000000000, 1.000000000000000000 ) ) ;
#15689 = DIRECTION ( 'NONE',  ( 0.000000000000000000, -1.000000000000000000, 0.000000000000000000 ) ) ;
#15690 = ORIENTED_EDGE ( 'NONE', *, *, #47700, .T. ) ;
#15691 =( BOUNDED_SURFACE ( )  B_SPLINE_SURFACE ( 3, 2, ( 
 ( #47839, #8457, #48900 ),
 ( #6861, #97457, #41357 ),
 ( #74251, #14946, #58066 ),
 ( #98001, #25212, #89396 ),
 ( #89913, #82349, #81795 ),
 ( #7920, #15490, #327 ),
 ( #24154, #90989, #23614 ),
 ( #33291, #40824, #66162 ),
 ( #81272, #7384, #57525 ),
 ( #99044, #33831, #17100 ),
 ( #73716, #49976, #82884 ),
 ( #106076, #106619, #41886 ) ),
 .UNSPECIFIED., .F., .F., .F. ) 
 B_SPLINE_SURFACE_WITH_KNOTS ( ( 4, 2, 2, 2, 2, 4 ),
 ( 3, 3 ),
 ( 1.734723475976807094E-18, 0.001187588843296134801, 0.001781383264944201225, 0.002375177686592267867, 0.003562766529888400716, 0.004750355373184533998 ),
 ( 0.000000000000000000, 1.000000000000000000 ),
 .UNSPECIFIED. ) 
 GEOMETRIC_REPRESENTATION_ITEM ( )  RATIONAL_B_SPLINE_SURFACE ( (
 ( 1.000000000000000000, 0.9359444767143318966, 1.000000000000000000),
 ( 1.000000000000000000, 0.9295581727144621720, 1.000000000000000000),
 ( 1.000000000000000000, 0.9234593375674586824, 1.000000000000000000),
 ( 1.000000000000000000, 0.9150808072273581839, 1.000000000000000000),
 ( 1.000000000000000000, 0.9124161408737813117, 1.000000000000000000),
 ( 1.000000000000000000, 0.9074047588826391619, 1.000000000000000000),
 ( 1.000000000000000000, 0.9050663310860130872, 1.000000000000000000),
 ( 1.000000000000000000, 0.8987692007139450601, 1.000000000000000000),
 ( 1.000000000000000000, 0.8954627112850828130, 1.000000000000000000),
 ( 1.000000000000000000, 0.8909338199771041911, 1.000000000000000000),
 ( 1.000000000000000000, 0.8897377579433939365, 1.000000000000000000),
 ( 1.000000000000000000, 0.8897565210026093796, 1.000000000000000000) ) ) 
 REPRESENTATION_ITEM ( '' )  SURFACE ( )  );
#15692 = SURFACE_STYLE_FILL_AREA ( #89599 ) ;
#15693 = LINE ( 'NONE', #41569, #17512 ) ;
#15694 = CARTESIAN_POINT ( 'NONE',  ( 16.14595037822608603, 7.274337365584590209, -6.616591826375515240 ) ) ;
#15695 = UNCERTAINTY_MEASURE_WITH_UNIT (LENGTH_MEASURE( 1.000000000000000082E-05 ), #8663, 'distance_accuracy_value', 'NONE');
#15696 = CARTESIAN_POINT ( 'NONE',  ( -112.2059321623641495, -60.00000000000000000, 170.3870518237542342 ) ) ;
#15697 = CARTESIAN_POINT ( 'NONE',  ( 28.73029465396662374, 18.79238081053093623, -40.04376963015472057 ) ) ;
#15698 = CARTESIAN_POINT ( 'NONE',  ( -21.51569398614863715, 294.9107018935607130, -9.987480606144508499 ) ) ;
#15699 = CARTESIAN_POINT ( 'NONE',  ( 53.78349330513380266, 6.975173280561618775E-15, 0.000000000000000000 ) ) ;
#15700 = CARTESIAN_POINT ( 'NONE',  ( -32.85880617213487653, 464.9534634096118566, 11.16102948071628198 ) ) ;
#15701 =( BOUNDED_SURFACE ( )  B_SPLINE_SURFACE ( 3, 2, ( 
 ( #100673, #67785, #33311 ),
 ( #26836, #50515, #58082 ),
 ( #66723, #99062, #74793 ),
 ( #17652, #83962, #83428 ),
 ( #16574, #59708, #92584 ),
 ( #8472, #9525, #74268 ),
 ( #10072, #75327, #34919 ),
 ( #42983, #76392, #49996 ),
 ( #26311, #82903, #27375 ),
 ( #41906, #17119, #101218 ),
 ( #18189, #9000, #49457 ),
 ( #1429, #18739, #51046 ),
 ( #34390, #41377, #84507 ),
 ( #1968, #873, #10596 ),
 ( #91011, #2505, #35452 ),
 ( #99605, #25781, #68324 ),
 ( #60255, #82367, #343 ),
 ( #66183, #25228, #31153 ),
 ( #62965, #105532, #64040 ),
 ( #62438, #97425, #96918 ),
 ( #6832, #79134, #88823 ),
 ( #80715, #14381, #71045 ),
 ( #13856, #7357, #63503 ),
 ( #96402, #79666, #95329 ),
 ( #39751, #72630, #54300 ),
 ( #22534, #95865, #87244 ),
 ( #5774, #103937, #30617 ),
 ( #14918, #47287, #55376 ),
 ( #31673, #56432, #23050 ),
 ( #46247, #64556, #30080 ),
 ( #5259, #38697, #89365 ),
 ( #23586, #88305, #15454 ),
 ( #38186, #21462, #48347 ),
 ( #80186, #6291, #81240 ),
 ( #40268, #13324, #55888 ),
 ( #105011, #73142, #71563 ),
 ( #106046, #47810, #46769 ),
 ( #104469, #21993, #54846 ),
 ( #87775, #39230, #72105 ),
 ( #83382, #83916, #32741 ),
 ( #49948, #89885, #73689 ),
 ( #56969, #65610, #75283 ),
 ( #10027, #32199, #67220 ),
 ( #9478, #42390, #48874 ),
 ( #1379, #66136, #106591 ),
 ( #49414, #7888, #90420 ),
 ( #33264, #99557, #99015 ),
 ( #65075, #34347, #100096 ),
 ( #24124, #25180, #58038 ),
 ( #15995, #26264, #82317 ),
 ( #16523, #75825, #50470 ),
 ( #66676, #59126, #92008 ) ),
 .UNSPECIFIED., .F., .F., .F. ) 
 B_SPLINE_SURFACE_WITH_KNOTS ( ( 4, 2, 2, 2, 2, 2, 2, 2, 2, 2, 2, 2, 2, 2, 2, 2, 2, 2, 2, 2, 2, 2, 2, 2, 2, 4 ),
 ( 3, 3 ),
 ( 0.05020300464300656018, 0.05910007010879590045, 0.06799713557458524071, 0.08579126650616392125, 0.1035853974377426157, 0.1213795283693212962, 0.1391736593008999767, 0.1480707247666893100, 0.1569677902324786711, 0.1614163229653733378, 0.1658648556982680322, 0.1703133884311626989, 0.1747619211640573655, 0.1792104538969520322, 0.1814347202633993517, 0.1836589866298466989, 0.1847711198130703725, 0.1858832529962940461, 0.1869953861795177197, 0.1881075193627413655, 0.1886635859543531746, 0.1892196525459650114, 0.1897757191375768482, 0.1903317857291886850, 0.1914439189124123586, 0.1925560520956360322 ),
 ( 0.000000000000000000, 1.000000000000000000 ),
 .UNSPECIFIED. ) 
 GEOMETRIC_REPRESENTATION_ITEM ( )  RATIONAL_B_SPLINE_SURFACE ( (
 ( 1.000000000000000000, 0.7071068713987338494, 1.000000000000000000),
 ( 1.000000000000000000, 0.7071068931945895253, 1.000000000000000000),
 ( 1.000000000000000000, 0.7071068799682457273, 1.000000000000000000),
 ( 1.000000000000000000, 0.7071068179960090516, 1.000000000000000000),
 ( 1.000000000000000000, 0.7071067808170531377, 1.000000000000000000),
 ( 1.000000000000000000, 0.7071067808170531377, 1.000000000000000000),
 ( 1.000000000000000000, 0.7071067795768681830, 1.000000000000000000),
 ( 1.000000000000000000, 0.7071067795768681830, 1.000000000000000000),
 ( 1.000000000000000000, 0.7071059205153482630, 1.000000000000000000),
 ( 1.000000000000000000, 0.7071040215992112632, 1.000000000000000000),
 ( 1.000000000000000000, 0.7071071097139771666, 1.000000000000000000),
 ( 1.000000000000000000, 0.7071064172135144155, 1.000000000000000000),
 ( 1.000000000000000000, 0.7071032627269669968, 1.000000000000000000),
 ( 1.000000000000000000, 0.7071054807186710756, 1.000000000000000000),
 ( 1.000000000000000000, 0.7071073488286629960, 1.000000000000000000),
 ( 1.000000000000000000, 0.7071060878131381067, 1.000000000000000000),
 ( 1.000000000000000000, 0.7071042701205316749, 1.000000000000000000),
 ( 1.000000000000000000, 0.7071061885472514907, 1.000000000000000000),
 ( 1.000000000000000000, 0.7071092460169422500, 1.000000000000000000),
 ( 1.000000000000000000, 0.7071028304568526268, 1.000000000000000000),
 ( 1.000000000000000000, 0.7070913726372183294, 1.000000000000000000),
 ( 1.000000000000000000, 0.7070821465654113513, 1.000000000000000000),
 ( 1.000000000000000000, 0.7070849791653976979, 1.000000000000000000),
 ( 1.000000000000000000, 0.7071006344750183636, 1.000000000000000000),
 ( 1.000000000000000000, 0.7071084549986811352, 1.000000000000000000),
 ( 1.000000000000000000, 0.7071012737890344235, 1.000000000000000000),
 ( 1.000000000000000000, 0.7071050044716787886, 1.000000000000000000),
 ( 1.000000000000000000, 0.7071073700438799126, 1.000000000000000000),
 ( 1.000000000000000000, 0.7070678821743980880, 1.000000000000000000),
 ( 1.000000000000000000, 0.7070089177333229724, 1.000000000000000000),
 ( 1.000000000000000000, 0.7070191433436773254, 1.000000000000000000),
 ( 1.000000000000000000, 0.7070838732338704524, 1.000000000000000000),
 ( 1.000000000000000000, 0.7071074894229318897, 1.000000000000000000),
 ( 1.000000000000000000, 0.7071058915519934374, 1.000000000000000000),
 ( 1.000000000000000000, 0.7071009288909754220, 1.000000000000000000),
 ( 1.000000000000000000, 0.7071026537070833617, 1.000000000000000000),
 ( 1.000000000000000000, 0.7071047596603757812, 1.000000000000000000),
 ( 1.000000000000000000, 0.7071143613427882668, 1.000000000000000000),
 ( 1.000000000000000000, 0.7071126439119755913, 1.000000000000000000),
 ( 1.000000000000000000, 0.7071061363862406468, 1.000000000000000000),
 ( 1.000000000000000000, 0.7071052386115821431, 1.000000000000000000),
 ( 1.000000000000000000, 0.7070937592812094330, 1.000000000000000000),
 ( 1.000000000000000000, 0.7070897429712678095, 1.000000000000000000),
 ( 1.000000000000000000, 0.7070917291181727515, 1.000000000000000000),
 ( 1.000000000000000000, 0.7070968323554049917, 1.000000000000000000),
 ( 1.000000000000000000, 0.7071053620208651580, 1.000000000000000000),
 ( 1.000000000000000000, 0.7071090935628171481, 1.000000000000000000),
 ( 1.000000000000000000, 0.7070966954647354141, 1.000000000000000000),
 ( 1.000000000000000000, 0.7070788515582973055, 1.000000000000000000),
 ( 1.000000000000000000, 0.7070871700188539055, 1.000000000000000000),
 ( 1.000000000000000000, 0.7071059307897505919, 1.000000000000000000),
 ( 1.000000000000000000, 0.7071067811865311414, 1.000000000000000000) ) ) 
 REPRESENTATION_ITEM ( '' )  SURFACE ( )  );
#15703 = CARTESIAN_POINT ( 'NONE',  ( -15.47206823513576524, 2.694788529767829122, 1.611870258443510728 ) ) ;
#15702 = CARTESIAN_POINT ( 'NONE',  ( 6.145467200820721843, -5.000000000000002665, -77.00333157708637088 ) ) ;
#15704 = CARTESIAN_POINT ( 'NONE',  ( -84.63106176657737478, -32.40589074336656950, 174.3468092685627369 ) ) ;
#15705 = ORIENTED_EDGE ( 'NONE', *, *, #99020, .F. ) ;
#15706 = FILL_AREA_STYLE_COLOUR ( '', #53894 ) ;
#15707 = STYLED_ITEM ( 'NONE', ( #5495 ), #7868 ) ;
#15708 = TOROIDAL_SURFACE ( 'NONE', #21009, 9.000000000000000000, 0.5000000000000000000 ) ;
#15709 = EDGE_LOOP ( 'NONE', ( #64348, #35106 ) ) ;
#15710 = CIRCLE ( 'NONE', #36415, 5.400000000000001243 ) ;
#15711 = ORIENTED_EDGE ( 'NONE', *, *, #105237, .T. ) ;
#15712 = CARTESIAN_POINT ( 'NONE',  ( 26.84999999999999787, 1.533819458162526451E-15, 0.000000000000000000 ) ) ;
#15713 = EDGE_CURVE ( 'NONE', #89211, #59582, #52899, .T. ) ;
#15714 = B_SPLINE_CURVE_WITH_KNOTS ( 'NONE', 3,
 ( #17736, #13736, #38070, #87126, #13203, #38577, #59796, #26922, #92672, #93747, #36083, #79018, #95737, #47165 ),
 .UNSPECIFIED., .F., .F.,
 ( 4, 2, 2, 2, 2, 2, 4 ),
 ( 1.430489624538199204E-17, 0.0002431197374324345079, 0.0004862394748648547044, 0.0007293592122972748738, 0.0009724789497296950974, 0.001458718424594527630, 0.001944957899459360271 ),
 .UNSPECIFIED. ) ;
#15715 = STYLED_ITEM ( 'NONE', ( #95969 ), #79708 ) ;
#15716 = CARTESIAN_POINT ( 'NONE',  ( 35.59999999999999432, 1.533819458162526451E-15, 0.000000000000000000 ) ) ;
#15717 = CARTESIAN_POINT ( 'NONE',  ( -14.29190075645222180, 6.456385560667815326, -7.561819230143193238 ) ) ;
#15718 = CARTESIAN_POINT ( 'NONE',  ( 3.591939471458723609, 23.61027659479541896, -5.000000000000000000 ) ) ;
#15719 = CARTESIAN_POINT ( 'NONE',  ( -10.50000000000000711, -5.000000000000000000, -77.33514508527181874 ) ) ;
#15720 = CARTESIAN_POINT ( 'NONE',  ( -44.08840282922863452, 485.7747746244176597, 4.178803824087133911 ) ) ;
#15721 = AXIS2_PLACEMENT_3D ( 'NONE', #54304, #12274, #60853 ) ;
#15722 = CARTESIAN_POINT ( 'NONE',  ( 105.8603286302927984, -14.21045842199436571, 153.6005582235227678 ) ) ;
#15723 = EDGE_CURVE ( 'NONE', #9744, #76326, #106228, .T. ) ;
#15724 = CARTESIAN_POINT ( 'NONE',  ( -109.1953414053527780, -30.00000000000001066, 161.8807222540328894 ) ) ;
#15725 = CARTESIAN_POINT ( 'NONE',  ( -63.35317981673050980, -39.48581946695038170, 81.40797789241049998 ) ) ;
#15726 = ORIENTED_EDGE ( 'NONE', *, *, #31715, .T. ) ;
#15727 = CARTESIAN_POINT ( 'NONE',  ( -59.20842685209844092, 38.95251792617707309, 23.59073220948269878 ) ) ;
#15728 = CARTESIAN_POINT ( 'NONE',  ( 110.4834380140601695, -59.99999999996104805, 129.5980811341964056 ) ) ;
#15729 = B_SPLINE_CURVE_WITH_KNOTS ( 'NONE', 3,
 ( #83474, #68914, #43558, #10639 ),
 .UNSPECIFIED., .F., .F.,
 ( 4, 4 ),
 ( 0.000000000000000000, 0.1960348326659903384 ),
 .UNSPECIFIED. ) ;
#15730 = ORIENTED_EDGE ( 'NONE', *, *, #70013, .T. ) ;
#15731 = CARTESIAN_POINT ( 'NONE',  ( 0.000000000000000000, 0.000000000000000000, 0.000000000000000000 ) ) ;
#15732 = CARTESIAN_POINT ( 'NONE',  ( 7.188101187500000044, -13.53125000204838457, 0.000000000000000000 ) ) ;
#15733 = CARTESIAN_POINT ( 'NONE',  ( -5.621309607737247305, 52.00056912798299180, 6.031152949374553707 ) ) ;
#15734 = ORIENTED_EDGE ( 'NONE', *, *, #86746, .T. ) ;
#15735 = CARTESIAN_POINT ( 'NONE',  ( -5.000000000000002665, 152.0000000000000000, 5.000000000000000000 ) ) ;
#15736 = ORIENTED_EDGE ( 'NONE', *, *, #98301, .T. ) ;
#15737 = DIRECTION ( 'NONE',  ( -1.000000000000000000, -0.000000000000000000, -0.000000000000000000 ) ) ;
#15738 = CARTESIAN_POINT ( 'NONE',  ( -7.894787914004607998, 0.7647108141804102033, -7.591390474663421983 ) ) ;
#15739 = CARTESIAN_POINT ( 'NONE',  ( -97.18990194766369939, -60.00000000000000000, 63.92461308931969910 ) ) ;
#15740 =( LENGTH_UNIT ( ) NAMED_UNIT ( * ) SI_UNIT ( .MILLI., .METRE. ) );
#15741 = CARTESIAN_POINT ( 'NONE',  ( -7.188101187500001821, -29.37500000204838457, -2.977408999572651371 ) ) ;
#15742 = ADVANCED_FACE ( 'NONE', ( #8141 ), #23667, .F. ) ;
#15743 = DIRECTION ( 'NONE',  ( 0.000000000000000000, 1.000000000000000000, 0.000000000000000000 ) ) ;
#15744 = CARTESIAN_POINT ( 'NONE',  ( -6.273349488839427224, 53.84215621584975509, -6.493349957603958167 ) ) ;
#15745 = CARTESIAN_POINT ( 'NONE',  ( -10.96784672161025753, -4.990140223832483457, -12.57412324632270284 ) ) ;
#15746 = CARTESIAN_POINT ( 'NONE',  ( 32.17646412119353272, 464.6980787822282082, 10.84896803613062666 ) ) ;
#15747 = CARTESIAN_POINT ( 'NONE',  ( 12.22086015683302129, -5.459618031741397814, 20.16641550308944630 ) ) ;
#15748 = CARTESIAN_POINT ( 'NONE',  ( -33.20189241797189794, 300.3220019530701848, -0.7726951009200400122 ) ) ;
#15749 = CARTESIAN_POINT ( 'NONE',  ( 106.4731662889862349, -60.00000000000002132, 174.0751867897438103 ) ) ;
#15750 = CARTESIAN_POINT ( 'NONE',  ( -31.12606138324045446, -18.66557501722132528, 29.72691873377532445 ) ) ;
#15751 =( GEOMETRIC_REPRESENTATION_CONTEXT ( 3 ) GLOBAL_UNCERTAINTY_ASSIGNED_CONTEXT ( ( #106555 ) ) GLOBAL_UNIT_ASSIGNED_CONTEXT ( ( #76735, #27713, #60588 ) ) REPRESENTATION_CONTEXT ( 'NONE', 'WORKASPACE' ) );
#15752 =( LENGTH_UNIT ( ) NAMED_UNIT ( * ) SI_UNIT ( .MILLI., .METRE. ) );
#15753 = CARTESIAN_POINT ( 'NONE',  ( 41.03672742457499822, -60.25176818595546280, 44.31207356424504695 ) ) ;
#15754 = MECHANICAL_DESIGN_GEOMETRIC_PRESENTATION_REPRESENTATION (  '', ( #74333 ), #38199 ) ;
#15755 = DIRECTION ( 'NONE',  ( -0.000000000000000000, 1.000000000000000000, -0.000000000000000000 ) ) ;
#15756 = ORIENTED_EDGE ( 'NONE', *, *, #2506, .F. ) ;
#15757 = CARTESIAN_POINT ( 'NONE',  ( -7.619701877737480977, 88.17442159532770063, -2.447562251315978710 ) ) ;
#15758 = CIRCLE ( 'NONE', #242, 2.999999999999996447 ) ;
#15759 = CARTESIAN_POINT ( 'NONE',  ( -74.04571983938727442, -38.32706951796213701, 160.7403410287773227 ) ) ;
#15760 = ORIENTED_EDGE ( 'NONE', *, *, #78358, .F. ) ;
#15762 = CARTESIAN_POINT ( 'NONE',  ( 43.29658055318886767, 324.1952503670673877, -2.852919881210743913 ) ) ;
#15761 = CARTESIAN_POINT ( 'NONE',  ( 43.00000000000000000, 450.0000000000002274, 13.20242257375370976 ) ) ;
#15763 = FACE_BOUND ( 'NONE', #39524, .T. ) ;
#15764 = CARTESIAN_POINT ( 'NONE',  ( -7.150000055923752207, 41.64999994407625650, -59.82695526654634222 ) ) ;
#15765 = CARTESIAN_POINT ( 'NONE',  ( 1.006201139504063979, 43.34891076668851184, -18.24605675915023184 ) ) ;
#15766 = DIRECTION ( 'NONE',  ( -1.000000000000000000, -1.224606353822377258E-16, -0.000000000000000000 ) ) ;
#15767 = DIRECTION ( 'NONE',  ( -1.000000000000000000, -0.000000000000000000, -0.000000000000000000 ) ) ;
#15768 = CARTESIAN_POINT ( 'NONE',  ( -8.000000000000000000, -25.53125000409676915, -3.313708498984762496 ) ) ;
#15769 = CARTESIAN_POINT ( 'NONE',  ( 100.7796288034784169, -60.00000000000002132, 85.60714601047209271 ) ) ;
#15770 = B_SPLINE_CURVE_WITH_KNOTS ( 'NONE', 3,
 ( #30384, #63273, #96171, #55147, #88077, #14155, #47059, #79959, #6071, #55663, #88600, #47588, #90189, #599, #43237, #34117, #82629, #58901, #58351, #41639, #9253, #33564, #49721, #75595, #16291, #99320 ),
 .UNSPECIFIED., .F., .F.,
 ( 4, 2, 2, 2, 2, 2, 2, 2, 2, 2, 2, 2, 4 ),
 ( 0.003090333073482953025, 0.003342552850341273894, 0.003594772627199594763, 0.003846992404057915631, 0.004099212180916236500, 0.004603651734632870432, 0.004855871511491187398, 0.005108091288349503496, 0.006116970395782786105, 0.006369190172641096999, 0.006621409949499407893, 0.006873629726357717920, 0.007125849503216027947 ),
 .UNSPECIFIED. ) ;
#15771 = CARTESIAN_POINT ( 'NONE',  ( 40.92692307692308162, 1.411358822780289120E-15, 0.000000000000000000 ) ) ;
#15772 = DIRECTION ( 'NONE',  ( 1.000000000000000000, 1.224606353822377258E-16, 0.000000000000000000 ) ) ;
#15773 = CARTESIAN_POINT ( 'NONE',  ( 4.205882352941182845, -5.000000000000000000, -72.69916451482998809 ) ) ;
#15774 = ORIENTED_EDGE ( 'NONE', *, *, #24625, .T. ) ;
#15775 = EDGE_CURVE ( 'NONE', #86058, #36198, #44283, .T. ) ;
#15776 = CARTESIAN_POINT ( 'NONE',  ( -90.13898955460108198, -29.99999999999991473, 189.9826003834946562 ) ) ;
#15777 = ORIENTED_EDGE ( 'NONE', *, *, #92646, .T. ) ;
#15778 = CARTESIAN_POINT ( 'NONE',  ( 0.000000000000000000, 0.000000000000000000, 4.000000000000000000 ) ) ;
#15779 = CARTESIAN_POINT ( 'NONE',  ( -15.91668924485766112, 3.370617522767656027, 2.350968163848803361 ) ) ;
#15780 = CARTESIAN_POINT ( 'NONE',  ( 8.830611806799852914, 18.20472706776858018, 6.133090346964878919E-13 ) ) ;
#15781 = DIRECTION ( 'NONE',  ( -0.5735764363510461594, 0.8191520442889916875, 1.003171929053524870E-16 ) ) ;
#15782 = CARTESIAN_POINT ( 'NONE',  ( -22.46054152223504019, 27.61307239794276924, -32.95409374511062595 ) ) ;
#15783 = CARTESIAN_POINT ( 'NONE',  ( 5.082755093536325930, -26.84375000204838813, -5.082755093536325042 ) ) ;
#15784 = FACE_OUTER_BOUND ( 'NONE', #43769, .T. ) ;
#15786 = EDGE_CURVE ( 'NONE', #20310, #75040, #20239, .T. ) ;
#15785 = CARTESIAN_POINT ( 'NONE',  ( 7.204798266847586952, 41.05104862198670190, -70.50691143559862439 ) ) ;
#15787 = EDGE_CURVE ( 'NONE', #85444, #17070, #47396, .T. ) ;
#15788 = EDGE_LOOP ( 'NONE', ( #105525, #85735, #28213, #71402 ) ) ;
#15789 = B_SPLINE_CURVE_WITH_KNOTS ( 'NONE', 3,
 ( #91207, #48583, #80955, #9185 ),
 .UNSPECIFIED., .F., .F.,
 ( 4, 4 ),
 ( 0.000000000000000000, 1.000000000000000000 ),
 .UNSPECIFIED. ) ;
#15791 = ORIENTED_EDGE ( 'NONE', *, *, #34418, .T. ) ;
#15790 = CARTESIAN_POINT ( 'NONE',  ( 46.00000000000000000, 438.3878896346935790, 16.22878885428537998 ) ) ;
#15792 = CARTESIAN_POINT ( 'NONE',  ( 80.10507346880626756, -46.43520559967900851, 154.7484568511157477 ) ) ;
#15793 = DIRECTION ( 'NONE',  ( 0.000000000000000000, -1.000000000000000000, 0.000000000000000000 ) ) ;
#15794 = CARTESIAN_POINT ( 'NONE',  ( -38.64252647164300924, 27.44902043786143153, -11.54866764408293811 ) ) ;
#15795 = EDGE_LOOP ( 'NONE', ( #34786, #36071, #100139, #11003, #69701 ) ) ;
#15796 = CARTESIAN_POINT ( 'NONE',  ( -50.32426797222468196, 50.00000000000001421, 38.04620492663661935 ) ) ;
#15797 = CARTESIAN_POINT ( 'NONE',  ( 6.928203230275508773, -85.26883324508999351, -4.000000000000002665 ) ) ;
#15798 = CARTESIAN_POINT ( 'NONE',  ( -2.977408999572654480, -15.12500000204838457, 7.188101187499999156 ) ) ;
#15799 = CARTESIAN_POINT ( 'NONE',  ( 0.7145311798163234140, -9.237604307034013473, 6.198474679904167468E-16 ) ) ;
#15800 = VECTOR ( 'NONE', #90209, 1000.000000000000000 ) ;
#15801 = EDGE_CURVE ( 'NONE', #51255, #47192, #42570, .T. ) ;
#15802 = CARTESIAN_POINT ( 'NONE',  ( -68.42433815231228778, -57.68192485334662933, 143.8276693603407068 ) ) ;
#15803 = ADVANCED_FACE ( 'NONE', ( #65325 ), #97147, .T. ) ;
#15804 = ORIENTED_EDGE ( 'NONE', *, *, #71346, .T. ) ;
#15805 = CARTESIAN_POINT ( 'NONE',  ( 3.225563553360615288, 115.6469223491950515, 5.000000000000000000 ) ) ;
#15806 = CARTESIAN_POINT ( 'NONE',  ( 7.149999999999998579, 41.65000000000000568, -59.82695526683419729 ) ) ;
#15807 = ADVANCED_FACE ( 'NONE', ( #89076 ), #27899, .F. ) ;
#15808 = AXIS2_PLACEMENT_3D ( 'NONE', #62787, #88643, #95676 ) ;
#15809 = DIRECTION ( 'NONE',  ( 0.5735764363510462704, 0.8191520442889915765, 0.000000000000000000 ) ) ;
#15810 = EDGE_LOOP ( 'NONE', ( #4627, #61421, #45617, #56824 ) ) ;
#15811 = CARTESIAN_POINT ( 'NONE',  ( -5.082755093536325042, -30.59375000204838813, -5.082755093536325930 ) ) ;
#15812 = CARTESIAN_POINT ( 'NONE',  ( -29.12521271972553194, -21.25831152097612886, 32.00366296159075574 ) ) ;
#15813 = DIRECTION ( 'NONE',  ( 0.8191520442889974607, 1.003171929053531649E-16, -0.5735764363510379438 ) ) ;
#15814 = CARTESIAN_POINT ( 'NONE',  ( 1.122371673248518720, 51.93028698896991813, -8.361323773265381121 ) ) ;
#15815 = EDGE_CURVE ( 'NONE', #6164, #86885, #37470, .T. ) ;
#15816 = DIRECTION ( 'NONE',  ( -1.000000000000000000, -1.224606353822377258E-16, -0.000000000000000000 ) ) ;
#15817 = DIRECTION ( 'NONE',  ( 0.000000000000000000, 0.000000000000000000, 1.000000000000000000 ) ) ;
#15818 = APPLICATION_PROTOCOL_DEFINITION ( 'draft international standard', 'automotive_design', 1998, #39724 ) ;
#15819 = CARTESIAN_POINT ( 'NONE',  ( -9.644834624769977438, 33.00890500205773748, 2.648308524638411932 ) ) ;
#15820 = EDGE_LOOP ( 'NONE', ( #54504, #68732, #40707, #19834, #50586, #87715 ) ) ;
#15821 = CARTESIAN_POINT ( 'NONE',  ( 10.92528302346674351, 43.17643060797472998, 15.23541717086651559 ) ) ;
#15822 = CARTESIAN_POINT ( 'NONE',  ( -2.802461721337177636, 15.83563386295778308, 9.606080321247327802 ) ) ;
#15823 = DIRECTION ( 'NONE',  ( -1.000000000000000000, -0.000000000000000000, -0.000000000000000000 ) ) ;
#15824 = CARTESIAN_POINT ( 'NONE',  ( -59.10698846045011834, -30.00000000000000000, 64.79178358224362455 ) ) ;
#15825 = SURFACE_STYLE_USAGE ( .BOTH. , #31514 ) ;
#15826 = CIRCLE ( 'NONE', #27902, 5.000000000000000000 ) ;
#15827 = ORIENTED_EDGE ( 'NONE', *, *, #75125, .F. ) ;
#15828 = CARTESIAN_POINT ( 'NONE',  ( 112.0288779015512119, -57.67108280594192138, 191.2312896774432147 ) ) ;
#15829 = CARTESIAN_POINT ( 'NONE',  ( 35.20412044861278389, 463.4819191117625792, 19.77841787010871855 ) ) ;
#15830 = AXIS2_PLACEMENT_3D ( 'NONE', #21845, #28895, #12638 ) ;
#15831 = DIRECTION ( 'NONE',  ( -1.000000000000000000, -1.224606353822377258E-16, -0.000000000000000000 ) ) ;
#15832 = CARTESIAN_POINT ( 'NONE',  ( 25.59999999999999787, 1.533819458162526451E-15, 0.000000000000000000 ) ) ;
#15833 = CARTESIAN_POINT ( 'NONE',  ( -5.453871017069856997, 54.16911077613673342, 6.031152949374326333 ) ) ;
#15834 = CARTESIAN_POINT ( 'NONE',  ( -75.37500990013671753, -60.00000000000000000, 183.7553592533116955 ) ) ;
#15835 = CARTESIAN_POINT ( 'NONE',  ( -41.58649125062324003, 315.0454808444952732, -5.157136739135766312 ) ) ;
#15836 =( NAMED_UNIT ( * ) PLANE_ANGLE_UNIT ( ) SI_UNIT ( $, .RADIAN. ) );
#15837 = CARTESIAN_POINT ( 'NONE',  ( -34.95237279327285762, 304.8277712208536627, 12.26231981495593537 ) ) ;
#15838 = CARTESIAN_POINT ( 'NONE',  ( -84.39447898885444488, -50.18442846096746024, 187.9382864958523669 ) ) ;
#15839 = VERTEX_POINT ( 'NONE', #64791 ) ;
#15840 = CARTESIAN_POINT ( 'NONE',  ( 21.12475202124109686, 303.9341318091517223, -9.982500423423047664 ) ) ;
#15841 =( BOUNDED_CURVE ( )  B_SPLINE_CURVE ( 2, ( #100410, #26572, #98802 ),
 .UNSPECIFIED., .F., .F. ) 
 B_SPLINE_CURVE_WITH_KNOTS ( ( 3, 3 ),
 ( 0.000000000000000000, 1.000000000000000000 ),
 .UNSPECIFIED. ) 
 CURVE ( )  GEOMETRIC_REPRESENTATION_ITEM ( )  RATIONAL_B_SPLINE_CURVE ( ( 1.000000000000000000, 1.857142857142858317, 1.000000000000000000 ) ) 
 REPRESENTATION_ITEM ( '' )  );
#15842 = ORIENTED_EDGE ( 'NONE', *, *, #42618, .F. ) ;
#15843 = CARTESIAN_POINT ( 'NONE',  ( 34.35000000000000142, 1.533819458162526451E-15, 0.000000000000000000 ) ) ;
#15844 = EDGE_CURVE ( 'NONE', #63495, #73065, #16710, .T. ) ;
#15845 = CARTESIAN_POINT ( 'NONE',  ( -6.642722259512091831, 41.46658730094534917, -70.60825968550385312 ) ) ;
#15846 = CARTESIAN_POINT ( 'NONE',  ( -86.24397153928001103, -60.23073308139314719, -13.36445785299144440 ) ) ;
#15847 = DIRECTION ( 'NONE',  ( 0.000000000000000000, -1.000000000000000000, 0.000000000000000000 ) ) ;
#15848 = ADVANCED_FACE ( 'NONE', ( #56131 ), #38875, .F. ) ;
#15849 = CARTESIAN_POINT ( 'NONE',  ( 6.683837171061802529, 3.955946848495958346, -6.851900933636989599 ) ) ;
#15850 = EDGE_LOOP ( 'NONE', ( #9628, #1261, #34472 ) ) ;
#15851 = DIRECTION ( 'NONE',  ( -1.000000000000000000, 0.000000000000000000, 0.000000000000000000 ) ) ;
#15852 = CARTESIAN_POINT ( 'NONE',  ( 11.09125750223364548, 19.52129652750905109, -8.745713487163543576 ) ) ;
#15853 = ADVANCED_FACE ( 'NONE', ( #93325 ), #27259, .F. ) ;
#15854 = CARTESIAN_POINT ( 'NONE',  ( 2.910977163135976653, -8.673617379884035472E-16, -22.23822744035697241 ) ) ;
#15855 = CARTESIAN_POINT ( 'NONE',  ( 23.21751746555220564, 25.25267828308493634, -33.20617127781077471 ) ) ;
#15856 = EDGE_CURVE ( 'NONE', #95206, #24536, #65370, .T. ) ;
#15857 = CARTESIAN_POINT ( 'NONE',  ( 17.10006063058271053, -59.99999999999996447, -44.43597027717249404 ) ) ;
#15858 = CARTESIAN_POINT ( 'NONE',  ( -76.14763078889043868, -56.84898049809550713, 140.2345650644058992 ) ) ;
#15859 = VERTEX_POINT ( 'NONE', #78195 ) ;
#15860 = CARTESIAN_POINT ( 'NONE',  ( 24.85181238201470322, -30.00000000000000000, 38.32581332381749206 ) ) ;
#15861 = CARTESIAN_POINT ( 'NONE',  ( 7.414580834929599185, 87.64656280281482736, 3.010264818013835164 ) ) ;
#15862 = CARTESIAN_POINT ( 'NONE',  ( 86.94765383177332296, -57.67023441083929214, -25.46996265147350869 ) ) ;
#15863 = CARTESIAN_POINT ( 'NONE',  ( 19.61638200451619696, 5.000000000000004441, 6.123233995736770227E-16 ) ) ;
#15864 = EDGE_CURVE ( 'NONE', #91623, #14996, #100136, .T. ) ;
#15865 = ADVANCED_FACE ( 'NONE', ( #63081 ), #70640, .T. ) ;
#15866 = DIRECTION ( 'NONE',  ( 0.9090909090909092827, 0.000000000000000000, -0.4165977904505306917 ) ) ;
#15867 = ORIENTED_EDGE ( 'NONE', *, *, #37443, .F. ) ;
#15868 = CYLINDRICAL_SURFACE ( 'NONE', #88951, 1.250000000000001110 ) ;
#15869 = AXIS2_PLACEMENT_3D ( 'NONE', #77764, #3877, #29772 ) ;
#15870 = CARTESIAN_POINT ( 'NONE',  ( 12.50000000000000533, 152.0000000000000000, 0.000000000000000000 ) ) ;
#15871 = DIRECTION ( 'NONE',  ( 1.000000000000000000, 0.000000000000000000, 0.000000000000000000 ) ) ;
#15872 = CARTESIAN_POINT ( 'NONE',  ( 5.082755093536324154, -16.34375000204838813, 5.082755093536326818 ) ) ;
#15873 = ADVANCED_FACE ( 'NONE', ( #69062 ), #54644, .T. ) ;
#15874 = EDGE_CURVE ( 'NONE', #94695, #826, #20014, .T. ) ;
#15875 = CARTESIAN_POINT ( 'NONE',  ( 44.24061507097197676, 485.5299576667521819, 3.142227259635101522 ) ) ;
#15876 = MECHANICAL_DESIGN_GEOMETRIC_PRESENTATION_REPRESENTATION (  '', ( #57193 ), #22841 ) ;
#15877 = CARTESIAN_POINT ( 'NONE',  ( 9.918579450955562038, 81.20696087031315358, 1.297207292923872046 ) ) ;
#15878 = FILL_AREA_STYLE_COLOUR ( '', #76081 ) ;
#15879 = CARTESIAN_POINT ( 'NONE',  ( -7.894955577759743548, 1.603085139993701169, -7.593799241562211755 ) ) ;
#15880 = SURFACE_SIDE_STYLE ('',( #31565 ) ) ;
#15881 = EDGE_LOOP ( 'NONE', ( #570, #611, #16798, #50920, #15141 ) ) ;
#15882 = CARTESIAN_POINT ( 'NONE',  ( -7.493258478124158906, 40.28998945925845021, -69.65507826025705640 ) ) ;
#15884 = CARTESIAN_POINT ( 'NONE',  ( 28.95048640063493295, -22.11353157157453353, 29.69856830660305391 ) ) ;
#15883 = CARTESIAN_POINT ( 'NONE',  ( -24.85253352225967660, -29.99999999999996092, 38.32597638696945097 ) ) ;
#15885 = CARTESIAN_POINT ( 'NONE',  ( 31.08222273432268068, 314.8424387781652172, -6.614865870714785601 ) ) ;
#15886 = ORIENTED_EDGE ( 'NONE', *, *, #17544, .F. ) ;
#15887 = AXIS2_PLACEMENT_3D ( 'NONE', #24605, #64005, #6795 ) ;
#15888 = ORIENTED_EDGE ( 'NONE', *, *, #43425, .F. ) ;
#15890 = CARTESIAN_POINT ( 'NONE',  ( 38.73386039798870684, 460.3889633641978207, 2.371405894923828139 ) ) ;
#15889 = DIRECTION ( 'NONE',  ( 0.000000000000000000, -1.000000000000000000, 0.000000000000000000 ) ) ;
#15891 = DIRECTION ( 'NONE',  ( 0.000000000000000000, 0.000000000000000000, 1.000000000000000000 ) ) ;
#15892 = FACE_OUTER_BOUND ( 'NONE', #66846, .T. ) ;
#15893 = CARTESIAN_POINT ( 'NONE',  ( -8.000000000000001776, -19.34375000409677270, 3.313708498984759387 ) ) ;
#15894 = CARTESIAN_POINT ( 'NONE',  ( 1.098080042019399905, 45.97102111612958453, 16.88153618267994815 ) ) ;
#15895 = DIRECTION ( 'NONE',  ( 1.000000000000000000, 0.000000000000000000, 0.000000000000000000 ) ) ;
#15896 = ORIENTED_EDGE ( 'NONE', *, *, #25905, .F. ) ;
#15897 = CARTESIAN_POINT ( 'NONE',  ( 0.000000000000000000, 0.000000000000000000, 0.000000000000000000 ) ) ;
#15898 = CARTESIAN_POINT ( 'NONE',  ( 32.17646412119353272, 464.6980787822282082, 10.84896803613094640 ) ) ;
#15899 = DIRECTION ( 'NONE',  ( 0.000000000000000000, 0.000000000000000000, 1.000000000000000000 ) ) ;
#15900 = CARTESIAN_POINT ( 'NONE',  ( 46.00000000000000000, 461.8820044443820620, 11.41122057645932308 ) ) ;
#15901 = CARTESIAN_POINT ( 'NONE',  ( 46.89572507581423366, 12.86406951795954434, -16.16260000396544783 ) ) ;
#15902 = EDGE_LOOP ( 'NONE', ( #93308, #28305 ) ) ;
#15903 = CIRCLE ( 'NONE', #100283, 4.000000000000001776 ) ;
#15904 = ORIENTED_EDGE ( 'NONE', *, *, #32316, .F. ) ;
#15905 = ORIENTED_EDGE ( 'NONE', *, *, #19217, .T. ) ;
#15906 = CARTESIAN_POINT ( 'NONE',  ( 0.7851006235064621475, 53.48263589571089227, 9.986492805000406037 ) ) ;
#15907 = CARTESIAN_POINT ( 'NONE',  ( 22.51022058473584053, 41.90417167145406552, -79.55356307799623039 ) ) ;
#15908 = CARTESIAN_POINT ( 'NONE',  ( -37.40775402191688670, 27.94109755877887125, 10.95617127781058642 ) ) ;
#15909 = CARTESIAN_POINT ( 'NONE',  ( 26.37453794305503152, 306.0354018384379060, 10.66098672490852550 ) ) ;
#15910 = CIRCLE ( 'NONE', #76179, 9.999999999999998224 ) ;
#15911 = CARTESIAN_POINT ( 'NONE',  ( -45.42083050872123096, 373.9457837719378972, 6.495393073555762342 ) ) ;
#15912 = CARTESIAN_POINT ( 'NONE',  ( -4.006803414943380659, -67.50235953894106444, 13.13861293866451696 ) ) ;
#15913 = CARTESIAN_POINT ( 'NONE',  ( -46.00000000000000000, 485.8996392799547266, 0.4531297708538281621 ) ) ;
#15914 = CARTESIAN_POINT ( 'NONE',  ( 12.50000000000000355, 39.75445632001817842, -65.02425370658717441 ) ) ;
#15915 = ORIENTED_EDGE ( 'NONE', *, *, #77201, .F. ) ;
#15917 = EDGE_CURVE ( 'NONE', #62818, #87124, #103944, .T. ) ;
#15916 = CARTESIAN_POINT ( 'NONE',  ( 30.55414771718632494, 11.21328959333584230, 39.95065846501993434 ) ) ;
#15918 = AXIS2_PLACEMENT_3D ( 'NONE', #35235, #101542, #99934 ) ;
#15919 = ORIENTED_EDGE ( 'NONE', *, *, #22137, .T. ) ;
#15920 = CARTESIAN_POINT ( 'NONE',  ( -7.681258945454893382E-14, -1.200000000000000030E-05, -39.50000000000000000 ) ) ;
#15921 = CARTESIAN_POINT ( 'NONE',  ( 19.07845090537422550, 294.6331628770684574, 9.890526070132905190 ) ) ;
#15922 = CYLINDRICAL_SURFACE ( 'NONE', #42096, 15.00000000000000000 ) ;
#15923 = VECTOR ( 'NONE', #22449, 1000.000000000000000 ) ;
#15924 = ADVANCED_FACE ( 'NONE', ( #56555 ), #42016, .F. ) ;
#15925 = CARTESIAN_POINT ( 'NONE',  ( -41.76078508741669992, -59.99999999999995026, 45.02266864589306294 ) ) ;
#15926 = CARTESIAN_POINT ( 'NONE',  ( 67.57980059920171811, -53.38336469478974067, 101.9910149677482565 ) ) ;
#15927 = EDGE_LOOP ( 'NONE', ( #55495, #52244, #64431 ) ) ;
#15928 = CARTESIAN_POINT ( 'NONE',  ( 6.957858546966888547, -47.06965355536787854, 39.14895102431469098 ) ) ;
#15929 = CARTESIAN_POINT ( 'NONE',  ( -32.89379909751026787, 463.7243792478176942, 7.148845075438585717 ) ) ;
#15930 = ADVANCED_FACE ( 'NONE', ( #30404 ), #46057, .T. ) ;
#15931 = CARTESIAN_POINT ( 'NONE',  ( 3.400000000000000355, 0.000000000000000000, -8.000000000000000000 ) ) ;
#15932 = ORIENTED_EDGE ( 'NONE', *, *, #86616, .T. ) ;
#15933 = CARTESIAN_POINT ( 'NONE',  ( -6.837824896291514243, 3.947820044545419016, -6.564402953523714501 ) ) ;
#15934 = CARTESIAN_POINT ( 'NONE',  ( -34.64166250171392392, 490.4813561613900674, 11.60003975507707175 ) ) ;
#15935 = B_SPLINE_CURVE_WITH_KNOTS ( 'NONE', 3,
 ( #24781, #39885, #32344, #97561, #90020, #57629, #56032, #8026, #80316, #81377, #7487, #23185, #89499, #96532, #6967, #65750, #39366, #98630, #90554, #16663, #65214, #72244 ),
 .UNSPECIFIED., .F., .F.,
 ( 4, 2, 2, 2, 2, 2, 2, 2, 2, 2, 4 ),
 ( 0.006438828156869064352, 0.006690637486827953097, 0.006942446816786841841, 0.007446065476704619331, 0.007949684136622395952, 0.008453302796540173442, 0.008956921456457950931, 0.009460540116375728420, 0.009964158776293505909, 0.01021596810625239465, 0.01046777743621128340 ),
 .UNSPECIFIED. ) ;
#15936 = CARTESIAN_POINT ( 'NONE',  ( -3.313708498984765161, -31.15625000409677270, 7.999999999999998224 ) ) ;
#15937 = CARTESIAN_POINT ( 'NONE',  ( 2.094395098902661179, -4.999999999999998224, 8.000000000000000000 ) ) ;
#15938 = CARTESIAN_POINT ( 'NONE',  ( 32.70825224882159432, 489.1175319723079724, 10.34480600317815835 ) ) ;
#15939 = AXIS2_PLACEMENT_3D ( 'NONE', #6705, #39632, #72503 ) ;
#15940 = CARTESIAN_POINT ( 'NONE',  ( -43.64534273044682067, 464.9151781295577734, 12.30378483073885221 ) ) ;
#15941 = EDGE_CURVE ( 'NONE', #54633, #64557, #44751, .T. ) ;
#15942 = CARTESIAN_POINT ( 'NONE',  ( -10.41860328468676755, 6.902172553357436513, 4.999999999999923617 ) ) ;
#15943 = CARTESIAN_POINT ( 'NONE',  ( -6.763850406535977022, 294.7356673863635592, 9.912314076180619438 ) ) ;
#15944 =( GEOMETRIC_REPRESENTATION_CONTEXT ( 3 ) GLOBAL_UNCERTAINTY_ASSIGNED_CONTEXT ( ( #85550 ) ) GLOBAL_UNIT_ASSIGNED_CONTEXT ( ( #100301, #59329, #58249 ) ) REPRESENTATION_CONTEXT ( 'NONE', 'WORKASPACE' ) );
#15945 = SURFACE_STYLE_USAGE ( .BOTH. , #7304 ) ;
#15946 =( NAMED_UNIT ( * ) SI_UNIT ( $, .STERADIAN. ) SOLID_ANGLE_UNIT ( ) );
#15947 = ORIENTED_EDGE ( 'NONE', *, *, #10689, .F. ) ;
#15948 = CARTESIAN_POINT ( 'NONE',  ( 0.5805565836007605673, 3.752776749732565253, 6.499999999999997335 ) ) ;
#15949 = AXIS2_PLACEMENT_3D ( 'NONE', #20414, #75927, #53258 ) ;
#15950 = CARTESIAN_POINT ( 'NONE',  ( 1.421012265766256721, -59.99999999999999289, 39.63907929704831190 ) ) ;
#15951 = CARTESIAN_POINT ( 'NONE',  ( -98.89902882238894222, -29.99999999999999645, 189.0609296686858158 ) ) ;
#15952 = CARTESIAN_POINT ( 'NONE',  ( -40.53459811498787957, 485.1082980165977006, -4.183568619536963240 ) ) ;
#15953 = AXIS2_PLACEMENT_3D ( 'NONE', #37967, #54610, #6609 ) ;
#15954 = CARTESIAN_POINT ( 'NONE',  ( 47.36048362120468624, -57.68077050285960894, 70.51996143053239052 ) ) ;
#15956 = CARTESIAN_POINT ( 'NONE',  ( -9.768722988854461775, 53.46525899633061130, 2.424613394572812997 ) ) ;
#15955 = CARTESIAN_POINT ( 'NONE',  ( -0.5676227808506075778, 26.02816272619953608, -38.38318647011021767 ) ) ;
#15957 = CARTESIAN_POINT ( 'NONE',  ( 14.74954138962861627, -24.00043886548641936, -38.53150145719773434 ) ) ;
#15958 = CARTESIAN_POINT ( 'NONE',  ( -1.219825599638223235, 43.50030555992006498, 17.81618553082049061 ) ) ;
#15960 = UNCERTAINTY_MEASURE_WITH_UNIT (LENGTH_MEASURE( 1.000000000000000082E-05 ), #96358, 'distance_accuracy_value', 'NONE');
#15959 = PRODUCT_DEFINITION ( 'UNKNOWN', '', #833, #67234 ) ;
#15961 = CARTESIAN_POINT ( 'NONE',  ( -44.19868099429154285, 435.2430970659380023, 14.45534906870889991 ) ) ;
#15962 = CARTESIAN_POINT ( 'NONE',  ( -27.03817179307704421, -60.00000000000001421, 41.77503236863146441 ) ) ;
#15963 = LINE ( 'NONE', #81733, #101987 ) ;
#15964 = CARTESIAN_POINT ( 'NONE',  ( 104.3757837139179117, 6.123233995736582872E-16, -5.000000000000011546 ) ) ;
#15965 = CARTESIAN_POINT ( 'NONE',  ( -86.71815218704666961, -20.66647618804140407, 185.1331831730891224 ) ) ;
#15966 = ORIENTED_EDGE ( 'NONE', *, *, #56368, .F. ) ;
#15967 = CARTESIAN_POINT ( 'NONE',  ( 17.50000000000000355, 51.12013589171683492, 63.06608111885196877 ) ) ;
#15968 = CARTESIAN_POINT ( 'NONE',  ( 10.52478704574295776, -11.52214087695234568, 17.76063389341357279 ) ) ;
#15969 = CARTESIAN_POINT ( 'NONE',  ( -6.057497750955408655, -32.51266269460595737, 29.29875079916816105 ) ) ;
#15970 = FACE_OUTER_BOUND ( 'NONE', #73013, .T. ) ;
#15971 = STYLED_ITEM ( 'NONE', ( #54925 ), #96092 ) ;
#15973 = CARTESIAN_POINT ( 'NONE',  ( 1.354611299910297717, -70.11838715117606569, 13.05944322661130919 ) ) ;
#15972 = CARTESIAN_POINT ( 'NONE',  ( 5.589124336234602808, -4.278671059403162502, -6.219623095962701242 ) ) ;
#15974 = ORIENTED_EDGE ( 'NONE', *, *, #86330, .F. ) ;
#15975 = CARTESIAN_POINT ( 'NONE',  ( -46.00000000000000000, 488.7529659943160709, 4.223909611883613913 ) ) ;
#15976 = CARTESIAN_POINT ( 'NONE',  ( -7.500141383061431632, -5.000000000000005329, -20.99866593659555036 ) ) ;
#15977 = CARTESIAN_POINT ( 'NONE',  ( -7.619701877737479201, 33.17442159532767221, -2.447562251315979598 ) ) ;
#15978 = VECTOR ( 'NONE', #28983, 1000.000000000000000 ) ;
#15979 = CARTESIAN_POINT ( 'NONE',  ( 33.49531054704386435, 300.6511913297455294, -0.6950156566324289242 ) ) ;
#15980 = CARTESIAN_POINT ( 'NONE',  ( 4.382959417677089853, -48.13794921561771645, 102.7400018439556391 ) ) ;
#15981 = ADVANCED_FACE ( 'NONE', ( #55166 ), #71358, .T. ) ;
#15982 =( NAMED_UNIT ( * ) SI_UNIT ( $, .STERADIAN. ) SOLID_ANGLE_UNIT ( ) );
#15983 = CARTESIAN_POINT ( 'NONE',  ( 73.51782150160397578, -60.00000000000000711, 167.3661187031590316 ) ) ;
#15984 = CARTESIAN_POINT ( 'NONE',  ( 105.4249980201500136, -14.21045842199437992, 149.5332359265665900 ) ) ;
#15985 = CARTESIAN_POINT ( 'NONE',  ( -45.29905483467455696, 497.0732240353902398, -8.041250874568902418 ) ) ;
#15986 = VERTEX_POINT ( 'NONE', #88616 ) ;
#15987 = DIRECTION ( 'NONE',  ( 0.000000000000000000, 1.000000000000000000, 0.000000000000000000 ) ) ;
#15988 = CARTESIAN_POINT ( 'NONE',  ( -9.165151389911699198, 250.2671078128291242, -4.000000000000002665 ) ) ;
#15989 = AXIS2_PLACEMENT_3D ( 'NONE', #36915, #61166, #85434 ) ;
#15991 = CARTESIAN_POINT ( 'NONE',  ( -37.24486667819202523, 485.5941914037269953, -4.198424488983384606 ) ) ;
#15990 = CARTESIAN_POINT ( 'NONE',  ( 8.180516222381777780, -14.21045842199445630, 34.35482301558341334 ) ) ;
#15992 = CARTESIAN_POINT ( 'NONE',  ( 21.84999999999999787, -3.309499999999999886, 4.475777889183790779E-16 ) ) ;
#15993 = ORIENTED_EDGE ( 'NONE', *, *, #68214, .F. ) ;
#15994 = UNCERTAINTY_MEASURE_WITH_UNIT (LENGTH_MEASURE( 1.000000000000000082E-05 ), #104552, 'distance_accuracy_value', 'NONE');
#15995 = CARTESIAN_POINT ( 'NONE',  ( -20.56423368124215756, 303.9071437805204710, 9.948769377620161336 ) ) ;
#15996 = EDGE_CURVE ( 'NONE', #63024, #71240, #47608, .T. ) ;
#15997 = ORIENTED_EDGE ( 'NONE', *, *, #101587, .T. ) ;
#15998 = CARTESIAN_POINT ( 'NONE',  ( 35.23119160525166649, 485.0602108522160734, -1.504563171983482661 ) ) ;
#15999 = EDGE_CURVE ( 'NONE', #72252, #74862, #49498, .T. ) ;
#16000 = PLANE ( 'NONE',  #54322 ) ;
#16001 = CARTESIAN_POINT ( 'NONE',  ( 0.000000000000000000, 0.000000000000000000, 0.000000000000000000 ) ) ;
#16002 = ORIENTED_EDGE ( 'NONE', *, *, #29366, .T. ) ;
#16003 = SURFACE_SIDE_STYLE ('',( #72637 ) ) ;
#16004 = CARTESIAN_POINT ( 'NONE',  ( -9.001979478496508591, 6.776006056211794082, -3.303702010581815784 ) ) ;
#16005 = CARTESIAN_POINT ( 'NONE',  ( -32.66239298923139245, -59.99999999999511147, 47.46693911184033254 ) ) ;
#16006 = CARTESIAN_POINT ( 'NONE',  ( 62.59428447264396311, -1.232595164407830946E-29, 4.000000000000007105 ) ) ;
#16007 = CARTESIAN_POINT ( 'NONE',  ( 73.38123138194130490, -59.99999999999997868, 165.9433868892914461 ) ) ;
#16009 = CARTESIAN_POINT ( 'NONE',  ( 13.37339337037409415, -32.51077182928822396, 29.38669317182240803 ) ) ;
#16008 = CARTESIAN_POINT ( 'NONE',  ( -109.1953414053527780, -30.00000000000001066, 161.8807222540328894 ) ) ;
#16010 = CARTESIAN_POINT ( 'NONE',  ( 99.45413243311152485, -38.00000000000002842, 191.4610151428277049 ) ) ;
#16011 = CARTESIAN_POINT ( 'NONE',  ( -44.74673245019804568, -39.53078959506873957, 43.36019415930032750 ) ) ;
#16012 = CARTESIAN_POINT ( 'NONE',  ( -11.09043181265275813, 18.64284798592964165, 36.79570967431529738 ) ) ;
#16013 = VERTEX_POINT ( 'NONE', #106368 ) ;
#16014 = CYLINDRICAL_SURFACE ( 'NONE', #61147, 4.000000000000000000 ) ;
#16015 = CARTESIAN_POINT ( 'NONE',  ( 6.163737169369001734, -12.13805321688063898, 11.84025182891623729 ) ) ;
#16016 = VECTOR ( 'NONE', #84064, 999.9999999999998863 ) ;
#16017 = CARTESIAN_POINT ( 'NONE',  ( 0.4033376246892499406, 7.198601258566903027, -0.5316568767328684331 ) ) ;
#16018 = CARTESIAN_POINT ( 'NONE',  ( 6.463481858019713755, 4.600809706232195317, 5.711197301637621848 ) ) ;
#16019 = CARTESIAN_POINT ( 'NONE',  ( 32.11411341898570981, 317.7919323371296514, -6.873671351699469412 ) ) ;
#16020 = ORIENTED_EDGE ( 'NONE', *, *, #586, .F. ) ;
#16021 = ORIENTED_EDGE ( 'NONE', *, *, #97680, .F. ) ;
#16022 = CARTESIAN_POINT ( 'NONE',  ( 80.75544287417717726, -30.00000000000002132, -12.51947141605529090 ) ) ;
#16023 = CARTESIAN_POINT ( 'NONE',  ( 23.39223446984816590, 41.66174788536504536, -75.12607633062728496 ) ) ;
#16024 = COLOUR_RGB ( '', 0.40784314, 0.44705882, 0.49803922) ;
#16025 = CARTESIAN_POINT ( 'NONE',  ( 24.20495127240709721, 25.63507095802091129, -31.17354648878573897 ) ) ;
#16026 = CARTESIAN_POINT ( 'NONE',  ( 94.63127039864093604, -30.00000000000000000, 115.7646022404933461 ) ) ;
#16027 =( GEOMETRIC_REPRESENTATION_CONTEXT ( 3 ) GLOBAL_UNCERTAINTY_ASSIGNED_CONTEXT ( ( #45961 ) ) GLOBAL_UNIT_ASSIGNED_CONTEXT ( ( #67594, #34720, #58973 ) ) REPRESENTATION_CONTEXT ( 'NONE', 'WORKASPACE' ) );
#16028 = PLANE ( 'NONE',  #51881 ) ;
#16029 = ORIENTED_EDGE ( 'NONE', *, *, #34009, .F. ) ;
#16030 = ORIENTED_EDGE ( 'NONE', *, *, #89402, .F. ) ;
#16031 = EDGE_LOOP ( 'NONE', ( #61422, #77537, #27839, #41532, #8378, #83597 ) ) ;
#16032 = FACE_OUTER_BOUND ( 'NONE', #9519, .T. ) ;
#16033 = CARTESIAN_POINT ( 'NONE',  ( -2.349680750045843425, -6.873796553395948195, -13.34206326735361081 ) ) ;
#16034 =( GEOMETRIC_REPRESENTATION_CONTEXT ( 3 ) GLOBAL_UNCERTAINTY_ASSIGNED_CONTEXT ( ( #16964 ) ) GLOBAL_UNIT_ASSIGNED_CONTEXT ( ( #17784, #64730, #56618 ) ) REPRESENTATION_CONTEXT ( 'NONE', 'WORKASPACE' ) );
#16035 = SURFACE_STYLE_FILL_AREA ( #64601 ) ;
#16036 = ORIENTED_EDGE ( 'NONE', *, *, #61300, .F. ) ;
#16038 = EDGE_CURVE ( 'NONE', #101842, #74993, #71857, .T. ) ;
#16037 = CARTESIAN_POINT ( 'NONE',  ( 9.699121749566359085, 108.1766876027581503, 2.444499528233566199 ) ) ;
#16039 = EDGE_LOOP ( 'NONE', ( #73498, #36751 ) ) ;
#16040 = DIRECTION ( 'NONE',  ( -1.000000000000000000, -1.224606353822377258E-16, -0.000000000000000000 ) ) ;
#16041 = CARTESIAN_POINT ( 'NONE',  ( 85.16262797248658956, -38.69119117541009700, 198.5801802344664111 ) ) ;
#16042 = CARTESIAN_POINT ( 'NONE',  ( 6.222742520105469133, 3.584500230190539316, -6.791463481567638460 ) ) ;
#16043 = CARTESIAN_POINT ( 'NONE',  ( 29.02256445720001565, 312.0358488567985660, 12.14896804447468526 ) ) ;
#16044 = SURFACE_STYLE_USAGE ( .BOTH. , #47868 ) ;
#16045 = DIRECTION ( 'NONE',  ( 1.000000000000000000, 0.000000000000000000, 0.000000000000000000 ) ) ;
#16046 = CARTESIAN_POINT ( 'NONE',  ( -27.26381482557892255, 34.42320106084914499, -10.05698433968609606 ) ) ;
#16047 = CARTESIAN_POINT ( 'NONE',  ( -4.980618096941786810, -46.46097021954794570, 103.2912570477109000 ) ) ;
#16048 = AXIS2_PLACEMENT_3D ( 'NONE', #11700, #3096, #77523 ) ;
#16049 = EDGE_CURVE ( 'NONE', #93186, #36646, #31959, .T. ) ;
#16050 = CYLINDRICAL_SURFACE ( 'NONE', #56636, 4.000000000000000888 ) ;
#16051 = CARTESIAN_POINT ( 'NONE',  ( 0.000000000000000000, 0.000000000000000000, -13.00000000000000000 ) ) ;
#16052 = ORIENTED_EDGE ( 'NONE', *, *, #44622, .F. ) ;
#16053 = DIRECTION ( 'NONE',  ( 0.000000000000000000, 0.000000000000000000, 1.000000000000000000 ) ) ;
#16055 = CARTESIAN_POINT ( 'NONE',  ( 5.420470438621123321, 41.88321586334136981, -59.04137885805280916 ) ) ;
#16054 =( LENGTH_UNIT ( ) NAMED_UNIT ( * ) SI_UNIT ( .MILLI., .METRE. ) );
#16056 = UNCERTAINTY_MEASURE_WITH_UNIT (LENGTH_MEASURE( 1.000000000000000082E-05 ), #76106, 'distance_accuracy_value', 'NONE');
#16057 = DIRECTION ( 'NONE',  ( -1.000000000000000000, -1.224606353822377258E-16, -0.000000000000000000 ) ) ;
#16058 = CARTESIAN_POINT ( 'NONE',  ( -3.313708498984765161, -15.96874999999999289, 7.999999999999998224 ) ) ;
#16059 = CIRCLE ( 'NONE', #47079, 13.50000000000000000 ) ;
#16060 = CARTESIAN_POINT ( 'NONE',  ( -7.422993619742127791, -19.22976363275861900, 35.19469004974323667 ) ) ;
#16061 = CARTESIAN_POINT ( 'NONE',  ( 32.33349330513380693, 1.593028355512270962E-15, 0.000000000000000000 ) ) ;
#16062 = CARTESIAN_POINT ( 'NONE',  ( 0.000000000000000000, 1.500000000000000000, -60.00000000000000000 ) ) ;
#16063 = ORIENTED_EDGE ( 'NONE', *, *, #81063, .T. ) ;
#16064 = CARTESIAN_POINT ( 'NONE',  ( 83.95501332274635331, -53.77704049164677969, 188.7737198488325134 ) ) ;
#16065 = CARTESIAN_POINT ( 'NONE',  ( 2.450541714948253347, 15.75132464342601146, -9.701712097384769251 ) ) ;
#16066 = EDGE_CURVE ( 'NONE', #63698, #26216, #77069, .T. ) ;
#16067 = CARTESIAN_POINT ( 'NONE',  ( 2.422472278927138599E-15, -0.1944580884125599318, 19.78098730681987760 ) ) ;
#16068 = EDGE_LOOP ( 'NONE', ( #64969, #88370 ) ) ;
#16069 = CARTESIAN_POINT ( 'NONE',  ( 92.89556986967913588, -57.65649627823201229, -17.47502724792872186 ) ) ;
#16070 = EDGE_CURVE ( 'NONE', #1254, #10915, #101173, .T. ) ;
#16071 = CARTESIAN_POINT ( 'NONE',  ( 36.07271708247883168, 437.4941479923609791, 4.311972135659492444 ) ) ;
#16072 = FILL_AREA_STYLE ('',( #98578 ) ) ;
#16073 = CARTESIAN_POINT ( 'NONE',  ( 28.71655383515135185, 10.49725697686260872, 41.65669210871947570 ) ) ;
#16074 = EDGE_CURVE ( 'NONE', #71070, #48348, #934, .T. ) ;
#16075 = CARTESIAN_POINT ( 'NONE',  ( -81.00880480115741022, -29.99999999999999645, 21.10007109864825736 ) ) ;
#16076 = CARTESIAN_POINT ( 'NONE',  ( -72.14820142673382009, -37.99999999999997158, 108.4616125675222094 ) ) ;
#16077 = CARTESIAN_POINT ( 'NONE',  ( 0.000000000000000000, -4.999999999999998224, 8.000000000000000000 ) ) ;
#16078 = CARTESIAN_POINT ( 'NONE',  ( -2.459698528280935381, 7.240146430416063872, -0.09933465333850977075 ) ) ;
#16080 = DIRECTION ( 'NONE',  ( -1.000000000000000000, -1.224606353822377258E-16, -0.000000000000000000 ) ) ;
#16079 = FACE_OUTER_BOUND ( 'NONE', #81506, .T. ) ;
#16081 = DIRECTION ( 'NONE',  ( 0.000000000000000000, 1.000000000000000000, 0.000000000000000000 ) ) ;
#16082 = CARTESIAN_POINT ( 'NONE',  ( -31.35596682365705945, 438.0939828603719093, 22.55458131664414267 ) ) ;
#16083 = CARTESIAN_POINT ( 'NONE',  ( 5.725004243152312711, -81.42480851744635117, -1.812899781754687911 ) ) ;
#16084 = CARTESIAN_POINT ( 'NONE',  ( -12.74625527888247944, -23.93263146839674604, -30.51339262294724008 ) ) ;
#16085 = FILL_AREA_STYLE_COLOUR ( '', #14994 ) ;
#16086 = CIRCLE ( 'NONE', #90156, 4.000000000000000000 ) ;
#16087 = CARTESIAN_POINT ( 'NONE',  ( 33.81613602128341967, 485.0484310908490784, 1.468412048127565761 ) ) ;
#16088 = EDGE_CURVE ( 'NONE', #48472, #9392, #11034, .T. ) ;
#16089 = VECTOR ( 'NONE', #103792, 1000.000000000000000 ) ;
#16090 = ADVANCED_FACE ( 'NONE', ( #77213 ), #73002, .T. ) ;
#16091 = ORIENTED_EDGE ( 'NONE', *, *, #89847, .F. ) ;
#16092 = DIRECTION ( 'NONE',  ( 0.000000000000000000, 1.000000000000000000, 0.000000000000000000 ) ) ;
#16093 = CARTESIAN_POINT ( 'NONE',  ( 7.808623696107068746, -4.508310992948072915, -7.999704684617485739 ) ) ;
#16094 = AXIS2_PLACEMENT_3D ( 'NONE', #20301, #36996, #11065 ) ;
#16095 = CARTESIAN_POINT ( 'NONE',  ( -35.84592417077619331, -23.58871961031537978, -31.12588894592865785 ) ) ;
#16097 = CARTESIAN_POINT ( 'NONE',  ( -56.21085237342701646, -34.58943223605337636, -26.29373296556804362 ) ) ;
#16096 = CARTESIAN_POINT ( 'NONE',  ( 9.250997389131581983, 1.340359594676612611E-15, 0.000000000000000000 ) ) ;
#16098 = VERTEX_POINT ( 'NONE', #84775 ) ;
#16100 = ORIENTED_EDGE ( 'NONE', *, *, #94161, .T. ) ;
#16099 = COLOUR_RGB ( '', 0.66274510, 0.83137255, 0.94901961) ;
#16101 = LINE ( 'NONE', #75071, #96510 ) ;
#16102 = FILL_AREA_STYLE ('',( #31778 ) ) ;
#16103 = CARTESIAN_POINT ( 'NONE',  ( -2.499999999999978684, -29.99999999999999645, 28.88619816519791073 ) ) ;
#16104 = CARTESIAN_POINT ( 'NONE',  ( -81.49343273877569516, -60.00000000000002132, -27.02824350414386245 ) ) ;
#16105 = ORIENTED_EDGE ( 'NONE', *, *, #68196, .F. ) ;
#16106 = CARTESIAN_POINT ( 'NONE',  ( 8.431489367831275672, -22.82219903641888337, -30.52630000682834677 ) ) ;
#16107 = CARTESIAN_POINT ( 'NONE',  ( 100.7081988093182190, -60.27117616117514132, 195.3567347834335806 ) ) ;
#16108 = CARTESIAN_POINT ( 'NONE',  ( -47.78440564129563484, 10.33446651290970486, 16.83708170412465677 ) ) ;
#16109 = ORIENTED_EDGE ( 'NONE', *, *, #15786, .F. ) ;
#16110 = COLOUR_RGB ( '', 0.31764706, 0.68627451, 0.89019608) ;
#16111 = EDGE_LOOP ( 'NONE', ( #103322, #92492, #101614, #97977, #14187, #94699 ) ) ;
#16112 = EDGE_LOOP ( 'NONE', ( #2964, #24048, #88041, #97993 ) ) ;
#16113 = CARTESIAN_POINT ( 'NONE',  ( 29.02089222109925615, 322.4236678735347255, 14.27358046319127283 ) ) ;
#16114 = EDGE_CURVE ( 'NONE', #54299, #81845, #14418, .T. ) ;
#16115 = CARTESIAN_POINT ( 'NONE',  ( -5.959015317364962705, -13.75072846948174998, 13.79531249880972510 ) ) ;
#16116 = ORIENTED_EDGE ( 'NONE', *, *, #95044, .T. ) ;
#16117 = MECHANICAL_DESIGN_GEOMETRIC_PRESENTATION_REPRESENTATION (  '', ( #95366 ), #10954 ) ;
#16118 = CARTESIAN_POINT ( 'NONE',  ( 16.64348903516512834, 45.88445698070336931, -4.157797401561768247 ) ) ;
#16119 = CARTESIAN_POINT ( 'NONE',  ( 0.000000000000000000, 152.0000000000000000, 5.000000000000000000 ) ) ;
#16120 = CIRCLE ( 'NONE', #102209, 4.000000000000001776 ) ;
#16121 = LINE ( 'NONE', #40932, #15061 ) ;
#16122 = CARTESIAN_POINT ( 'NONE',  ( -31.30247466046573379, -57.68739127208316120, 46.06264550376279487 ) ) ;
#16123 = CARTESIAN_POINT ( 'NONE',  ( -5.082755093536326818, -33.21875000204838813, 5.082755093536325042 ) ) ;
#16124 = CARTESIAN_POINT ( 'NONE',  ( 7.151597709147948123, -66.78929265052218511, 3.587174531012141898 ) ) ;
#16125 = DIRECTION ( 'NONE',  ( 1.000000000000000000, 1.224606353822377258E-16, 0.000000000000000000 ) ) ;
#16126 = FACE_BOUND ( 'NONE', #44145, .T. ) ;
#16127 = EDGE_CURVE ( 'NONE', #27903, #75855, #70532, .T. ) ;
#16128 = CARTESIAN_POINT ( 'NONE',  ( 42.61132677773223065, -60.00000000000003553, -41.65900251181847125 ) ) ;
#16129 = CARTESIAN_POINT ( 'NONE',  ( 0.000000000000000000, 6.928203230275505220, -4.000000000000007105 ) ) ;
#16130 = CARTESIAN_POINT ( 'NONE',  ( -54.15982943992869281, -32.56507362313620746, 55.81706142454490305 ) ) ;
#16131 = CARTESIAN_POINT ( 'NONE',  ( 4.000000000000000888, 18.12356304358896608, -5.744562646538073913 ) ) ;
#16132 = B_SPLINE_CURVE_WITH_KNOTS ( 'NONE', 3,
 ( #48731, #75131, #73007, #64425, #97294, #56285, #74606, #49266 ),
 .UNSPECIFIED., .F., .F.,
 ( 4, 2, 2, 4 ),
 ( -1.267662083608645886E-05, 0.002237097954985276579, 0.003361985242895957748, 0.004486872530806639350 ),
 .UNSPECIFIED. ) ;
#16133 = ORIENTED_EDGE ( 'NONE', *, *, #12003, .T. ) ;
#16134 = CARTESIAN_POINT ( 'NONE',  ( -97.87568255775092041, -37.71879727302795970, 192.5524585354622786 ) ) ;
#16135 = CARTESIAN_POINT ( 'NONE',  ( -0.6295717879345569257, 294.8518027745081440, -10.00000000000725109 ) ) ;
#16136 = ORIENTED_EDGE ( 'NONE', *, *, #41821, .T. ) ;
#16137 = CARTESIAN_POINT ( 'NONE',  ( -17.40116869051068704, 43.25107240467212932, 6.405389961558260126 ) ) ;
#16138 = CARTESIAN_POINT ( 'NONE',  ( 106.5513553430678684, -38.35592835780060739, 127.5841831557265067 ) ) ;
#16139 = CARTESIAN_POINT ( 'NONE',  ( 105.5353273971932140, -5.000000000000000000, 6.123233995736778115E-16 ) ) ;
#16140 = CARTESIAN_POINT ( 'NONE',  ( -6.045900698167796072, 51.82901340926924405, -6.272940833958317697 ) ) ;
#16141 = CARTESIAN_POINT ( 'NONE',  ( -4.238144987383360096, 302.8058397689824801, 9.927349000678042046 ) ) ;
#16142 =( BOUNDED_CURVE ( )  B_SPLINE_CURVE ( 2, ( #60253, #35448, #49048, #1426, #85579, #19292, #68322, #3043, #43511 ),
 .UNSPECIFIED., .F., .F. ) 
 B_SPLINE_CURVE_WITH_KNOTS ( ( 3, 2, 2, 2, 3 ),
 ( 0.7500000000000001110, 0.7573529411764706731, 0.7647058823529412352, 0.7720588235294119084, 0.7794117647058824705 ),
 .UNSPECIFIED. ) 
 CURVE ( )  GEOMETRIC_REPRESENTATION_ITEM ( )  RATIONAL_B_SPLINE_CURVE ( ( 0.9999999999999988898, 0.9238795325112878487, 1.000000000000000000, 0.9238795325112867385, 1.000000000000000000, 0.9238795325112867385, 1.000000000000000000, 0.9238795325112856283, 1.000000000000001110 ) ) 
 REPRESENTATION_ITEM ( '' )  );
#16143 = DIRECTION ( 'NONE',  ( 0.000000000000000000, -1.000000000000000000, 0.000000000000000000 ) ) ;
#16145 = CARTESIAN_POINT ( 'NONE',  ( 83.63598298596150471, -30.00000000000000000, 157.8859991142867614 ) ) ;
#16144 = UNCERTAINTY_MEASURE_WITH_UNIT (LENGTH_MEASURE( 1.000000000000000082E-05 ), #22431, 'distance_accuracy_value', 'NONE');
#16146 = CARTESIAN_POINT ( 'NONE',  ( -10.61502689374716191, 43.20235065847915479, -15.36667125108853327 ) ) ;
#16147 = CARTESIAN_POINT ( 'NONE',  ( -31.97926341577425546, 464.8423874313697297, 12.51531747069310363 ) ) ;
#16148 = DIRECTION ( 'NONE',  ( -1.000000000000000000, -1.224606353822377258E-16, -0.000000000000000000 ) ) ;
#16149 = ORIENTED_EDGE ( 'NONE', *, *, #44547, .T. ) ;
#16150 = ORIENTED_EDGE ( 'NONE', *, *, #12428, .T. ) ;
#16151 = CARTESIAN_POINT ( 'NONE',  ( 50.61148790639070683, -46.43901393920370424, 54.16023664066702281 ) ) ;
#16152 = CARTESIAN_POINT ( 'NONE',  ( 6.690415142086857614, 41.73276191905608812, -59.04972836783017698 ) ) ;
#16153 = FACE_OUTER_BOUND ( 'NONE', #72604, .T. ) ;
#16154 = VERTEX_POINT ( 'NONE', #19022 ) ;
#16156 = EDGE_CURVE ( 'NONE', #21912, #52979, #101485, .T. ) ;
#16155 = CARTESIAN_POINT ( 'NONE',  ( -110.3885816063411767, -38.35608404332607790, 159.0436535490340759 ) ) ;
#16157 = ORIENTED_EDGE ( 'NONE', *, *, #50687, .T. ) ;
#16158 = CARTESIAN_POINT ( 'NONE',  ( 28.28051920154564769, 34.26500913490271216, -8.373811989914575094 ) ) ;
#16159 = CARTESIAN_POINT ( 'NONE',  ( 92.04552895760792808, -38.35407921060832592, 35.17533269925505124 ) ) ;
#16160 = CARTESIAN_POINT ( 'NONE',  ( 12.04303557248932677, 10.55999509045389928, -9.701624603060800212 ) ) ;
#16161 = LINE ( 'NONE', #76932, #22466 ) ;
#16162 = CARTESIAN_POINT ( 'NONE',  ( 96.37451246332086896, -52.71696751734791064, 101.1475834991004348 ) ) ;
#16163 = CARTESIAN_POINT ( 'NONE',  ( -17.25498915691571966, 43.52709508488109691, -4.306061980902978981 ) ) ;
#16164 = SURFACE_STYLE_USAGE ( .BOTH. , #64214 ) ;
#16165 = CARTESIAN_POINT ( 'NONE',  ( -29.84737552601459143, 311.4075149060049625, -8.473334882481744046 ) ) ;
#16166 = VECTOR ( 'NONE', #13567, 1000.000000000000000 ) ;
#16167 = CARTESIAN_POINT ( 'NONE',  ( 6.562974947121710478, 4.277474787035884241, -6.282829635893496523 ) ) ;
#16168 = CARTESIAN_POINT ( 'NONE',  ( 75.46832707863339351, -60.00000000000002132, 184.3015218829329172 ) ) ;
#16169 = EDGE_CURVE ( 'NONE', #12195, #81281, #31754, .T. ) ;
#16170 = CIRCLE ( 'NONE', #43742, 5.000000000000011546 ) ;
#16171 = CARTESIAN_POINT ( 'NONE',  ( 17.54774805024657880, 45.00000000000000711, 63.32653931362602862 ) ) ;
#16173 = ORIENTED_EDGE ( 'NONE', *, *, #23274, .F. ) ;
#16172 =( BOUNDED_CURVE ( )  B_SPLINE_CURVE ( 2, ( #9384, #27773, #59574, #2897, #60647, #100009, #93533, #26177, #8870 ),
 .UNSPECIFIED., .F., .F. ) 
 B_SPLINE_CURVE_WITH_KNOTS ( ( 3, 2, 2, 2, 3 ),
 ( 0.9264705882352942679, 0.9338235294117648300, 0.9411764705882352811, 0.9485294117647058432, 0.9558823529411765163 ),
 .UNSPECIFIED. ) 
 CURVE ( )  GEOMETRIC_REPRESENTATION_ITEM ( )  RATIONAL_B_SPLINE_CURVE ( ( 0.9999999999999988898, 0.9238795325112878487, 1.000000000000000000, 0.9238795325112867385, 1.000000000000000000, 0.9238795325112867385, 1.000000000000000000, 0.9238795325112867385, 1.000000000000000000 ) ) 
 REPRESENTATION_ITEM ( '' )  );
#16174 = CARTESIAN_POINT ( 'NONE',  ( 59.14149476428188734, -22.12859458409723601, 62.21351809755216777 ) ) ;
#16175 = PRESENTATION_STYLE_ASSIGNMENT (( #48531 ) ) ;
#16176 = EDGE_CURVE ( 'NONE', #19689, #47334, #2238, .T. ) ;
#16177 = CARTESIAN_POINT ( 'NONE',  ( -33.00000000000000000, 450.0000000000002274, 1.202422573753698876 ) ) ;
#16178 = CARTESIAN_POINT ( 'NONE',  ( -9.366249310892840185, -5.000000000000000888, -18.69166165298246085 ) ) ;
#16180 = CARTESIAN_POINT ( 'NONE',  ( -9.442659817596066318, -51.55747247252177345, 30.29540378708609794 ) ) ;
#16179 = CARTESIAN_POINT ( 'NONE',  ( -78.30510816835224830, -30.00000000001010036, 184.2198921887762140 ) ) ;
#16181 = CARTESIAN_POINT ( 'NONE',  ( -42.75482810540037804, 382.1613480202358346, 18.98079264414366918 ) ) ;
#16182 = CARTESIAN_POINT ( 'NONE',  ( 28.25162732096593032, 316.4114759038795910, 11.76994533560096556 ) ) ;
#16183 = DIRECTION ( 'NONE',  ( 0.000000000000000000, -1.000000000000000000, 0.000000000000000000 ) ) ;
#16184 = CARTESIAN_POINT ( 'NONE',  ( 3.313708498984762052, -33.21875000000000000, -8.000000000000000000 ) ) ;
#16185 = CARTESIAN_POINT ( 'NONE',  ( 5.700000000000000178, 0.000000000000000000, 4.000000000000000000 ) ) ;
#16186 = CARTESIAN_POINT ( 'NONE',  ( 29.68315524076926337, -1.200000000000000030E-05, -39.60535821593530414 ) ) ;
#16187 = ORIENTED_EDGE ( 'NONE', *, *, #19931, .T. ) ;
#16188 = CARTESIAN_POINT ( 'NONE',  ( 83.05676702380381471, -42.97589841844901315, 175.6755486148402099 ) ) ;
#16189 = CARTESIAN_POINT ( 'NONE',  ( 4.784092644813104478, -14.50372857256071235, -7.881152805799183092 ) ) ;
#16190 = CARTESIAN_POINT ( 'NONE',  ( -41.87449068006959862, 436.7861666052169767, 20.35960683049020048 ) ) ;
#16191 = ORIENTED_EDGE ( 'NONE', *, *, #49809, .T. ) ;
#16192 = CARTESIAN_POINT ( 'NONE',  ( 6.563035550597769330, -3.302680408004400991, 6.845819698387220598 ) ) ;
#16193 = CONICAL_SURFACE ( 'NONE', #90263, 4.000000000000001776, 0.9599310885968774798 ) ;
#16194 = CARTESIAN_POINT ( 'NONE',  ( 7.499143977329139510, -3.006661276311841213, -20.23006715386459220 ) ) ;
#16195 = CARTESIAN_POINT ( 'NONE',  ( 40.36577318854557461, 468.8231693121321655, -0.04448211817721040712 ) ) ;
#16196 = PLANE ( 'NONE',  #103724 ) ;
#16197 = CARTESIAN_POINT ( 'NONE',  ( 43.00000000000000000, 450.0000000000002274, 13.20242257375370976 ) ) ;
#16198 = CARTESIAN_POINT ( 'NONE',  ( -44.20231929237294821, 435.2535292332385097, 14.52165647984114294 ) ) ;
#16199 = AXIS2_PLACEMENT_3D ( 'NONE', #74281, #72691, #358 ) ;
#16200 = ADVANCED_FACE ( 'NONE', ( #50783 ), #98868, .T. ) ;
#16201 =( GEOMETRIC_REPRESENTATION_CONTEXT ( 3 ) GLOBAL_UNCERTAINTY_ASSIGNED_CONTEXT ( ( #90975 ) ) GLOBAL_UNIT_ASSIGNED_CONTEXT ( ( #100830, #67428, #16739 ) ) REPRESENTATION_CONTEXT ( 'NONE', 'WORKASPACE' ) );
#16202 = SURFACE_STYLE_USAGE ( .BOTH. , #90097 ) ;
#16203 = DIRECTION ( 'NONE',  ( -0.000000000000000000, 1.000000000000000000, 0.000000000000000000 ) ) ;
#16204 = CYLINDRICAL_SURFACE ( 'NONE', #18763, 4.000000000000000888 ) ;
#16205 = ADVANCED_FACE ( 'NONE', ( #85306 ), #58915, .T. ) ;
#16207 = CARTESIAN_POINT ( 'NONE',  ( -10.10574779088694441, 15.34502448090799653, -10.31986842472087673 ) ) ;
#16206 = CARTESIAN_POINT ( 'NONE',  ( -8.658620422836460051, -19.69050060409069758, 35.27988606632377611 ) ) ;
#16208 = CARTESIAN_POINT ( 'NONE',  ( -7.188101187500000044, -13.90625000204838457, -8.802885111219163269E-16 ) ) ;
#16209 = CARTESIAN_POINT ( 'NONE',  ( -28.94897463965919471, 18.87963818668123395, -39.84074594005996772 ) ) ;
#16210 = ORIENTED_EDGE ( 'NONE', *, *, #62542, .F. ) ;
#16211 = EDGE_CURVE ( 'NONE', #27527, #7464, #83695, .T. ) ;
#16212 = CARTESIAN_POINT ( 'NONE',  ( -19.31075363035708037, 49.87050359945074263, 61.31541196678981009 ) ) ;
#16213 = CARTESIAN_POINT ( 'NONE',  ( 23.97256388385797266, 25.74924427912474911, 30.95680134856036148 ) ) ;
#16214 = CARTESIAN_POINT ( 'NONE',  ( -9.230092720259007066, 139.8575112583662019, -5.000000000000000888 ) ) ;
#16215 = CARTESIAN_POINT ( 'NONE',  ( -3.400000000000000355, 4.163799117101001052E-16, -1.581124522925831499 ) ) ;
#16216 = DIRECTION ( 'NONE',  ( -1.000000000000000000, -0.000000000000000000, -0.000000000000000000 ) ) ;
#16217 = COLOUR_RGB ( '', 0.08235294, 0.09019608, 0.10196078) ;
#16218 = EDGE_LOOP ( 'NONE', ( #15997, #23239, #39573, #87353 ) ) ;
#16219 = CARTESIAN_POINT ( 'NONE',  ( -5.980543423763064581, -88.97096407501076953, -0.5500789318242851333 ) ) ;
#16220 = CARTESIAN_POINT ( 'NONE',  ( -4.962805741472906540, 51.42064187080856641, 8.490339940873784741 ) ) ;
#16221 = VERTEX_POINT ( 'NONE', #1712 ) ;
#16222 =( NAMED_UNIT ( * ) SI_UNIT ( $, .STERADIAN. ) SOLID_ANGLE_UNIT ( ) );
#16223 = LINE ( 'NONE', #98208, #87311 ) ;
#16224 = VECTOR ( 'NONE', #48274, 1000.000000000000000 ) ;
#16225 = CARTESIAN_POINT ( 'NONE',  ( -103.7468799687159873, -59.99999999999999289, 102.9567143256649189 ) ) ;
#16226 = CYLINDRICAL_SURFACE ( 'NONE', #77311, 8.000000000000000000 ) ;
#16227 = CARTESIAN_POINT ( 'NONE',  ( 43.68988669995316343, 484.5122128850408671, 2.637743764868108354 ) ) ;
#16228 = VECTOR ( 'NONE', #47793, 1000.000000000000000 ) ;
#16229 = CARTESIAN_POINT ( 'NONE',  ( 27.57151080649627417, 314.0751515626058676, 12.18133379269485239 ) ) ;
#16231 = CARTESIAN_POINT ( 'NONE',  ( -14.32829664253850765, 0.6308854439496920374, 14.98913826414629824 ) ) ;
#16230 = APPLICATION_CONTEXT ( 'automotive_design' ) ;
#16233 = CARTESIAN_POINT ( 'NONE',  ( 30.00000000000000355, 489.0575207958582382, 4.971052219124123539 ) ) ;
#16232 = CARTESIAN_POINT ( 'NONE',  ( -1.570796324980114456, -5.000000000000002665, -73.00000000000001421 ) ) ;
#16234 = CARTESIAN_POINT ( 'NONE',  ( -81.24902549186542444, -60.56381191490225291, 184.6567455024997457 ) ) ;
#16235 = EDGE_LOOP ( 'NONE', ( #27180, #23625, #45310, #84678, #55412 ) ) ;
#16236 = MECHANICAL_DESIGN_GEOMETRIC_PRESENTATION_REPRESENTATION (  '', ( #4106 ), #85164 ) ;
#16237 = PRESENTATION_STYLE_ASSIGNMENT (( #31919 ) ) ;
#16238 = ORIENTED_EDGE ( 'NONE', *, *, #58104, .T. ) ;
#16239 = ORIENTED_EDGE ( 'NONE', *, *, #18891, .T. ) ;
#16240 = FACE_BOUND ( 'NONE', #65381, .T. ) ;
#16241 = EDGE_CURVE ( 'NONE', #7939, #30765, #85861, .T. ) ;
#16242 = CARTESIAN_POINT ( 'NONE',  ( 0.000000000000000000, 80.00000000000000000, 0.000000000000000000 ) ) ;
#16243 = ORIENTED_EDGE ( 'NONE', *, *, #35361, .T. ) ;
#16244 = CARTESIAN_POINT ( 'NONE',  ( -6.663826174190587537, 304.7444947287337413, 9.914190384935233524 ) ) ;
#16245 = CARTESIAN_POINT ( 'NONE',  ( 0.000000000000000000, 0.000000000000000000, 4.000000000000000888 ) ) ;
#16246 =( NAMED_UNIT ( * ) SI_UNIT ( $, .STERADIAN. ) SOLID_ANGLE_UNIT ( ) );
#16247 = CARTESIAN_POINT ( 'NONE',  ( 4.474875413804290325, 9.478657632136659572, -5.000000000000000000 ) ) ;
#16248 = CARTESIAN_POINT ( 'NONE',  ( -10.36961810765524206, -5.000000000000000000, -92.92744404105623346 ) ) ;
#16249 = DIRECTION ( 'NONE',  ( -0.000000000000000000, -1.000000000000000000, -0.000000000000000000 ) ) ;
#16250 = EDGE_CURVE ( 'NONE', #16689, #26284, #67538, .T. ) ;
#16251 = MANIFOLD_SOLID_BREP ( 'CirPattern1', #99654 ) ;
#16252 = CARTESIAN_POINT ( 'NONE',  ( 109.5916899561874942, -30.00000000000003197, 172.2594225519244446 ) ) ;
#16253 = CARTESIAN_POINT ( 'NONE',  ( -105.6361520504002840, -30.00000000000002132, 194.5259906914266139 ) ) ;
#16254 = CARTESIAN_POINT ( 'NONE',  ( -60.20847870758737486, -56.86770172147161873, 81.17039900336807534 ) ) ;
#16255 = ORIENTED_EDGE ( 'NONE', *, *, #104668, .F. ) ;
#16256 = CARTESIAN_POINT ( 'NONE',  ( -22.83134759184064677, 38.95245226452999532, 59.50471635465192577 ) ) ;
#16257 = CARTESIAN_POINT ( 'NONE',  ( 114.5004563705182221, -60.00000000000000000, 167.5904344248802431 ) ) ;
#16258 = ORIENTED_EDGE ( 'NONE', *, *, #50420, .T. ) ;
#16259 = CARTESIAN_POINT ( 'NONE',  ( 13.80753398876933247, -57.17957583240082897, 24.67600335260435074 ) ) ;
#16260 = CARTESIAN_POINT ( 'NONE',  ( 5.082755093536324154, -15.21875000204838457, 5.082755093536326818 ) ) ;
#16261 = SURFACE_SIDE_STYLE ('',( #73423 ) ) ;
#16262 = ORIENTED_EDGE ( 'NONE', *, *, #27462, .F. ) ;
#16263 = CARTESIAN_POINT ( 'NONE',  ( 6.889848939933039595, -30.00000000000001066, 2.062583278641663576 ) ) ;
#16264 = ORIENTED_EDGE ( 'NONE', *, *, #40608, .F. ) ;
#16265 = SURFACE_STYLE_FILL_AREA ( #7626 ) ;
#16266 = VECTOR ( 'NONE', #100704, 1000.000000000000000 ) ;
#16267 = CARTESIAN_POINT ( 'NONE',  ( -111.6028829027016940, -59.99999999999997158, 183.7673010694335574 ) ) ;
#16268 = CARTESIAN_POINT ( 'NONE',  ( 9.521335790331885818, -56.44303812043972357, 23.93938989165062026 ) ) ;
#16269 = CARTESIAN_POINT ( 'NONE',  ( 5.082755093536325930, -25.34375000204838813, -5.082755093536325042 ) ) ;
#16270 = CARTESIAN_POINT ( 'NONE',  ( 45.99999999999999289, 462.0285355451086957, 5.456504273769160918 ) ) ;
#16271 = CARTESIAN_POINT ( 'NONE',  ( -23.54393690455800936, 28.03570273098069876, -30.73873073986574411 ) ) ;
#16272 = CIRCLE ( 'NONE', #61097, 2.000000000000000000 ) ;
#16273 = CARTESIAN_POINT ( 'NONE',  ( -32.84237740334621236, 485.2251842821281116, 5.746442123025396143 ) ) ;
#16274 = FACE_OUTER_BOUND ( 'NONE', #88106, .T. ) ;
#16275 = CARTESIAN_POINT ( 'NONE',  ( 14.61159326615946163, -7.489307139270665381, 13.00852779383240510 ) ) ;
#16276 = CARTESIAN_POINT ( 'NONE',  ( -35.60192394405001437, 303.3476854347574090, -0.05210932705592784958 ) ) ;
#16277 = ADVANCED_FACE ( 'NONE', ( #26583 ), #87443, .F. ) ;
#16278 = CARTESIAN_POINT ( 'NONE',  ( 85.18902050349326771, -60.00000000000000000, -15.68190703514374107 ) ) ;
#16279 = CONICAL_SURFACE ( 'NONE', #69653, 4.172000000000001485, 0.9599310885968750373 ) ;
#16280 = CARTESIAN_POINT ( 'NONE',  ( -33.11049135242710406, -49.90384961613743542, 36.32409600320708165 ) ) ;
#16281 = CARTESIAN_POINT ( 'NONE',  ( -2.067305840858939536, -49.86416495495519285, 102.1177254334556181 ) ) ;
#16282 = CARTESIAN_POINT ( 'NONE',  ( 39.55699615616754272, -25.68728013176338365, 35.29738370701448247 ) ) ;
#16283 = DIRECTION ( 'NONE',  ( 0.000000000000000000, -1.000000000000000000, 0.000000000000000000 ) ) ;
#16284 = ORIENTED_EDGE ( 'NONE', *, *, #79485, .T. ) ;
#16285 = CARTESIAN_POINT ( 'NONE',  ( -7.999912353029504430, 88.99982470603096374, -0.2691822806795016731 ) ) ;
#16286 = CARTESIAN_POINT ( 'NONE',  ( -81.55799083263947580, -38.84168887015896132, 195.3484558550406405 ) ) ;
#16287 = ORIENTED_EDGE ( 'NONE', *, *, #74546, .T. ) ;
#16289 = CARTESIAN_POINT ( 'NONE',  ( -42.89842744829972077, 435.5680593355726842, 8.824050052237332409 ) ) ;
#16288 = CARTESIAN_POINT ( 'NONE',  ( -3.999994092537668244, -10.00072617203139380, 6.928206640937045080 ) ) ;
#16290 = CARTESIAN_POINT ( 'NONE',  ( -10.17232223684046311, 15.97894553443599719, 10.19325617881414914 ) ) ;
#16291 = CARTESIAN_POINT ( 'NONE',  ( 16.66949223230267307, 36.40081923159284116, 24.30698433968582606 ) ) ;
#16292 = CARTESIAN_POINT ( 'NONE',  ( -6.933421966067523812, 41.67527023642382034, -59.13217477274009326 ) ) ;
#16293 = LINE ( 'NONE', #8201, #4537 ) ;
#16294 = CARTESIAN_POINT ( 'NONE',  ( -37.56673239365851913, 25.75719283951025673, 10.95617127780993449 ) ) ;
#16295 = CARTESIAN_POINT ( 'NONE',  ( -27.41598304250715401, 312.9579576083220900, 10.89685229489437646 ) ) ;
#16296 = CARTESIAN_POINT ( 'NONE',  ( 104.9332722526575168, -60.00000000000000711, 109.9670046731016697 ) ) ;
#16297 = DIRECTION ( 'NONE',  ( 0.000000000000000000, -1.000000000000000000, 0.000000000000000000 ) ) ;
#16298 = CARTESIAN_POINT ( 'NONE',  ( -38.86575330739522371, 477.1834804722099079, -1.710715794009403989 ) ) ;
#16299 = VERTEX_POINT ( 'NONE', #5449 ) ;
#16300 = EDGE_CURVE ( 'NONE', #17856, #16922, #71756, .T. ) ;
#16301 = AXIS2_PLACEMENT_3D ( 'NONE', #14696, #47068, #63815 ) ;
#16302 = CARTESIAN_POINT ( 'NONE',  ( -98.27005700444449587, -30.00000000000002132, 190.2025997981200476 ) ) ;
#16303 = VERTEX_POINT ( 'NONE', #11934 ) ;
#16304 = CARTESIAN_POINT ( 'NONE',  ( -9.336538098104073313, -56.01031256472166575, 30.58506923019146839 ) ) ;
#16305 = CARTESIAN_POINT ( 'NONE',  ( -15.93923796801708015, 3.103382665673234619, 0.7338764875060157511 ) ) ;
#16306 = CARTESIAN_POINT ( 'NONE',  ( 4.699999999999999289, 3.752776749732553263, -6.499999999999999112 ) ) ;
#16307 = CARTESIAN_POINT ( 'NONE',  ( 9.380894568449074100, 27.98869366889058696, -3.467341429141167719 ) ) ;
#16308 = CARTESIAN_POINT ( 'NONE',  ( -7.188101187500001821, -27.87500000204838457, -2.977408999572651371 ) ) ;
#16309 = CARTESIAN_POINT ( 'NONE',  ( -4.472135954999579610, -85.00000000000000000, -4.000000000000001776 ) ) ;
#16310 = CARTESIAN_POINT ( 'NONE',  ( 7.150000000000015454, 41.65000000000000568, -68.91429206202192859 ) ) ;
#16311 = ORIENTED_EDGE ( 'NONE', *, *, #355, .T. ) ;
#16312 = AXIS2_PLACEMENT_3D ( 'NONE', #22772, #88547, #55609 ) ;
#16313 = AXIS2_PLACEMENT_3D ( 'NONE', #42808, #75161, #18561 ) ;
#16314 = CIRCLE ( 'NONE', #76590, 6.499999999999999112 ) ;
#16315 = AXIS2_PLACEMENT_3D ( 'NONE', #48230, #23474, #31043 ) ;
#16317 = ORIENTED_EDGE ( 'NONE', *, *, #54899, .T. ) ;
#16316 = CARTESIAN_POINT ( 'NONE',  ( -7.126148247341459019, 41.12758119229484066, -58.55282700859728351 ) ) ;
#16318 = CARTESIAN_POINT ( 'NONE',  ( 79.61275247625323459, -56.85118161666118652, 165.3693179662261912 ) ) ;
#16319 = DIRECTION ( 'NONE',  ( 0.000000000000000000, 0.000000000000000000, 1.000000000000000000 ) ) ;
#16320 = SURFACE_STYLE_FILL_AREA ( #91297 ) ;
#16321 = ORIENTED_EDGE ( 'NONE', *, *, #36108, .T. ) ;
#16322 = SURFACE_SIDE_STYLE ('',( #628 ) ) ;
#16323 = CARTESIAN_POINT ( 'NONE',  ( 7.897196874019792645, -88.79127204167808429, -1.302055520192090032 ) ) ;
#16324 = CARTESIAN_POINT ( 'NONE',  ( -2.977408999572650039, -14.18750000204838457, -7.188101187500000933 ) ) ;
#16325 = CARTESIAN_POINT ( 'NONE',  ( 7.934914944860278041, 26.13154352799888258, -1.051261972695687774 ) ) ;
#16326 = AXIS2_PLACEMENT_3D ( 'NONE', #93540, #34794, #26183 ) ;
#16327 = CARTESIAN_POINT ( 'NONE',  ( 2.272164087111425257, -60.00000000000000000, -36.90211091601013749 ) ) ;
#16328 = CARTESIAN_POINT ( 'NONE',  ( -32.63902298026128079, 347.2392149251367641, 20.22000167947927451 ) ) ;
#16329 = CARTESIAN_POINT ( 'NONE',  ( 32.62207953394533178, 1.482358050883964840E-15, 0.000000000000000000 ) ) ;
#16330 = EDGE_CURVE ( 'NONE', #3167, #12701, #87970, .T. ) ;
#16331 = VERTEX_POINT ( 'NONE', #55562 ) ;
#16332 =( NAMED_UNIT ( * ) PLANE_ANGLE_UNIT ( ) SI_UNIT ( $, .RADIAN. ) );
#16333 = B_SPLINE_CURVE_WITH_KNOTS ( 'NONE', 3,
 ( #77147, #43187, #18401, #93867, #60461, #36204 ),
 .UNSPECIFIED., .F., .F.,
 ( 4, 2, 4 ),
 ( 0.000000000000000000, 0.0004189869898914156798, 0.0008379739797828313595 ),
 .UNSPECIFIED. ) ;
#16334 = CARTESIAN_POINT ( 'NONE',  ( 5.799999999999999822, -4.618802153517009401, -8.000000000000001776 ) ) ;
#16336 = CARTESIAN_POINT ( 'NONE',  ( 7.500000000000007105, 40.28750351091937176, -59.87155384411956760 ) ) ;
#16335 = SHAPE_REPRESENTATION ( '1. Base', ( #10728 ), #103758 ) ;
#16337 = EDGE_CURVE ( 'NONE', #66185, #3581, #18986, .T. ) ;
#16338 = DIRECTION ( 'NONE',  ( -0.000000000000000000, -0.000000000000000000, 1.000000000000000000 ) ) ;
#16339 = CARTESIAN_POINT ( 'NONE',  ( -7.188101187500002709, -30.31250000204838813, 2.977408999572648707 ) ) ;
#16340 = CARTESIAN_POINT ( 'NONE',  ( 23.92965011663618213, -28.31131868122402295, 37.91106159048879931 ) ) ;
#16341 = CARTESIAN_POINT ( 'NONE',  ( 9.673800154114779559, 15.30085158940939571, 2.563280883360070206 ) ) ;
#16342 = CARTESIAN_POINT ( 'NONE',  ( -1.000000000000000222, -32.36379547066005813, -3.982563152095341952 ) ) ;
#16343 = CARTESIAN_POINT ( 'NONE',  ( 37.72766253904391931, 438.6261178958072264, 23.63852112544520523 ) ) ;
#16344 = SHAPE_DEFINITION_REPRESENTATION ( #52755, #25516 ) ;
#16345 = CARTESIAN_POINT ( 'NONE',  ( 48.55396075288199853, 8.676907163023365399, 16.74236275264500051 ) ) ;
#16346 = ORIENTED_EDGE ( 'NONE', *, *, #14245, .F. ) ;
#16347 = EDGE_CURVE ( 'NONE', #78006, #55436, #30024, .T. ) ;
#16348 = CARTESIAN_POINT ( 'NONE',  ( 43.61212006920802509, 434.3223099624050860, 14.49719201759555354 ) ) ;
#16349 = LINE ( 'NONE', #8253, #41134 ) ;
#16350 = AXIS2_PLACEMENT_3D ( 'NONE', #100300, #67943, #26992 ) ;
#16351 = CARTESIAN_POINT ( 'NONE',  ( -58.62616826898538847, -30.00000000000000000, 63.65786219019150849 ) ) ;
#16352 = LINE ( 'NONE', #56260, #58323 ) ;
#16353 = CARTESIAN_POINT ( 'NONE',  ( -19.42937650476450173, 49.96296734528215211, 60.82359239913852633 ) ) ;
#16354 = VERTEX_POINT ( 'NONE', #95010 ) ;
#16355 = CARTESIAN_POINT ( 'NONE',  ( -7.500000000000004441, 24.91666666666666430, -71.71180648257555390 ) ) ;
#16356 = CARTESIAN_POINT ( 'NONE',  ( 97.43174647595270699, -57.67122121763508602, 52.28073263135593862 ) ) ;
#16357 = SURFACE_STYLE_USAGE ( .BOTH. , #142 ) ;
#16358 = CARTESIAN_POINT ( 'NONE',  ( 3.866984248298421356, 16.79585448967792516, 5.835281178490491882 ) ) ;
#16359 = DIRECTION ( 'NONE',  ( 1.000000000000000000, 0.000000000000000000, 0.000000000000000000 ) ) ;
#16360 = CARTESIAN_POINT ( 'NONE',  ( 55.22048556069530889, 40.83906611472065862, 34.80214219327351799 ) ) ;
#16361 = CARTESIAN_POINT ( 'NONE',  ( -76.88100059106110962, -59.99999999999998579, 190.1002214371410162 ) ) ;
#16362 =( NAMED_UNIT ( * ) SI_UNIT ( $, .STERADIAN. ) SOLID_ANGLE_UNIT ( ) );
#16363 = FACE_OUTER_BOUND ( 'NONE', #44200, .T. ) ;
#16364 = CARTESIAN_POINT ( 'NONE',  ( -22.20318009218133071, 295.0333587257888439, 9.975590323731541531 ) ) ;
#16365 = CARTESIAN_POINT ( 'NONE',  ( -84.09290747704537239, -53.79517231171755043, 189.0853069011170362 ) ) ;
#16366 = ORIENTED_EDGE ( 'NONE', *, *, #33907, .F. ) ;
#16367 = CARTESIAN_POINT ( 'NONE',  ( 23.66013301062279695, 305.5857861401792661, -8.841988464366599132 ) ) ;
#16368 = VERTEX_POINT ( 'NONE', #21146 ) ;
#16369 = CARTESIAN_POINT ( 'NONE',  ( 16.01236936003240885, 3.722446712626720888, -0.6596918664728864679 ) ) ;
#16370 = ADVANCED_FACE ( 'NONE', ( #53977 ), #102294, .T. ) ;
#16372 = DIRECTION ( 'NONE',  ( 0.000000000000000000, -1.000000000000000000, 0.000000000000000000 ) ) ;
#16371 = VECTOR ( 'NONE', #37974, 1000.000000000000000 ) ;
#16373 = CARTESIAN_POINT ( 'NONE',  ( -86.01413558773862178, -60.22748779183664425, -14.08703606452684376 ) ) ;
#16374 = CARTESIAN_POINT ( 'NONE',  ( -43.33388476023132085, 464.9733321035732274, 13.99141793828976610 ) ) ;
#16375 = CARTESIAN_POINT ( 'NONE',  ( 0.000000000000000000, 0.000000000000000000, 0.000000000000000000 ) ) ;
#16376 = ORIENTED_EDGE ( 'NONE', *, *, #38291, .F. ) ;
#16377 = DIRECTION ( 'NONE',  ( 0.000000000000000000, 0.000000000000000000, -1.000000000000000000 ) ) ;
#16378 = CARTESIAN_POINT ( 'NONE',  ( 14.11595029532510104, 2.410436752314617959, -5.024000119269091513 ) ) ;
#16379 = EDGE_CURVE ( 'NONE', #21078, #62090, #19655, .T. ) ;
#16380 = ADVANCED_FACE ( 'NONE', ( #64231 ), #67870, .T. ) ;
#16381 = CARTESIAN_POINT ( 'NONE',  ( 8.569529079650926917, -1.734723475976807094E-15, 14.86825985027943808 ) ) ;
#16382 = CARTESIAN_POINT ( 'NONE',  ( -36.57768354961639545, 437.5705742298923724, 4.260889744331883833 ) ) ;
#16383 = CARTESIAN_POINT ( 'NONE',  ( 42.61132677773223065, -60.00000000000003553, -41.65900251181847125 ) ) ;
#16384 = CARTESIAN_POINT ( 'NONE',  ( -78.83331469179402973, -18.67150368877627997, 121.1180772619996162 ) ) ;
#16385 = CIRCLE ( 'NONE', #64661, 3.400000000000000355 ) ;
#16386 = VERTEX_POINT ( 'NONE', #6492 ) ;
#16387 = CARTESIAN_POINT ( 'NONE',  ( 31.98199460507809277, -29.99999999999994316, 41.00477363309762779 ) ) ;
#16388 = CARTESIAN_POINT ( 'NONE',  ( 55.00571552735602410, 6.975173280561618775E-15, 0.000000000000000000 ) ) ;
#16389 = CARTESIAN_POINT ( 'NONE',  ( 112.4234441501388204, -57.67115680235927755, 189.8840207355380585 ) ) ;
#16390 = COLOUR_RGB ( '', 0.31764706, 0.68627451, 0.89019608) ;
#16392 = ORIENTED_EDGE ( 'NONE', *, *, #52749, .F. ) ;
#16391 = CONICAL_SURFACE ( 'NONE', #76674, 3.309500000000001663, 0.9599310885968770357 ) ;
#16393 = CARTESIAN_POINT ( 'NONE',  ( -89.99999999999997158, -52.00000000000000000, 198.0238439516549818 ) ) ;
#16394 = COLOUR_RGB ( '', 0.09019608, 0.27058824, 0.51372549) ;
#16395 = B_SPLINE_CURVE_WITH_KNOTS ( 'NONE', 3,
 ( #68796, #68251, #92511, #10003 ),
 .UNSPECIFIED., .F., .F.,
 ( 4, 4 ),
 ( 0.000000000000000000, 0.003262827847964568182 ),
 .UNSPECIFIED. ) ;
#16396 = DIRECTION ( 'NONE',  ( 1.000000000000000000, 0.000000000000000000, -0.000000000000000000 ) ) ;
#16397 = EDGE_LOOP ( 'NONE', ( #65278, #82030, #46752, #83283, #924 ) ) ;
#16398 =( GEOMETRIC_REPRESENTATION_CONTEXT ( 3 ) GLOBAL_UNCERTAINTY_ASSIGNED_CONTEXT ( ( #18563 ) ) GLOBAL_UNIT_ASSIGNED_CONTEXT ( ( #104499, #30647, #48380 ) ) REPRESENTATION_CONTEXT ( 'NONE', 'WORKASPACE' ) );
#16399 = FACE_OUTER_BOUND ( 'NONE', #70062, .T. ) ;
#16400 = DIRECTION ( 'NONE',  ( 1.000000000000000000, 0.000000000000000000, -0.000000000000000000 ) ) ;
#16401 = CARTESIAN_POINT ( 'NONE',  ( -5.082755093536325042, -21.59375000204838457, -5.082755093536325930 ) ) ;
#16402 = CARTESIAN_POINT ( 'NONE',  ( 2.352174619733123695, -7.302225387960472602, -7.450218641349906967 ) ) ;
#16403 = CONICAL_SURFACE ( 'NONE', #21595, 4.000000000000007105, 0.9599310885968835860 ) ;
#16404 = CARTESIAN_POINT ( 'NONE',  ( 9.165151389911681434, 84.73680493705116135, 4.000000000000001776 ) ) ;
#16405 = DIRECTION ( 'NONE',  ( -1.000000000000000000, -0.000000000000000000, -0.000000000000000000 ) ) ;
#16406 = CARTESIAN_POINT ( 'NONE',  ( -7.499999999999999112, 4.651022038490012278, -7.928862870699868282 ) ) ;
#16407 = CARTESIAN_POINT ( 'NONE',  ( -6.999999999999999112, -14.05766640829038394, -5.232782735144285269 ) ) ;
#16408 = ADVANCED_FACE ( 'NONE', ( #24317 ), #40309, .T. ) ;
#16409 = ORIENTED_EDGE ( 'NONE', *, *, #85983, .F. ) ;
#16410 = CARTESIAN_POINT ( 'NONE',  ( -6.819782170910313468, 41.52802923942638103, -70.37695045795369708 ) ) ;
#16412 = CARTESIAN_POINT ( 'NONE',  ( 29.49176342059628197, -46.43232445692602539, 34.17932786961914360 ) ) ;
#16411 = CARTESIAN_POINT ( 'NONE',  ( 6.243930039575695118E-05, -60.00000000000000000, 42.00000000000000711 ) ) ;
#16413 = CARTESIAN_POINT ( 'NONE',  ( 35.46821841662498542, 430.5464760133320965, 5.814236037882207775 ) ) ;
#16414 = ORIENTED_EDGE ( 'NONE', *, *, #76256, .T. ) ;
#16415 = EDGE_CURVE ( 'NONE', #95473, #16098, #56633, .T. ) ;
#16416 = ORIENTED_EDGE ( 'NONE', *, *, #8892, .T. ) ;
#16418 = CARTESIAN_POINT ( 'NONE',  ( 0.7814291517363842754, 52.07069370489680438, 8.010806432753755146 ) ) ;
#16417 = SURFACE_STYLE_FILL_AREA ( #90309 ) ;
#16419 = CARTESIAN_POINT ( 'NONE',  ( 31.36650669486618881, 1.474610560812782335E-15, 0.000000000000000000 ) ) ;
#16420 = CARTESIAN_POINT ( 'NONE',  ( 35.59999999999999432, -3.309499999999999886, 4.475777889183790779E-16 ) ) ;
#16421 = DIRECTION ( 'NONE',  ( 0.000000000000000000, 0.000000000000000000, -1.000000000000000000 ) ) ;
#16422 = DIRECTION ( 'NONE',  ( 0.000000000000000000, 0.000000000000000000, 1.000000000000000000 ) ) ;
#16423 = CARTESIAN_POINT ( 'NONE',  ( 1.106266637551095000, 17.29082734553924539, -49.90197654099129920 ) ) ;
#16424 = VERTEX_POINT ( 'NONE', #65804 ) ;
#16425 = CARTESIAN_POINT ( 'NONE',  ( 11.77556225125753642, -59.99999999999999289, -42.34068502047673377 ) ) ;
#16426 = CARTESIAN_POINT ( 'NONE',  ( 23.21751746555220564, 25.98869614573808917, -30.70617127781077116 ) ) ;
#16428 = CARTESIAN_POINT ( 'NONE',  ( -15.10151546872593187, -0.2204499704438013796, 15.00000000000002665 ) ) ;
#16427 = B_SPLINE_CURVE_WITH_KNOTS ( 'NONE', 3,
 ( #31438, #72903, #98775, #49704, #105813, #49157, #82063, #96673, #55645, #82609, #18432, #581, #9766, #100380, #66969, #26543, #91773, #50236 ),
 .UNSPECIFIED., .F., .F.,
 ( 4, 2, 2, 2, 2, 2, 2, 2, 4 ),
 ( 0.01918577306495539495, 0.01998357421775985229, 0.02078137537056430964, 0.02157917652336876352, 0.02237697767617322087, 0.02317477882897767821, 0.02397257998178213556, 0.02477038113458659291, 0.02556818228739105026 ),
 .UNSPECIFIED. ) ;
#16429 = CARTESIAN_POINT ( 'NONE',  ( -9.610124387782905231, -5.000000000000000000, -92.36062461491069087 ) ) ;
#16430 = AXIS2_PLACEMENT_3D ( 'NONE', #3890, #44349, #37351 ) ;
#16431 = DIRECTION ( 'NONE',  ( -1.000000000000000000, -1.224606353822377258E-16, -0.000000000000000000 ) ) ;
#16432 = ORIENTED_EDGE ( 'NONE', *, *, #93021, .T. ) ;
#16433 = CARTESIAN_POINT ( 'NONE',  ( -42.19180677453720563, 462.2931784592652207, 3.389262873192004477 ) ) ;
#16434 = VERTEX_POINT ( 'NONE', #8090 ) ;
#16435 = ORIENTED_EDGE ( 'NONE', *, *, #71644, .T. ) ;
#16436 = CARTESIAN_POINT ( 'NONE',  ( 32.99999999999948130, 488.9035777786946824, 11.52689957822645717 ) ) ;
#16437 = CARTESIAN_POINT ( 'NONE',  ( 20.94716680843786705, 41.83711872324442993, -78.41834032275426125 ) ) ;
#16438 = CARTESIAN_POINT ( 'NONE',  ( -33.66371007201963295, 439.0645587366565792, 24.00940545830350459 ) ) ;
#16439 = CARTESIAN_POINT ( 'NONE',  ( 31.34373427653038746, 325.5152829962089527, 15.50537047965048387 ) ) ;
#16440 = CARTESIAN_POINT ( 'NONE',  ( -42.58760755508850337, 320.1910284125954718, -3.858661461815260818 ) ) ;
#16441 = CARTESIAN_POINT ( 'NONE',  ( -3.329593175259680127, -68.60467830133228517, 13.06284992371192999 ) ) ;
#16442 = CARTESIAN_POINT ( 'NONE',  ( 12.50000000000000711, 34.86365967266531385, -54.17194305995318615 ) ) ;
#16443 = ORIENTED_EDGE ( 'NONE', *, *, #7846, .F. ) ;
#16444 = CARTESIAN_POINT ( 'NONE',  ( -10.20315579733895639, 44.01148501590944306, 12.90779740156163768 ) ) ;
#16445 = ORIENTED_EDGE ( 'NONE', *, *, #53077, .F. ) ;
#16446 = CARTESIAN_POINT ( 'NONE',  ( -7.500000000000007105, 39.99999999999998579, -68.91429205786793943 ) ) ;
#16447 = CARTESIAN_POINT ( 'NONE',  ( 13.68764148674883430, 294.5450735065955996, 9.871802096439328267 ) ) ;
#16448 =( NAMED_UNIT ( * ) PLANE_ANGLE_UNIT ( ) SI_UNIT ( $, .RADIAN. ) );
#16449 = CARTESIAN_POINT ( 'NONE',  ( -78.89501011019794419, -59.99999999999995737, 163.3001588117704159 ) ) ;
#16450 = CARTESIAN_POINT ( 'NONE',  ( 66.84561192680622810, -46.43373246685565903, 95.56824384552960794 ) ) ;
#16451 = CIRCLE ( 'NONE', #35436, 7.499999999992679633 ) ;
#16452 = VERTEX_POINT ( 'NONE', #15121 ) ;
#16453 = CARTESIAN_POINT ( 'NONE',  ( 4.954231026949447170, -46.71441375836365495, 40.29635317557408314 ) ) ;
#16454 = CARTESIAN_POINT ( 'NONE',  ( 5.082755093536324154, -29.84375000204838813, 5.082755093536326818 ) ) ;
#16455 = DIRECTION ( 'NONE',  ( 0.000000000000000000, 0.000000000000000000, 1.000000000000000000 ) ) ;
#16456 = EDGE_CURVE ( 'NONE', #57008, #9879, #47482, .T. ) ;
#16457 = CONICAL_SURFACE ( 'NONE', #99125, 5.000000000000001776, 0.9599310885968803664 ) ;
#16458 = VERTEX_POINT ( 'NONE', #23244 ) ;
#16459 = SHAPE_REPRESENTATION_RELATIONSHIP ( 'NONE' , 'NONE' ,  #19231, #31828 ) ;
#16460 = DIRECTION ( 'NONE',  ( -1.000000000000000000, 0.000000000000000000, 0.000000000000000000 ) ) ;
#16461 = MECHANICAL_DESIGN_GEOMETRIC_PRESENTATION_REPRESENTATION (  '', ( #42327 ), #40631 ) ;
#16462 = VECTOR ( 'NONE', #81015, 1000.000000000000000 ) ;
#16463 = EDGE_CURVE ( 'NONE', #59429, #63495, #9959, .T. ) ;
#16464 = DIRECTION ( 'NONE',  ( -0.000000000000000000, -1.000000000000000000, -0.000000000000000000 ) ) ;
#16465 = EDGE_CURVE ( 'NONE', #4091, #90588, #79873, .T. ) ;
#16466 = CARTESIAN_POINT ( 'NONE',  ( 34.35000000000000142, -3.309499999999999886, 0.000000000000000000 ) ) ;
#16467 =( GEOMETRIC_REPRESENTATION_CONTEXT ( 3 ) GLOBAL_UNCERTAINTY_ASSIGNED_CONTEXT ( ( #73304 ) ) GLOBAL_UNIT_ASSIGNED_CONTEXT ( ( #7352, #105528, #47283 ) ) REPRESENTATION_CONTEXT ( 'NONE', 'WORKASPACE' ) );
#16468 = CARTESIAN_POINT ( 'NONE',  ( 3.313708498984762496, -26.46875000409677625, 7.999999999999998224 ) ) ;
#16469 = CIRCLE ( 'NONE', #37146, 4.000000000000001776 ) ;
#16470 = CARTESIAN_POINT ( 'NONE',  ( 0.1061556211655350773, 6.421950209808282573, 1.876855952934449734 ) ) ;
#16471 = PRESENTATION_LAYER_ASSIGNMENT (  '', '', ( #97376 ) ) ;
#16472 = CARTESIAN_POINT ( 'NONE',  ( 32.46586666336925475, 488.6856797979017415, 9.810357008081247443 ) ) ;
#16473 = VECTOR ( 'NONE', #91346, 1000.000000000000000 ) ;
#16474 = EDGE_CURVE ( 'NONE', #63843, #13645, #47147, .T. ) ;
#16475 = LINE ( 'NONE', #80139, #51632 ) ;
#16476 = CARTESIAN_POINT ( 'NONE',  ( -5.952443285071600698, 4.563276076495102807, 4.999999999999999112 ) ) ;
#16477 = CARTESIAN_POINT ( 'NONE',  ( 7.211357414135266986, -7.988534600655595064, 3.467230644691329466 ) ) ;
#16478 = CYLINDRICAL_SURFACE ( 'NONE', #3945, 1.250000000000001110 ) ;
#16479 = ORIENTED_EDGE ( 'NONE', *, *, #81982, .T. ) ;
#16480 = EDGE_CURVE ( 'NONE', #92048, #33852, #60958, .T. ) ;
#16481 = DIRECTION ( 'NONE',  ( 0.000000000000000000, -0.000000000000000000, -1.000000000000000000 ) ) ;
#16482 = AXIS2_PLACEMENT_3D ( 'NONE', #9824, #83195, #50811 ) ;
#16484 = CARTESIAN_POINT ( 'NONE',  ( -10.28624191511830155, -1.200000000000000030E-05, -15.40779740156157196 ) ) ;
#16483 =( BOUNDED_SURFACE ( )  B_SPLINE_SURFACE ( 3, 2, ( 
 ( #35583, #43637, #101350 ),
 ( #36129, #68997, #101872 ),
 ( #28032, #60903, #44719 ),
 ( #77607, #36656, #69520 ),
 ( #62461, #18845, #85680 ),
 ( #94298, #52760, #68968 ),
 ( #19389, #52221, #70014 ),
 ( #61946, #86749, #68429 ) ),
 .UNSPECIFIED., .F., .F., .F. ) 
 B_SPLINE_SURFACE_WITH_KNOTS ( ( 4, 2, 2, 4 ),
 ( 3, 3 ),
 ( 0.03205733154476830132, 0.03606343422293256662, 0.03806648556201469580, 0.04006953690109683192 ),
 ( 0.000000000000000000, 1.000000000000000000 ),
 .UNSPECIFIED. ) 
 GEOMETRIC_REPRESENTATION_ITEM ( )  RATIONAL_B_SPLINE_SURFACE ( (
 ( 1.000000000000000000, 0.8047781205924506853, 1.000000000000000000),
 ( 1.000000000000000000, 0.8123783054473237009, 1.000000000000000000),
 ( 1.000000000000000000, 0.8190665327891030190, 1.000000000000000000),
 ( 1.000000000000000000, 0.8191934993920665375, 1.000000000000000000),
 ( 1.000000000000000000, 0.8176088856299702501, 1.000000000000000000),
 ( 1.000000000000000000, 0.8122958243107715193, 1.000000000000000000),
 ( 1.000000000000000000, 0.8086309198479471050, 1.000000000000000000),
 ( 1.000000000000000000, 0.8047712443299024354, 1.000000000000000000) ) ) 
 REPRESENTATION_ITEM ( '' )  SURFACE ( )  );
#16485 = CARTESIAN_POINT ( 'NONE',  ( -92.77811343242147757, -29.99999999999999645, 191.0689905325092184 ) ) ;
#16486 = CARTESIAN_POINT ( 'NONE',  ( 0.000000000000000000, 0.000000000000000000, 4.000000000000000000 ) ) ;
#16487 = CARTESIAN_POINT ( 'NONE',  ( 62.75430164509801756, -57.67841677346302021, 117.5347977078399140 ) ) ;
#16489 = CARTESIAN_POINT ( 'NONE',  ( -9.500381993471846087, 53.42959890879150464, 3.608304243553658974 ) ) ;
#16488 = CARTESIAN_POINT ( 'NONE',  ( -1.094645143735793358, 25.39612329712696948, -40.10891261621117110 ) ) ;
#16490 = CARTESIAN_POINT ( 'NONE',  ( -40.19525959765014278, 459.8689882208905146, 1.906254677025774669 ) ) ;
#16491 = CARTESIAN_POINT ( 'NONE',  ( -0.7776801151804421108, 43.26715133920247780, 18.48212775743904501 ) ) ;
#16492 = DIRECTION ( 'NONE',  ( 0.000000000000000000, -1.000000000000000000, 0.000000000000000000 ) ) ;
#16493 = CARTESIAN_POINT ( 'NONE',  ( -5.044614528818932797, -59.99999999999999289, 39.62871590938365784 ) ) ;
#16494 = DIRECTION ( 'NONE',  ( 0.5735764363510557073, -0.8191520442889850262, 1.003171929053516612E-16 ) ) ;
#16495 = CARTESIAN_POINT ( 'NONE',  ( -87.03184277043726524, -39.08917807867680239, 189.1309292593449243 ) ) ;
#16496 = ORIENTED_EDGE ( 'NONE', *, *, #47816, .T. ) ;
#16497 = CARTESIAN_POINT ( 'NONE',  ( 12.37144696128342147, -4.000000000000003553, 20.44658103856077602 ) ) ;
#16498 = CARTESIAN_POINT ( 'NONE',  ( -9.023399056601082435, -18.58633034970281273, 26.98791154383341251 ) ) ;
#16499 = VECTOR ( 'NONE', #105414, 1000.000000000000000 ) ;
#16500 = DIRECTION ( 'NONE',  ( 0.000000000000000000, 1.000000000000000000, 0.000000000000000000 ) ) ;
#16502 = CARTESIAN_POINT ( 'NONE',  ( 2.560557749087981616, -69.78870608840574619, 13.23340540258364584 ) ) ;
#16501 = CARTESIAN_POINT ( 'NONE',  ( -101.5568998084323056, -60.00000000000000000, 194.6300538685317463 ) ) ;
#16503 = VERTEX_POINT ( 'NONE', #39423 ) ;
#16504 = SURFACE_SIDE_STYLE ('',( #83362 ) ) ;
#16505 = CARTESIAN_POINT ( 'NONE',  ( -5.686850908485443057, -4.337623088834303253, -16.91150612931922836 ) ) ;
#16506 = CARTESIAN_POINT ( 'NONE',  ( -7.343637806710344051, 32.44363121900617841, 3.177475076494671313 ) ) ;
#16507 = CARTESIAN_POINT ( 'NONE',  ( 33.15431920332005689, 300.2961132513346456, -0.7782802253148046745 ) ) ;
#16508 = FACE_OUTER_BOUND ( 'NONE', #2586, .T. ) ;
#16509 = EDGE_CURVE ( 'NONE', #93762, #38295, #59260, .T. ) ;
#16510 = CARTESIAN_POINT ( 'NONE',  ( -6.928203230275507885, -85.00000000000000000, -4.000000000000001776 ) ) ;
#16511 = CARTESIAN_POINT ( 'NONE',  ( -43.00000000000000000, 461.4080316921935605, 3.462976341553817949 ) ) ;
#16512 = CARTESIAN_POINT ( 'NONE',  ( 114.3489886862215883, -60.00000000000002842, 164.2602920347584359 ) ) ;
#16513 = CARTESIAN_POINT ( 'NONE',  ( 86.75754961941542831, -2.002967142162725287E-29, 5.000000000000011546 ) ) ;
#16514 = ORIENTED_EDGE ( 'NONE', *, *, #70657, .T. ) ;
#16515 = CARTESIAN_POINT ( 'NONE',  ( -34.92499999999994742, 1.714505518806294638E-15, -14.00000000000000000 ) ) ;
#16516 = CARTESIAN_POINT ( 'NONE',  ( 0.3173508448886485089, -5.375634714784611745, 6.689127551062004962 ) ) ;
#16517 = CARTESIAN_POINT ( 'NONE',  ( -8.559508646656370345, 53.68473964988125857, 4.031152949374564365 ) ) ;
#16518 = CARTESIAN_POINT ( 'NONE',  ( 23.86650669486618881, 1.474610560812782335E-15, 0.000000000000000000 ) ) ;
#16519 = CARTESIAN_POINT ( 'NONE',  ( 43.59493452178210759, 373.1075246076704843, 14.23911768532198430 ) ) ;
#16520 = CARTESIAN_POINT ( 'NONE',  ( 44.28408485722940924, 463.6816916292668793, 7.557853517648653430 ) ) ;
#16521 = ORIENTED_EDGE ( 'NONE', *, *, #53506, .F. ) ;
#16522 = AXIS2_PLACEMENT_3D ( 'NONE', #99005, #24638, #25170 ) ;
#16523 = CARTESIAN_POINT ( 'NONE',  ( -20.20043710121002078, 303.8503592077864255, 9.936692575589569643 ) ) ;
#16524 = ORIENTED_EDGE ( 'NONE', *, *, #89297, .T. ) ;
#16525 = LINE ( 'NONE', #49417, #36279 ) ;
#16526 =( NAMED_UNIT ( * ) PLANE_ANGLE_UNIT ( ) SI_UNIT ( $, .RADIAN. ) );
#16527 = DIRECTION ( 'NONE',  ( 0.000000000000000000, 0.000000000000000000, -1.000000000000000000 ) ) ;
#16528 = CARTESIAN_POINT ( 'NONE',  ( 36.64823341582350480, 437.5392299810053487, 4.281405873620231617 ) ) ;
#16529 = EDGE_LOOP ( 'NONE', ( #39971, #24978, #105122, #77480, #54463, #83624 ) ) ;
#16530 = CIRCLE ( 'NONE', #80266, 5.000000000000002665 ) ;
#16531 = CARTESIAN_POINT ( 'NONE',  ( 5.000000000000040856, -14.59885031841967518, 13.58543933205510079 ) ) ;
#16532 = CARTESIAN_POINT ( 'NONE',  ( -49.37845040383849238, -60.00000000003905853, 76.62573825319901744 ) ) ;
#16533 = CARTESIAN_POINT ( 'NONE',  ( 46.00000000000000000, 438.0901456946865551, 11.29311581785116125 ) ) ;
#16534 = ORIENTED_EDGE ( 'NONE', *, *, #35288, .F. ) ;
#16535 = CARTESIAN_POINT ( 'NONE',  ( 91.88848222090017259, -59.99999999999997158, 9.002118979807052668 ) ) ;
#16536 = AXIS2_PLACEMENT_3D ( 'NONE', #84922, #19171, #40861 ) ;
#16538 = CARTESIAN_POINT ( 'NONE',  ( 17.81248185889901592, -35.99250062930340732, 30.19708477161321269 ) ) ;
#16537 = CARTESIAN_POINT ( 'NONE',  ( -114.2223820868815380, -59.99999999999997868, 162.1253058113985048 ) ) ;
#16540 = CARTESIAN_POINT ( 'NONE',  ( 18.71440884245025060, 61.34242035161803841, 9.357204421225128854 ) ) ;
#16539 = UNCERTAINTY_MEASURE_WITH_UNIT (LENGTH_MEASURE( 1.000000000000000082E-05 ), #17816, 'distance_accuracy_value', 'NONE');
#16541 = DIRECTION ( 'NONE',  ( 0.000000000000000000, 1.000000000000000000, 0.000000000000000000 ) ) ;
#16542 = ADVANCED_FACE ( 'NONE', ( #41523 ), #82517, .T. ) ;
#16543 = CARTESIAN_POINT ( 'NONE',  ( -41.52699401632758480, -22.24292886909580957, 35.91547177849930961 ) ) ;
#16544 = DIRECTION ( 'NONE',  ( -1.000000000000000000, -1.224606353822377258E-16, -0.000000000000000000 ) ) ;
#16545 = ORIENTED_EDGE ( 'NONE', *, *, #99307, .T. ) ;
#16546 = CONICAL_SURFACE ( 'NONE', #57872, 3.309500000000001663, 0.9599310885968770357 ) ;
#16547 = DIRECTION ( 'NONE',  ( -0.000000000000000000, -1.000000000000000000, -0.000000000000000000 ) ) ;
#16548 = AXIS2_PLACEMENT_3D ( 'NONE', #67621, #12016, #36874 ) ;
#16549 = CARTESIAN_POINT ( 'NONE',  ( 16.10373777989397226, 21.82388053252877569, 0.8730104595026707548 ) ) ;
#16550 = CARTESIAN_POINT ( 'NONE',  ( 31.11679462788039530, 441.4271381875185511, 23.27438508043199406 ) ) ;
#16551 = PRESENTATION_LAYER_ASSIGNMENT (  '', '', ( #83680 ) ) ;
#16552 = CARTESIAN_POINT ( 'NONE',  ( 2.499999999999984457, -21.99834388059804269, -30.53959902372158908 ) ) ;
#16553 = EDGE_CURVE ( 'NONE', #44948, #94312, #72814, .T. ) ;
#16554 = CARTESIAN_POINT ( 'NONE',  ( -8.000000000000000000, -28.43750000409677270, -9.797174393178825657E-16 ) ) ;
#16555 = CARTESIAN_POINT ( 'NONE',  ( 9.475800981716794524, -0.4480317257901532124, 19.86715792471738951 ) ) ;
#16556 = VERTEX_POINT ( 'NONE', #64744 ) ;
#16557 =( LENGTH_UNIT ( ) NAMED_UNIT ( * ) SI_UNIT ( .MILLI., .METRE. ) );
#16558 = VERTEX_POINT ( 'NONE', #48541 ) ;
#16559 = CARTESIAN_POINT ( 'NONE',  ( 72.67119523410620729, -30.00000000000000000, -19.29465872568861684 ) ) ;
#16560 = CARTESIAN_POINT ( 'NONE',  ( 46.77752740700951506, 13.53072847091734054, 15.64014710929875740 ) ) ;
#16561 = AXIS2_PLACEMENT_3D ( 'NONE', #105924, #32074, #14793 ) ;
#16562 = DIRECTION ( 'NONE',  ( 0.000000000000000000, 1.000000000000000000, 0.000000000000000000 ) ) ;
#16563 = AXIS2_PLACEMENT_3D ( 'NONE', #55727, #98336, #57327 ) ;
#16564 = CARTESIAN_POINT ( 'NONE',  ( 16.75187969033571989, -1.200000000000000030E-05, 24.30698433968583316 ) ) ;
#16565 = CARTESIAN_POINT ( 'NONE',  ( 98.02403481859347778, -29.99999999999999645, 137.7085981003935444 ) ) ;
#16566 = CARTESIAN_POINT ( 'NONE',  ( -19.83463548332447601, 303.8035096162418540, 9.926734387303332241 ) ) ;
#16567 = ORIENTED_EDGE ( 'NONE', *, *, #28385, .T. ) ;
#16568 = EDGE_LOOP ( 'NONE', ( #82835, #48822, #66187, #14354, #22692 ) ) ;
#16569 = ORIENTED_EDGE ( 'NONE', *, *, #81711, .F. ) ;
#16570 = CIRCLE ( 'NONE', #76844, 2.000000000000000000 ) ;
#16571 = CARTESIAN_POINT ( 'NONE',  ( 0.000000000000000000, 50.00000000000000000, 60.00000000000000000 ) ) ;
#16572 = CARTESIAN_POINT ( 'NONE',  ( -6.531358237270333156, -12.73775376330297782, -7.942398969220734628 ) ) ;
#16573 = CARTESIAN_POINT ( 'NONE',  ( -40.48182439570949498, 464.0838927029486172, 18.36806636631758849 ) ) ;
#16574 = CARTESIAN_POINT ( 'NONE',  ( -32.14109322893018827, 425.0905581414837684, 24.99384153588575685 ) ) ;
#16575 = ORIENTED_EDGE ( 'NONE', *, *, #48575, .F. ) ;
#16576 = CARTESIAN_POINT ( 'NONE',  ( 9.918325909156569864, 108.7923523170742754, 1.298699613733150571 ) ) ;
#16577 = VERTEX_POINT ( 'NONE', #81432 ) ;
#16578 = CARTESIAN_POINT ( 'NONE',  ( 32.92225573320253318, 439.7404251386080318, 24.14402493977489783 ) ) ;
#16579 = CARTESIAN_POINT ( 'NONE',  ( 79.85416194052990591, -38.77095264444343314, 192.7203380926642069 ) ) ;
#16580 = CARTESIAN_POINT ( 'NONE',  ( 5.975663821523083286, 4.257391242883784344, -5.625982059626467802 ) ) ;
#16581 = CARTESIAN_POINT ( 'NONE',  ( 33.70642115557484431, 302.7255462307956009, 11.75075386443325876 ) ) ;
#16582 = CARTESIAN_POINT ( 'NONE',  ( 42.19179521601817839, 485.4956273777428919, -3.824025998174080510 ) ) ;
#16583 = AXIS2_PLACEMENT_3D ( 'NONE', #42387, #74215, #106588 ) ;
#16584 = DIRECTION ( 'NONE',  ( 0.000000000000000000, -1.000000000000000000, 0.000000000000000000 ) ) ;
#16585 = CARTESIAN_POINT ( 'NONE',  ( -5.803898591548167119, -46.53140123172381948, 103.8893302396403868 ) ) ;
#16586 =( LENGTH_UNIT ( ) NAMED_UNIT ( * ) SI_UNIT ( .MILLI., .METRE. ) );
#16587 = LINE ( 'NONE', #39817, #102213 ) ;
#16588 = ORIENTED_EDGE ( 'NONE', *, *, #38880, .T. ) ;
#16589 = CARTESIAN_POINT ( 'NONE',  ( 6.683837171061806082, 7.911893696991934455, 7.436622852660996417E-19 ) ) ;
#16590 = CARTESIAN_POINT ( 'NONE',  ( -23.16554820189585229, 303.5579005584135075, 10.08982211509187010 ) ) ;
#16591 = SURFACE_STYLE_USAGE ( .BOTH. , #57035 ) ;
#16592 = EDGE_CURVE ( 'NONE', #5765, #17391, #23090, .T. ) ;
#16593 = CARTESIAN_POINT ( 'NONE',  ( -14.33580413397241315, 42.00000000000000000, -89.41414995581023106 ) ) ;
#16594 = CARTESIAN_POINT ( 'NONE',  ( -5.656854249492381470, -11.56249999999999289, 5.656854249492379694 ) ) ;
#16595 = DIRECTION ( 'NONE',  ( -1.000000000000000000, -1.224606353822377258E-16, -0.000000000000000000 ) ) ;
#16596 = EDGE_CURVE ( 'NONE', #20391, #42289, #38266, .T. ) ;
#16597 = DIRECTION ( 'NONE',  ( 0.000000000000000000, 1.000000000000000000, 0.000000000000000000 ) ) ;
#16598 = EDGE_CURVE ( 'NONE', #31318, #7161, #36959, .T. ) ;
#16599 =( NAMED_UNIT ( * ) PLANE_ANGLE_UNIT ( ) SI_UNIT ( $, .RADIAN. ) );
#16600 = ORIENTED_EDGE ( 'NONE', *, *, #53947, .F. ) ;
#16601 = CARTESIAN_POINT ( 'NONE',  ( 86.27972295779851208, -24.64005545529337127, 181.9969923761166513 ) ) ;
#16602 = DIRECTION ( 'NONE',  ( 0.000000000000000000, 0.000000000000000000, 1.000000000000000000 ) ) ;
#16603 = CARTESIAN_POINT ( 'NONE',  ( -9.291504854928620105, 140.5441818689093054, 5.000000000000954792 ) ) ;
#16604 = EDGE_LOOP ( 'NONE', ( #80934, #36185, #47905, #91015, #38617, #10962, #48597 ) ) ;
#16605 = CARTESIAN_POINT ( 'NONE',  ( 94.56681692940503581, -57.65518366666022132, -10.45629857477335456 ) ) ;
#16606 = DIRECTION ( 'NONE',  ( -1.000000000000000000, -1.224606353822377258E-16, -0.000000000000000000 ) ) ;
#16607 = LINE ( 'NONE', #7433, #35240 ) ;
#16608 = ADVANCED_FACE ( 'NONE', ( #1023 ), #23161, .T. ) ;
#16609 = CARTESIAN_POINT ( 'NONE',  ( 28.72976249129374082, 13.62251309882733175, 40.04442010369683658 ) ) ;
#16610 = CARTESIAN_POINT ( 'NONE',  ( -80.98592521388407306, -29.99999999999999645, 20.65126904418409026 ) ) ;
#16611 = AXIS2_PLACEMENT_3D ( 'NONE', #91576, #2006, #35487 ) ;
#16612 = CARTESIAN_POINT ( 'NONE',  ( 28.94897463965949314, 18.87963818668124105, 39.84074594005971903 ) ) ;
#16613 = CARTESIAN_POINT ( 'NONE',  ( -6.921856738059538827, 41.59435685020019235, -70.13580383255586526 ) ) ;
#16614 = FACE_OUTER_BOUND ( 'NONE', #50930, .T. ) ;
#16615 = DIRECTION ( 'NONE',  ( 1.000000000000000000, 1.224606353822377258E-16, 0.000000000000000000 ) ) ;
#16616 = CARTESIAN_POINT ( 'NONE',  ( 30.11650669486618881, 1.474610560812782335E-15, 0.000000000000000000 ) ) ;
#16617 = CARTESIAN_POINT ( 'NONE',  ( 0.000000000000000000, 0.000000000000000000, -7.381345277524544279 ) ) ;
#16618 = DIRECTION ( 'NONE',  ( 0.000000000000000000, -1.000000000000000000, 0.000000000000000000 ) ) ;
#16619 = CARTESIAN_POINT ( 'NONE',  ( -34.84618260875176787, 489.9833681528637044, 11.97975507378787619 ) ) ;
#16620 = DIRECTION ( 'NONE',  ( -1.000000000000000000, -1.224606353822377258E-16, -0.000000000000000000 ) ) ;
#16621 = DIRECTION ( 'NONE',  ( -1.000000000000000000, -1.224606353822377258E-16, -0.000000000000000000 ) ) ;
#16622 = AXIS2_PLACEMENT_3D ( 'NONE', #75325, #1425, #52645 ) ;
#16623 = CONICAL_SURFACE ( 'NONE', #52808, 3.309500000000001663, 0.9599310885968770357 ) ;
#16624 = AXIS2_PLACEMENT_3D ( 'NONE', #47017, #22255, #61655 ) ;
#16625 = FACE_OUTER_BOUND ( 'NONE', #81159, .T. ) ;
#16626 = CONICAL_SURFACE ( 'NONE', #47568, 4.172000000000001485, 0.9599310885968750373 ) ;
#16627 = ORIENTED_EDGE ( 'NONE', *, *, #45301, .F. ) ;
#16628 = CARTESIAN_POINT ( 'NONE',  ( 6.289692432696854851, -5.239086202715443896, -4.583616368338468305 ) ) ;
#16629 = CIRCLE ( 'NONE', #95866, 3.400000000000000355 ) ;
#16630 = CARTESIAN_POINT ( 'NONE',  ( 5.299999999999999822, 3.752776749732569694, 6.499999999999997335 ) ) ;
#16631 = DIRECTION ( 'NONE',  ( -1.000000000000000000, -0.000000000000000000, -0.000000000000000000 ) ) ;
#16633 = DIRECTION ( 'NONE',  ( 0.000000000000000000, -1.000000000000000000, 0.000000000000000000 ) ) ;
#16632 = LINE ( 'NONE', #97528, #63951 ) ;
#16634 = ORIENTED_EDGE ( 'NONE', *, *, #91949, .F. ) ;
#16635 = DIRECTION ( 'NONE',  ( 0.000000000000000000, 1.000000000000000000, 0.000000000000000000 ) ) ;
#16636 = ORIENTED_EDGE ( 'NONE', *, *, #68160, .F. ) ;
#16637 = CARTESIAN_POINT ( 'NONE',  ( -25.85202045074685984, 35.07630312271587769, 8.665166400306999250 ) ) ;
#16638 = EDGE_CURVE ( 'NONE', #47158, #20792, #85194, .T. ) ;
#16639 = CARTESIAN_POINT ( 'NONE',  ( 10.61390424674485899, 43.90835935462011008, -12.94086579116563485 ) ) ;
#16640 = DIRECTION ( 'NONE',  ( 0.000000000000000000, 0.000000000000000000, 1.000000000000000000 ) ) ;
#16641 = CARTESIAN_POINT ( 'NONE',  ( -33.37378058036343731, -60.00000000000000000, -40.51130621461524584 ) ) ;
#16642 = ORIENTED_EDGE ( 'NONE', *, *, #18306, .T. ) ;
#16643 = CARTESIAN_POINT ( 'NONE',  ( 71.17283260602091843, -38.00000000000000000, -21.88484610531455488 ) ) ;
#16644 = DIRECTION ( 'NONE',  ( 0.9727555100395958165, 0.000000000000000000, -0.2318333834623605982 ) ) ;
#16645 = CARTESIAN_POINT ( 'NONE',  ( 99.38078780120881106, -60.31955890522991126, 196.1176621183285818 ) ) ;
#16647 = CARTESIAN_POINT ( 'NONE',  ( 18.86650669486618881, 0.000000000000000000, 4.000000000000000888 ) ) ;
#16646 =( LENGTH_UNIT ( ) NAMED_UNIT ( * ) SI_UNIT ( .MILLI., .METRE. ) );
#16648 = CIRCLE ( 'NONE', #47666, 7.000000000000000000 ) ;
#16649 = ORIENTED_EDGE ( 'NONE', *, *, #59776, .F. ) ;
#16650 = ORIENTED_EDGE ( 'NONE', *, *, #81112, .F. ) ;
#16651 = ORIENTED_EDGE ( 'NONE', *, *, #4968, .T. ) ;
#16652 = CARTESIAN_POINT ( 'NONE',  ( 32.01718455759882431, 362.9122997726822746, 22.63193864108178488 ) ) ;
#16653 = ADVANCED_FACE ( 'NONE', ( #92187, #1574 ), #59858, .F. ) ;
#16654 = CARTESIAN_POINT ( 'NONE',  ( -5.000000000000000000, -13.79684580107980985, 10.70524563036346599 ) ) ;
#16655 = CARTESIAN_POINT ( 'NONE',  ( 8.718677345792714917, 53.63232851853486238, 4.031152949374446237 ) ) ;
#16656 = ORIENTED_EDGE ( 'NONE', *, *, #21272, .T. ) ;
#16657 = CARTESIAN_POINT ( 'NONE',  ( 26.11923076923076792, 1.411358822780289120E-15, 0.000000000000000000 ) ) ;
#16658 = DIRECTION ( 'NONE',  ( -1.000000000000000000, 0.000000000000000000, 0.000000000000000000 ) ) ;
#16659 = FACE_OUTER_BOUND ( 'NONE', #84846, .T. ) ;
#16660 = CARTESIAN_POINT ( 'NONE',  ( -9.856791769558052252, -57.67120557387264768, 41.61776228975389813 ) ) ;
#16661 = CARTESIAN_POINT ( 'NONE',  ( 2.977408999572650927, -33.87500000204838813, -7.188101187500001821 ) ) ;
#16662 = DIRECTION ( 'NONE',  ( -1.000000000000000000, -1.224606353822377258E-16, -0.000000000000000000 ) ) ;
#16663 = CARTESIAN_POINT ( 'NONE',  ( -0.1698250053810657911, 25.17129873335319346, 40.74125109472547024 ) ) ;
#16664 = DIRECTION ( 'NONE',  ( 0.000000000000000000, 0.000000000000000000, -1.000000000000000000 ) ) ;
#16665 = CARTESIAN_POINT ( 'NONE',  ( -8.180708021844917965, -14.21045842199436926, -37.25108655295423432 ) ) ;
#16666 = FACE_OUTER_BOUND ( 'NONE', #46662, .T. ) ;
#16667 = CARTESIAN_POINT ( 'NONE',  ( -53.88432441057622668, -39.50293457858858659, 57.94454880366763661 ) ) ;
#16668 = DIRECTION ( 'NONE',  ( 1.000000000000000000, 0.000000000000000000, 0.000000000000000000 ) ) ;
#16669 = VERTEX_POINT ( 'NONE', #100287 ) ;
#16670 = CARTESIAN_POINT ( 'NONE',  ( -99.48109555172277396, -45.25232648423930470, 193.0206739817450625 ) ) ;
#16671 = AXIS2_PLACEMENT_3D ( 'NONE', #92483, #51493, #2940 ) ;
#16672 = CARTESIAN_POINT ( 'NONE',  ( 0.000000000000000000, 294.8518027762758038, -10.00000000000000178 ) ) ;
#16673 = EDGE_CURVE ( 'NONE', #99028, #69704, #36141, .T. ) ;
#16674 = CARTESIAN_POINT ( 'NONE',  ( 12.32678244424858072, -2.923755400730654319, 20.67306671305708576 ) ) ;
#16675 = VERTEX_POINT ( 'NONE', #60394 ) ;
#16676 = CARTESIAN_POINT ( 'NONE',  ( -17.19159652742020228, 43.30607723763039019, 6.534202769278905976 ) ) ;
#16677 = MECHANICAL_DESIGN_GEOMETRIC_PRESENTATION_REPRESENTATION (  '', ( #95920 ), #102843 ) ;
#16678 = CARTESIAN_POINT ( 'NONE',  ( 71.73296838179494728, -38.32718984392275985, 144.1581809263412879 ) ) ;
#16679 = DIRECTION ( 'NONE',  ( 0.000000000000000000, 0.000000000000000000, -1.000000000000000000 ) ) ;
#16680 = CARTESIAN_POINT ( 'NONE',  ( -6.542072687172704626, 51.42643242773939249, -7.321406361055552203 ) ) ;
#16681 = DIRECTION ( 'NONE',  ( -1.000000000000000000, -1.224606353822377258E-16, -0.000000000000000000 ) ) ;
#16682 = CARTESIAN_POINT ( 'NONE',  ( 72.41885610124130324, 42.00000000000000000, 55.65414010178505322 ) ) ;
#16683 = CARTESIAN_POINT ( 'NONE',  ( 85.25629243111305300, -30.00000000000000000, 172.6978005289113298 ) ) ;
#16684 = ADVANCED_FACE ( 'NONE', ( #92729 ), #10734, .T. ) ;
#16685 = CARTESIAN_POINT ( 'NONE',  ( 35.00143047691824449, 490.1822567707094436, 12.08765882793104574 ) ) ;
#16686 = CARTESIAN_POINT ( 'NONE',  ( -35.99391350154813551, 473.1341906942088826, 18.08607326236544921 ) ) ;
#16687 = PRESENTATION_STYLE_ASSIGNMENT (( #6990 ) ) ;
#16688 = ORIENTED_EDGE ( 'NONE', *, *, #44488, .F. ) ;
#16689 = VERTEX_POINT ( 'NONE', #50648 ) ;
#16690 = CARTESIAN_POINT ( 'NONE',  ( 51.69300476518706944, -60.30369315783265449, 61.32240503668131026 ) ) ;
#16691 = AXIS2_PLACEMENT_3D ( 'NONE', #5374, #38293, #47400 ) ;
#16692 = CARTESIAN_POINT ( 'NONE',  ( 6.706751688761142027, 41.66489572023301946, -58.91094412759547794 ) ) ;
#16693 = CIRCLE ( 'NONE', #85618, 4.000000000000000888 ) ;
#16694 = CARTESIAN_POINT ( 'NONE',  ( 37.24829029260226321, 27.71736929400079319, -13.42529695738276629 ) ) ;
#16695 = ORIENTED_EDGE ( 'NONE', *, *, #28939, .F. ) ;
#16696 = CARTESIAN_POINT ( 'NONE',  ( -110.7188736420333299, -38.35613913791396357, 163.9771080353006596 ) ) ;
#16697 = VERTEX_POINT ( 'NONE', #68473 ) ;
#16698 =( LENGTH_UNIT ( ) NAMED_UNIT ( * ) SI_UNIT ( .MILLI., .METRE. ) );
#16699 = CARTESIAN_POINT ( 'NONE',  ( 90.82053129898724819, -38.35077124885843602, 19.83685144799958877 ) ) ;
#16700 = CARTESIAN_POINT ( 'NONE',  ( 15.42500621734827781, 22.80173751655717496, -2.001677017651171564 ) ) ;
#16701 = CARTESIAN_POINT ( 'NONE',  ( 103.1792978025558369, -45.28266199700388484, 156.3515883262585930 ) ) ;
#16702 = CARTESIAN_POINT ( 'NONE',  ( -17.63776521792187069, 43.19898629042302929, -6.169977679521857716 ) ) ;
#16703 = AXIS2_PLACEMENT_3D ( 'NONE', #50772, #18458, #83684 ) ;
#16704 =( NAMED_UNIT ( * ) PLANE_ANGLE_UNIT ( ) SI_UNIT ( $, .RADIAN. ) );
#16705 = CARTESIAN_POINT ( 'NONE',  ( -31.42089174849851574, 315.4419851189811084, -7.466270551174265968 ) ) ;
#16706 = CARTESIAN_POINT ( 'NONE',  ( 1.460859247228877278, -69.63554188353550956, 12.81388706339240358 ) ) ;
#16707 = CARTESIAN_POINT ( 'NONE',  ( 77.51769761606085751, -60.00000000000000711, 191.8023382803138475 ) ) ;
#16708 = B_SPLINE_CURVE_WITH_KNOTS ( 'NONE', 3,
 ( #9815, #42732, #19036, #43267, #76150, #2250, #41667, #74555, #68071, #100962, #629, #66471, #25529, #69670, #54512, #93949, #93419, #13001, #53989, #78806, #20646, #4937, #29253, #4398, #62134, #95024, #45927, #52403, #85322, #102569 ),
 .UNSPECIFIED., .F., .F.,
 ( 4, 2, 2, 2, 2, 2, 2, 2, 2, 2, 2, 2, 2, 2, 4 ),
 ( 0.002924093377768991441, 0.003854458377717581014, 0.004784823377666175791, 0.005715188377614770568, 0.006180370877589073594, 0.006645553377563376621, 0.007110735877537680515, 0.007343327127524836365, 0.007575918377511992215, 0.007808509627499148065, 0.008041100877486304782, 0.008506283377460621686, 0.008971465877434938591, 0.009436648377409257230, 0.01036701337735790318 ),
 .UNSPECIFIED. ) ;
#16709 = AXIS2_PLACEMENT_3D ( 'NONE', #6827, #56427, #65071 ) ;
#16710 = CIRCLE ( 'NONE', #68385, 0.9999999999999984457 ) ;
#16711 = CARTESIAN_POINT ( 'NONE',  ( 17.99657652128994201, 44.99999999999999289, 62.56960515030601755 ) ) ;
#16712 = ORIENTED_EDGE ( 'NONE', *, *, #98052, .F. ) ;
#16713 = CARTESIAN_POINT ( 'NONE',  ( 61.96504965809006649, -39.48483385517126720, 77.49375403494420311 ) ) ;
#16714 = CARTESIAN_POINT ( 'NONE',  ( -23.64706605907013781, 295.2260419621491678, -9.920446719441185834 ) ) ;
#16715 = CARTESIAN_POINT ( 'NONE',  ( 9.771805689013445928, -50.53686792747097911, 29.13556849961307194 ) ) ;
#16716 = CARTESIAN_POINT ( 'NONE',  ( -6.686471517026126854, -4.999999999999999112, -15.36038768879105731 ) ) ;
#16718 = CARTESIAN_POINT ( 'NONE',  ( -36.94935132573986891, 484.7118958255200027, -3.060944727314145020 ) ) ;
#16717 = CARTESIAN_POINT ( 'NONE',  ( -88.93458861890022149, -38.38101198339035136, -18.16568902887404491 ) ) ;
#16719 = CARTESIAN_POINT ( 'NONE',  ( -42.75446687478902419, 415.2909853957704058, 19.76521844420199159 ) ) ;
#16720 = DIRECTION ( 'NONE',  ( 0.000000000000000000, 1.000000000000000000, 0.000000000000000000 ) ) ;
#16721 = DIRECTION ( 'NONE',  ( 0.000000000000000000, 1.224646799147352468E-16, 1.000000000000000000 ) ) ;
#16722 = CARTESIAN_POINT ( 'NONE',  ( 8.000000000000000000, -25.99999999999999645, 0.000000000000000000 ) ) ;
#16723 = SURFACE_STYLE_USAGE ( .BOTH. , #31866 ) ;
#16725 = B_SPLINE_CURVE_WITH_KNOTS ( 'NONE', 3,
 ( #75868, #35446, #44038, #3041, #35989, #9521, #18733, #51043, #34386, #85577, #42433, #34915, #68862, #51584, #42978, #67262, #44581, #75324, #77472, #33847, #2500, #58636, #83959, #10068, #91535, #84502, #92579, #17649, #26306, #26830 ),
 .UNSPECIFIED., .F., .F.,
 ( 4, 2, 2, 2, 2, 2, 2, 2, 2, 2, 2, 2, 2, 2, 4 ),
 ( 0.004754800762794661635, 0.005690253947496225727, 0.006157980539847006905, 0.006625707132197788951, 0.006859570428373176071, 0.007093433724548564925, 0.007327297020723952913, 0.007561160316899340900, 0.007795023613074728887, 0.008028886909250116874, 0.008496613501600898052, 0.009432066686302465613, 0.01036751987100403144, 0.01130297305570559900, 0.01223842624040716656 ),
 .UNSPECIFIED. ) ;
#16724 = DIRECTION ( 'NONE',  ( -0.000000000000000000, 0.000000000000000000, 1.000000000000000000 ) ) ;
#16726 = ORIENTED_EDGE ( 'NONE', *, *, #39067, .T. ) ;
#16727 = CARTESIAN_POINT ( 'NONE',  ( 85.88214304176412384, -21.77332349503629416, 171.2076137571639549 ) ) ;
#16729 = CIRCLE ( 'NONE', #18521, 4.000000000000007105 ) ;
#16728 = DIRECTION ( 'NONE',  ( 0.000000000000000000, 0.000000000000000000, 1.000000000000000000 ) ) ;
#16730 = CARTESIAN_POINT ( 'NONE',  ( -42.56547585809266110, 436.9993064646045582, 20.73740471268625996 ) ) ;
#16731 = EDGE_LOOP ( 'NONE', ( #75305, #20553, #18929, #61120, #51446, #91306 ) ) ;
#16732 = FACE_OUTER_BOUND ( 'NONE', #70923, .T. ) ;
#16733 = CARTESIAN_POINT ( 'NONE',  ( 37.06438722625302518, -5.000000000000000000, 6.123233995736768255E-16 ) ) ;
#16734 = SURFACE_STYLE_USAGE ( .BOTH. , #32946 ) ;
#16735 = SURFACE_STYLE_USAGE ( .BOTH. , #90630 ) ;
#16736 = EDGE_CURVE ( 'NONE', #77573, #106581, #93271, .T. ) ;
#16737 = SURFACE_SIDE_STYLE ('',( #57702 ) ) ;
#16738 = EDGE_CURVE ( 'NONE', #58245, #48348, #34537, .T. ) ;
#16739 =( NAMED_UNIT ( * ) SI_UNIT ( $, .STERADIAN. ) SOLID_ANGLE_UNIT ( ) );
#16740 = EDGE_CURVE ( 'NONE', #33104, #43441, #43649, .T. ) ;
#16741 = CARTESIAN_POINT ( 'NONE',  ( 0.1685831701706822228, 25.16821295365200228, 40.75000000000013500 ) ) ;
#16742 = CIRCLE ( 'NONE', #16999, 64.50000000000000000 ) ;
#16744 = CARTESIAN_POINT ( 'NONE',  ( -12.93345011515627796, 23.56910474203129269, 4.607970287769207474 ) ) ;
#16743 = CARTESIAN_POINT ( 'NONE',  ( -15.92201275013530726, -23.21266242509823741, 36.07010217149083076 ) ) ;
#16745 = CARTESIAN_POINT ( 'NONE',  ( 4.401442555609581635E-16, -12.78125000204838280, -7.188101187500000044 ) ) ;
#16746 = DIRECTION ( 'NONE',  ( -1.000000000000000000, -1.224606353822377258E-16, -0.000000000000000000 ) ) ;
#16747 = DIRECTION ( 'NONE',  ( 0.000000000000000000, -1.000000000000000000, 0.000000000000000000 ) ) ;
#16748 = MECHANICAL_DESIGN_GEOMETRIC_PRESENTATION_REPRESENTATION (  '', ( #11577 ), #2959 ) ;
#16749 = VERTEX_POINT ( 'NONE', #27517 ) ;
#16750 = AXIS2_PLACEMENT_3D ( 'NONE', #44324, #21670, #87448 ) ;
#16751 = CARTESIAN_POINT ( 'NONE',  ( -19.07202809346026129, 49.63760697579748182, 61.78692401719171556 ) ) ;
#16752 = CARTESIAN_POINT ( 'NONE',  ( 24.03417899433058835, 25.72120757053723494, 31.00649972266041132 ) ) ;
#16753 = CARTESIAN_POINT ( 'NONE',  ( -2.860373741371127654, 85.40625066822151723, -5.000000000000002665 ) ) ;
#16755 = CARTESIAN_POINT ( 'NONE',  ( 45.16937095488047760, -60.22825610313712019, -33.02226515330256973 ) ) ;
#16754 = DIRECTION ( 'NONE',  ( 0.000000000000000000, -1.000000000000000000, 0.000000000000000000 ) ) ;
#16756 = VERTEX_POINT ( 'NONE', #10212 ) ;
#16757 = CARTESIAN_POINT ( 'NONE',  ( 11.50456601593190342, 15.12187630717486009, -9.781292348127028191 ) ) ;
#16758 = CARTESIAN_POINT ( 'NONE',  ( -4.151814662913274390, 52.11326435471435303, 6.758048296790627241 ) ) ;
#16759 =( GEOMETRIC_REPRESENTATION_CONTEXT ( 3 ) GLOBAL_UNCERTAINTY_ASSIGNED_CONTEXT ( ( #36501 ) ) GLOBAL_UNIT_ASSIGNED_CONTEXT ( ( #82971, #409, #58154 ) ) REPRESENTATION_CONTEXT ( 'NONE', 'WORKASPACE' ) );
#16760 = ORIENTED_EDGE ( 'NONE', *, *, #91938, .F. ) ;
#16761 = CARTESIAN_POINT ( 'NONE',  ( 64.29999999999999716, 6.915964383211875250E-15, 0.000000000000000000 ) ) ;
#16762 = EDGE_CURVE ( 'NONE', #21657, #13347, #35247, .T. ) ;
#16763 = FACE_OUTER_BOUND ( 'NONE', #101922, .T. ) ;
#16764 = DIRECTION ( 'NONE',  ( 0.000000000000000000, 0.000000000000000000, 1.000000000000000000 ) ) ;
#16765 = CARTESIAN_POINT ( 'NONE',  ( -95.60614214828055424, -60.00000000000000711, 53.33793432721193284 ) ) ;
#16766 = CIRCLE ( 'NONE', #11603, 3.309500000000001663 ) ;
#16767 = MECHANICAL_DESIGN_GEOMETRIC_PRESENTATION_REPRESENTATION (  '', ( #9914 ), #47780 ) ;
#16768 = FACE_OUTER_BOUND ( 'NONE', #57091, .T. ) ;
#16769 = AXIS2_PLACEMENT_3D ( 'NONE', #20016, #94402, #93858 ) ;
#16770 = CARTESIAN_POINT ( 'NONE',  ( 0.000000000000000000, 0.000000000000000000, 0.000000000000000000 ) ) ;
#16771 = DIRECTION ( 'NONE',  ( 1.000000000000000000, -0.000000000000000000, -0.000000000000000000 ) ) ;
#16772 = CARTESIAN_POINT ( 'NONE',  ( 0.000000000000000000, -30.00000000000000000, 0.000000000000000000 ) ) ;
#16774 = CARTESIAN_POINT ( 'NONE',  ( 32.31817526860642431, 488.2662992775009343, 9.217981799629473727 ) ) ;
#16773 = CARTESIAN_POINT ( 'NONE',  ( -10.48543666094594862, -5.000000000000002665, -91.04342776276726568 ) ) ;
#16775 = CARTESIAN_POINT ( 'NONE',  ( -84.78841041186234406, -28.94319752679387392, 170.4401308887547373 ) ) ;
#16776 = ORIENTED_EDGE ( 'NONE', *, *, #69071, .F. ) ;
#16777 = B_SPLINE_CURVE_WITH_KNOTS ( 'NONE', 3,
 ( #38265, #54382, #104017, #30160, #90498, #14462, #39312, #72194, #80265, #57050, #16609, #72711, #49499, #89967, #65694, #105098, #57576, #105612, #71643, #63591, #40351, #16073, #47374, #23136, #31237, #82405, #81849, #24202 ),
 .UNSPECIFIED., .F., .F.,
 ( 4, 2, 2, 2, 2, 2, 2, 2, 2, 2, 2, 2, 2, 4 ),
 ( 0.007040904414468415924, 0.007507994684082267001, 0.007741539818889188636, 0.007975084953696110271, 0.008208630088503032773, 0.008442175223309953541, 0.008909265492923810689, 0.009376355762537667837, 0.009843446032151523251, 0.01077762657137924275, 0.01171180711060696052, 0.01264598764983468002, 0.01358016818906239778, 0.01451434872829011555 ),
 .UNSPECIFIED. ) ;
#16778 = AXIS2_PLACEMENT_3D ( 'NONE', #102680, #28841, #66460 ) ;
#16779 = EDGE_LOOP ( 'NONE', ( #50340, #16020, #22654, #94734 ) ) ;
#16780 = ORIENTED_EDGE ( 'NONE', *, *, #92637, .F. ) ;
#16781 = DIRECTION ( 'NONE',  ( -1.000000000000000000, -1.224606353822377258E-16, -0.000000000000000000 ) ) ;
#16782 = EDGE_CURVE ( 'NONE', #55816, #79598, #55830, .T. ) ;
#16783 = EDGE_CURVE ( 'NONE', #10653, #3603, #50142, .T. ) ;
#16784 = DIRECTION ( 'NONE',  ( -1.000000000000000000, -0.000000000000000000, -0.000000000000000000 ) ) ;
#16785 = ORIENTED_EDGE ( 'NONE', *, *, #96237, .F. ) ;
#16786 = FACE_OUTER_BOUND ( 'NONE', #65415, .T. ) ;
#16787 = SURFACE_SIDE_STYLE ('',( #74475 ) ) ;
#16788 = DIRECTION ( 'NONE',  ( -1.000000000000000000, -1.224606353822377258E-16, -0.000000000000000000 ) ) ;
#16789 = CARTESIAN_POINT ( 'NONE',  ( 30.00000000000000000, 490.5636507777048791, 7.413185101890151785 ) ) ;
#16790 = DIRECTION ( 'NONE',  ( 0.000000000000000000, 0.000000000000000000, 1.000000000000000000 ) ) ;
#16791 = CARTESIAN_POINT ( 'NONE',  ( -12.86258593040350995, -5.000000000000000000, -82.77024182148061016 ) ) ;
#16792 = DIRECTION ( 'NONE',  ( 0.000000000000000000, -1.000000000000000000, 0.000000000000000000 ) ) ;
#16793 = MANIFOLD_SOLID_BREP ( 'Fillet2', #94614 ) ;
#16794 = CARTESIAN_POINT ( 'NONE',  ( 109.1953510978495956, -29.99999999999998934, 161.8808647345001646 ) ) ;
#16795 = CARTESIAN_POINT ( 'NONE',  ( -106.6034117734591860, -29.99999999999999645, 192.6833206840571791 ) ) ;
#16796 = CARTESIAN_POINT ( 'NONE',  ( -62.29161391638449885, -22.11170671976271862, 69.90898424290641344 ) ) ;
#16797 = AXIS2_PLACEMENT_3D ( 'NONE', #91916, #83290, #2892 ) ;
#16798 = ORIENTED_EDGE ( 'NONE', *, *, #70267, .T. ) ;
#16799 = CARTESIAN_POINT ( 'NONE',  ( -50.58582176620591753, 38.95379933617689971, 38.77008064533420395 ) ) ;
#16800 = CARTESIAN_POINT ( 'NONE',  ( 113.6477508017368194, -59.99999999999997158, 154.8077346558557679 ) ) ;
#16801 = ORIENTED_EDGE ( 'NONE', *, *, #24809, .F. ) ;
#16802 = CARTESIAN_POINT ( 'NONE',  ( 4.998710019538861182, -25.54820205286554469, 28.13823241950028020 ) ) ;
#16803 = CARTESIAN_POINT ( 'NONE',  ( -105.8794421244064097, -60.15508394961005934, 158.7618641718036088 ) ) ;
#16804 = CARTESIAN_POINT ( 'NONE',  ( 2.977408999572650927, -14.75000000204838457, -7.188101187500000933 ) ) ;
#16805 = CARTESIAN_POINT ( 'NONE',  ( -13.50000000000000000, -7.794228634059985339, -1.205771365940065953 ) ) ;
#16806 = ORIENTED_EDGE ( 'NONE', *, *, #37517, .F. ) ;
#16807 = AXIS2_PLACEMENT_3D ( 'NONE', #17375, #24942, #65378 ) ;
#16808 = EDGE_CURVE ( 'NONE', #50186, #59786, #45878, .T. ) ;
#16809 = CARTESIAN_POINT ( 'NONE',  ( 0.000000000000000000, 80.00000000000000000, 0.000000000000000000 ) ) ;
#16810 = ORIENTED_EDGE ( 'NONE', *, *, #57377, .T. ) ;
#16811 = CARTESIAN_POINT ( 'NONE',  ( 0.000000000000000000, 0.000000000000000000, 0.000000000000000000 ) ) ;
#16812 = CARTESIAN_POINT ( 'NONE',  ( -78.29652527090244973, -60.00000000000002132, 193.4105370956309002 ) ) ;
#16813 = CARTESIAN_POINT ( 'NONE',  ( 9.337186727013605747, -56.01312624425312237, 30.58335800272115534 ) ) ;
#16814 = CARTESIAN_POINT ( 'NONE',  ( 5.082755093536324154, -18.21875000204838457, 5.082755093536326818 ) ) ;
#16815 = CARTESIAN_POINT ( 'NONE',  ( 33.71029056097465570, 485.0094969250627628, -0.6083101643369144274 ) ) ;
#16816 = VECTOR ( 'NONE', #70586, 1000.000000000000000 ) ;
#16817 = CARTESIAN_POINT ( 'NONE',  ( 37.56673239365873940, 27.88554838446218653, 10.95617127780822564 ) ) ;
#16818 = CARTESIAN_POINT ( 'NONE',  ( -11.41770977658351427, 13.86023221547256412, 9.965253901235293199 ) ) ;
#16819 = CARTESIAN_POINT ( 'NONE',  ( 13.50000000000000533, 5.257130651325587323, -12.46102409077683326 ) ) ;
#16820 = CARTESIAN_POINT ( 'NONE',  ( 32.12958771267408054, 464.7275665249412100, 11.12424126545838909 ) ) ;
#16821 = ADVANCED_FACE ( 'NONE', ( #87309 ), #16279, .T. ) ;
#16822 = DIRECTION ( 'NONE',  ( 0.000000000000000000, -1.000000000000000000, 0.000000000000000000 ) ) ;
#16823 = CARTESIAN_POINT ( 'NONE',  ( -30.49051837336642024, 298.0882550346395874, -1.287325532041848186 ) ) ;
#16824 = DIRECTION ( 'NONE',  ( -0.5735764363510510444, -0.8191520442889883569, 0.000000000000000000 ) ) ;
#16825 = CARTESIAN_POINT ( 'NONE',  ( -32.06874758335647613, -36.02319553862302115, 33.29146392800486609 ) ) ;
#16826 = CARTESIAN_POINT ( 'NONE',  ( 100.0424503805845831, 5.000000000000023093, 6.123233995736781074E-16 ) ) ;
#16827 = CARTESIAN_POINT ( 'NONE',  ( 42.58818415145629643, -53.34091589762581265, 44.38045783418311174 ) ) ;
#16828 =( LENGTH_UNIT ( ) NAMED_UNIT ( * ) SI_UNIT ( .MILLI., .METRE. ) );
#16829 = ORIENTED_EDGE ( 'NONE', *, *, #70200, .T. ) ;
#16831 = AXIS2_PLACEMENT_3D ( 'NONE', #100637, #52086, #76895 ) ;
#16830 = CARTESIAN_POINT ( 'NONE',  ( 43.04469050570446598, 434.7734435962917132, 9.248231035223279051 ) ) ;
#16832 = EDGE_CURVE ( 'NONE', #71609, #14235, #4202, .T. ) ;
#16833 = CARTESIAN_POINT ( 'NONE',  ( -76.00620243949536814, -38.37823116147261260, 178.4010451240498867 ) ) ;
#16834 = B_SPLINE_CURVE_WITH_KNOTS ( 'NONE', 3,
 ( #105101, #65699, #98584, #72713, #89449, #24206, #15541, #16612, #82410, #8510, #7436, #23138, #40353, #48956, #106131, #32289, #39316, #47378, #81853, #74306, #57055, #40888, #383, #97000, #88389, #65159, #80268, #6381, #72196, #64131 ),
 .UNSPECIFIED., .F., .F.,
 ( 4, 2, 2, 2, 2, 2, 2, 2, 2, 2, 2, 2, 2, 2, 4 ),
 ( 0.006732386592399308353, 0.007201418480221453110, 0.007435934424132525054, 0.007670450368043596999, 0.007904966311954668076, 0.008139482255865740021, 0.008373998199776811965, 0.008608514143687885645, 0.009077546031510029534, 0.009546577919332173423, 0.01048464169497645079, 0.01142270547062072990, 0.01236076924626500900, 0.01329883302190928637, 0.01423689679755356548 ),
 .UNSPECIFIED. ) ;
#16835 = ORIENTED_EDGE ( 'NONE', *, *, #105556, .T. ) ;
#16837 = CARTESIAN_POINT ( 'NONE',  ( 38.68218982724705057, 320.0845437455996603, 16.10279619727025135 ) ) ;
#16836 = CARTESIAN_POINT ( 'NONE',  ( -5.956988534971662475, 4.556784786910193397, 5.000000000000000000 ) ) ;
#16838 = CARTESIAN_POINT ( 'NONE',  ( 68.96826172936565058, -59.99999999999997158, 110.4669535869814467 ) ) ;
#16840 = EDGE_CURVE ( 'NONE', #25868, #96063, #76555, .T. ) ;
#16839 = CARTESIAN_POINT ( 'NONE',  ( -48.87836615495903914, 8.113987396617073244, -16.52312645342838238 ) ) ;
#16841 = CARTESIAN_POINT ( 'NONE',  ( -44.11327388758642343, 464.4313852428376777, 9.822198357559813076 ) ) ;
#16842 = CARTESIAN_POINT ( 'NONE',  ( 6.619572829571047201, 41.38254192185750924, -70.73105035554675624 ) ) ;
#16843 = CARTESIAN_POINT ( 'NONE',  ( 0.000000000000000000, 0.000000000000000000, -7.974599999999995248 ) ) ;
#16845 = COLOUR_RGB ( '', 0.66274510, 0.83137255, 0.94901961) ;
#16844 = CARTESIAN_POINT ( 'NONE',  ( 0.000000000000000000, 0.000000000000000000, 0.000000000000000000 ) ) ;
#16846 = CARTESIAN_POINT ( 'NONE',  ( 17.89001738438794931, 45.34603189753767083, 5.216234635019720400 ) ) ;
#16847 = CARTESIAN_POINT ( 'NONE',  ( 106.3832165010686737, -59.99999999999999289, 118.7897376084098369 ) ) ;
#16848 = AXIS2_PLACEMENT_3D ( 'NONE', #96866, #38137, #4145 ) ;
#16849 = DIRECTION ( 'NONE',  ( 0.000000000000000000, 1.000000000000000000, 0.000000000000000000 ) ) ;
#16850 = CARTESIAN_POINT ( 'NONE',  ( -7.002619243997878051, -66.05007318013817041, -3.868708944013001361 ) ) ;
#16851 = ORIENTED_EDGE ( 'NONE', *, *, #21881, .T. ) ;
#16852 = B_SPLINE_CURVE_WITH_KNOTS ( 'NONE', 3,
 ( #22291, #62221, #97197, #55137, #88067, #14146, #79949, #6059, #15218, #81006, #30915, #38985 ),
 .UNSPECIFIED., .F., .F.,
 ( 4, 2, 2, 2, 2, 4 ),
 ( 0.000000000000000000, 0.001936431260136990684, 0.002904646890205480388, 0.003872862520273970960, 0.005809293780410951236, 0.007745725040547933246 ),
 .UNSPECIFIED. ) ;
#16853 = CARTESIAN_POINT ( 'NONE',  ( -89.59768141200925129, -30.00000000000018474, 189.4893437224044987 ) ) ;
#16854 = ORIENTED_EDGE ( 'NONE', *, *, #56086, .F. ) ;
#16855 = CARTESIAN_POINT ( 'NONE',  ( 5.363597346073513350, 41.33266196706048845, -58.39526881795627844 ) ) ;
#16856 = FACE_OUTER_BOUND ( 'NONE', #104468, .T. ) ;
#16857 = CARTESIAN_POINT ( 'NONE',  ( 7.869432500667418395, 87.30546385994318825, 0.000000000000000000 ) ) ;
#16858 = CARTESIAN_POINT ( 'NONE',  ( 26.35185796998234409, 307.8658938434331844, 10.86782115656190406 ) ) ;
#16860 = CARTESIAN_POINT ( 'NONE',  ( -21.97741296367594543, 27.90380497738007293, -32.31715157276733663 ) ) ;
#16859 = TOROIDAL_SURFACE ( 'NONE', #58177, 7.500000000000000888, 5.000000000000000000 ) ;
#16861 = STYLED_ITEM ( 'NONE', ( #23717 ), #60625 ) ;
#16862 = CARTESIAN_POINT ( 'NONE',  ( -2.977408999572654480, -17.00000000204838457, 7.188101187499999156 ) ) ;
#16863 = DIRECTION ( 'NONE',  ( -0.000000000000000000, 0.000000000000000000, 1.000000000000000000 ) ) ;
#16864 = CARTESIAN_POINT ( 'NONE',  ( 7.452250447672242650, 40.95020998762944942, -69.64366759659492345 ) ) ;
#16865 = COLOUR_RGB ( '', 0.72549020, 0.75294118, 0.79215686) ;
#16866 = AXIS2_PLACEMENT_3D ( 'NONE', #95443, #46366, #98614 ) ;
#16867 =( GEOMETRIC_REPRESENTATION_CONTEXT ( 3 ) GLOBAL_UNCERTAINTY_ASSIGNED_CONTEXT ( ( #32264 ) ) GLOBAL_UNIT_ASSIGNED_CONTEXT ( ( #74122, #51976, #9925 ) ) REPRESENTATION_CONTEXT ( 'NONE', 'WORKASPACE' ) );
#16869 = ORIENTED_EDGE ( 'NONE', *, *, #42087, .F. ) ;
#16868 = SURFACE_SIDE_STYLE ('',( #60527 ) ) ;
#16870 = CARTESIAN_POINT ( 'NONE',  ( 79.71048774950203608, -49.90412405833568243, 156.1982597888667499 ) ) ;
#16871 = FACE_OUTER_BOUND ( 'NONE', #93649, .T. ) ;
#16872 = CARTESIAN_POINT ( 'NONE',  ( -30.00000000000000000, 450.0000000000002274, 13.20242257375370976 ) ) ;
#16873 = EDGE_LOOP ( 'NONE', ( #12716, #60138, #58162, #94005, #34673 ) ) ;
#16874 =( NAMED_UNIT ( * ) SI_UNIT ( $, .STERADIAN. ) SOLID_ANGLE_UNIT ( ) );
#16875 = CARTESIAN_POINT ( 'NONE',  ( 38.75747312663246902, 27.29554786619022622, -12.59589368416849453 ) ) ;
#16876 = CARTESIAN_POINT ( 'NONE',  ( 7.743982712349854580, 26.53786985239263529, 2.020119794285908821 ) ) ;
#16877 = CARTESIAN_POINT ( 'NONE',  ( 14.89431991952050538, -60.00000000000000711, -36.42525387037616724 ) ) ;
#16878 = CARTESIAN_POINT ( 'NONE',  ( -21.43128638237507388, 303.0517047904468200, 9.980147555062945486 ) ) ;
#16879 = CARTESIAN_POINT ( 'NONE',  ( 18.71538461538461462, 1.411358822780289120E-15, 0.000000000000000000 ) ) ;
#16880 = EDGE_CURVE ( 'NONE', #8756, #30104, #69533, .T. ) ;
#16881 = ORIENTED_EDGE ( 'NONE', *, *, #55075, .T. ) ;
#16882 = CIRCLE ( 'NONE', #104705, 4.000000000000007105 ) ;
#16883 = CARTESIAN_POINT ( 'NONE',  ( 45.94900261086841198, 1.482358050883964840E-15, 0.000000000000000000 ) ) ;
#16884 = ADVANCED_FACE ( 'NONE', ( #29632 ), #49883, .T. ) ;
#16885 = CARTESIAN_POINT ( 'NONE',  ( 7.054522925320324767, 41.71556257522360767, -59.55896313260247865 ) ) ;
#16886 = CARTESIAN_POINT ( 'NONE',  ( 86.79590143382110057, -31.74670322683050117, 186.8222491938091423 ) ) ;
#16887 = CARTESIAN_POINT ( 'NONE',  ( 0.000000000000000000, -30.00000000000000000, 8.000000000000000000 ) ) ;
#16888 = STYLED_ITEM ( 'NONE', ( #100385 ), #42426 ) ;
#16889 = CARTESIAN_POINT ( 'NONE',  ( -7.188101187500001821, -33.50000000204838813, -2.977408999572651371 ) ) ;
#16890 = CARTESIAN_POINT ( 'NONE',  ( 21.52054819351988613, -26.69862200661779994, 37.20882657828786222 ) ) ;
#16891 = CARTESIAN_POINT ( 'NONE',  ( -38.02377251231919075, 490.5703810925436414, 12.25131830484250628 ) ) ;
#16892 = CARTESIAN_POINT ( 'NONE',  ( -72.50181434431193850, -38.00000000001091394, -21.26203725901419261 ) ) ;
#16893 = CIRCLE ( 'NONE', #77170, 1.999999999999998224 ) ;
#16894 = DIRECTION ( 'NONE',  ( 1.000000000000000000, 0.000000000000000000, 0.000000000000000000 ) ) ;
#16895 = CARTESIAN_POINT ( 'NONE',  ( 48.87836615495911730, 8.113987396617103443, 16.52312645342804842 ) ) ;
#16896 = ORIENTED_EDGE ( 'NONE', *, *, #100922, .F. ) ;
#16897 = CARTESIAN_POINT ( 'NONE',  ( 1.249445774276175536, 43.67355798807202660, 17.33679506162915374 ) ) ;
#16898 = CARTESIAN_POINT ( 'NONE',  ( 13.44879422951056291, 42.85243152879387196, -92.01096473121475583 ) ) ;
#16899 = DIRECTION ( 'NONE',  ( 0.000000000000000000, 0.000000000000000000, 1.000000000000000000 ) ) ;
#16900 = DIRECTION ( 'NONE',  ( 0.000000000000000000, -1.000000000000000000, 0.000000000000000000 ) ) ;
#16901 = EDGE_CURVE ( 'NONE', #6505, #1485, #81701, .T. ) ;
#16902 = ORIENTED_EDGE ( 'NONE', *, *, #18140, .T. ) ;
#16903 = AXIS2_PLACEMENT_3D ( 'NONE', #27820, #87085, #53113 ) ;
#16904 = CARTESIAN_POINT ( 'NONE',  ( -43.00000000000001421, 461.4080316921935605, 3.462976341553827275 ) ) ;
#16905 = CARTESIAN_POINT ( 'NONE',  ( 113.3004268891054522, -57.67143715891052125, 155.2604439073490425 ) ) ;
#16906 = CIRCLE ( 'NONE', #11659, 2.000000000000000000 ) ;
#16907 = CARTESIAN_POINT ( 'NONE',  ( 35.52386467438406470, 464.2380653034119860, 19.26634992204540708 ) ) ;
#16908 = ADVANCED_FACE ( 'NONE', ( #6901 ), #11111, .T. ) ;
#16909 = FACE_OUTER_BOUND ( 'NONE', #14377, .T. ) ;
#16910 = FACE_OUTER_BOUND ( 'NONE', #33756, .T. ) ;
#16911 = CARTESIAN_POINT ( 'NONE',  ( 99.17777777777777715, 1.023464760207051730E-14, 0.000000000000000000 ) ) ;
#16912 = CARTESIAN_POINT ( 'NONE',  ( -75.55177680087479075, -60.00000000000000000, 184.7945938706629931 ) ) ;
#16913 = CARTESIAN_POINT ( 'NONE',  ( -25.93947128054312756, 296.0094280503604978, 10.18659011856751384 ) ) ;
#16914 = VECTOR ( 'NONE', #13460, 999.9999999999998863 ) ;
#16915 = CARTESIAN_POINT ( 'NONE',  ( -35.76379064120181539, 307.0162303970107587, 12.81051142610679960 ) ) ;
#16917 = VECTOR ( 'NONE', #16203, 1000.000000000000000 ) ;
#16916 = B_SPLINE_CURVE_WITH_KNOTS ( 'NONE', 3,
 ( #87548, #5550, #96172, #22302, #6072, #72409 ),
 .UNSPECIFIED., .F., .F.,
 ( 4, 2, 4 ),
 ( -4.698498716301142229E-06, 0.0003457374136927998383, 0.0006961733261019008171 ),
 .UNSPECIFIED. ) ;
#16918 = B_SPLINE_CURVE_WITH_KNOTS ( 'NONE', 3,
 ( #72027, #104934, #73058, #56881, #7801, #55807, #10463, #33709 ),
 .UNSPECIFIED., .F., .F.,
 ( 4, 2, 2, 4 ),
 ( 2.096953513055919001E-16, 0.002585882924094807904, 0.003878824386142106905, 0.005171765848189405906 ),
 .UNSPECIFIED. ) ;
#16919 = CARTESIAN_POINT ( 'NONE',  ( -85.67931066178286414, -35.66015517622967224, 184.2351685365583478 ) ) ;
#16920 = ORIENTED_EDGE ( 'NONE', *, *, #26573, .F. ) ;
#16921 = CARTESIAN_POINT ( 'NONE',  ( 25.90835893021727898, 306.6868635151020612, -9.596616819076174920 ) ) ;
#16922 = VERTEX_POINT ( 'NONE', #48416 ) ;
#16923 = CARTESIAN_POINT ( 'NONE',  ( 9.797174393178825657E-16, -30.00000000000000000, -8.000000000000000000 ) ) ;
#16924 = EDGE_CURVE ( 'NONE', #40083, #45434, #95514, .T. ) ;
#16925 = CARTESIAN_POINT ( 'NONE',  ( 0.000000000000000000, 0.000000000000000000, 0.000000000000000000 ) ) ;
#16926 = CARTESIAN_POINT ( 'NONE',  ( -86.84696613357556316, -60.22825968734050406, -10.54492661878714443 ) ) ;
#16927 = CIRCLE ( 'NONE', #94388, 5.000000000000002665 ) ;
#16928 = CARTESIAN_POINT ( 'NONE',  ( -4.640293713146470544, 8.300177736797209604, -5.000000000000000000 ) ) ;
#16929 = CARTESIAN_POINT ( 'NONE',  ( 36.08349330513379982, -7.703719777548943412E-31, 4.000000000000001776 ) ) ;
#16931 = CARTESIAN_POINT ( 'NONE',  ( 6.562974947121711367, 4.277474787035885129, -6.282829635893498299 ) ) ;
#16930 = AXIS2_PLACEMENT_3D ( 'NONE', #38800, #54952, #104576 ) ;
#16932 = CARTESIAN_POINT ( 'NONE',  ( 13.39830318362800909, 24.42447744924177400, -2.536416954090644271 ) ) ;
#16933 = LINE ( 'NONE', #80049, #47770 ) ;
#16934 = CARTESIAN_POINT ( 'NONE',  ( -36.73553355714307145, 438.2340261154905647, 3.898456086346344218 ) ) ;
#16935 = CARTESIAN_POINT ( 'NONE',  ( 60.74900604410193239, -14.21045842199440301, -29.98664384297035213 ) ) ;
#16936 = CARTESIAN_POINT ( 'NONE',  ( -75.82081383092520355, -60.31953473974737534, 141.6095240737906238 ) ) ;
#16937 = ORIENTED_EDGE ( 'NONE', *, *, #77466, .T. ) ;
#16938 = CARTESIAN_POINT ( 'NONE',  ( 66.01776342811430709, -14.21045842199433373, 101.7751388943407989 ) ) ;
#16939 = CARTESIAN_POINT ( 'NONE',  ( 7.002990960197237769, 86.05266818383456950, 3.868040364119521790 ) ) ;
#16940 = CARTESIAN_POINT ( 'NONE',  ( 112.3945400198572884, -57.67111632160943913, 146.4074606690158760 ) ) ;
#16941 = VECTOR ( 'NONE', #48553, 1000.000000000000114 ) ;
#16942 = ORIENTED_EDGE ( 'NONE', *, *, #92199, .T. ) ;
#16943 = CARTESIAN_POINT ( 'NONE',  ( 95.42421628608209971, 1.030564683017419500E-14, 0.000000000000000000 ) ) ;
#16944 = CARTESIAN_POINT ( 'NONE',  ( 43.86650669486618881, 4.898587196589411843E-16, -4.000000000000000888 ) ) ;
#16945 = ORIENTED_EDGE ( 'NONE', *, *, #67860, .T. ) ;
#16946 =( NAMED_UNIT ( * ) SI_UNIT ( $, .STERADIAN. ) SOLID_ANGLE_UNIT ( ) );
#16947 = CARTESIAN_POINT ( 'NONE',  ( 0.000000000000000000, 6.123233995736767268E-16, -5.000000000000000888 ) ) ;
#16948 = CARTESIAN_POINT ( 'NONE',  ( 16.32461263189640377, 43.58742806653211943, 6.626833409472919989 ) ) ;
#16949 = CARTESIAN_POINT ( 'NONE',  ( -7.188101187500002709, -10.81250000204838457, 2.977408999572648707 ) ) ;
#16950 = CARTESIAN_POINT ( 'NONE',  ( 4.406466114818337942, -6.116179640279066909, -7.446478553994767324 ) ) ;
#16951 = CARTESIAN_POINT ( 'NONE',  ( 9.644834624769973885, 81.99109499794225542, 2.648308524638419925 ) ) ;
#16952 = CARTESIAN_POINT ( 'NONE',  ( 1.224646799147353454E-15, 0.000000000000000000, 10.00000000000000178 ) ) ;
#16953 = EDGE_CURVE ( 'NONE', #42491, #80498, #98953, .T. ) ;
#16954 = CARTESIAN_POINT ( 'NONE',  ( -2.500000000000001332, 14.00000000000000000, 0.000000000000000000 ) ) ;
#16955 = CIRCLE ( 'NONE', #84080, 3.309500000000001663 ) ;
#16956 = ORIENTED_EDGE ( 'NONE', *, *, #60660, .T. ) ;
#16957 = CARTESIAN_POINT ( 'NONE',  ( -6.941422770587817759, 41.41225025357826439, -70.44081391737150000 ) ) ;
#16959 = CARTESIAN_POINT ( 'NONE',  ( 30.49012212078099893, -29.07017293858438478, 31.42300344396308631 ) ) ;
#16958 = FILL_AREA_STYLE_COLOUR ( '', #21733 ) ;
#16960 = CARTESIAN_POINT ( 'NONE',  ( 20.94643265517294850, 304.9211962324576461, -8.985249965551574292 ) ) ;
#16961 = ORIENTED_EDGE ( 'NONE', *, *, #83587, .F. ) ;
#16962 = EDGE_CURVE ( 'NONE', #84319, #59024, #48939, .T. ) ;
#16963 = CARTESIAN_POINT ( 'NONE',  ( -1.249013534494713751, 16.16290615548213694, 50.37193964746203534 ) ) ;
#16964 = UNCERTAINTY_MEASURE_WITH_UNIT (LENGTH_MEASURE( 1.000000000000000082E-05 ), #17784, 'distance_accuracy_value', 'NONE');
#16965 = ORIENTED_EDGE ( 'NONE', *, *, #60292, .F. ) ;
#16967 = CARTESIAN_POINT ( 'NONE',  ( -0.3342755987430475195, 44.06880435339610358, -16.29260335467761323 ) ) ;
#16966 = CARTESIAN_POINT ( 'NONE',  ( 10.59999999999999609, 1.533819458162526451E-15, 0.000000000000000000 ) ) ;
#16968 = FACE_OUTER_BOUND ( 'NONE', #81119, .T. ) ;
#16969 = CARTESIAN_POINT ( 'NONE',  ( -16.12995111408092441, 294.5641271688412530, -2.061085572538797983 ) ) ;
#16970 = DIRECTION ( 'NONE',  ( 0.000000000000000000, 0.000000000000000000, 1.000000000000000000 ) ) ;
#16971 = CARTESIAN_POINT ( 'NONE',  ( 32.28552837373268147, 464.7648866755951644, 15.30384310833112060 ) ) ;
#16972 = CARTESIAN_POINT ( 'NONE',  ( -37.67124221001142814, 463.6239404278534266, 19.49545380201571021 ) ) ;
#16973 = VERTEX_POINT ( 'NONE', #32804 ) ;
#16974 = CARTESIAN_POINT ( 'NONE',  ( 91.58819796920066381, -60.00000000000000000, -15.36446433908737319 ) ) ;
#16975 = CARTESIAN_POINT ( 'NONE',  ( -9.267538580112278268, 46.19448214903181338, 13.41394971794136559 ) ) ;
#16977 = ADVANCED_FACE ( 'NONE', ( #64109 ), #73757, .T. ) ;
#16976 = CARTESIAN_POINT ( 'NONE',  ( 32.06413248787634274, 464.8630579811580219, 13.97151946468930461 ) ) ;
#16978 = CARTESIAN_POINT ( 'NONE',  ( 23.15769230769230802, -4.171999999999999709, 5.616230220889763424E-16 ) ) ;
#16979 = VERTEX_POINT ( 'NONE', #81307 ) ;
#16980 = CARTESIAN_POINT ( 'NONE',  ( -36.31529515053280477, 28.19075680830513875, 12.14815066672548305 ) ) ;
#16981 = ORIENTED_EDGE ( 'NONE', *, *, #34881, .F. ) ;
#16982 = AXIS2_PLACEMENT_3D ( 'NONE', #43168, #101407, #35644 ) ;
#16983 = ORIENTED_EDGE ( 'NONE', *, *, #46780, .T. ) ;
#16984 =( LENGTH_UNIT ( ) NAMED_UNIT ( * ) SI_UNIT ( .MILLI., .METRE. ) );
#16985 = DIRECTION ( 'NONE',  ( -1.000000000000000000, -1.224606353822377258E-16, -0.000000000000000000 ) ) ;
#16986 = CARTESIAN_POINT ( 'NONE',  ( 22.25669491856071858, 6.123233995736772199E-16, -5.000000000000001776 ) ) ;
#16987 = CARTESIAN_POINT ( 'NONE',  ( 84.09803781733121752, -45.28736737590700301, 1.238215950073735527 ) ) ;
#16988 = CARTESIAN_POINT ( 'NONE',  ( -42.94810946381694805, 342.9651505394211313, 9.411812260929616869 ) ) ;
#16989 = CARTESIAN_POINT ( 'NONE',  ( -6.008858299639965317, -63.46485955003367252, 14.35488293964984585 ) ) ;
#16990 = CARTESIAN_POINT ( 'NONE',  ( 12.50000000000000000, 28.57588390897651820, -46.22316309954614155 ) ) ;
#16991 = MANIFOLD_SOLID_BREP ( 'Cut-Extrude3', #77348 ) ;
#16992 = AXIS2_PLACEMENT_3D ( 'NONE', #35848, #43370, #92977 ) ;
#16993 = EDGE_LOOP ( 'NONE', ( #80122, #65507, #32173, #1434, #68175 ) ) ;
#16994 = CARTESIAN_POINT ( 'NONE',  ( 0.000000000000000000, 45.89575828009193259, -11.27631144943088337 ) ) ;
#16995 = EDGE_LOOP ( 'NONE', ( #54580, #96182, #636, #29609 ) ) ;
#16996 = DIRECTION ( 'NONE',  ( -0.000000000000000000, 0.000000000000000000, -1.000000000000000000 ) ) ;
#16997 = CARTESIAN_POINT ( 'NONE',  ( -91.09125006954968740, -38.50546275171844712, 200.8230852611536932 ) ) ;
#16998 = CARTESIAN_POINT ( 'NONE',  ( 41.11448970373153600, 464.2845792240962055, 17.78478044672835168 ) ) ;
#16999 = AXIS2_PLACEMENT_3D ( 'NONE', #51008, #18152, #83390 ) ;
#17001 = EDGE_LOOP ( 'NONE', ( #20340, #17878, #92691, #73566 ) ) ;
#17000 = CARTESIAN_POINT ( 'NONE',  ( -35.51287843845796033, -60.00000000000001421, 39.56491211972655009 ) ) ;
#17002 = CARTESIAN_POINT ( 'NONE',  ( 65.14337256760538253, -32.53026157264622498, 82.99388498196113062 ) ) ;
#17003 = MECHANICAL_DESIGN_GEOMETRIC_PRESENTATION_REPRESENTATION (  '', ( #8360 ), #70433 ) ;
#17004 = VERTEX_POINT ( 'NONE', #47881 ) ;
#17005 = CARTESIAN_POINT ( 'NONE',  ( 16.66584972137510690, 38.95383793069935763, 62.01418705508215368 ) ) ;
#17006 = CARTESIAN_POINT ( 'NONE',  ( -7.188101187500002709, -28.81250000204838813, 2.977408999572647819 ) ) ;
#17007 = CARTESIAN_POINT ( 'NONE',  ( -83.74719587345013849, -57.67098913794580994, -27.91190304260424071 ) ) ;
#17009 = EDGE_CURVE ( 'NONE', #88573, #36200, #22605, .T. ) ;
#17008 = B_SPLINE_CURVE_WITH_KNOTS ( 'NONE', 3,
 ( #10845, #28156, #69125, #35717, #101479, #86381, #27630, #52922, #93396, #4369, #36781, #11380, #44304, #100936 ),
 .UNSPECIFIED., .F., .F.,
 ( 4, 2, 2, 2, 2, 2, 4 ),
 ( 8.482014475176614844E-15, 0.003029464007163871000, 0.004544196010741614541, 0.006058928014319358082, 0.007573660017897102491, 0.009088392021474845164, 0.01211785602863033745 ),
 .UNSPECIFIED. ) ;
#17010 = ORIENTED_EDGE ( 'NONE', *, *, #105904, .T. ) ;
#17011 = CARTESIAN_POINT ( 'NONE',  ( 6.643884894376894223, -7.802125718944335375, 4.061124033062993374E-12 ) ) ;
#17012 = CIRCLE ( 'NONE', #78972, 1.000000000000023981 ) ;
#17013 = EDGE_CURVE ( 'NONE', #21895, #36223, #23121, .T. ) ;
#17014 = CARTESIAN_POINT ( 'NONE',  ( -34.98071605568955533, 490.8360413343443724, 11.88490725385787705 ) ) ;
#17015 = CARTESIAN_POINT ( 'NONE',  ( -5.656854249492381470, -25.25000000409677270, 5.656854249492379694 ) ) ;
#17016 = CARTESIAN_POINT ( 'NONE',  ( 35.00384615384614762, -4.171999999999999709, 0.000000000000000000 ) ) ;
#17017 = AXIS2_PLACEMENT_3D ( 'NONE', #46218, #58416, #83733 ) ;
#17018 = CARTESIAN_POINT ( 'NONE',  ( 33.38504658727612906, 488.8572893496567531, 10.16177171493806952 ) ) ;
#17019 = CARTESIAN_POINT ( 'NONE',  ( -7.500000000000007105, 40.28750026290749275, -59.87155394325278479 ) ) ;
#17020 = CARTESIAN_POINT ( 'NONE',  ( -10.11206553723567936, 7.339953826372402013, 5.000000000000038192 ) ) ;
#17021 = CARTESIAN_POINT ( 'NONE',  ( 6.928203230275511437, -9.734738430674132914, 4.000000000000000000 ) ) ;
#17022 = DIRECTION ( 'NONE',  ( 0.9984574205382035217, -8.193440825348730876E-15, -0.05552278246086851665 ) ) ;
#17023 = EDGE_LOOP ( 'NONE', ( #63418, #40567, #3669, #76789, #52329 ) ) ;
#17024 = FILL_AREA_STYLE_COLOUR ( '', #52235 ) ;
#17025 = CARTESIAN_POINT ( 'NONE',  ( 10.59999999999999609, 1.533819458162526451E-15, 0.000000000000000000 ) ) ;
#17026 = DIRECTION ( 'NONE',  ( 0.000000000000000000, 1.000000000000000000, 0.000000000000000000 ) ) ;
#17027 = CARTESIAN_POINT ( 'NONE',  ( -91.19955518054493382, -29.99999999999999645, 190.5738738779320158 ) ) ;
#17028 = EDGE_CURVE ( 'NONE', #61182, #96036, #66012, .T. ) ;
#17029 = VECTOR ( 'NONE', #6538, 1000.000000000000000 ) ;
#17030 = CARTESIAN_POINT ( 'NONE',  ( 38.64176212055058812, 25.32107803816180791, -11.54726517548278686 ) ) ;
#17031 = CARTESIAN_POINT ( 'NONE',  ( 71.85927879119853401, -57.67665524272614164, 170.6229705935681409 ) ) ;
#17033 = CARTESIAN_POINT ( 'NONE',  ( -9.810861164843071691, 53.41087315403468239, 2.841314465358082852 ) ) ;
#17032 = CARTESIAN_POINT ( 'NONE',  ( -1.469576158976823947E-15, -16.06250000409677270, 8.000000000000000000 ) ) ;
#17034 = AXIS2_PLACEMENT_3D ( 'NONE', #64339, #15766, #7657 ) ;
#17035 = CIRCLE ( 'NONE', #73836, 12.00000000000003908 ) ;
#17036 = CARTESIAN_POINT ( 'NONE',  ( 23.83070367701998649, -27.26789081566746020, -38.40467348746060594 ) ) ;
#17037 = CARTESIAN_POINT ( 'NONE',  ( -0.4150371643087381601, 43.19867153370302759, 18.68204839779363624 ) ) ;
#17038 = CARTESIAN_POINT ( 'NONE',  ( -38.51282804766191248, 490.3045649922998450, 12.08595093631691952 ) ) ;
#17039 = CARTESIAN_POINT ( 'NONE',  ( -47.23625786575815511, -60.00000000000000000, 65.30679591831491848 ) ) ;
#17040 = CARTESIAN_POINT ( 'NONE',  ( 14.15481990207392649, 21.07020540569414635, 5.915594321928214327 ) ) ;
#17041 = AXIS2_PLACEMENT_3D ( 'NONE', #75289, #2463, #83385 ) ;
#17042 = CARTESIAN_POINT ( 'NONE',  ( 34.64581139903178553, 463.6418748650359589, 19.44242283797247239 ) ) ;
#17043 = CARTESIAN_POINT ( 'NONE',  ( -86.96091939859486786, -35.41414515093074300, 188.0763737881594579 ) ) ;
#17044 = ORIENTED_EDGE ( 'NONE', *, *, #50019, .T. ) ;
#17045 = CARTESIAN_POINT ( 'NONE',  ( 18.91772294109960484, 48.25776538899425816, 62.18609455222646432 ) ) ;
#17046 = CARTESIAN_POINT ( 'NONE',  ( -8.168619677412065627, -39.47607859267740338, 30.46221458393393888 ) ) ;
#17048 = CARTESIAN_POINT ( 'NONE',  ( 4.749156675558425356, -64.72194359721190438, 13.06006237490043453 ) ) ;
#17047 = CARTESIAN_POINT ( 'NONE',  ( -102.3236051589763207, -60.00000000000002132, 193.7633069716393095 ) ) ;
#17049 = VERTEX_POINT ( 'NONE', #47363 ) ;
#17050 = PRESENTATION_STYLE_ASSIGNMENT (( #66118 ) ) ;
#17051 = B_SPLINE_CURVE_WITH_KNOTS ( 'NONE', 3,
 ( #33501, #42634, #2702, #100337, #66376, #43177 ),
 .UNSPECIFIED., .F., .F.,
 ( 4, 2, 4 ),
 ( 0.000000000000000000, 0.001916782365093508281, 0.003833564730187016562 ),
 .UNSPECIFIED. ) ;
#17052 = VECTOR ( 'NONE', #64237, 1000.000000000000000 ) ;
#17053 = CARTESIAN_POINT ( 'NONE',  ( -7.543027128863474040, -5.000000000008911982, -20.22853049137013315 ) ) ;
#17054 = CARTESIAN_POINT ( 'NONE',  ( -7.986452802927061612, 33.97309757691886034, 0.5332468218996333498 ) ) ;
#17055 = CARTESIAN_POINT ( 'NONE',  ( 36.48153863437710243, 303.2350093248795702, -8.088982545662673829 ) ) ;
#17056 = DIRECTION ( 'NONE',  ( 0.000000000000000000, 0.000000000000000000, 1.000000000000000000 ) ) ;
#17057 = CARTESIAN_POINT ( 'NONE',  ( -7.344361273354515163, -82.55439469411474818, -3.175733139645588121 ) ) ;
#17058 = CYLINDRICAL_SURFACE ( 'NONE', #32422, 4.000000000000000000 ) ;
#17059 = CARTESIAN_POINT ( 'NONE',  ( 114.0149080866908946, -60.00000000000002132, 183.4845764411877553 ) ) ;
#17060 = DIRECTION ( 'NONE',  ( 0.000000000000000000, 1.000000000000000000, 0.000000000000000000 ) ) ;
#17061 = ORIENTED_EDGE ( 'NONE', *, *, #86349, .T. ) ;
#17062 = CARTESIAN_POINT ( 'NONE',  ( 0.000000000000000000, 0.000000000000000000, 3.469446951953614189E-15 ) ) ;
#17063 = FACE_OUTER_BOUND ( 'NONE', #38412, .T. ) ;
#17064 =( NAMED_UNIT ( * ) SI_UNIT ( $, .STERADIAN. ) SOLID_ANGLE_UNIT ( ) );
#17065 = TOROIDAL_SURFACE ( 'NONE', #60136, 8.400000000000000355, 0.5999999999999978684 ) ;
#17066 = CARTESIAN_POINT ( 'NONE',  ( 6.499999999999999112, -3.752776749732586126, -8.000000000000000000 ) ) ;
#17067 = CARTESIAN_POINT ( 'NONE',  ( 43.66704108187254008, 409.2854991616131315, 16.12724780824946791 ) ) ;
#17068 = PRESENTATION_LAYER_ASSIGNMENT (  '', '', ( #103226 ) ) ;
#17069 = CARTESIAN_POINT ( 'NONE',  ( 6.683837171061803417, -3.955946848495962787, 6.851900933636989599 ) ) ;
#17070 = VERTEX_POINT ( 'NONE', #80250 ) ;
#17071 = DIRECTION ( 'NONE',  ( 1.000000000000000000, 0.000000000000000000, -0.000000000000000000 ) ) ;
#17072 = ORIENTED_EDGE ( 'NONE', *, *, #56000, .F. ) ;
#17073 = CARTESIAN_POINT ( 'NONE',  ( 35.40294873602728387, 484.3215194930215830, -1.486762578860570283 ) ) ;
#17074 =( LENGTH_UNIT ( ) NAMED_UNIT ( * ) SI_UNIT ( .MILLI., .METRE. ) );
#17075 = CARTESIAN_POINT ( 'NONE',  ( 32.80261435968075290, 487.0248074982611115, 8.977354182173554520 ) ) ;
#17076 = EDGE_CURVE ( 'NONE', #12958, #40315, #102198, .T. ) ;
#17077 = CARTESIAN_POINT ( 'NONE',  ( 43.69716417794892749, 48.00000000000000000, 48.48761666242516100 ) ) ;
#17078 = CARTESIAN_POINT ( 'NONE',  ( 5.959015317364894315, -13.75072846948223493, 13.79531249880999155 ) ) ;
#17079 = B_SPLINE_CURVE_WITH_KNOTS ( 'NONE', 3,
 ( #83630, #9733, #42650, #67473, #59930, #92795 ),
 .UNSPECIFIED., .F., .F.,
 ( 4, 2, 4 ),
 ( 2.103915656028635642E-15, 0.01115854487611434888, 0.02231708975222659180 ),
 .UNSPECIFIED. ) ;
#17080 = CARTESIAN_POINT ( 'NONE',  ( -40.83166867234564279, -60.00000000001944755, 57.76263198987851410 ) ) ;
#17081 = CARTESIAN_POINT ( 'NONE',  ( 46.00000000000000000, 438.0166301925371499, 11.64259471674452229 ) ) ;
#17082 = ORIENTED_EDGE ( 'NONE', *, *, #57053, .F. ) ;
#17083 = CARTESIAN_POINT ( 'NONE',  ( 91.93227393908065892, -60.00000000000002842, 7.599392352668481010 ) ) ;
#17085 = CARTESIAN_POINT ( 'NONE',  ( 14.39634327219153143, -29.02992103934742474, 28.84133556504098905 ) ) ;
#17084 = CARTESIAN_POINT ( 'NONE',  ( -80.78871696068775066, -30.00000000000004974, 192.9492619026495390 ) ) ;
#17086 = AXIS2_PLACEMENT_3D ( 'NONE', #13006, #102573, #45931 ) ;
#17087 = CARTESIAN_POINT ( 'NONE',  ( 34.14662298548351771, 464.2250883195994220, 6.054123830998662470 ) ) ;
#17088 = FACE_OUTER_BOUND ( 'NONE', #78016, .T. ) ;
#17089 = EDGE_CURVE ( 'NONE', #63464, #39277, #105649, .T. ) ;
#17090 = CARTESIAN_POINT ( 'NONE',  ( -43.50443149440654622, -22.24771747397159061, 37.57252092150835665 ) ) ;
#17091 = FACE_OUTER_BOUND ( 'NONE', #25008, .T. ) ;
#17092 = ORIENTED_EDGE ( 'NONE', *, *, #67802, .T. ) ;
#17093 = CARTESIAN_POINT ( 'NONE',  ( -19.00223544648545015, -4.285714285714296246, 16.66764709352487017 ) ) ;
#17094 = AXIS2_PLACEMENT_3D ( 'NONE', #55599, #72341, #23284 ) ;
#17095 = DIRECTION ( 'NONE',  ( -0.000000000000000000, -1.000000000000000000, -0.000000000000000000 ) ) ;
#17096 = CARTESIAN_POINT ( 'NONE',  ( 31.19652432992544888, 378.3327707670021027, 24.28948218791313707 ) ) ;
#17097 = AXIS2_PLACEMENT_3D ( 'NONE', #66042, #89795, #41234 ) ;
#17098 = CARTESIAN_POINT ( 'NONE',  ( -30.00000000000000355, 489.4338083968330579, 5.745752720312972350 ) ) ;
#17099 = EDGE_LOOP ( 'NONE', ( #18099, #85694 ) ) ;
#17100 = CARTESIAN_POINT ( 'NONE',  ( 4.973317752991470719, -46.53140123174533471, 102.2736751349651456 ) ) ;
#17101 = CARTESIAN_POINT ( 'NONE',  ( 18.13561277374696701, 1.340359594676612611E-15, 0.000000000000000000 ) ) ;
#17102 = VERTEX_POINT ( 'NONE', #7958 ) ;
#17103 = CARTESIAN_POINT ( 'NONE',  ( 78.27425760720375081, -30.00000000000000711, -15.63494901230772349 ) ) ;
#17104 = CARTESIAN_POINT ( 'NONE',  ( 47.55322331356174459, 10.90908589463668754, 16.76771630193798046 ) ) ;
#17105 = UNCERTAINTY_MEASURE_WITH_UNIT (LENGTH_MEASURE( 1.000000000000000082E-05 ), #57913, 'distance_accuracy_value', 'NONE');
#17107 = EDGE_CURVE ( 'NONE', #75282, #5164, #9170, .T. ) ;
#17106 = LINE ( 'NONE', #83414, #20362 ) ;
#17108 = CARTESIAN_POINT ( 'NONE',  ( 0.000000000000000000, 0.000000000000000000, -5.575057142857143155 ) ) ;
#17109 = CARTESIAN_POINT ( 'NONE',  ( 80.87643365138157492, -30.00000000000000711, 6.461220206471677052 ) ) ;
#17110 = CARTESIAN_POINT ( 'NONE',  ( 7.743982712349851916, 101.5378698523926033, 2.020119794285909265 ) ) ;
#17111 = ORIENTED_EDGE ( 'NONE', *, *, #55288, .F. ) ;
#17112 = MECHANICAL_DESIGN_GEOMETRIC_PRESENTATION_REPRESENTATION (  '', ( #32597 ), #82535 ) ;
#17113 = ORIENTED_EDGE ( 'NONE', *, *, #22161, .T. ) ;
#17114 = VERTEX_POINT ( 'NONE', #91563 ) ;
#17115 = CARTESIAN_POINT ( 'NONE',  ( 19.29515645702225868, 5.000000000000003553, 0.000000000000000000 ) ) ;
#17116 = CARTESIAN_POINT ( 'NONE',  ( -1.338977211094423136, -5.480044445862255031, -13.97241428226087301 ) ) ;
#17117 = CARTESIAN_POINT ( 'NONE',  ( -19.46358522980415273, 49.98601987196752106, 60.49302799977217404 ) ) ;
#17118 = CARTESIAN_POINT ( 'NONE',  ( -41.35772432385135033, 464.3624544568689316, 17.55089308074047949 ) ) ;
#17119 = CARTESIAN_POINT ( 'NONE',  ( -31.19347262973593615, 380.6645121172051631, 24.42694056262163116 ) ) ;
#17120 = DIRECTION ( 'NONE',  ( -1.000000000000000000, -0.000000000000000000, -0.000000000000000000 ) ) ;
#17122 = ORIENTED_EDGE ( 'NONE', *, *, #26387, .F. ) ;
#17121 = AXIS2_PLACEMENT_3D ( 'NONE', #105187, #14556, #55544 ) ;
#17123 = CARTESIAN_POINT ( 'NONE',  ( 42.43166099483027409, 436.1632441641384617, 19.16791492759929838 ) ) ;
#17124 = ORIENTED_EDGE ( 'NONE', *, *, #92804, .F. ) ;
#17125 = FILL_AREA_STYLE ('',( #26317 ) ) ;
#17126 = CARTESIAN_POINT ( 'NONE',  ( 81.60207891900830646, -38.84190146155946621, 195.4036435249389854 ) ) ;
#17127 = CARTESIAN_POINT ( 'NONE',  ( 6.289692432696804225, 5.239086202715451002, -4.583616368338175207 ) ) ;
#17128 = CARTESIAN_POINT ( 'NONE',  ( 29.32203595473246693, 297.8341598778472985, 10.59484822235428325 ) ) ;
#17129 = DIRECTION ( 'NONE',  ( 1.150791560227848051E-16, -0.3420201433256733758, 0.9396926207859066515 ) ) ;
#17130 = FILL_AREA_STYLE ('',( #91025 ) ) ;
#17131 = B_SPLINE_CURVE_WITH_KNOTS ( 'NONE', 3,
 ( #100098, #7890, #40798, #26266 ),
 .UNSPECIFIED., .F., .F.,
 ( 4, 4 ),
 ( 2.409751485173049940E-15, 0.0004300933845494213218 ),
 .UNSPECIFIED. ) ;
#17132 = CARTESIAN_POINT ( 'NONE',  ( -27.10511071441192144, 34.47735702144345282, -10.05698433968589178 ) ) ;
#17133 = CARTESIAN_POINT ( 'NONE',  ( 42.62984607896018474, 365.9487680686676754, 17.22660553029483665 ) ) ;
#17134 =( BOUNDED_SURFACE ( )  B_SPLINE_SURFACE ( 3, 2, ( 
 ( #686, #82713, #89223 ),
 ( #73539, #83239, #162 ),
 ( #17467, #32063, #81622 ),
 ( #8816, #24517, #66530 ) ),
 .UNSPECIFIED., .F., .F., .F. ) 
 B_SPLINE_SURFACE_WITH_KNOTS ( ( 4, 4 ),
 ( 3, 3 ),
 ( 4.640385298237958978E-17, 0.002473307515785300430 ),
 ( 0.000000000000000000, 1.000000000000000000 ),
 .UNSPECIFIED. ) 
 GEOMETRIC_REPRESENTATION_ITEM ( )  RATIONAL_B_SPLINE_SURFACE ( (
 ( 1.000000000000000000, 0.7904469216846371493, 1.000000000000000000),
 ( 1.000000000000000000, 0.7997328579911862079, 1.000000000000000000),
 ( 1.000000000000000000, 0.8083744009265905195, 1.000000000000000000),
 ( 1.000000000000000000, 0.8138888783291118312, 1.000000000000000000) ) ) 
 REPRESENTATION_ITEM ( '' )  SURFACE ( )  );
#17135 = DIRECTION ( 'NONE',  ( -1.000000000000000000, -0.000000000000000000, -0.000000000000000000 ) ) ;
#17136 = EDGE_CURVE ( 'NONE', #4391, #81365, #41917, .T. ) ;
#17137 = DIRECTION ( 'NONE',  ( 0.000000000000000000, 0.000000000000000000, 1.000000000000000000 ) ) ;
#17138 = ORIENTED_EDGE ( 'NONE', *, *, #82945, .F. ) ;
#17139 = CARTESIAN_POINT ( 'NONE',  ( -27.42347756180437557, 296.7082162746293648, 10.34135678911163048 ) ) ;
#17140 = CARTESIAN_POINT ( 'NONE',  ( 0.000000000000000000, -14.49999999999999822, 0.000000000000000000 ) ) ;
#17141 = UNCERTAINTY_MEASURE_WITH_UNIT (LENGTH_MEASURE( 1.000000000000000082E-05 ), #9670, 'distance_accuracy_value', 'NONE');
#17142 = DIRECTION ( 'NONE',  ( 0.000000000000000000, 0.000000000000000000, -1.000000000000000000 ) ) ;
#17143 = CARTESIAN_POINT ( 'NONE',  ( 3.313708498984762496, -11.28124999999999289, 7.999999999999998224 ) ) ;
#17144 = DIRECTION ( 'NONE',  ( -1.000000000000000000, -1.224606353822377258E-16, -0.000000000000000000 ) ) ;
#17145 = EDGE_CURVE ( 'NONE', #46054, #96778, #3476, .T. ) ;
#17146 = ADVANCED_FACE ( 'NONE', ( #51067 ), #93823, .F. ) ;
#17147 = CARTESIAN_POINT ( 'NONE',  ( 1.406471811252868021, 302.0905290902286424, 9.901083696907180709 ) ) ;
#17148 = AXIS2_PLACEMENT_3D ( 'NONE', #101580, #27195, #36361 ) ;
#17149 = DIRECTION ( 'NONE',  ( 0.000000000000000000, 1.000000000000000000, 0.000000000000000000 ) ) ;
#17150 = CARTESIAN_POINT ( 'NONE',  ( 85.09886940956974399, -46.56413427295240837, 187.7708649785900832 ) ) ;
#17151 = B_SPLINE_CURVE_WITH_KNOTS ( 'NONE', 3,
 ( #69813, #35895, #36430, #93567 ),
 .UNSPECIFIED., .F., .F.,
 ( 4, 4 ),
 ( 4.906538933386797242E-17, 0.001346487449956126773 ),
 .UNSPECIFIED. ) ;
#17152 = SURFACE_STYLE_FILL_AREA ( #25256 ) ;
#17153 = AXIS2_PLACEMENT_3D ( 'NONE', #79648, #5761, #48331 ) ;
#17154 = CARTESIAN_POINT ( 'NONE',  ( 36.48461538461538822, 1.411358822780289120E-15, 0.000000000000000000 ) ) ;
#17155 = ORIENTED_EDGE ( 'NONE', *, *, #74493, .F. ) ;
#17156 = CARTESIAN_POINT ( 'NONE',  ( 93.03188089276335404, -57.65588774053570376, -17.14181286654005376 ) ) ;
#17157 = CYLINDRICAL_SURFACE ( 'NONE', #29689, 5.000000000000002665 ) ;
#17158 = LINE ( 'NONE', #59741, #11025 ) ;
#17159 = CARTESIAN_POINT ( 'NONE',  ( 0.5805565836007605673, 3.752776749732565253, 6.499999999999997335 ) ) ;
#17160 = CARTESIAN_POINT ( 'NONE',  ( -81.59247734337886016, -30.00000000000000000, -7.117116539340933024 ) ) ;
#17161 = EDGE_CURVE ( 'NONE', #18270, #87322, #43536, .T. ) ;
#17162 = CARTESIAN_POINT ( 'NONE',  ( 99.75754961941544252, 5.000000000000020428, 0.000000000000000000 ) ) ;
#17163 = CARTESIAN_POINT ( 'NONE',  ( 22.13642162920427126, 27.78492472323462792, -32.60352800065684420 ) ) ;
#17164 = DIRECTION ( 'NONE',  ( 0.000000000000000000, 0.000000000000000000, -1.000000000000000000 ) ) ;
#17166 = CARTESIAN_POINT ( 'NONE',  ( 33.00000000000000000, 461.8887775513397855, 11.55279652844103566 ) ) ;
#17165 = CARTESIAN_POINT ( 'NONE',  ( 3.508895115991522928, -48.85046701618207265, 104.5950737443334759 ) ) ;
#17167 = CARTESIAN_POINT ( 'NONE',  ( -10.12668159690567649, 1.256356190803089060E-15, -10.00000000000000000 ) ) ;
#17168 = CARTESIAN_POINT ( 'NONE',  ( -28.61312531052638519, 18.65874454358749190, 40.19656138064493689 ) ) ;
#17169 = CARTESIAN_POINT ( 'NONE',  ( -15.89325899475126391, 43.76119630618126877, -6.420346730828080162 ) ) ;
#17170 = CARTESIAN_POINT ( 'NONE',  ( 5.477432325710316796, -81.83520464429525987, 2.459915882346686899 ) ) ;
#17171 = DIRECTION ( 'NONE',  ( -1.000000000000000000, -1.224606353822377258E-16, -0.000000000000000000 ) ) ;
#17172 = DIRECTION ( 'NONE',  ( 0.5735764363510557073, -0.8191520442889850262, 1.003171929053516612E-16 ) ) ;
#17173 = EDGE_CURVE ( 'NONE', #4466, #105449, #33322, .T. ) ;
#17174 = CARTESIAN_POINT ( 'NONE',  ( -96.81748461682487061, -38.00000000001091394, 192.8978395531862020 ) ) ;
#17175 = ORIENTED_EDGE ( 'NONE', *, *, #68885, .T. ) ;
#17176 = CARTESIAN_POINT ( 'NONE',  ( 6.770548583014334376, 9.415629875647791636, 1.794845940801068851 ) ) ;
#17177 = DIRECTION ( 'NONE',  ( 1.000000000000000000, 0.000000000000000000, 0.000000000000000000 ) ) ;
#17178 = CARTESIAN_POINT ( 'NONE',  ( 53.29999999999999716, 6.915964383211875250E-15, 0.000000000000000000 ) ) ;
#17179 = CARTESIAN_POINT ( 'NONE',  ( -67.34689840167415298, -29.89196498055581230, -22.02968126997568632 ) ) ;
#17181 = CARTESIAN_POINT ( 'NONE',  ( 30.56153846153846132, 1.411358822780289120E-15, 0.000000000000000000 ) ) ;
#17180 = DIRECTION ( 'NONE',  ( 0.000000000000000000, 0.000000000000000000, 1.000000000000000000 ) ) ;
#17182 = ORIENTED_EDGE ( 'NONE', *, *, #72214, .T. ) ;
#17183 = VECTOR ( 'NONE', #92000, 1000.000000000000000 ) ;
#17184 =( LENGTH_UNIT ( ) NAMED_UNIT ( * ) SI_UNIT ( .MILLI., .METRE. ) );
#17185 = CIRCLE ( 'NONE', #10310, 4.250000000000000000 ) ;
#17186 = ORIENTED_EDGE ( 'NONE', *, *, #66634, .T. ) ;
#17187 = CARTESIAN_POINT ( 'NONE',  ( 0.01372220897661740636, -5.309964801958117597, 3.802871176606131609 ) ) ;
#17188 = CARTESIAN_POINT ( 'NONE',  ( 37.50059943756055247, 490.7879993827821181, 12.38039871356680344 ) ) ;
#17189 = FACE_OUTER_BOUND ( 'NONE', #29690, .T. ) ;
#17190 = CARTESIAN_POINT ( 'NONE',  ( -76.04298135053677754, -59.99999999999997868, -30.12288092604498146 ) ) ;
#17191 = ORIENTED_EDGE ( 'NONE', *, *, #93644, .F. ) ;
#17192 = CARTESIAN_POINT ( 'NONE',  ( 8.604130785002874120E-16, 67.00000000000002842, 7.025805963803935406 ) ) ;
#17193 = CARTESIAN_POINT ( 'NONE',  ( -6.086036594375756614, 294.7541636957752758, -7.939907524234526726 ) ) ;
#17194 = CARTESIAN_POINT ( 'NONE',  ( 99.74981209804160187, -45.27117877547765801, 192.8220496481170585 ) ) ;
#17196 = CARTESIAN_POINT ( 'NONE',  ( -46.92658635379587651, 13.66002169525844145, 15.01004073971070341 ) ) ;
#17195 = CARTESIAN_POINT ( 'NONE',  ( 31.97977251168731527, -31.54705716108501790, 32.42483364381936184 ) ) ;
#17197 = ORIENTED_EDGE ( 'NONE', *, *, #103518, .T. ) ;
#17198 = ORIENTED_EDGE ( 'NONE', *, *, #96075, .F. ) ;
#17199 = VERTEX_POINT ( 'NONE', #25249 ) ;
#17200 = CARTESIAN_POINT ( 'NONE',  ( 31.18696128861778760, 357.2396685113180865, 20.55154636943739632 ) ) ;
#17201 = VECTOR ( 'NONE', #84609, 1000.000000000000000 ) ;
#17202 = DIRECTION ( 'NONE',  ( 0.000000000000000000, 0.000000000000000000, 1.000000000000000000 ) ) ;
#17203 = CARTESIAN_POINT ( 'NONE',  ( 9.500000000000003553, -5.000000000000000000, -68.91429205785459544 ) ) ;
#17204 = ORIENTED_EDGE ( 'NONE', *, *, #81339, .F. ) ;
#17205 = EDGE_CURVE ( 'NONE', #98241, #82573, #64344, .T. ) ;
#17206 = CYLINDRICAL_SURFACE ( 'NONE', #41017, 8.000000000000000000 ) ;
#17207 = CARTESIAN_POINT ( 'NONE',  ( -7.150000000000003908, 41.64999999999997726, -68.91429205801804869 ) ) ;
#17208 = CARTESIAN_POINT ( 'NONE',  ( -5.290067270632215823, 53.47475093287481229, 8.531152949374556371 ) ) ;
#17209 = CARTESIAN_POINT ( 'NONE',  ( -32.88842731267402542, -57.69106633777249016, 47.18465683205923966 ) ) ;
#17210 = CARTESIAN_POINT ( 'NONE',  ( 7.188101187500000044, -28.15625000204838813, 0.000000000000000000 ) ) ;
#17211 = CIRCLE ( 'NONE', #77497, 5.000000000000000000 ) ;
#17212 = CARTESIAN_POINT ( 'NONE',  ( 28.58349330513380337, 4.000000000000002665, 0.000000000000000000 ) ) ;
#17213 = CARTESIAN_POINT ( 'NONE',  ( -23.61963550967466574, 306.0340374937824777, 10.19690224617928287 ) ) ;
#17214 = DIRECTION ( 'NONE',  ( -1.000000000000000000, 0.000000000000000000, 0.000000000000000000 ) ) ;
#17215 = CARTESIAN_POINT ( 'NONE',  ( 2.769948622550640671, -30.00000000000000000, -40.00000000000000000 ) ) ;
#17216 = EDGE_CURVE ( 'NONE', #66061, #10937, #50534, .T. ) ;
#17217 = CARTESIAN_POINT ( 'NONE',  ( -51.84566471874714466, -38.00000000000001421, 53.44666163652544100 ) ) ;
#17218 = ADVANCED_FACE ( 'NONE', ( #76415, #99087 ), #67809, .T. ) ;
#17219 = CARTESIAN_POINT ( 'NONE',  ( -49.20250961229047704, -46.44356504767149119, 51.70527583391724136 ) ) ;
#17220 = AXIS2_PLACEMENT_3D ( 'NONE', #75025, #85821, #62594 ) ;
#17221 = DIRECTION ( 'NONE',  ( 0.000000000000000000, -1.000000000000000000, 0.000000000000000000 ) ) ;
#17222 = ORIENTED_EDGE ( 'NONE', *, *, #62626, .F. ) ;
#17223 = CARTESIAN_POINT ( 'NONE',  ( -101.1758500044991820, -60.25291044919993055, 194.9948784670219766 ) ) ;
#17224 = CIRCLE ( 'NONE', #93046, 4.000000000000000000 ) ;
#17225 = FACE_OUTER_BOUND ( 'NONE', #71537, .T. ) ;
#17226 = CIRCLE ( 'NONE', #70643, 1.000000000000014877 ) ;
#17227 = CARTESIAN_POINT ( 'NONE',  ( 9.275666170511263076, -2.831271561983539797, 14.74122513583426120 ) ) ;
#17228 = ORIENTED_EDGE ( 'NONE', *, *, #62201, .F. ) ;
#17229 = CARTESIAN_POINT ( 'NONE',  ( -17.07866832072232910, 34.90909537143385677, -21.83975874131578720 ) ) ;
#17230 = CARTESIAN_POINT ( 'NONE',  ( 80.05853955895231877, -38.78746072163605163, 193.1034648313674893 ) ) ;
#17231 = DIRECTION ( 'NONE',  ( 0.000000000000000000, 1.000000000000000000, 0.000000000000000000 ) ) ;
#17232 = DIRECTION ( 'NONE',  ( -0.000000000000000000, 1.000000000000000000, -0.000000000000000000 ) ) ;
#17234 = EDGE_CURVE ( 'NONE', #50622, #51147, #4041, .T. ) ;
#17233 = CARTESIAN_POINT ( 'NONE',  ( -17.19041072168119300, 294.5876824650746357, 9.880858205605974831 ) ) ;
#17235 = EDGE_CURVE ( 'NONE', #20011, #36994, #24701, .T. ) ;
#17236 = CARTESIAN_POINT ( 'NONE',  ( -41.46910480219105466, 484.7338956289799512, -3.418960549710621244 ) ) ;
#17237 = CARTESIAN_POINT ( 'NONE',  ( 85.91789968996276627, -30.00000000000000000, 178.0337372095932835 ) ) ;
#17238 = CARTESIAN_POINT ( 'NONE',  ( 35.47838770905575956, 490.5979824477001330, 12.29204623667445340 ) ) ;
#17239 = CARTESIAN_POINT ( 'NONE',  ( -29.27148335582101879, 13.57837266936924614, 39.67318301868861852 ) ) ;
#17240 = PLANE ( 'NONE',  #113 ) ;
#17241 = ORIENTED_EDGE ( 'NONE', *, *, #79990, .T. ) ;
#17242 = VERTEX_POINT ( 'NONE', #26860 ) ;
#17243 = CARTESIAN_POINT ( 'NONE',  ( 53.00628815327823418, -49.90450768202155274, 60.14456217209944100 ) ) ;
#17244 = DIRECTION ( 'NONE',  ( -1.000000000000000000, -1.224606353822377258E-16, -0.000000000000000000 ) ) ;
#17245 = AXIS2_PLACEMENT_3D ( 'NONE', #102709, #61744, #21292 ) ;
#17246 = DIRECTION ( 'NONE',  ( 0.000000000000000000, 0.000000000000000000, -1.000000000000000000 ) ) ;
#17247 = ORIENTED_EDGE ( 'NONE', *, *, #46916, .F. ) ;
#17248 = CARTESIAN_POINT ( 'NONE',  ( -92.73019748878142821, -38.35494930991703200, 41.19300550259715266 ) ) ;
#17249 = ORIENTED_EDGE ( 'NONE', *, *, #66554, .T. ) ;
#17250 = SURFACE_STYLE_FILL_AREA ( #26432 ) ;
#17251 = CARTESIAN_POINT ( 'NONE',  ( 98.52895140874336732, -38.35583712414237567, 79.77947616707253076 ) ) ;
#17252 = CARTESIAN_POINT ( 'NONE',  ( 12.87288491891443165, 21.40780029432582765, -5.438759071948315871 ) ) ;
#17253 = CARTESIAN_POINT ( 'NONE',  ( 83.90565905403732927, -45.28278352932714768, 21.05830037911174202 ) ) ;
#17254 = CARTESIAN_POINT ( 'NONE',  ( -31.03678703374875525, 438.6650838204938623, 21.86890379898548176 ) ) ;
#17255 = CARTESIAN_POINT ( 'NONE',  ( -33.77559172535808329, 464.7834715296605737, 7.192701217093241617 ) ) ;
#17256 = CARTESIAN_POINT ( 'NONE',  ( -32.96072870876664496, 317.2200023992991191, -6.776755668305763258 ) ) ;
#17257 = PRESENTATION_STYLE_ASSIGNMENT (( #98668 ) ) ;
#17258 = CARTESIAN_POINT ( 'NONE',  ( 75.51285980042941048, -59.99999999999997868, 184.5535044986175706 ) ) ;
#17259 = CARTESIAN_POINT ( 'NONE',  ( -43.42366826522957268, 435.2488004288641719, 10.12833319149509315 ) ) ;
#17260 = ORIENTED_EDGE ( 'NONE', *, *, #71006, .T. ) ;
#17261 = CARTESIAN_POINT ( 'NONE',  ( 62.01696980690892502, -49.91133272125355091, 82.86793255174956130 ) ) ;
#17262 = CARTESIAN_POINT ( 'NONE',  ( -24.69387026086019432, 295.5389138248296490, -1.852611171248429445 ) ) ;
#17263 = CARTESIAN_POINT ( 'NONE',  ( 9.269255467170962604, -52.95527593926346555, 23.24713075214419433 ) ) ;
#17264 = MECHANICAL_DESIGN_GEOMETRIC_PRESENTATION_REPRESENTATION (  '', ( #5174 ), #8614 ) ;
#17266 = CARTESIAN_POINT ( 'NONE',  ( -36.37693845632723111, 485.4380683983963536, -3.604171430931530029 ) ) ;
#17265 = CARTESIAN_POINT ( 'NONE',  ( -83.01601276650154659, -38.35698986964714408, -24.47564496195118977 ) ) ;
#17267 = CARTESIAN_POINT ( 'NONE',  ( -32.85315808798738146, 354.3401018246705689, 21.52737482615226483 ) ) ;
#17268 = DIRECTION ( 'NONE',  ( 0.000000000000000000, 0.000000000000000000, 1.000000000000000000 ) ) ;
#17269 = CARTESIAN_POINT ( 'NONE',  ( -10.00000000000000355, 30.00000000000000000, 4.000000000000000000 ) ) ;
#17270 = CARTESIAN_POINT ( 'NONE',  ( -3.313708498984760720, -28.53124999999999289, -8.000000000000000000 ) ) ;
#17271 = LINE ( 'NONE', #97622, #27946 ) ;
#17272 = CIRCLE ( 'NONE', #15545, 4.000000000000001776 ) ;
#17273 = ADVANCED_FACE ( 'NONE', ( #75891 ), #84531, .T. ) ;
#17274 = DIRECTION ( 'NONE',  ( -1.000000000000000000, -1.224606353822377258E-16, -0.000000000000000000 ) ) ;
#17275 = ORIENTED_EDGE ( 'NONE', *, *, #76613, .F. ) ;
#17276 = CARTESIAN_POINT ( 'NONE',  ( 85.81319990892043847, -21.82339626730217930, 170.1690506418119355 ) ) ;
#17277 = CARTESIAN_POINT ( 'NONE',  ( 30.00000000000000000, 489.8676322012278774, 6.488549987513861694 ) ) ;
#17278 = CARTESIAN_POINT ( 'NONE',  ( -40.49327943412436071, 437.8143148761543557, 21.96882124328788066 ) ) ;
#17279 = EDGE_LOOP ( 'NONE', ( #33067, #18100 ) ) ;
#17280 = CARTESIAN_POINT ( 'NONE',  ( 0.000000000000000000, 70.00000000000000000, -10.00000000000000178 ) ) ;
#17281 = CIRCLE ( 'NONE', #77550, 4.000000000000007105 ) ;
#17282 = FACE_OUTER_BOUND ( 'NONE', #47614, .T. ) ;
#17283 = FACE_OUTER_BOUND ( 'NONE', #16218, .T. ) ;
#17284 = CARTESIAN_POINT ( 'NONE',  ( 0.000000000000000000, 67.00000000000002842, 0.000000000000000000 ) ) ;
#17285 = CARTESIAN_POINT ( 'NONE',  ( -18.75852657729457107, -25.38507213530491669, -38.49965030021739665 ) ) ;
#17286 = CARTESIAN_POINT ( 'NONE',  ( -11.84876416945811961, -1.967757499684315237, 20.63514712866197343 ) ) ;
#17287 = AXIS2_PLACEMENT_3D ( 'NONE', #69771, #61702, #94594 ) ;
#17288 = EDGE_CURVE ( 'NONE', #18270, #91139, #93147, .T. ) ;
#17289 = B_SPLINE_CURVE_WITH_KNOTS ( 'NONE', 3,
 ( #58001, #66103, #17038, #50966, #34308, #9992, #26754, #76851, #33230, #66638, #68240, #25700 ),
 .UNSPECIFIED., .F., .F.,
 ( 4, 2, 2, 2, 2, 4 ),
 ( 4.993455085690288581E-15, 0.001726505353950908653, 0.002589758030923909431, 0.003453010707896910208, 0.005179516061842909594, 0.006906021415788908546 ),
 .UNSPECIFIED. ) ;
#17290 = TOROIDAL_SURFACE ( 'NONE', #27640, 8.000000000000000000, 1.000000000000000000 ) ;
#17291 = CARTESIAN_POINT ( 'NONE',  ( 56.62629245603895356, -60.00000000000001421, 90.03670186600696468 ) ) ;
#17292 = CARTESIAN_POINT ( 'NONE',  ( 46.00000000000000000, 488.7529659943156162, 4.223909611882176840 ) ) ;
#17293 = CARTESIAN_POINT ( 'NONE',  ( 29.05774046782589437, -21.22587610620614740, 31.99305267930822794 ) ) ;
#17295 = CARTESIAN_POINT ( 'NONE',  ( -13.68089852145233820, 22.80932735910137055, 2.024255124915971482 ) ) ;
#17294 = CARTESIAN_POINT ( 'NONE',  ( -21.88691883039211561, -26.94070025036754856, 37.30577011176958990 ) ) ;
#17296 = VECTOR ( 'NONE', #99676, 1000.000000000000114 ) ;
#17297 = CARTESIAN_POINT ( 'NONE',  ( 2.977408999572651815, -16.43750000204838457, 7.188101187500000933 ) ) ;
#17298 = FACE_OUTER_BOUND ( 'NONE', #31600, .T. ) ;
#17299 = CARTESIAN_POINT ( 'NONE',  ( 0.000000000000000000, 0.000000000000000000, -0.02540000000000007530 ) ) ;
#17300 = ADVANCED_FACE ( 'NONE', ( #50017 ), #97032, .T. ) ;
#17301 = VERTEX_POINT ( 'NONE', #42458 ) ;
#17302 = EDGE_CURVE ( 'NONE', #17325, #82529, #96117, .T. ) ;
#17303 = COLOUR_RGB ( '', 0.40784314, 0.44705882, 0.49803922) ;
#17304 = CARTESIAN_POINT ( 'NONE',  ( -17.49999999999077360, 50.03176226080658040, 60.82931034967823081 ) ) ;
#17305 = SURFACE_STYLE_USAGE ( .BOTH. , #91197 ) ;
#17307 = CARTESIAN_POINT ( 'NONE',  ( 19.18395041998931205, -47.40891687610037053, -34.01679967311604713 ) ) ;
#17306 = LINE ( 'NONE', #83085, #88030 ) ;
#17308 = VERTEX_POINT ( 'NONE', #21409 ) ;
#17309 = DIRECTION ( 'NONE',  ( -1.000000000000000000, -0.000000000000000000, -0.000000000000000000 ) ) ;
#17310 = CARTESIAN_POINT ( 'NONE',  ( -4.504790317111235787, 52.18342994161649528, 6.294253490234988924 ) ) ;
#17311 = ORIENTED_EDGE ( 'NONE', *, *, #80192, .T. ) ;
#17312 = VECTOR ( 'NONE', #101394, 1000.000000000000000 ) ;
#17313 = SURFACE_SIDE_STYLE ('',( #91206 ) ) ;
#17314 = LINE ( 'NONE', #74455, #79466 ) ;
#17315 = PRESENTATION_LAYER_ASSIGNMENT (  '', '', ( #67291 ) ) ;
#17316 = CARTESIAN_POINT ( 'NONE',  ( -23.57474994864879037, 41.64982833201018053, -74.87904004496073185 ) ) ;
#17317 = CARTESIAN_POINT ( 'NONE',  ( -95.84732615451282811, -59.99999999999999289, 55.00258849229039981 ) ) ;
#17318 = CARTESIAN_POINT ( 'NONE',  ( 0.000000000000000000, 0.000000000000000000, -6.724735318933162453 ) ) ;
#17319 = CARTESIAN_POINT ( 'NONE',  ( 0.6511518506208968660, -8.763486134561278007, -7.907570769506055086 ) ) ;
#17320 = CARTESIAN_POINT ( 'NONE',  ( 40.44189562491348511, 465.0930618392404199, 17.36238218226302621 ) ) ;
#17322 = CARTESIAN_POINT ( 'NONE',  ( -15.19395690307318425, 3.423339800917871933, 3.910915912819011186 ) ) ;
#17321 = CARTESIAN_POINT ( 'NONE',  ( -34.54755545858651544, 435.5422147998195896, 9.163155746809447777 ) ) ;
#17323 = CARTESIAN_POINT ( 'NONE',  ( -82.57273120623599993, -46.48239456925677615, 176.6345680876003712 ) ) ;
#17324 = B_SPLINE_CURVE_WITH_KNOTS ( 'NONE', 3,
 ( #99541, #83364, #74201, #40776, #65593, #33248, #81748, #105518, #41312, #9463, #15977, #65060, #106573, #49931, #32723, #72615, #24631, #25718, #17054, #41842, #17592, #74730, #90404, #33782, #31659, #66657, #16506, #278, #58577, #49392, #66120, #813, #64542, #89350 ),
 .UNSPECIFIED., .F., .F.,
 ( 4, 2, 2, 2, 2, 2, 2, 2, 2, 2, 2, 2, 2, 2, 2, 2, 4 ),
 ( 3.576224061345498009E-18, 0.0007951492273476417835, 0.001590298454695279881, 0.002385447682042917978, 0.003180596909390556292, 0.003975746136738194172, 0.004770895364085832487, 0.005566044591433469933, 0.006361193818781108247, 0.007156343046128743959, 0.007951492273476381406, 0.008746641500824020588, 0.009541790728171658034, 0.01033693995551929548, 0.01113208918286693466, 0.01192723841021457384, 0.01272238763756220956 ),
 .UNSPECIFIED. ) ;
#17325 = VERTEX_POINT ( 'NONE', #61865 ) ;
#17326 = CARTESIAN_POINT ( 'NONE',  ( 0.000000000000000000, -54.00000000000000711, 41.00000000000000000 ) ) ;
#17327 = ORIENTED_EDGE ( 'NONE', *, *, #50569, .T. ) ;
#17328 = ORIENTED_EDGE ( 'NONE', *, *, #96837, .F. ) ;
#17329 = DIRECTION ( 'NONE',  ( 1.000000000000000000, 1.224606353822377258E-16, 0.000000000000000000 ) ) ;
#17330 = DIRECTION ( 'NONE',  ( 0.000000000000000000, 0.000000000000000000, 1.000000000000000000 ) ) ;
#17331 = EDGE_LOOP ( 'NONE', ( #85703, #14920, #65742, #56077, #58794 ) ) ;
#17332 = CONICAL_SURFACE ( 'NONE', #34602, 6.500000000000000000, 1.047197551196600296 ) ;
#17333 = DIRECTION ( 'NONE',  ( 0.000000000000000000, 0.000000000000000000, -1.000000000000000000 ) ) ;
#17334 = CARTESIAN_POINT ( 'NONE',  ( 0.000000000000000000, -5.629165124598853431, -3.249999999999994227 ) ) ;
#17335 = DIRECTION ( 'NONE',  ( -1.000000000000000000, -1.224606353822377258E-16, -0.000000000000000000 ) ) ;
#17336 = DIRECTION ( 'NONE',  ( 0.000000000000000000, 1.000000000000000000, 0.000000000000000000 ) ) ;
#17337 = DIRECTION ( 'NONE',  ( -1.000000000000000000, 3.552713678800500929E-15, 0.000000000000000000 ) ) ;
#17338 = CARTESIAN_POINT ( 'NONE',  ( 6.735557395310442615E-15, 0.000000000000000000, 55.00000000000000000 ) ) ;
#17339 = CARTESIAN_POINT ( 'NONE',  ( 43.58525529925911712, 435.7810014872755460, 17.82021598409033913 ) ) ;
#17340 = MANIFOLD_SOLID_BREP ( 'ThdSchPat', #32555 ) ;
#17341 = CARTESIAN_POINT ( 'NONE',  ( 109.3240791159541345, -30.00000000000000000, 163.9544119406666596 ) ) ;
#17342 = EDGE_CURVE ( 'NONE', #99464, #21850, #40218, .T. ) ;
#17343 = CARTESIAN_POINT ( 'NONE',  ( -106.9542266815933829, -14.21045842199434084, 174.0135369018153995 ) ) ;
#17344 = CARTESIAN_POINT ( 'NONE',  ( -59.20415057809159265, -36.01949179644289956, 68.56425315889141814 ) ) ;
#17345 = EDGE_LOOP ( 'NONE', ( #11191, #95108, #54883 ) ) ;
#17346 = CARTESIAN_POINT ( 'NONE',  ( 5.816656174490083764, 38.95337264755559659, 63.46943632529147550 ) ) ;
#17347 = CARTESIAN_POINT ( 'NONE',  ( 105.9609827248825269, -59.99999999999754863, 201.5202930408333657 ) ) ;
#17348 = AXIS2_PLACEMENT_3D ( 'NONE', #94928, #78188, #22643 ) ;
#17349 = ORIENTED_EDGE ( 'NONE', *, *, #90558, .T. ) ;
#17350 = CARTESIAN_POINT ( 'NONE',  ( 6.099794669406291447, -39.47249940446795335, 30.45861396544772859 ) ) ;
#17351 = CARTESIAN_POINT ( 'NONE',  ( -99.88241335914844399, -45.26548971045986036, 130.2270573400364242 ) ) ;
#17352 = CARTESIAN_POINT ( 'NONE',  ( 2.977408999572652260, -13.81250000204838457, 7.188101187500000044 ) ) ;
#17353 = DIRECTION ( 'NONE',  ( 0.000000000000000000, 1.000000000000000000, 0.000000000000000000 ) ) ;
#17354 = CARTESIAN_POINT ( 'NONE',  ( 34.88900972249397370, 464.6206820655982028, 18.69027339340997784 ) ) ;
#17355 = VERTEX_POINT ( 'NONE', #79081 ) ;
#17356 = CARTESIAN_POINT ( 'NONE',  ( -4.358513833876425991, -4.989164364209899283, -0.07763482564822386800 ) ) ;
#17357 = CARTESIAN_POINT ( 'NONE',  ( -30.87285025321662602, -60.00000000000000000, 43.49705760221775819 ) ) ;
#17358 = CARTESIAN_POINT ( 'NONE',  ( -3.801077171203097294, -1.110903940591820627, 104.1059035333590401 ) ) ;
#17359 = CARTESIAN_POINT ( 'NONE',  ( -7.188101187500000044, -20.28125000204838813, -8.802885111219163269E-16 ) ) ;
#17360 = FACE_BOUND ( 'NONE', #3771, .T. ) ;
#17362 = EDGE_CURVE ( 'NONE', #2115, #74776, #93686, .T. ) ;
#17361 = CARTESIAN_POINT ( 'NONE',  ( 73.33904886068935980, 4.898587196589294500E-16, -4.000000000000007105 ) ) ;
#17363 = CARTESIAN_POINT ( 'NONE',  ( 8.521464936441633498, -0.000000000000000000, -14.76977913854613789 ) ) ;
#17364 = CARTESIAN_POINT ( 'NONE',  ( 5.000000000000000000, -25.24897476799365492, -2.444053521653484662 ) ) ;
#17365 = AXIS2_PLACEMENT_3D ( 'NONE', #47991, #74269, #42439 ) ;
#17366 = DIRECTION ( 'NONE',  ( 0.000000000000000000, 0.000000000000000000, 1.000000000000000000 ) ) ;
#17367 = EDGE_CURVE ( 'NONE', #105711, #24672, #37607, .T. ) ;
#17368 = CARTESIAN_POINT ( 'NONE',  ( 82.70911704725124025, 1.016364837396684119E-14, 0.000000000000000000 ) ) ;
#17369 = CARTESIAN_POINT ( 'NONE',  ( 87.35463798683012726, -60.00000000000003553, 33.86768253245171678 ) ) ;
#17370 = CARTESIAN_POINT ( 'NONE',  ( -32.97757523807047164, -36.02761452523677832, 33.68363220189284135 ) ) ;
#17371 =( GEOMETRIC_REPRESENTATION_CONTEXT ( 3 ) GLOBAL_UNCERTAINTY_ASSIGNED_CONTEXT ( ( #75846 ) ) GLOBAL_UNIT_ASSIGNED_CONTEXT ( ( #26225, #33760, #93039 ) ) REPRESENTATION_CONTEXT ( 'NONE', 'WORKASPACE' ) );
#17372 = CARTESIAN_POINT ( 'NONE',  ( 46.33896657480098469, -49.89527275971956755, 48.28554634053408989 ) ) ;
#17373 = DIRECTION ( 'NONE',  ( -1.000000000000000000, -0.000000000000000000, -0.000000000000000000 ) ) ;
#17374 = VERTEX_POINT ( 'NONE', #94214 ) ;
#17375 = CARTESIAN_POINT ( 'NONE',  ( 42.99999999999997868, 465.8747179598608454, 15.20075430169040231 ) ) ;
#17376 = AXIS2_PLACEMENT_3D ( 'NONE', #84247, #27112, #34671 ) ;
#17377 = CARTESIAN_POINT ( 'NONE',  ( -80.00263769476747200, -38.78215726861950685, 192.9944101463111394 ) ) ;
#17378 = ORIENTED_EDGE ( 'NONE', *, *, #90686, .F. ) ;
#17380 = FILL_AREA_STYLE ('',( #18448 ) ) ;
#17379 = DIRECTION ( 'NONE',  ( 1.000000000000000000, 0.000000000000000000, 0.000000000000000000 ) ) ;
#17381 = CARTESIAN_POINT ( 'NONE',  ( 44.30795271925991585, -59.99999999999998579, 48.19995158061011153 ) ) ;
#17382 = CYLINDRICAL_SURFACE ( 'NONE', #21737, 9.999999999999994671 ) ;
#17383 = CARTESIAN_POINT ( 'NONE',  ( -43.18901105325944201, 465.6357412884333939, 10.74839809646403488 ) ) ;
#17384 = CARTESIAN_POINT ( 'NONE',  ( 11.08349330513380515, 1.593028355512270962E-15, 0.000000000000000000 ) ) ;
#17385 = LINE ( 'NONE', #19540, #89413 ) ;
#17386 = DIRECTION ( 'NONE',  ( 1.000000000000000000, -0.000000000000000000, -0.000000000000000000 ) ) ;
#17387 = CARTESIAN_POINT ( 'NONE',  ( -3.313708498984783812, -25.15625000409677270, 7.999999999999979572 ) ) ;
#17388 = CARTESIAN_POINT ( 'NONE',  ( 110.0156358204719140, -59.99999999999999289, 143.5755394574415504 ) ) ;
#17389 = DIRECTION ( 'NONE',  ( -1.000000000000000000, -1.224606353822377258E-16, -0.000000000000000000 ) ) ;
#17390 = DIRECTION ( 'NONE',  ( 0.000000000000000000, 0.000000000000000000, -1.000000000000000000 ) ) ;
#17391 = VERTEX_POINT ( 'NONE', #37069 ) ;
#17392 = CARTESIAN_POINT ( 'NONE',  ( -98.64861594025600766, -30.00000000000004619, 189.5816746752348365 ) ) ;
#17393 = VERTEX_POINT ( 'NONE', #11676 ) ;
#17394 = CARTESIAN_POINT ( 'NONE',  ( 26.78521724860346254, 36.99578157268295797, -7.587698921419404385 ) ) ;
#17395 = LINE ( 'NONE', #59449, #63214 ) ;
#17396 = CARTESIAN_POINT ( 'NONE',  ( 27.25733410137293689, 309.8297720804826554, 11.35386381468975614 ) ) ;
#17397 = CARTESIAN_POINT ( 'NONE',  ( -22.01999690012023692, 28.11337147615393306, -31.58836928537003175 ) ) ;
#17398 = CARTESIAN_POINT ( 'NONE',  ( 2.977408999572650927, -19.25000000204838813, -7.188101187500001821 ) ) ;
#17399 = AXIS2_PLACEMENT_3D ( 'NONE', #55255, #54189, #38071 ) ;
#17400 = CARTESIAN_POINT ( 'NONE',  ( 80.00000000000000000, -52.00000000000000000, -21.09707704303352926 ) ) ;
#17401 = EDGE_CURVE ( 'NONE', #75237, #101842, #81537, .T. ) ;
#17402 = CIRCLE ( 'NONE', #27825, 4.000000000000001776 ) ;
#17403 = DIRECTION ( 'NONE',  ( 1.734723475976806108E-16, -1.000000000000000000, 0.000000000000000000 ) ) ;
#17405 = ORIENTED_EDGE ( 'NONE', *, *, #96581, .F. ) ;
#17404 = FACE_OUTER_BOUND ( 'NONE', #94315, .T. ) ;
#17406 = CARTESIAN_POINT ( 'NONE',  ( 83.89049488352652872, -25.60224597872077013, 156.2394836556818518 ) ) ;
#17407 = FACE_OUTER_BOUND ( 'NONE', #76475, .T. ) ;
#17408 = VERTEX_POINT ( 'NONE', #20910 ) ;
#17409 = CARTESIAN_POINT ( 'NONE',  ( -63.05056382741410204, 50.00000000000000711, -0.01919565705159020919 ) ) ;
#17410 = CARTESIAN_POINT ( 'NONE',  ( 101.2019940638598854, 1.030564683017419500E-14, 0.000000000000000000 ) ) ;
#17411 = FACE_OUTER_BOUND ( 'NONE', #98495, .T. ) ;
#17412 = CARTESIAN_POINT ( 'NONE',  ( 21.84999999999999787, -3.309499999999999886, 0.000000000000000000 ) ) ;
#17413 = CARTESIAN_POINT ( 'NONE',  ( -4.905018583967747148, 252.0235998567968352, -3.459768807258299272 ) ) ;
#17414 = CARTESIAN_POINT ( 'NONE',  ( -31.01653611012242706, 322.5997654333527294, 14.79674070695548060 ) ) ;
#17415 =( NAMED_UNIT ( * ) PLANE_ANGLE_UNIT ( ) SI_UNIT ( $, .RADIAN. ) );
#17416 = EDGE_CURVE ( 'NONE', #39236, #2917, #103877, .T. ) ;
#17417 = ORIENTED_EDGE ( 'NONE', *, *, #27591, .T. ) ;
#17418 = CARTESIAN_POINT ( 'NONE',  ( -1.128238012697766912, 300.0000000000000000, 9.936150108905552614 ) ) ;
#17419 =( LENGTH_UNIT ( ) NAMED_UNIT ( * ) SI_UNIT ( .MILLI., .METRE. ) );
#17420 = CARTESIAN_POINT ( 'NONE',  ( 87.01900733993701920, -57.36609141436630210, 193.9082884220253220 ) ) ;
#17421 = LINE ( 'NONE', #42207, #41287 ) ;
#17422 = CARTESIAN_POINT ( 'NONE',  ( -7.188101187500000044, -33.40625000204838813, -8.802885111219163269E-16 ) ) ;
#17423 = CARTESIAN_POINT ( 'NONE',  ( 19.38947238167622089, 294.6924519132794558, -2.033477040682234893 ) ) ;
#17424 = DIRECTION ( 'NONE',  ( 0.000000000000000000, 1.000000000000000000, 0.000000000000000000 ) ) ;
#17425 = EDGE_CURVE ( 'NONE', #46183, #876, #53744, .T. ) ;
#17426 = CARTESIAN_POINT ( 'NONE',  ( 0.000000000000000000, 0.000000000000000000, -8.125150395352576993 ) ) ;
#17427 = CONTEXT_DEPENDENT_SHAPE_REPRESENTATION ( #65851, #4467 ) ;
#17428 = CARTESIAN_POINT ( 'NONE',  ( -9.797537890442935549, 33.46557797666191902, 2.014215961808868638 ) ) ;
#17429 = ORIENTED_EDGE ( 'NONE', *, *, #97770, .T. ) ;
#17430 = AXIS2_PLACEMENT_3D ( 'NONE', #70367, #103262, #29411 ) ;
#17431 =( GEOMETRIC_REPRESENTATION_CONTEXT ( 3 ) GLOBAL_UNCERTAINTY_ASSIGNED_CONTEXT ( ( #1399 ) ) GLOBAL_UNIT_ASSIGNED_CONTEXT ( ( #35187, #27106, #84774 ) ) REPRESENTATION_CONTEXT ( 'NONE', 'WORKASPACE' ) );
#17432 = DIRECTION ( 'NONE',  ( -0.5735764363510497121, 0.8191520442889892450, 1.003171929053521665E-16 ) ) ;
#17434 = CARTESIAN_POINT ( 'NONE',  ( -33.07276483573667747, 438.9325140356154975, 23.89537236861306013 ) ) ;
#17433 =( BOUNDED_SURFACE ( )  B_SPLINE_SURFACE ( 3, 2, ( 
 ( #76959, #103884, #19321 ),
 ( #3076, #37076, #54254 ),
 ( #61872, #68896, #29520 ),
 ( #79086, #101769, #5209 ),
 ( #3619, #30031, #62920 ),
 ( #52148, #94220, #60799 ) ),
 .UNSPECIFIED., .F., .F., .F. ) 
 B_SPLINE_SURFACE_WITH_KNOTS ( ( 4, 2, 4 ),
 ( 3, 3 ),
 ( 0.003190620565844217750, 0.007281897438794487573, 0.01137317431174475826 ),
 ( 0.000000000000000000, 1.000000000000000000 ),
 .UNSPECIFIED. ) 
 GEOMETRIC_REPRESENTATION_ITEM ( )  RATIONAL_B_SPLINE_SURFACE ( (
 ( 1.000000000000000000, 0.8047731410850402778, 1.000000000000000000),
 ( 1.000000000000000000, 0.8125552299160839764, 1.000000000000000000),
 ( 1.000000000000000000, 0.8191520442883742925, 1.000000000000000000),
 ( 1.000000000000000000, 0.8191520442895997567, 1.000000000000000000),
 ( 1.000000000000000000, 0.8125552299151627134, 1.000000000000000000),
 ( 1.000000000000000000, 0.8047731410850398337, 1.000000000000000000) ) ) 
 REPRESENTATION_ITEM ( '' )  SURFACE ( )  );
#17435 = VECTOR ( 'NONE', #13653, 1000.000000000000000 ) ;
#17436 = EDGE_CURVE ( 'NONE', #45973, #9363, #74622, .T. ) ;
#17437 = DIRECTION ( 'NONE',  ( -0.000000000000000000, -0.000000000000000000, 1.000000000000000000 ) ) ;
#17438 = EDGE_LOOP ( 'NONE', ( #78120, #18827, #70788, #46253, #68382 ) ) ;
#17439 = VECTOR ( 'NONE', #82962, 1000.000000000000000 ) ;
#17440 =( LENGTH_UNIT ( ) NAMED_UNIT ( * ) SI_UNIT ( .MILLI., .METRE. ) );
#17441 = LINE ( 'NONE', #1749, #94638 ) ;
#17442 = CARTESIAN_POINT ( 'NONE',  ( -43.27198366478794611, 461.7520071969213404, 3.865882560831350290 ) ) ;
#17443 = CARTESIAN_POINT ( 'NONE',  ( 110.3719848560278365, -57.66928927736454114, 195.3984882421133307 ) ) ;
#17444 =( GEOMETRIC_REPRESENTATION_CONTEXT ( 3 ) GLOBAL_UNCERTAINTY_ASSIGNED_CONTEXT ( ( #44029 ) ) GLOBAL_UNIT_ASSIGNED_CONTEXT ( ( #72237, #64166, #32335 ) ) REPRESENTATION_CONTEXT ( 'NONE', 'WORKASPACE' ) );
#17445 = EDGE_CURVE ( 'NONE', #73295, #78525, #29872, .T. ) ;
#17447 = CARTESIAN_POINT ( 'NONE',  ( 33.50694624596046367, 434.8929047988108323, 13.71597635161211848 ) ) ;
#17446 = CONICAL_SURFACE ( 'NONE', #43297, 4.250000000000000000, 0.9599310885968754814 ) ;
#17448 = DIRECTION ( 'NONE',  ( 0.000000000000000000, 0.5000000000000004441, -0.8660254037844383745 ) ) ;
#17449 = FACE_OUTER_BOUND ( 'NONE', #90083, .T. ) ;
#17450 = SURFACE_SIDE_STYLE ('',( #75654 ) ) ;
#17451 = CARTESIAN_POINT ( 'NONE',  ( -75.41928457129522201, -60.00000000000000000, 184.0178555490668373 ) ) ;
#17452 = FACE_OUTER_BOUND ( 'NONE', #37728, .T. ) ;
#17453 = CARTESIAN_POINT ( 'NONE',  ( -27.47093694407817210, 296.2799286419132727, -9.692114557243211692 ) ) ;
#17454 = CARTESIAN_POINT ( 'NONE',  ( -85.85852585477157106, -25.04863950330571143, 177.1364756427148848 ) ) ;
#17456 = EDGE_CURVE ( 'NONE', #25785, #22430, #57373, .T. ) ;
#17455 = ORIENTED_EDGE ( 'NONE', *, *, #27401, .F. ) ;
#17457 = CARTESIAN_POINT ( 'NONE',  ( 24.91130217974400196, 306.1405592189659046, -8.719263803201467766 ) ) ;
#17458 = ORIENTED_EDGE ( 'NONE', *, *, #8972, .T. ) ;
#17459 = CARTESIAN_POINT ( 'NONE',  ( 16.02741078272304875, 4.186345391437675367, 2.546409592411958744 ) ) ;
#17460 =( NAMED_UNIT ( * ) PLANE_ANGLE_UNIT ( ) SI_UNIT ( $, .RADIAN. ) );
#17461 = CARTESIAN_POINT ( 'NONE',  ( -83.10302969860578060, -37.77014383597931868, -10.04599949963776595 ) ) ;
#17462 = CONICAL_SURFACE ( 'NONE', #93211, 3.309500000000007880, 0.9599310885968770357 ) ;
#17463 = CARTESIAN_POINT ( 'NONE',  ( -4.956067050182347167, -15.30475822382919837, -6.874165724332737426 ) ) ;
#17464 = CARTESIAN_POINT ( 'NONE',  ( -15.70312386038158792, 44.04645639395336332, 4.579973510850313900 ) ) ;
#17465 = AXIS2_PLACEMENT_3D ( 'NONE', #73846, #57120, #24794 ) ;
#17466 = CARTESIAN_POINT ( 'NONE',  ( -15.81527375476383668, -3.786780092678120102, 14.52839066106889554 ) ) ;
#17467 = CARTESIAN_POINT ( 'NONE',  ( -33.21051451599209514, 465.5912171658555394, 15.87385029336180509 ) ) ;
#17468 = CARTESIAN_POINT ( 'NONE',  ( 72.41885610124130324, 42.00000000000000000, 55.65414010178505322 ) ) ;
#17469 = CARTESIAN_POINT ( 'NONE',  ( -21.97272370781284323, 27.95363515319932191, 32.15429476236987938 ) ) ;
#17470 = CARTESIAN_POINT ( 'NONE',  ( -35.41405072743933147, 437.5080630478298076, 4.889382217448016377 ) ) ;
#17471 = CARTESIAN_POINT ( 'NONE',  ( -63.50642133866089978, -59.99999999999999289, -37.13819210229684842 ) ) ;
#17472 = AXIS2_PLACEMENT_3D ( 'NONE', #5188, #87703, #34262 ) ;
#17473 = CARTESIAN_POINT ( 'NONE',  ( -70.96999627002507793, -39.48937251510619006, 105.0534544120589118 ) ) ;
#17474 = ORIENTED_EDGE ( 'NONE', *, *, #58343, .T. ) ;
#17475 = CARTESIAN_POINT ( 'NONE',  ( 63.58274112560721392, -14.21045842199431242, 93.96243211080884805 ) ) ;
#17476 = CARTESIAN_POINT ( 'NONE',  ( 18.58349330513380693, 1.593028355512270962E-15, 0.000000000000000000 ) ) ;
#17477 = CARTESIAN_POINT ( 'NONE',  ( 94.69573144448894197, -57.66415873669975412, -4.953024160301185752 ) ) ;
#17478 = EDGE_LOOP ( 'NONE', ( #67641, #35875, #77440, #55530, #68792 ) ) ;
#17479 = CARTESIAN_POINT ( 'NONE',  ( 15.19779194289341895, -6.149863736328142316, 13.69448736525634303 ) ) ;
#17480 = DIRECTION ( 'NONE',  ( -1.000000000000000000, -1.224606353822377258E-16, -0.000000000000000000 ) ) ;
#17481 = VERTEX_POINT ( 'NONE', #15933 ) ;
#17482 = FACE_OUTER_BOUND ( 'NONE', #93522, .T. ) ;
#17483 = FACE_OUTER_BOUND ( 'NONE', #102714, .T. ) ;
#17484 = CARTESIAN_POINT ( 'NONE',  ( 15.51790693666056065, 44.08177281019668925, 4.857540322262676291 ) ) ;
#17485 = CARTESIAN_POINT ( 'NONE',  ( -2.977408999572654480, -13.62500000204838457, 7.188101187499999156 ) ) ;
#17486 = PLANE ( 'NONE',  #3599 ) ;
#17487 = CARTESIAN_POINT ( 'NONE',  ( 8.127057321558247338, -4.285714285714295357, -23.93420880016849139 ) ) ;
#17488 = CARTESIAN_POINT ( 'NONE',  ( 6.575918192882433289, 3.850883087735903043, -6.669925161966314242 ) ) ;
#17489 = FACE_OUTER_BOUND ( 'NONE', #93097, .T. ) ;
#17490 = EDGE_CURVE ( 'NONE', #30746, #103131, #71453, .T. ) ;
#17491 = CARTESIAN_POINT ( 'NONE',  ( 16.33361799548379523, 1.482358050883964840E-15, 0.000000000000000000 ) ) ;
#17492 = CARTESIAN_POINT ( 'NONE',  ( 14.85284876471456350, -5.000000000000000888, 6.123233995736769241E-16 ) ) ;
#17493 = CIRCLE ( 'NONE', #27840, 4.000000000000001776 ) ;
#17494 = B_SPLINE_CURVE_WITH_KNOTS ( 'NONE', 3,
 ( #30717, #63059, #78687, #87868, #54940, #53886, #88399, #37756 ),
 .UNSPECIFIED., .F., .F.,
 ( 4, 2, 2, 4 ),
 ( 0.007886720825438791813, 0.009850969036564004647, 0.01181521724768921922, 0.01574371366993964488 ),
 .UNSPECIFIED. ) ;
#17495 = ORIENTED_EDGE ( 'NONE', *, *, #50787, .T. ) ;
#17496 = CARTESIAN_POINT ( 'NONE',  ( -7.354129747669107431, 40.93126392605007879, -70.29718773507885032 ) ) ;
#17498 = CARTESIAN_POINT ( 'NONE',  ( 32.84200068835146880, -56.84013278135907399, 37.45145004404182032 ) ) ;
#17497 = CARTESIAN_POINT ( 'NONE',  ( -4.195612334301150881, -48.94124001270379409, 104.4881327927213448 ) ) ;
#17499 = CARTESIAN_POINT ( 'NONE',  ( -4.278756001540764409, 52.15505427271036609, -6.541747321572864315 ) ) ;
#17500 = EDGE_CURVE ( 'NONE', #84731, #20623, #89304, .T. ) ;
#17501 = ORIENTED_EDGE ( 'NONE', *, *, #32460, .F. ) ;
#17502 = CARTESIAN_POINT ( 'NONE',  ( 9.797174393178825657E-16, -15.00000000000000000, 8.000000000000000000 ) ) ;
#17503 = ORIENTED_EDGE ( 'NONE', *, *, #68160, .T. ) ;
#17504 = LINE ( 'NONE', #8320, #65806 ) ;
#17505 = CARTESIAN_POINT ( 'NONE',  ( 4.377363093174522650E-05, -49.99999999999997868, 32.22298329293570873 ) ) ;
#17506 = DIRECTION ( 'NONE',  ( 0.000000000000000000, -1.000000000000000000, 0.000000000000000000 ) ) ;
#17507 = EDGE_CURVE ( 'NONE', #14406, #7125, #28182, .T. ) ;
#17508 = CARTESIAN_POINT ( 'NONE',  ( 1.101584607545897043, 45.52388203129090982, 18.11230536840457361 ) ) ;
#17509 = CARTESIAN_POINT ( 'NONE',  ( 1.251018392637836651, 15.60415866083139136, -50.60639602862229935 ) ) ;
#17510 = VERTEX_POINT ( 'NONE', #65017 ) ;
#17511 = CARTESIAN_POINT ( 'NONE',  ( 92.70420653547968470, -60.00000000000001421, -9.023355465272066667 ) ) ;
#17512 = VECTOR ( 'NONE', #25424, 1000.000000000000000 ) ;
#17513 = AXIS2_PLACEMENT_3D ( 'NONE', #9548, #75348, #51066 ) ;
#17514 = PRESENTATION_LAYER_ASSIGNMENT (  '', '', ( #93335 ) ) ;
#17515 = CARTESIAN_POINT ( 'NONE',  ( -47.03591514779362370, 18.70176887044695846, -14.84266952052386124 ) ) ;
#17516 = ORIENTED_EDGE ( 'NONE', *, *, #31994, .T. ) ;
#17517 = EDGE_CURVE ( 'NONE', #32589, #96921, #78172, .T. ) ;
#17518 = DIRECTION ( 'NONE',  ( 1.000000000000000000, 1.224606353822377258E-16, 0.000000000000000000 ) ) ;
#17519 = ORIENTED_EDGE ( 'NONE', *, *, #9553, .T. ) ;
#17520 = ORIENTED_EDGE ( 'NONE', *, *, #38184, .T. ) ;
#17521 = CARTESIAN_POINT ( 'NONE',  ( 7.045965687440314262, 83.69607536213965204, 3.790395326974318913 ) ) ;
#17522 = DIRECTION ( 'NONE',  ( 0.05555555555555524022, 0.000000000000000000, 0.9984555975339683975 ) ) ;
#17523 = DIRECTION ( 'NONE',  ( 0.5735764363510491570, -0.8191520442889895781, 1.003171929053522035E-16 ) ) ;
#17524 = CARTESIAN_POINT ( 'NONE',  ( 87.03145172370204818, -60.20135443965438071, -7.696256136449998841 ) ) ;
#17525 = CARTESIAN_POINT ( 'NONE',  ( -30.58328632870184549, 308.7181655071192949, -8.654209201893030112 ) ) ;
#17526 = DIRECTION ( 'NONE',  ( 0.000000000000000000, -1.000000000000000000, 0.000000000000000000 ) ) ;
#17527 = CARTESIAN_POINT ( 'NONE',  ( 12.50000000000000000, 35.04556876861937553, -54.45246410008698490 ) ) ;
#17528 = MANIFOLD_SOLID_BREP ( 'ThdSchPat', #4966 ) ;
#17529 = ORIENTED_EDGE ( 'NONE', *, *, #16638, .T. ) ;
#17530 = DIRECTION ( 'NONE',  ( 0.000000000000000000, 0.000000000000000000, 1.000000000000000000 ) ) ;
#17531 = VECTOR ( 'NONE', #78552, 1000.000000000000000 ) ;
#17532 = VERTEX_POINT ( 'NONE', #22475 ) ;
#17533 = EDGE_CURVE ( 'NONE', #96921, #32589, #50584, .T. ) ;
#17534 = CARTESIAN_POINT ( 'NONE',  ( -4.852941176470598528, -3.000000000000002665, -70.80672828634229177 ) ) ;
#17535 = CARTESIAN_POINT ( 'NONE',  ( 38.99314007804239424, 463.6591011809805991, 19.41136731754987821 ) ) ;
#17537 = ORIENTED_EDGE ( 'NONE', *, *, #14937, .F. ) ;
#17536 = CARTESIAN_POINT ( 'NONE',  ( 6.399925260777681757, 51.30561996063480024, 7.879653260259286363 ) ) ;
#17538 = CARTESIAN_POINT ( 'NONE',  ( 76.34208424054833131, -46.43307427196572235, 131.9837883314934572 ) ) ;
#17539 = VERTEX_POINT ( 'NONE', #1312 ) ;
#17540 = SURFACE_STYLE_USAGE ( .BOTH. , #40729 ) ;
#17541 = CARTESIAN_POINT ( 'NONE',  ( -5.082755093536325042, -26.09375000204838813, -5.082755093536325930 ) ) ;
#17542 = CARTESIAN_POINT ( 'NONE',  ( -93.33808876947477984, -57.65441397348698160, -16.37300446327261128 ) ) ;
#17543 = EDGE_CURVE ( 'NONE', #60305, #27490, #17920, .T. ) ;
#17544 = EDGE_CURVE ( 'NONE', #106075, #62805, #34274, .T. ) ;
#17545 = VERTEX_POINT ( 'NONE', #74684 ) ;
#17546 = AXIS2_PLACEMENT_3D ( 'NONE', #88442, #24259, #40938 ) ;
#17547 =( NAMED_UNIT ( * ) SI_UNIT ( $, .STERADIAN. ) SOLID_ANGLE_UNIT ( ) );
#17548 = CARTESIAN_POINT ( 'NONE',  ( -43.00000000000000000, 450.0000000000002274, 13.20242257375370976 ) ) ;
#17549 = CARTESIAN_POINT ( 'NONE',  ( 106.2885998856441745, -60.15149245731204530, 179.7510284545313937 ) ) ;
#17550 = CARTESIAN_POINT ( 'NONE',  ( -36.08160016962256833, 491.3801102092016890, 12.28496641015634872 ) ) ;
#17551 =( GEOMETRIC_REPRESENTATION_CONTEXT ( 3 ) GLOBAL_UNCERTAINTY_ASSIGNED_CONTEXT ( ( #97938 ) ) GLOBAL_UNIT_ASSIGNED_CONTEXT ( ( #4038, #14230, #4570 ) ) REPRESENTATION_CONTEXT ( 'NONE', 'WORKASPACE' ) );
#17552 = CARTESIAN_POINT ( 'NONE',  ( 100.0424503805845831, 1.016364837396684119E-14, 0.000000000000000000 ) ) ;
#17553 = CARTESIAN_POINT ( 'NONE',  ( -5.656854249492379694, -24.12500000409677270, -5.656854249492380582 ) ) ;
#17554 = CARTESIAN_POINT ( 'NONE',  ( 12.33349330513380693, 4.000000000000003553, 0.000000000000000000 ) ) ;
#17555 = CARTESIAN_POINT ( 'NONE',  ( -36.36519827644053038, 25.99686924827267731, 12.56069422975649630 ) ) ;
#17556 = LINE ( 'NONE', #75772, #98204 ) ;
#17557 = DIRECTION ( 'NONE',  ( 0.000000000000000000, -1.000000000000000000, 0.000000000000000000 ) ) ;
#17558 = CARTESIAN_POINT ( 'NONE',  ( 7.412906595240166041, -7.358117271477464527, 3.014362223629233561 ) ) ;
#17559 = DIRECTION ( 'NONE',  ( 1.000000000000000000, 6.989781874810890086E-17, -5.620325286447034103E-17 ) ) ;
#17560 = DIRECTION ( 'NONE',  ( 0.000000000000000000, -1.000000000000000000, 0.000000000000000000 ) ) ;
#17561 = ORIENTED_EDGE ( 'NONE', *, *, #104872, .F. ) ;
#17562 = CARTESIAN_POINT ( 'NONE',  ( 35.90484354297773706, 1.340359594676612611E-15, 0.000000000000000000 ) ) ;
#17563 = CARTESIAN_POINT ( 'NONE',  ( 12.82717339738770512, -60.00000000000000000, 39.70944106662322781 ) ) ;
#17564 = CARTESIAN_POINT ( 'NONE',  ( -88.45143479841831891, -29.99999999999999645, 187.7855393631011225 ) ) ;
#17565 = EDGE_CURVE ( 'NONE', #35775, #25464, #42865, .T. ) ;
#17566 = EDGE_LOOP ( 'NONE', ( #21990, #10550, #18968, #36637, #31902 ) ) ;
#17567 = VERTEX_POINT ( 'NONE', #58530 ) ;
#17568 = CARTESIAN_POINT ( 'NONE',  ( 38.54716475372293871, 25.36783991978645147, -11.41422472833605006 ) ) ;
#17569 = CARTESIAN_POINT ( 'NONE',  ( 70.40948563225279599, -57.68249254348480548, 157.3593782098396900 ) ) ;
#17571 = CARTESIAN_POINT ( 'NONE',  ( -9.749942471036476377, 53.39674074574894291, 3.171770270685806636 ) ) ;
#17570 = DIRECTION ( 'NONE',  ( -0.000000000000000000, -0.000000000000000000, -1.000000000000000000 ) ) ;
#17572 = EDGE_CURVE ( 'NONE', #43166, #59552, #57309, .T. ) ;
#17573 = CARTESIAN_POINT ( 'NONE',  ( 14.58136264770422130, -23.94594737508124993, -38.53227127598449187 ) ) ;
#17574 = DIRECTION ( 'NONE',  ( -1.000000000000000000, -0.000000000000000000, -0.000000000000000000 ) ) ;
#17575 = CARTESIAN_POINT ( 'NONE',  ( -46.72192845272360273, -59.99999999999999289, 64.17803650344802691 ) ) ;
#17576 = CARTESIAN_POINT ( 'NONE',  ( 13.69330508143927538, -5.000000000000000000, 0.000000000000000000 ) ) ;
#17577 = CARTESIAN_POINT ( 'NONE',  ( 35.69355135759132480, 463.3819780847712195, 19.97922827668278245 ) ) ;
#17578 = CARTESIAN_POINT ( 'NONE',  ( -86.05365282663042592, -39.21241181629545736, 187.0849633868903084 ) ) ;
#17580 = EDGE_CURVE ( 'NONE', #63495, #15128, #4131, .T. ) ;
#17579 = AXIS2_PLACEMENT_3D ( 'NONE', #35475, #24467, #106385 ) ;
#17581 = VERTEX_POINT ( 'NONE', #67149 ) ;
#17582 = LINE ( 'NONE', #8402, #71146 ) ;
#17583 = CARTESIAN_POINT ( 'NONE',  ( -10.08550511080940915, -22.06801976977802227, 27.57672000808223700 ) ) ;
#17584 = CARTESIAN_POINT ( 'NONE',  ( -6.831363903021533623, 41.73171925724633979, -59.17722475679354233 ) ) ;
#17585 = AXIS2_PLACEMENT_3D ( 'NONE', #16879, #42737, #98828 ) ;
#17586 = CARTESIAN_POINT ( 'NONE',  ( -37.48079203514996038, 473.0293823827626056, 17.43706145210287062 ) ) ;
#17588 = CARTESIAN_POINT ( 'NONE',  ( 3.908772774635062230, -67.68245115326362793, 13.12901559851279387 ) ) ;
#17587 = DIRECTION ( 'NONE',  ( 0.000000000000000000, -1.000000000000000000, 0.000000000000000000 ) ) ;
#17589 = EDGE_LOOP ( 'NONE', ( #94029, #69736 ) ) ;
#17590 = CARTESIAN_POINT ( 'NONE',  ( 26.49164619350623440, 34.70556741407747126, 9.907652308642946437 ) ) ;
#17591 = LINE ( 'NONE', #41841, #27051 ) ;
#17592 = CARTESIAN_POINT ( 'NONE',  ( -7.896571385775229324, 33.78997999345754266, 1.305932416347437952 ) ) ;
#17593 = CARTESIAN_POINT ( 'NONE',  ( 30.93562973191455612, 298.0458768196136248, -9.298557881189427832 ) ) ;
#17594 = DIRECTION ( 'NONE',  ( -0.000000000000000000, -1.000000000000000000, -0.000000000000000000 ) ) ;
#17595 = CONICAL_SURFACE ( 'NONE', #14092, 3.309500000000001663, 0.9599310885968770357 ) ;
#17596 = DIRECTION ( 'NONE',  ( 0.000000000000000000, 0.000000000000000000, 1.000000000000000000 ) ) ;
#17597 = CARTESIAN_POINT ( 'NONE',  ( 0.000000000000000000, 0.000000000000000000, 0.000000000000000000 ) ) ;
#17598 = CARTESIAN_POINT ( 'NONE',  ( 109.3240791159541345, -30.00000000000000000, 163.9544119406666596 ) ) ;
#17599 = CARTESIAN_POINT ( 'NONE',  ( -83.92326679681109169, -29.05553059583932907, 161.8043818697931897 ) ) ;
#17600 = EDGE_LOOP ( 'NONE', ( #69826, #70623 ) ) ;
#17601 = CARTESIAN_POINT ( 'NONE',  ( 74.56127108291157413, 6.975173280561618775E-15, 0.000000000000000000 ) ) ;
#17602 = CARTESIAN_POINT ( 'NONE',  ( -9.253800200985708102, 251.3001033108817523, -3.791983798715478304 ) ) ;
#17603 = CARTESIAN_POINT ( 'NONE',  ( -5.047120108843201614, 5.746297884371388776, -0.1007566405101762153 ) ) ;
#17604 = CARTESIAN_POINT ( 'NONE',  ( 37.64398511886353305, 375.6922506333542060, 4.851078712600862985 ) ) ;
#17605 = CARTESIAN_POINT ( 'NONE',  ( 6.289812543865804351, -5.581224740283311725, 3.991031161979334385 ) ) ;
#17606 = ORIENTED_EDGE ( 'NONE', *, *, #5276, .F. ) ;
#17607 = CARTESIAN_POINT ( 'NONE',  ( -8.000000000000001776, -22.15624999999999645, 3.313708498984759387 ) ) ;
#17608 = EDGE_LOOP ( 'NONE', ( #78479, #739, #32811, #57935, #53089, #101735, #10317 ) ) ;
#17609 = CARTESIAN_POINT ( 'NONE',  ( 34.28461378013923166, 484.9851079380702572, 0.1119777429318196682 ) ) ;
#17610 = CARTESIAN_POINT ( 'NONE',  ( 3.836411046841927686, 15.00000000000001066, 9.999999999999959144 ) ) ;
#17611 = CARTESIAN_POINT ( 'NONE',  ( 37.29743259733411520, 437.4067882691435898, 4.451017177258780322 ) ) ;
#17612 = EDGE_CURVE ( 'NONE', #16558, #45991, #34815, .T. ) ;
#17613 =( NAMED_UNIT ( * ) SI_UNIT ( $, .STERADIAN. ) SOLID_ANGLE_UNIT ( ) );
#17614 = DIRECTION ( 'NONE',  ( -1.000000000000000000, -1.224606353822377258E-16, -0.000000000000000000 ) ) ;
#17615 = CIRCLE ( 'NONE', #41696, 4.000000000000007105 ) ;
#17616 = CARTESIAN_POINT ( 'NONE',  ( 0.000000000000000000, 23.58303312036771615, 0.000000000000000000 ) ) ;
#17617 = ORIENTED_EDGE ( 'NONE', *, *, #2098, .T. ) ;
#17618 = CARTESIAN_POINT ( 'NONE',  ( 96.95221799863543310, -60.00000000000002132, 202.4789020112573610 ) ) ;
#17619 = AXIS2_PLACEMENT_3D ( 'NONE', #27213, #53574, #94032 ) ;
#17621 = CARTESIAN_POINT ( 'NONE',  ( 14.50450630449079092, -35.99182772622528859, 30.00711302977329709 ) ) ;
#17620 = CARTESIAN_POINT ( 'NONE',  ( -98.15060533238310825, -14.21045842199422715, 197.6136055373540614 ) ) ;
#17622 = UNCERTAINTY_MEASURE_WITH_UNIT (LENGTH_MEASURE( 1.000000000000000082E-05 ), #94362, 'distance_accuracy_value', 'NONE');
#17624 = ADVANCED_FACE ( 'NONE', ( #59598, #92472 ), #18078, .F. ) ;
#17623 = CARTESIAN_POINT ( 'NONE',  ( 0.08413355536092814724, 53.39766064372320642, -10.25000000000000000 ) ) ;
#17625 = CARTESIAN_POINT ( 'NONE',  ( -42.47994433708600326, -49.89231707659487824, 43.43423702368624362 ) ) ;
#17626 = AXIS2_PLACEMENT_3D ( 'NONE', #86968, #11986, #4432 ) ;
#17627 = CARTESIAN_POINT ( 'NONE',  ( 34.83349330513379982, -4.000000000000000888, 4.898587196589416773E-16 ) ) ;
#17628 = ORIENTED_EDGE ( 'NONE', *, *, #13178, .F. ) ;
#17629 = FACE_OUTER_BOUND ( 'NONE', #13855, .T. ) ;
#17630 = CARTESIAN_POINT ( 'NONE',  ( -43.04469050570867239, 434.7734435962895532, 9.248231035232468145 ) ) ;
#17631 = CARTESIAN_POINT ( 'NONE',  ( 30.12932728364529922, 334.4140447340107585, 17.11298374841474867 ) ) ;
#17632 = CIRCLE ( 'NONE', #84828, 5.000000000000000888 ) ;
#17633 = PRESENTATION_STYLE_ASSIGNMENT (( #18166 ) ) ;
#17634 = CARTESIAN_POINT ( 'NONE',  ( 6.222742520105470021, 3.584500230190543313, 6.791463481567635796 ) ) ;
#17635 = CARTESIAN_POINT ( 'NONE',  ( -29.99999999996959588, 488.4085301725142472, 8.313477165056513130 ) ) ;
#17636 = VERTEX_POINT ( 'NONE', #33732 ) ;
#17637 = CARTESIAN_POINT ( 'NONE',  ( -15.93287854420827721, 36.64197083639891872, -24.00465449142953744 ) ) ;
#17638 = ORIENTED_EDGE ( 'NONE', *, *, #17533, .F. ) ;
#17639 = CARTESIAN_POINT ( 'NONE',  ( 69.85629772084516276, -29.99999999999997868, 125.7656138327989481 ) ) ;
#17640 = CARTESIAN_POINT ( 'NONE',  ( 47.44481056709881273, 11.19259812317959124, 16.71748578406432273 ) ) ;
#17641 = LINE ( 'NONE', #99591, #11717 ) ;
#17642 = CARTESIAN_POINT ( 'NONE',  ( 6.874999999999998224, 4.690970937165705124, -7.298562697733106397 ) ) ;
#17643 = CARTESIAN_POINT ( 'NONE',  ( 80.91584140846381956, -30.00000000000000000, 5.600791395715724263 ) ) ;
#17644 = DIRECTION ( 'NONE',  ( 0.9861333108788017388, 0.1659550938513567886, 0.000000000000000000 ) ) ;
#17645 = ORIENTED_EDGE ( 'NONE', *, *, #10670, .T. ) ;
#17646 = EDGE_CURVE ( 'NONE', #92260, #103853, #49348, .T. ) ;
#17647 = EDGE_LOOP ( 'NONE', ( #50301, #13111, #91000, #33393 ) ) ;
#17648 = ORIENTED_EDGE ( 'NONE', *, *, #8900, .F. ) ;
#17649 = CARTESIAN_POINT ( 'NONE',  ( -47.78242936231056603, 10.33916499670815270, -16.83675847388958147 ) ) ;
#17650 = LINE ( 'NONE', #83426, #99285 ) ;
#17651 = CARTESIAN_POINT ( 'NONE',  ( 4.497472161260650303, -10.54222546625947388, -3.972129482042464410 ) ) ;
#17652 = CARTESIAN_POINT ( 'NONE',  ( -32.13233948541094520, 428.0625681181319919, 24.77049652713832728 ) ) ;
#17653 = VERTEX_POINT ( 'NONE', #74157 ) ;
#17654 = VERTEX_POINT ( 'NONE', #67682 ) ;
#17655 = DIRECTION ( 'NONE',  ( -1.000000000000000000, -1.224606353822377258E-16, -0.000000000000000000 ) ) ;
#17656 = CARTESIAN_POINT ( 'NONE',  ( 74.78018824853795365, -38.33359745921677586, 167.4195336213977328 ) ) ;
#17657 = DIRECTION ( 'NONE',  ( 0.000000000000000000, -1.000000000000000000, 0.000000000000000000 ) ) ;
#17658 = CARTESIAN_POINT ( 'NONE',  ( 26.18291261871826237, 305.7871056458065482, 10.60176253965241777 ) ) ;
#17659 = CARTESIAN_POINT ( 'NONE',  ( -5.725004243152317152, 246.4248085174462801, -1.812899781754681472 ) ) ;
#17660 = ORIENTED_EDGE ( 'NONE', *, *, #6606, .F. ) ;
#17661 = LINE ( 'NONE', #40855, #59595 ) ;
#17662 = AXIS2_PLACEMENT_3D ( 'NONE', #57071, #66779, #399 ) ;
#17663 = CARTESIAN_POINT ( 'NONE',  ( 28.69273362649255077, 297.1307134239958714, 2.434641731654969110 ) ) ;
#17664 = CARTESIAN_POINT ( 'NONE',  ( -29.00000000000000355, 0.000000000000000000, 0.000000000000000000 ) ) ;
#17665 = ORIENTED_EDGE ( 'NONE', *, *, #58972, .T. ) ;
#17667 = CARTESIAN_POINT ( 'NONE',  ( -24.44168859681608907, 295.5650463862446600, 10.09009199608876983 ) ) ;
#17666 =( NAMED_UNIT ( * ) SI_UNIT ( $, .STERADIAN. ) SOLID_ANGLE_UNIT ( ) );
#17668 = DIRECTION ( 'NONE',  ( 0.000000000000000000, -1.000000000000000000, 0.000000000000000000 ) ) ;
#17669 = DIRECTION ( 'NONE',  ( 1.000000000000000000, -0.000000000000000000, 1.224646799147353207E-16 ) ) ;
#17670 = FACE_OUTER_BOUND ( 'NONE', #96617, .T. ) ;
#17671 = LINE ( 'NONE', #52144, #34782 ) ;
#17672 = COLOUR_RGB ( '', 0.40784314, 0.44705882, 0.49803922) ;
#17673 = CARTESIAN_POINT ( 'NONE',  ( -7.212994264445060644, 102.9828865565996097, 3.463766307298588032 ) ) ;
#17674 = VERTEX_POINT ( 'NONE', #101105 ) ;
#17675 = CARTESIAN_POINT ( 'NONE',  ( 60.14984002819952025, 6.856755485862130937E-15, 0.000000000000000000 ) ) ;
#17676 = APPLICATION_CONTEXT ( 'automotive_design' ) ;
#17677 = CARTESIAN_POINT ( 'NONE',  ( 84.08575072203289835, -61.04859098016596874, 192.4284686294917321 ) ) ;
#17678 = CARTESIAN_POINT ( 'NONE',  ( 17.94999111897404731, 36.38767359518976718, -23.42285042635058900 ) ) ;
#17679 = ORIENTED_EDGE ( 'NONE', *, *, #15564, .F. ) ;
#17680 = CARTESIAN_POINT ( 'NONE',  ( 83.51201917109111150, -57.67104594142430329, -28.06691757407987708 ) ) ;
#17681 = CYLINDRICAL_SURFACE ( 'NONE', #55572, 5.000000000000000888 ) ;
#17682 = CARTESIAN_POINT ( 'NONE',  ( 0.000000000000000000, 6.123233995736767268E-16, -5.000000000000000888 ) ) ;
#17683 = DIRECTION ( 'NONE',  ( 0.000000000000000000, 0.000000000000000000, 1.000000000000000000 ) ) ;
#17684 = COLOUR_RGB ( '', 0.66274510, 0.83137255, 0.94901961) ;
#17685 = CARTESIAN_POINT ( 'NONE',  ( -80.78186281600028451, -30.00000000000000000, 9.678833486316271717 ) ) ;
#17686 = EDGE_CURVE ( 'NONE', #56853, #71627, #60946, .T. ) ;
#17687 = EDGE_CURVE ( 'NONE', #58935, #16697, #93448, .T. ) ;
#17688 = CYLINDRICAL_SURFACE ( 'NONE', #12407, 8.000000000000000000 ) ;
#17689 = DIRECTION ( 'NONE',  ( 0.000000000000000000, -1.000000000000000000, 0.000000000000000000 ) ) ;
#17690 = CARTESIAN_POINT ( 'NONE',  ( 98.59800593614012598, 6.123233995736582872E-16, -5.000000000000011546 ) ) ;
#17692 = DIRECTION ( 'NONE',  ( 0.000000000000000000, 0.000000000000000000, 1.000000000000000000 ) ) ;
#17691 = CARTESIAN_POINT ( 'NONE',  ( -7.922281120364393914, -4.573931137438282057, -8.047472243342934206 ) ) ;
#17693 = EDGE_CURVE ( 'NONE', #47749, #96624, #82795, .T. ) ;
#17694 = CARTESIAN_POINT ( 'NONE',  ( -17.49999999999997868, 49.03511921915654170, 64.04809060635940909 ) ) ;
#17695 = CARTESIAN_POINT ( 'NONE',  ( -28.71513376685318164, 15.67191133428136673, 41.65496614056284841 ) ) ;
#17696 = DIRECTION ( 'NONE',  ( -1.000000000000000000, -0.000000000000000000, -0.000000000000000000 ) ) ;
#17697 = DIRECTION ( 'NONE',  ( 0.000000000000000000, -1.000000000000000000, 0.000000000000000000 ) ) ;
#17698 = CYLINDRICAL_SURFACE ( 'NONE', #88884, 5.000000000000000888 ) ;
#17699 = CARTESIAN_POINT ( 'NONE',  ( 41.44325323473465517, 477.1522009800042952, -1.085119017178377554 ) ) ;
#17700 =( GEOMETRIC_REPRESENTATION_CONTEXT ( 3 ) GLOBAL_UNCERTAINTY_ASSIGNED_CONTEXT ( ( #20058 ) ) GLOBAL_UNIT_ASSIGNED_CONTEXT ( ( #69265, #5564, #28291 ) ) REPRESENTATION_CONTEXT ( 'NONE', 'WORKASPACE' ) );
#17701 = CARTESIAN_POINT ( 'NONE',  ( 26.36650669486618881, 1.474610560812782335E-15, 0.000000000000000000 ) ) ;
#17702 = EDGE_CURVE ( 'NONE', #59703, #66543, #105732, .T. ) ;
#17703 = EDGE_LOOP ( 'NONE', ( #70524, #54562, #90879, #19165, #94118, #99473 ) ) ;
#17704 = CARTESIAN_POINT ( 'NONE',  ( 6.585468679846623097, -7.640532685286896886, 0.2337908078075559004 ) ) ;
#17705 = SURFACE_STYLE_USAGE ( .BOTH. , #66235 ) ;
#17706 = CARTESIAN_POINT ( 'NONE',  ( -6.944371705245973914, 84.46100308575449844, -3.972324460300559856 ) ) ;
#17707 = CARTESIAN_POINT ( 'NONE',  ( -38.88645629453070285, -24.53144980621419080, -30.52333081557608097 ) ) ;
#17709 = CARTESIAN_POINT ( 'NONE',  ( -71.72561805443079663, -34.58960680145646194, -21.02611375570996444 ) ) ;
#17708 = DIRECTION ( 'NONE',  ( 0.000000000000000000, 1.000000000000000000, 0.000000000000000000 ) ) ;
#17710 = EDGE_LOOP ( 'NONE', ( #60220, #1962, #545, #45402, #90755, #50711 ) ) ;
#17711 = CARTESIAN_POINT ( 'NONE',  ( -14.91271302809441401, 41.98564543112699710, -86.62215342991694911 ) ) ;
#17712 = ORIENTED_EDGE ( 'NONE', *, *, #69849, .F. ) ;
#17713 = FACE_OUTER_BOUND ( 'NONE', #30618, .T. ) ;
#17714 = CARTESIAN_POINT ( 'NONE',  ( 16.04721880643842979, 4.604982429971628655, 3.436919038180027641 ) ) ;
#17715 = CARTESIAN_POINT ( 'NONE',  ( -63.73407763263179504, -60.00000000000000711, -34.61716371171238649 ) ) ;
#17716 = VERTEX_POINT ( 'NONE', #43407 ) ;
#17717 = DIRECTION ( 'NONE',  ( -1.000000000000000000, -1.224606353822377258E-16, -0.000000000000000000 ) ) ;
#17718 = CARTESIAN_POINT ( 'NONE',  ( 15.30754850745360862, 3.114812942699181075, -3.172027124395669695 ) ) ;
#17719 = CARTESIAN_POINT ( 'NONE',  ( 102.1330484602042787, -60.20162503959858213, 194.0437069272821873 ) ) ;
#17720 = AXIS2_PLACEMENT_3D ( 'NONE', #92684, #51685, #84605 ) ;
#17722 = CARTESIAN_POINT ( 'NONE',  ( -47.24160628166287523, 11.75468494072141112, 16.58444347056430956 ) ) ;
#17721 = CARTESIAN_POINT ( 'NONE',  ( 5.862635191369047760, 294.7602340196642103, -8.121464904941849028 ) ) ;
#17723 = EDGE_LOOP ( 'NONE', ( #13149, #24165, #59547, #43121 ) ) ;
#17724 = B_SPLINE_CURVE_WITH_KNOTS ( 'NONE', 3,
 ( #85463, #35347, #68210, #101107, #11548, #27267, #60151, #6113, #54121, #20244, #12086, #95672, #47102, #45018, #62784, #77899, #104824, #53093, #28866, #4008, #80004, #45543, #78416, #38517, #21813, #5072, #38005, #63321, #86015, #36939, #69805, #13137, #54653, #12606 ),
 .UNSPECIFIED., .F., .F.,
 ( 4, 2, 2, 2, 2, 2, 2, 2, 2, 2, 2, 2, 2, 2, 2, 2, 4 ),
 ( 0.01263889472610568374, 0.01342810546992895954, 0.01421731621375223360, 0.01500652695757550940, 0.01579573770139878347, 0.01658494844522205927, 0.01737415918904533507, 0.01816336993286861087, 0.01895258067669188667, 0.01974179142051516248, 0.02053100216433843828, 0.02132021290816171408, 0.02210942365198498988, 0.02289863439580826915, 0.02368784513963154148, 0.02447705588345482075, 0.02526626662727809655 ),
 .UNSPECIFIED. ) ;
#17725 = AXIS2_PLACEMENT_3D ( 'NONE', #41939, #65692, #58672 ) ;
#17726 = ORIENTED_EDGE ( 'NONE', *, *, #9891, .T. ) ;
#17727 = VECTOR ( 'NONE', #71539, 1000.000000000000000 ) ;
#17728 = EDGE_LOOP ( 'NONE', ( #62051, #91091, #53396, #7396 ) ) ;
#17729 = CARTESIAN_POINT ( 'NONE',  ( 28.62319560939385710, 318.3944600039412194, 12.26906456063335149 ) ) ;
#17730 = CARTESIAN_POINT ( 'NONE',  ( -3.313708498984783812, -27.96874999999999645, 7.999999999999979572 ) ) ;
#17731 = DIRECTION ( 'NONE',  ( -1.000000000000000000, 0.000000000000000000, 0.000000000000000000 ) ) ;
#17732 = ORIENTED_EDGE ( 'NONE', *, *, #31054, .T. ) ;
#17733 = EDGE_CURVE ( 'NONE', #97465, #26579, #25265, .T. ) ;
#17734 = DIRECTION ( 'NONE',  ( -1.000000000000000000, -0.000000000000000000, -0.000000000000000000 ) ) ;
#17735 = CARTESIAN_POINT ( 'NONE',  ( 6.463344223170841119, 7.245769408789096921, 1.129975644293424786 ) ) ;
#17736 = CARTESIAN_POINT ( 'NONE',  ( 32.09911992168216699, 438.9232547152094526, 23.66653216045977359 ) ) ;
#17737 = CARTESIAN_POINT ( 'NONE',  ( -71.68202686650683120, -57.67896093159416893, 168.8233993379761557 ) ) ;
#17738 = CARTESIAN_POINT ( 'NONE',  ( 5.082755093536324154, -31.34375000204838457, 5.082755093536326818 ) ) ;
#17739 = CARTESIAN_POINT ( 'NONE',  ( -29.85155995213069247, 18.03343143632516643, 39.61445771744197231 ) ) ;
#17740 = CARTESIAN_POINT ( 'NONE',  ( -0.4000000000000045186, 0.000000000000000000, 8.500000000000000000 ) ) ;
#17741 = CARTESIAN_POINT ( 'NONE',  ( -6.690415133250795954, 41.73276121203647904, -59.04972748448755482 ) ) ;
#17742 =( GEOMETRIC_REPRESENTATION_CONTEXT ( 3 ) GLOBAL_UNCERTAINTY_ASSIGNED_CONTEXT ( ( #26675 ) ) GLOBAL_UNIT_ASSIGNED_CONTEXT ( ( #58357, #57272, #9788 ) ) REPRESENTATION_CONTEXT ( 'NONE', 'WORKASPACE' ) );
#17743 = CARTESIAN_POINT ( 'NONE',  ( -87.60281504538382080, -14.21045842199439946, -3.799590761493521374 ) ) ;
#17744 = EDGE_CURVE ( 'NONE', #45380, #54954, #76289, .T. ) ;
#17746 = EDGE_CURVE ( 'NONE', #7616, #20102, #82253, .T. ) ;
#17745 = CARTESIAN_POINT ( 'NONE',  ( -43.51084452654468748, 465.2903130129675446, 9.421687747985348693 ) ) ;
#17747 = CARTESIAN_POINT ( 'NONE',  ( -49.98625063665457446, -18.73833733594818085, 43.94435920909415927 ) ) ;
#17748 = CARTESIAN_POINT ( 'NONE',  ( 4.898587196589412829E-16, -25.62499999999999645, -8.000000000000000000 ) ) ;
#17749 = ORIENTED_EDGE ( 'NONE', *, *, #34723, .T. ) ;
#17750 = CARTESIAN_POINT ( 'NONE',  ( 12.50000000000000355, 16.77477425093740848, -34.50590399936646691 ) ) ;
#17751 = CARTESIAN_POINT ( 'NONE',  ( -7.196962703048771282, 302.2659962052633773, -10.02664813804980959 ) ) ;
#17752 = LINE ( 'NONE', #83525, #45158 ) ;
#17753 = ORIENTED_EDGE ( 'NONE', *, *, #89247, .T. ) ;
#17754 = CARTESIAN_POINT ( 'NONE',  ( 0.000000000000000000, 0.000000000000000000, -9.078441367943003826 ) ) ;
#17755 = CARTESIAN_POINT ( 'NONE',  ( 84.77133682389549563, -38.71704634458406957, 198.3318700654770339 ) ) ;
#17756 = SURFACE_SIDE_STYLE ('',( #93231 ) ) ;
#17757 = CARTESIAN_POINT ( 'NONE',  ( -6.133251129394694523, 51.27079673972909291, -8.207848847617324139 ) ) ;
#17758 = DIRECTION ( 'NONE',  ( -0.5735764363510494901, -0.8191520442889894671, 0.000000000000000000 ) ) ;
#17759 = CARTESIAN_POINT ( 'NONE',  ( -41.66301127302556750, 485.3863426732056041, -3.409513628938169116 ) ) ;
#17760 = CARTESIAN_POINT ( 'NONE',  ( 92.71251373007059726, -30.00000000000000355, 191.0549262315104784 ) ) ;
#17761 =( BOUNDED_SURFACE ( )  B_SPLINE_SURFACE ( 3, 2, ( 
 ( #76991, #44101, #95310 ),
 ( #87220, #38162, #85634 ),
 ( #3646, #70505, #36050 ),
 ( #103394, #79113, #27962 ),
 ( #36581, #103912, #12774 ),
 ( #61899, #86175, #69447 ),
 ( #29546, #28478, #12247 ),
 ( #102329, #29033, #86703 ),
 ( #45177, #60825, #68921 ),
 ( #4706, #4172, #71021 ),
 ( #61359, #20413, #94794 ),
 ( #45692, #62416, #94252 ),
 ( #101795, #54277, #21969 ),
 ( #21442, #13299, #30060 ) ),
 .UNSPECIFIED., .F., .F., .F. ) 
 B_SPLINE_SURFACE_WITH_KNOTS ( ( 4, 2, 2, 2, 2, 2, 4 ),
 ( 3, 3 ),
 ( 1.019150042136374168E-17, 0.001037790322792903758, 0.001556685484189350649, 0.002075580645585797541, 0.002594475806982244649, 0.003113370968378691324, 0.004151161291171584673 ),
 ( 0.000000000000000000, 1.000000000000000000 ),
 .UNSPECIFIED. ) 
 GEOMETRIC_REPRESENTATION_ITEM ( )  RATIONAL_B_SPLINE_SURFACE ( (
 ( 1.000000000000000000, 0.8266506655096989009, 1.000000000000000000),
 ( 1.000000000000000000, 0.8403402121222391941, 1.000000000000000000),
 ( 1.000000000000000000, 0.8527375874874671968, 1.000000000000000000),
 ( 1.000000000000000000, 0.8685816477866979968, 1.000000000000000000),
 ( 1.000000000000000000, 0.8733924426142005704, 1.000000000000000000),
 ( 1.000000000000000000, 0.8815965360735344980, 1.000000000000000000),
 ( 1.000000000000000000, 0.8850417602701512454, 1.000000000000000000),
 ( 1.000000000000000000, 0.8904811663267429012, 1.000000000000000000),
 ( 1.000000000000000000, 0.8924856662909712579, 1.000000000000000000),
 ( 1.000000000000000000, 0.8947492012709854503, 1.000000000000000000),
 ( 1.000000000000000000, 0.8950270886654364544, 1.000000000000000000),
 ( 1.000000000000000000, 0.8933353874799748739, 1.000000000000000000),
 ( 1.000000000000000000, 0.8887179207583161267, 1.000000000000000000),
 ( 1.000000000000000000, 0.8812198548864902392, 1.000000000000000000) ) ) 
 REPRESENTATION_ITEM ( '' )  SURFACE ( )  );
#17762 = VECTOR ( 'NONE', #24564, 1000.000000000000000 ) ;
#17763 = CARTESIAN_POINT ( 'NONE',  ( 27.33349330513380693, 1.593028355512270962E-15, 0.000000000000000000 ) ) ;
#17764 = CARTESIAN_POINT ( 'NONE',  ( -29.59213159313646457, 8.427504962981458903, 42.10535821593508388 ) ) ;
#17765 = CARTESIAN_POINT ( 'NONE',  ( -34.56726037194436429, 484.1545686971863347, -0.1516737162322892851 ) ) ;
#17766 = EDGE_CURVE ( 'NONE', #71682, #1581, #62648, .T. ) ;
#17767 = PRESENTATION_LAYER_ASSIGNMENT (  '', '', ( #60811 ) ) ;
#17768 = ORIENTED_EDGE ( 'NONE', *, *, #91249, .T. ) ;
#17769 = ORIENTED_EDGE ( 'NONE', *, *, #46663, .T. ) ;
#17770 = CARTESIAN_POINT ( 'NONE',  ( 51.29641226325185954, -18.72494439718292369, 45.83502416631164067 ) ) ;
#17771 = STYLED_ITEM ( 'NONE', ( #12598 ), #95272 ) ;
#17772 = CARTESIAN_POINT ( 'NONE',  ( 5.663715349034363022, 41.53602215441348022, -58.55436094691613391 ) ) ;
#17773 = EDGE_CURVE ( 'NONE', #92669, #94251, #72995, .T. ) ;
#17774 = ORIENTED_EDGE ( 'NONE', *, *, #18862, .F. ) ;
#17775 = CARTESIAN_POINT ( 'NONE',  ( -90.68311849838809735, -38.34324579396269428, 8.149761933289237703 ) ) ;
#17776 = ORIENTED_EDGE ( 'NONE', *, *, #81707, .T. ) ;
#17777 = CARTESIAN_POINT ( 'NONE',  ( 61.37206225042174879, 4.898587196589294500E-16, -4.000000000000007105 ) ) ;
#17778 = CARTESIAN_POINT ( 'NONE',  ( 108.4115401993842340, -38.35734607969845911, 191.8602404080995996 ) ) ;
#17779 = CARTESIAN_POINT ( 'NONE',  ( 15.57921808388646312, 22.99888987748559899, -0.5943451063223359476 ) ) ;
#17780 = CARTESIAN_POINT ( 'NONE',  ( 87.59251117718669377, -37.84866951032316251, 63.63991520629491561 ) ) ;
#17781 = CARTESIAN_POINT ( 'NONE',  ( -17.89009921150046623, 43.21754357103051092, -5.217241991157013814 ) ) ;
#17782 = CARTESIAN_POINT ( 'NONE',  ( -1.098564211878685359, 45.97059960990146266, -16.88266418162399063 ) ) ;
#17783 = CARTESIAN_POINT ( 'NONE',  ( -25.62494917502693781, 306.5451325936110152, -8.628440507281284866 ) ) ;
#17784 =( LENGTH_UNIT ( ) NAMED_UNIT ( * ) SI_UNIT ( .MILLI., .METRE. ) );
#17785 = ADVANCED_FACE ( 'NONE', ( #2929 ), #27799, .T. ) ;
#17786 = CARTESIAN_POINT ( 'NONE',  ( 74.84415321082225603, -59.99999999999998579, 180.0616514280479805 ) ) ;
#17787 = DIRECTION ( 'NONE',  ( 0.000000000000000000, 1.000000000000000000, 0.000000000000000000 ) ) ;
#17788 = CARTESIAN_POINT ( 'NONE',  ( -43.37695759419973740, 434.6160983767828725, 10.05510951421886645 ) ) ;
#17789 = ORIENTED_EDGE ( 'NONE', *, *, #35904, .T. ) ;
#17790 = CARTESIAN_POINT ( 'NONE',  ( 61.45962890681138902, -36.01090048717188097, 74.41309228244647045 ) ) ;
#17791 = FILL_AREA_STYLE ('',( #58780 ) ) ;
#17792 = DIRECTION ( 'NONE',  ( -1.000000000000000000, -1.224606353822377258E-16, -0.000000000000000000 ) ) ;
#17793 = B_SPLINE_CURVE_WITH_KNOTS ( 'NONE', 3,
 ( #18305, #10180, #35032, #68439, #91463, #41829, #15428, #65580, #7325, #25704, #57465, #89856, #65046, #74187, #66642, #41300, #83351, #25148, #33233, #90388 ),
 .UNSPECIFIED., .F., .F.,
 ( 4, 2, 2, 2, 2, 2, 2, 2, 2, 4 ),
 ( 0.003226290335689578279, 0.003730299423990245979, 0.004234308512290913679, 0.004738317600591582246, 0.005242326688892249079, 0.005746335777192917646, 0.006250344865493585346, 0.006502349409643918762, 0.006754353953794253046, 0.007258363042094923348 ),
 .UNSPECIFIED. ) ;
#17794 = CARTESIAN_POINT ( 'NONE',  ( -7.462369933651546106, -5.000000000000000000, -15.56882655052671005 ) ) ;
#17795 = DIRECTION ( 'NONE',  ( 0.000000000000000000, -1.000000000000000000, 0.000000000000000000 ) ) ;
#17796 = CARTESIAN_POINT ( 'NONE',  ( -33.16875022513573867, 397.0288761002586284, 25.82781127675604438 ) ) ;
#17797 = DIRECTION ( 'NONE',  ( -0.000000000000000000, -1.000000000000000000, -0.000000000000000000 ) ) ;
#17798 = DIRECTION ( 'NONE',  ( 0.000000000000000000, 0.000000000000000000, 1.000000000000000000 ) ) ;
#17799 = CARTESIAN_POINT ( 'NONE',  ( -8.000000000000000000, -25.24999999999999289, -9.797174393178825657E-16 ) ) ;
#17800 = CARTESIAN_POINT ( 'NONE',  ( 57.77058984079067017, 47.99999999999999289, 30.23507972700048541 ) ) ;
#17801 = AXIS2_PLACEMENT_3D ( 'NONE', #37096, #4164, #84553 ) ;
#17802 = VERTEX_POINT ( 'NONE', #88514 ) ;
#17803 = CARTESIAN_POINT ( 'NONE',  ( 83.33281023015626943, -50.09872871951235851, 184.7185439448685429 ) ) ;
#17804 = CARTESIAN_POINT ( 'NONE',  ( 2.607260012660386551E-19, 12.91535575337012354, -51.75000000000000711 ) ) ;
#17805 = CARTESIAN_POINT ( 'NONE',  ( 34.47678062874019389, 437.1474145881098821, 5.468662283308706407 ) ) ;
#17806 = ORIENTED_EDGE ( 'NONE', *, *, #22347, .F. ) ;
#17807 = CIRCLE ( 'NONE', #45377, 3.309500000000007880 ) ;
#17808 = CARTESIAN_POINT ( 'NONE',  ( -8.000000000000000000, -33.03125000409677625, -3.313708498984762496 ) ) ;
#17809 = CARTESIAN_POINT ( 'NONE',  ( 0.000000000000000000, 0.000000000000000000, 0.000000000000000000 ) ) ;
#17810 = DIRECTION ( 'NONE',  ( 1.000000000000000000, 0.000000000000000000, 0.000000000000000000 ) ) ;
#17811 = SURFACE_SIDE_STYLE ('',( #25943 ) ) ;
#17812 = CARTESIAN_POINT ( 'NONE',  ( -2.695484166377266178, -3.000000000000003109, -99.81725120020260533 ) ) ;
#17813 = CARTESIAN_POINT ( 'NONE',  ( -36.94718896193312219, -31.97723873816721962, -37.72039704602598675 ) ) ;
#17814 = DIRECTION ( 'NONE',  ( -0.000000000000000000, 1.000000000000000000, -0.000000000000000000 ) ) ;
#17815 = EDGE_CURVE ( 'NONE', #21876, #6068, #26570, .T. ) ;
#17816 =( LENGTH_UNIT ( ) NAMED_UNIT ( * ) SI_UNIT ( .MILLI., .METRE. ) );
#17817 = CARTESIAN_POINT ( 'NONE',  ( 53.83222069280748201, -59.99999999999999289, 81.95787437923988250 ) ) ;
#17818 = CIRCLE ( 'NONE', #105635, 4.172000000000001485 ) ;
#17819 = CARTESIAN_POINT ( 'NONE',  ( 94.26467260280679739, 1.016364837396684119E-14, 0.000000000000000000 ) ) ;
#17820 =( NAMED_UNIT ( * ) SI_UNIT ( $, .STERADIAN. ) SOLID_ANGLE_UNIT ( ) );
#17821 = ADVANCED_FACE ( 'NONE', ( #14590 ), #100577, .T. ) ;
#17823 = CARTESIAN_POINT ( 'NONE',  ( -12.69070879414525699, 23.10505005157635949, -5.367139868969495353 ) ) ;
#17822 = CARTESIAN_POINT ( 'NONE',  ( -17.86182390064972481, -24.36647526511750073, 36.39771317331339162 ) ) ;
#17824 = EDGE_CURVE ( 'NONE', #37165, #21469, #102419, .T. ) ;
#17825 = CARTESIAN_POINT ( 'NONE',  ( 46.02200000000003399, 0.000000000000000000, 5.000000000000004441 ) ) ;
#17826 = CARTESIAN_POINT ( 'NONE',  ( 4.401442555609581635E-16, -14.28125000204838457, -7.188101187500000044 ) ) ;
#17827 = CARTESIAN_POINT ( 'NONE',  ( -7.922281120364393914, 4.573931137438267847, -8.047472243342932430 ) ) ;
#17828 = ADVANCED_FACE ( 'NONE', ( #64244 ), #35176, .T. ) ;
#17829 = ORIENTED_EDGE ( 'NONE', *, *, #3881, .F. ) ;
#17830 = CARTESIAN_POINT ( 'NONE',  ( 6.976419320225629050, -21.93239868286991978, -38.54500339651450247 ) ) ;
#17831 = EDGE_CURVE ( 'NONE', #5588, #41982, #32948, .T. ) ;
#17832 = CARTESIAN_POINT ( 'NONE',  ( -19.21238756580856588, 49.78778941994462315, 61.53710458953445084 ) ) ;
#17833 = VECTOR ( 'NONE', #66743, 1000.000000000000227 ) ;
#17834 = EDGE_CURVE ( 'NONE', #43261, #49147, #82534, .T. ) ;
#17835 = ADVANCED_FACE ( 'NONE', ( #91179 ), #105735, .F. ) ;
#17836 = CARTESIAN_POINT ( 'NONE',  ( -9.335947753887891665, -2.525768943555868340, 14.78755529138710223 ) ) ;
#17837 =( LENGTH_UNIT ( ) NAMED_UNIT ( * ) SI_UNIT ( .MILLI., .METRE. ) );
#17839 = CARTESIAN_POINT ( 'NONE',  ( 31.96770739188477251, -47.40888721812473960, -32.79511155121236499 ) ) ;
#17838 = CARTESIAN_POINT ( 'NONE',  ( 5.125111398410182595, 53.50866886000678591, 8.522916231725279346 ) ) ;
#17840 = ORIENTED_EDGE ( 'NONE', *, *, #102333, .T. ) ;
#17841 = CARTESIAN_POINT ( 'NONE',  ( -5.190609988845227285, -87.63922286743591883, -3.016375611400009316 ) ) ;
#17842 = DIRECTION ( 'NONE',  ( 0.000000000000000000, 0.000000000000000000, 1.000000000000000000 ) ) ;
#17843 = AXIS2_PLACEMENT_3D ( 'NONE', #99222, #25937, #48551 ) ;
#17844 = ORIENTED_EDGE ( 'NONE', *, *, #25730, .T. ) ;
#17845 = CARTESIAN_POINT ( 'NONE',  ( 87.62222222222222001, 1.023464760207051730E-14, 0.000000000000000000 ) ) ;
#17846 = CARTESIAN_POINT ( 'NONE',  ( 30.92866670662933615, 8.704003156311262757, -40.98833526575349140 ) ) ;
#17847 = CARTESIAN_POINT ( 'NONE',  ( -19.47123783567355915, 41.87075544860245913, -80.42687978217861655 ) ) ;
#17848 = CARTESIAN_POINT ( 'NONE',  ( -95.31672547844928545, -59.99999999999999289, 51.31686920618464143 ) ) ;
#17849 = CARTESIAN_POINT ( 'NONE',  ( 4.898587196589412829E-16, -25.62499999999999645, -8.000000000000000000 ) ) ;
#17850 = CYLINDRICAL_SURFACE ( 'NONE', #59157, 4.000000000000000000 ) ;
#17851 = CARTESIAN_POINT ( 'NONE',  ( 35.69739812508499455, 430.4862580793411553, 4.964222856391316441 ) ) ;
#17852 = CARTESIAN_POINT ( 'NONE',  ( 40.06570913991743765, 460.7366702961331839, 2.123561850760146363 ) ) ;
#17854 = CARTESIAN_POINT ( 'NONE',  ( 32.04172522544141088, 487.4996691821121431, 8.071286837385784452 ) ) ;
#17853 = CARTESIAN_POINT ( 'NONE',  ( -34.47678062873981730, 437.1474145881089157, 5.468662283310409045 ) ) ;
#17855 = CARTESIAN_POINT ( 'NONE',  ( -85.16085110908363731, -25.44750803484134138, 168.5012799068713321 ) ) ;
#17856 = VERTEX_POINT ( 'NONE', #57179 ) ;
#17857 = CARTESIAN_POINT ( 'NONE',  ( 6.581905806972325301, 41.48827110309209587, -70.61906944721928880 ) ) ;
#17858 = VERTEX_POINT ( 'NONE', #90093 ) ;
#17859 = ORIENTED_EDGE ( 'NONE', *, *, #15564, .T. ) ;
#17860 = CARTESIAN_POINT ( 'NONE',  ( 0.000000000000000000, 0.000000000000000000, 0.000000000000000000 ) ) ;
#17861 = CARTESIAN_POINT ( 'NONE',  ( 33.94783393359906398, 484.1261039197348737, 1.321740980885009353 ) ) ;
#17862 = ORIENTED_EDGE ( 'NONE', *, *, #85143, .F. ) ;
#17863 = AXIS2_PLACEMENT_3D ( 'NONE', #36877, #13605, #46000 ) ;
#17864 = B_SPLINE_CURVE_WITH_KNOTS ( 'NONE', 3,
 ( #78220, #46391, #37807, #30221 ),
 .UNSPECIFIED., .F., .F.,
 ( 4, 4 ),
 ( 1.734723475976807094E-17, 0.002002602941643040913 ),
 .UNSPECIFIED. ) ;
#17865 = CARTESIAN_POINT ( 'NONE',  ( 53.78349330513380266, 6.975173280561618775E-15, 0.000000000000000000 ) ) ;
#17866 = PLANE ( 'NONE',  #61646 ) ;
#17867 = CARTESIAN_POINT ( 'NONE',  ( 41.50669491856072568, 1.482358050883964840E-15, 0.000000000000000000 ) ) ;
#17868 = DIRECTION ( 'NONE',  ( 0.5735764363510462704, 0.8191520442889915765, 0.000000000000000000 ) ) ;
#17869 = CARTESIAN_POINT ( 'NONE',  ( -0.6450442877596542779, 54.23802003939768923, 7.916300680330227379 ) ) ;
#17870 = DIRECTION ( 'NONE',  ( -0.000000000000000000, -1.000000000000000000, -0.000000000000000000 ) ) ;
#17871 = CARTESIAN_POINT ( 'NONE',  ( 19.61638200451619696, 6.123233995736770227E-16, -5.000000000000002665 ) ) ;
#17872 = CARTESIAN_POINT ( 'NONE',  ( 98.48959774644481513, -29.99999999999997158, 87.89110648026155559 ) ) ;
#17873 = EDGE_CURVE ( 'NONE', #67806, #63037, #33385, .T. ) ;
#17874 = CARTESIAN_POINT ( 'NONE',  ( -78.82101707352518360, -14.21045842199447584, 187.8153594499050882 ) ) ;
#17875 = CARTESIAN_POINT ( 'NONE',  ( -57.46856647868230539, -53.38719169883287208, 72.11333812933901299 ) ) ;
#17876 = VERTEX_POINT ( 'NONE', #66888 ) ;
#17877 = CARTESIAN_POINT ( 'NONE',  ( 19.61534071737431617, -60.00000000000000000, -44.23451022601076232 ) ) ;
#17878 = ORIENTED_EDGE ( 'NONE', *, *, #77608, .T. ) ;
#17879 = CARTESIAN_POINT ( 'NONE',  ( 7.255345346424188158, -56.87783837489315886, 33.35968231048251909 ) ) ;
#17880 = CARTESIAN_POINT ( 'NONE',  ( -106.4736054431515839, -60.15535417407983232, 175.2096886785453478 ) ) ;
#17881 = CARTESIAN_POINT ( 'NONE',  ( -7.188101187500000044, -9.781250002048384573, -8.802885111219163269E-16 ) ) ;
#17882 = CIRCLE ( 'NONE', #86796, 60.00000000000000000 ) ;
#17883 = CARTESIAN_POINT ( 'NONE',  ( -13.50000000000000178, 0.000000000000000000, 0.000000000000000000 ) ) ;
#17884 = EDGE_CURVE ( 'NONE', #63425, #83087, #58803, .T. ) ;
#17885 = CARTESIAN_POINT ( 'NONE',  ( 37.56673239365870387, 25.47613764497372557, 13.45617127780999134 ) ) ;
#17886 = ORIENTED_EDGE ( 'NONE', *, *, #79646, .T. ) ;
#17887 = DIRECTION ( 'NONE',  ( 0.000000000000000000, 1.000000000000000000, 0.000000000000000000 ) ) ;
#17888 = PRESENTATION_LAYER_ASSIGNMENT (  '', '', ( #4106 ) ) ;
#17889 = CARTESIAN_POINT ( 'NONE',  ( -51.57713148613659371, -59.99999999999998579, 75.78954276384915545 ) ) ;
#17890 = CARTESIAN_POINT ( 'NONE',  ( -1.112654532564758547, -3.176373552203621264E-18, 101.1535731093139816 ) ) ;
#17891 = CARTESIAN_POINT ( 'NONE',  ( 7.188101187499999156, -22.62500000204838813, 2.977408999572654924 ) ) ;
#17892 = CARTESIAN_POINT ( 'NONE',  ( 6.928203230275507885, 105.0000000000000000, -4.000000000000001776 ) ) ;
#17893 = CARTESIAN_POINT ( 'NONE',  ( 0.7145311798163270778, 9.237604307034018802, 2.885982852862873934E-16 ) ) ;
#17894 = CIRCLE ( 'NONE', #90245, 4.000000000000001776 ) ;
#17895 = CARTESIAN_POINT ( 'NONE',  ( 7.212408192734265810, -82.98482910679629754, -3.465038817813880456 ) ) ;
#17896 = CARTESIAN_POINT ( 'NONE',  ( -11.82790241188288149, -4.854504338693105048, -12.55817724909448785 ) ) ;
#17897 = SURFACE_STYLE_USAGE ( .BOTH. , #65892 ) ;
#17898 = FILL_AREA_STYLE ('',( #84740 ) ) ;
#17899 = DIRECTION ( 'NONE',  ( -0.5735764363510510444, -0.8191520442889883569, 0.000000000000000000 ) ) ;
#17900 = CARTESIAN_POINT ( 'NONE',  ( 86.12345145597880958, -60.00000000000003553, 8.975931401546647592 ) ) ;
#17901 = UNCERTAINTY_MEASURE_WITH_UNIT (LENGTH_MEASURE( 1.000000000000000082E-05 ), #28830, 'distance_accuracy_value', 'NONE');
#17902 = CARTESIAN_POINT ( 'NONE',  ( -30.84686216097265898, -36.01813085627019007, 32.80772232543694145 ) ) ;
#17903 = CARTESIAN_POINT ( 'NONE',  ( 45.00016045444848345, -56.79933079351206970, 48.30642181785263034 ) ) ;
#17904 = FILL_AREA_STYLE ('',( #83664 ) ) ;
#17905 = ORIENTED_EDGE ( 'NONE', *, *, #18520, .T. ) ;
#17906 = CARTESIAN_POINT ( 'NONE',  ( 43.63911886419051456, 435.1012159695193873, 10.95008075557279170 ) ) ;
#17907 = EDGE_CURVE ( 'NONE', #23499, #50026, #88510, .T. ) ;
#17908 = CARTESIAN_POINT ( 'NONE',  ( -80.97742334477548809, -38.83260288647188219, 194.5685436216422204 ) ) ;
#17909 = VERTEX_POINT ( 'NONE', #35076 ) ;
#17910 = DIRECTION ( 'NONE',  ( -0.000000000000000000, -1.000000000000000000, -0.000000000000000000 ) ) ;
#17911 = CARTESIAN_POINT ( 'NONE',  ( -13.92465259748497530, 2.727993544930908509, 5.548800750351575495 ) ) ;
#17912 = DIRECTION ( 'NONE',  ( -1.000000000000000000, -1.224606353822377258E-16, -0.000000000000000000 ) ) ;
#17913 = CARTESIAN_POINT ( 'NONE',  ( -7.262243269759384390, 41.41224259789315454, -59.17677581639546247 ) ) ;
#17914 = CARTESIAN_POINT ( 'NONE',  ( 35.60955124828987550, 461.3429156349023970, 3.374284740307414765 ) ) ;
#17915 = CARTESIAN_POINT ( 'NONE',  ( 104.3757837139179117, 1.016364837396684119E-14, 0.000000000000000000 ) ) ;
#17916 = CARTESIAN_POINT ( 'NONE',  ( -22.21408712632129934, 305.3228438409180967, 9.038496626227296105 ) ) ;
#17917 = EDGE_CURVE ( 'NONE', #7512, #21702, #20127, .T. ) ;
#17918 = CARTESIAN_POINT ( 'NONE',  ( 108.9248648557860975, -60.00000000000000000, 135.4428396493478886 ) ) ;
#17919 = CARTESIAN_POINT ( 'NONE',  ( 6.289692432696756264, -5.239086202715467877, 4.583616368337884772 ) ) ;
#17920 = CIRCLE ( 'NONE', #71246, 4.250000000000000000 ) ;
#17921 = PRESENTATION_LAYER_ASSIGNMENT (  '', '', ( #105738 ) ) ;
#17922 = DIRECTION ( 'NONE',  ( 0.000000000000000000, -1.000000000000000000, 0.000000000000000000 ) ) ;
#17923 = ORIENTED_EDGE ( 'NONE', *, *, #73053, .F. ) ;
#17924 =( GEOMETRIC_REPRESENTATION_CONTEXT ( 3 ) GLOBAL_UNCERTAINTY_ASSIGNED_CONTEXT ( ( #51293 ) ) GLOBAL_UNIT_ASSIGNED_CONTEXT ( ( #29240, #86916, #38371 ) ) REPRESENTATION_CONTEXT ( 'NONE', 'WORKASPACE' ) );
#17925 = CARTESIAN_POINT ( 'NONE',  ( -89.28786161495364126, -30.00000000000018474, 189.1170264501615463 ) ) ;
#17926 = EDGE_LOOP ( 'NONE', ( #26235, #32675, #23606, #75783 ) ) ;
#17927 = CARTESIAN_POINT ( 'NONE',  ( 25.88357335569430262, 37.21352753314932471, -8.492829661866421631 ) ) ;
#17928 = CARTESIAN_POINT ( 'NONE',  ( 43.10371592040107203, 462.6168321841715283, 4.970041475426227429 ) ) ;
#17929 = CARTESIAN_POINT ( 'NONE',  ( 21.29199042761633365, 304.0466698332161855, 9.978644581415256454 ) ) ;
#17930 = CARTESIAN_POINT ( 'NONE',  ( 9.165151389911681434, 29.73680493705114714, 3.999999999999999112 ) ) ;
#17931 = CARTESIAN_POINT ( 'NONE',  ( -7.188101187500001821, -20.37500000204838457, -2.977408999572651371 ) ) ;
#17932 = LINE ( 'NONE', #65404, #15800 ) ;
#17933 = PRODUCT_DEFINITION ( 'UNKNOWN', '', #54222, #75839 ) ;
#17934 = CARTESIAN_POINT ( 'NONE',  ( 4.898587196589412829E-16, -12.31250000409676915, -8.000000000000000000 ) ) ;
#17936 = ORIENTED_EDGE ( 'NONE', *, *, #76722, .T. ) ;
#17935 = CARTESIAN_POINT ( 'NONE',  ( -38.83537165123732393, 468.9475234385650992, 0.4936731619138239324 ) ) ;
#17937 = CARTESIAN_POINT ( 'NONE',  ( 80.20348483770095527, -60.38397368176433133, 177.1131073836802159 ) ) ;
#17938 = PRESENTATION_STYLE_ASSIGNMENT (( #8229 ) ) ;
#17939 = ORIENTED_EDGE ( 'NONE', *, *, #84944, .F. ) ;
#17940 = CARTESIAN_POINT ( 'NONE',  ( -20.49977525862259142, 302.8459220885798686, -10.00124997875687427 ) ) ;
#17941 = CYLINDRICAL_SURFACE ( 'NONE', #26976, 1.250000000000001110 ) ;
#17942 = LINE ( 'NONE', #35200, #62800 ) ;
#17943 = CARTESIAN_POINT ( 'NONE',  ( 40.59999999999999432, 1.533819458162526451E-15, 0.000000000000000000 ) ) ;
#17944 = CARTESIAN_POINT ( 'NONE',  ( -4.904566723942681783, 252.0224270247073832, 3.460360782932705437 ) ) ;
#17945 = CARTESIAN_POINT ( 'NONE',  ( -22.51188458451504104, 303.3301420540304321, 10.03976258024267842 ) ) ;
#17946 = ORIENTED_EDGE ( 'NONE', *, *, #34162, .F. ) ;
#17947 = APPLICATION_PROTOCOL_DEFINITION ( 'draft international standard', 'automotive_design', 1998, #30767 ) ;
#17948 = EDGE_CURVE ( 'NONE', #65653, #23677, #67941, .T. ) ;
#17949 = CARTESIAN_POINT ( 'NONE',  ( 45.59999999999999432, -3.309499999999999886, 0.000000000000000000 ) ) ;
#17950 = CARTESIAN_POINT ( 'NONE',  ( -5.000000000000000888, -64.69605072860053951, 10.12418081620033661 ) ) ;
#17951 = CARTESIAN_POINT ( 'NONE',  ( 87.35329077437620526, -35.37253959560227656, 188.8831662968735827 ) ) ;
#17952 = EDGE_CURVE ( 'NONE', #6487, #6569, #42063, .T. ) ;
#17953 = CARTESIAN_POINT ( 'NONE',  ( 1.219574468913127818, 34.50199799138920298, -28.81730245403649704 ) ) ;
#17954 = CARTESIAN_POINT ( 'NONE',  ( -5.082755093536325042, -32.09375000204838813, -5.082755093536325930 ) ) ;
#17955 = CARTESIAN_POINT ( 'NONE',  ( -13.50000000000000000, -7.794228634059976457, -13.00000000000000000 ) ) ;
#17956 = COLOUR_RGB ( '', 0.40784314, 0.44705882, 0.49803922) ;
#17957 = CARTESIAN_POINT ( 'NONE',  ( 8.239141761615604409, 51.66651536930677935, 3.999746327760523634 ) ) ;
#17958 = DIRECTION ( 'NONE',  ( 0.000000000000000000, -1.000000000000000000, 0.000000000000000000 ) ) ;
#17959 = PRESENTATION_LAYER_ASSIGNMENT (  '', '', ( #97153 ) ) ;
#17960 = ITEM_DEFINED_TRANSFORMATION ( 'NONE', 'NONE', #104123,  #10728 ) ;
#17961 = ORIENTED_EDGE ( 'NONE', *, *, #26824, .F. ) ;
#17962 = DIRECTION ( 'NONE',  ( 0.000000000000000000, 1.000000000000000000, 0.000000000000000000 ) ) ;
#17963 = EDGE_CURVE ( 'NONE', #62284, #66822, #54133, .T. ) ;
#17964 = CARTESIAN_POINT ( 'NONE',  ( -20.00000000000000000, 12.99999999999999289, 0.000000000000000000 ) ) ;
#17965 = CARTESIAN_POINT ( 'NONE',  ( -10.01459525654356852, 7.479155813459360758, 0.000000000000000000 ) ) ;
#17966 = EDGE_CURVE ( 'NONE', #23615, #4842, #35590, .T. ) ;
#17967 = CARTESIAN_POINT ( 'NONE',  ( 9.797174393178825657E-16, -30.00000000000000000, -8.000000000000000000 ) ) ;
#17968 = ORIENTED_EDGE ( 'NONE', *, *, #106108, .F. ) ;
#17969 = EDGE_CURVE ( 'NONE', #84701, #84646, #104906, .T. ) ;
#17970 = CARTESIAN_POINT ( 'NONE',  ( -30.00000000000000355, 462.0200324021746496, 12.95089283450024276 ) ) ;
#17971 = CARTESIAN_POINT ( 'NONE',  ( -7.500000000000005329, 42.83333333333328596, -68.91429205785459544 ) ) ;
#17972 = CARTESIAN_POINT ( 'NONE',  ( 112.5994561246894818, -57.67111607657447081, 189.2784257370963701 ) ) ;
#17973 = CARTESIAN_POINT ( 'NONE',  ( -8.559508646656381003, 51.83514083332404709, -1.531152949374265049 ) ) ;
#17974 = FACE_BOUND ( 'NONE', #137, .T. ) ;
#17975 = CARTESIAN_POINT ( 'NONE',  ( 36.48155966215278312, 26.06893451358279279, 11.58015166401925455 ) ) ;
#17976 = CARTESIAN_POINT ( 'NONE',  ( -76.90050140379315735, -60.00000000000000000, 190.1576257827158827 ) ) ;
#17977 = CARTESIAN_POINT ( 'NONE',  ( 9.089024885614422899, 43.98902913643783563, -13.78910996109302189 ) ) ;
#17978 = DIRECTION ( 'NONE',  ( -1.000000000000000000, -0.000000000000000000, -0.000000000000000000 ) ) ;
#17979 = DIRECTION ( 'NONE',  ( -0.5735764363510510444, -0.8191520442889883569, 0.000000000000000000 ) ) ;
#17980 = CARTESIAN_POINT ( 'NONE',  ( -84.00592508910983724, -50.16348015376611613, 186.9351520424663704 ) ) ;
#17982 = ORIENTED_EDGE ( 'NONE', *, *, #48061, .F. ) ;
#17981 = CIRCLE ( 'NONE', #92040, 3.309500000000001663 ) ;
#17983 =( NAMED_UNIT ( * ) PLANE_ANGLE_UNIT ( ) SI_UNIT ( $, .RADIAN. ) );
#17984 = AXIS2_PLACEMENT_3D ( 'NONE', #105219, #80929, #46968 ) ;
#17985 = ORIENTED_EDGE ( 'NONE', *, *, #63071, .T. ) ;
#17986 = CARTESIAN_POINT ( 'NONE',  ( 16.01290373797198541, 3.743961321039747769, 0.6473776101028398955 ) ) ;
#17987 = DIRECTION ( 'NONE',  ( 1.000000000000000000, 0.000000000000000000, 0.000000000000000000 ) ) ;
#17988 = AXIS2_PLACEMENT_3D ( 'NONE', #42342, #59612, #91445 ) ;
#17989 = AXIS2_PLACEMENT_3D ( 'NONE', #73342, #76010, #67411 ) ;
#17990 = CARTESIAN_POINT ( 'NONE',  ( -86.89782577854842316, -60.22521776081720901, -10.09765860210499788 ) ) ;
#17991 = CARTESIAN_POINT ( 'NONE',  ( -2.789712857209384556, -9.223132490779253345, -12.21941282805327234 ) ) ;
#17992 = CARTESIAN_POINT ( 'NONE',  ( -6.928203230275509661, -65.00000000000000000, -4.000000000000002665 ) ) ;
#17993 = CARTESIAN_POINT ( 'NONE',  ( 20.97754405179131254, 294.8763868968453608, 9.942224931492251727 ) ) ;
#17994 = CARTESIAN_POINT ( 'NONE',  ( 28.31356611659730760, 36.37420247609845347, -8.448101363750753379 ) ) ;
#17995 = CARTESIAN_POINT ( 'NONE',  ( -88.20421627925436781, 42.00000000000000000, 23.70422451878991765 ) ) ;
#17996 = CARTESIAN_POINT ( 'NONE',  ( -22.88454736421212488, 28.18015032983888801, 30.73969532942450300 ) ) ;
#17997 = CARTESIAN_POINT ( 'NONE',  ( 68.63284294399571195, -59.99999999999999289, 147.4025539660169954 ) ) ;
#17998 = CARTESIAN_POINT ( 'NONE',  ( -3.840629472727446691E-14, -1.200000000000000030E-05, -28.50000000000000000 ) ) ;
#17999 = EDGE_CURVE ( 'NONE', #102083, #82654, #74779, .T. ) ;
#18000 = CARTESIAN_POINT ( 'NONE',  ( 2.769948622550640671, -30.00000000000000000, -40.00000000000000000 ) ) ;
#18001 = CARTESIAN_POINT ( 'NONE',  ( -68.23005283090677153, -25.58391158071819405, 88.38719919826223759 ) ) ;
#18002 = ORIENTED_EDGE ( 'NONE', *, *, #15002, .F. ) ;
#18003 = CARTESIAN_POINT ( 'NONE',  ( 78.64960161195060095, -14.21045842199435860, 174.1843170503133251 ) ) ;
#18004 = CARTESIAN_POINT ( 'NONE',  ( -62.84963380242372466, 40.83902055873923587, -16.84608294976931120 ) ) ;
#18005 = CARTESIAN_POINT ( 'NONE',  ( 94.33413934944054802, -57.67234579118471061, 0.7340641395501579236 ) ) ;
#18006 = EDGE_LOOP ( 'NONE', ( #81141, #86298, #40585, #35604, #58156, #40823 ) ) ;
#18007 = CARTESIAN_POINT ( 'NONE',  ( 13.36289610070329381, 41.70153073425857571, -78.00930284188133612 ) ) ;
#18008 = CARTESIAN_POINT ( 'NONE',  ( 0.000000000000000000, 0.000000000000000000, 0.000000000000000000 ) ) ;
#18009 = ORIENTED_EDGE ( 'NONE', *, *, #62607, .F. ) ;
#18010 = CARTESIAN_POINT ( 'NONE',  ( 4.000000000000000000, 17.85270131633358304, -5.744562646538043715 ) ) ;
#18011 = FILL_AREA_STYLE ('',( #75152 ) ) ;
#18012 = CARTESIAN_POINT ( 'NONE',  ( 27.79797611564797322, 306.8793823578155298, -9.324996632398045548 ) ) ;
#18013 = CARTESIAN_POINT ( 'NONE',  ( -2.977408999572654480, -15.12500000204838457, 7.188101187499999156 ) ) ;
#18014 = CARTESIAN_POINT ( 'NONE',  ( -49.18736646279123903, 13.60337276043701671, 15.12866845614360223 ) ) ;
#18015 = CARTESIAN_POINT ( 'NONE',  ( 0.000000000000000000, 0.000000000000000000, -4.567799999999999194 ) ) ;
#18016 = SURFACE_STYLE_FILL_AREA ( #91890 ) ;
#18017 = CARTESIAN_POINT ( 'NONE',  ( 8.377077475354079672E-17, 56.87938524157181774, 0.6840402866513453084 ) ) ;
#18018 = EDGE_CURVE ( 'NONE', #3192, #74150, #30422, .T. ) ;
#18019 = DIRECTION ( 'NONE',  ( -0.5735764363510494901, -0.8191520442889894671, 0.000000000000000000 ) ) ;
#18020 = DIRECTION ( 'NONE',  ( 0.000000000000000000, 0.000000000000000000, 1.000000000000000000 ) ) ;
#18021 = EDGE_LOOP ( 'NONE', ( #94815, #33461, #71888, #100627, #103453 ) ) ;
#18022 = CARTESIAN_POINT ( 'NONE',  ( -7.224854285009186583, 41.52722297675348528, -69.60668029987157013 ) ) ;
#18024 = CARTESIAN_POINT ( 'NONE',  ( 32.29284039994544742, -29.08409890041876977, 32.09482466030329562 ) ) ;
#18023 = FACE_OUTER_BOUND ( 'NONE', #97531, .T. ) ;
#18025 = CARTESIAN_POINT ( 'NONE',  ( 27.63197730200188218, 308.2542597069073622, -8.233497725011043045 ) ) ;
#18026 = ORIENTED_EDGE ( 'NONE', *, *, #50408, .F. ) ;
#18027 = DIRECTION ( 'NONE',  ( -1.000000000000000000, -1.224606353822377258E-16, -0.000000000000000000 ) ) ;
#18029 = B_SPLINE_CURVE_WITH_KNOTS ( 'NONE', 3,
 ( #39981, #87483, #71795, #7063, #39463, #95565, #88536, #63740 ),
 .UNSPECIFIED., .F., .F.,
 ( 4, 2, 2, 4 ),
 ( 3.469446951953614189E-18, 0.002719188179122917007, 0.004078782268684381582, 0.005438376358245846157 ),
 .UNSPECIFIED. ) ;
#18028 = STYLED_ITEM ( 'NONE', ( #71495 ), #87112 ) ;
#18030 = ORIENTED_EDGE ( 'NONE', *, *, #104943, .T. ) ;
#18032 = CARTESIAN_POINT ( 'NONE',  ( 2.099928008175702901E-23, 44.08548369317413318, -16.25000000000000000 ) ) ;
#18031 = CARTESIAN_POINT ( 'NONE',  ( 0.7145311798163208605, 4.618802153517005848, 7.999999999999996447 ) ) ;
#18033 = DIRECTION ( 'NONE',  ( 0.000000000000000000, 0.000000000000000000, -1.000000000000000000 ) ) ;
#18034 = CARTESIAN_POINT ( 'NONE',  ( -5.500000000000007994, 42.00000000000000000, -68.91429205818155879 ) ) ;
#18035 = AXIS2_PLACEMENT_3D ( 'NONE', #22283, #20725, #29849 ) ;
#18036 = MECHANICAL_DESIGN_GEOMETRIC_PRESENTATION_REPRESENTATION (  '', ( #23197 ), #40412 ) ;
#18037 = CARTESIAN_POINT ( 'NONE',  ( 7.500000000000000000, -4.330127018922200755, -7.422398894150036064 ) ) ;
#18038 = AXIS2_PLACEMENT_3D ( 'NONE', #40679, #73565, #88716 ) ;
#18039 = FACE_OUTER_BOUND ( 'NONE', #46361, .T. ) ;
#18040 = CARTESIAN_POINT ( 'NONE',  ( 1.235826360310026795, 15.32379192987240657, -50.72445113533566285 ) ) ;
#18041 = EDGE_LOOP ( 'NONE', ( #56712, #57927 ) ) ;
#18042 = EDGE_CURVE ( 'NONE', #21685, #21200, #44550, .T. ) ;
#18043 = CARTESIAN_POINT ( 'NONE',  ( 80.91250902992011618, -60.00000000000000000, -27.39157300925418781 ) ) ;
#18044 = CARTESIAN_POINT ( 'NONE',  ( -9.177423055815456365, 46.16989776044872684, 13.55706802408392164 ) ) ;
#18045 = VECTOR ( 'NONE', #105301, 999.9999999999998863 ) ;
#18046 =( LENGTH_UNIT ( ) NAMED_UNIT ( * ) SI_UNIT ( .MILLI., .METRE. ) );
#18047 = CARTESIAN_POINT ( 'NONE',  ( -43.04469050570867239, 434.7734435962895532, 9.248231035232468145 ) ) ;
#18048 = EDGE_CURVE ( 'NONE', #61302, #89958, #21040, .T. ) ;
#18049 = CARTESIAN_POINT ( 'NONE',  ( 23.09999999999999432, -3.309499999999999886, 4.475777889183790779E-16 ) ) ;
#18050 = ORIENTED_EDGE ( 'NONE', *, *, #65794, .T. ) ;
#18051 = CARTESIAN_POINT ( 'NONE',  ( -20.00000000000000000, 12.99999999999999289, -7.500000000000000000 ) ) ;
#18052 = ORIENTED_EDGE ( 'NONE', *, *, #104075, .F. ) ;
#18053 = ORIENTED_EDGE ( 'NONE', *, *, #18444, .F. ) ;
#18054 = CYLINDRICAL_SURFACE ( 'NONE', #395, 9.000000000000000000 ) ;
#18055 =( NAMED_UNIT ( * ) PLANE_ANGLE_UNIT ( ) SI_UNIT ( $, .RADIAN. ) );
#18056 = CARTESIAN_POINT ( 'NONE',  ( -16.58625408824827119, 35.02807148468932752, -21.80698433968594685 ) ) ;
#18057 = FACE_OUTER_BOUND ( 'NONE', #8272, .T. ) ;
#18058 = CARTESIAN_POINT ( 'NONE',  ( 82.43496726913153339, -37.80750666079145361, -12.82402668043966720 ) ) ;
#18059 = CARTESIAN_POINT ( 'NONE',  ( -39.01698735643275029, 311.0398647938606587, 1.855041891536996834 ) ) ;
#18060 = DIRECTION ( 'NONE',  ( -0.5735764363510497121, 0.8191520442889892450, 1.003171929053521665E-16 ) ) ;
#18061 = CARTESIAN_POINT ( 'NONE',  ( 12.50000000000000533, 39.21611849718817666, -63.05155651949752382 ) ) ;
#18062 = ORIENTED_EDGE ( 'NONE', *, *, #97181, .T. ) ;
#18063 = PLANE ( 'NONE',  #6397 ) ;
#18065 = ADVANCED_FACE ( 'NONE', ( #13936 ), #31768, .F. ) ;
#18064 = VERTEX_POINT ( 'NONE', #87854 ) ;
#18066 = CARTESIAN_POINT ( 'NONE',  ( -5.693345022499886277, -3.000000000001474820, -71.09407784968050237 ) ) ;
#18067 = CARTESIAN_POINT ( 'NONE',  ( 42.43284980134657047, 464.7153848364305873, 16.15301860174535165 ) ) ;
#18069 = ORIENTED_EDGE ( 'NONE', *, *, #8662, .F. ) ;
#18068 = CARTESIAN_POINT ( 'NONE',  ( 6.536739755986783251, 51.40531100843265477, 7.403841948493273151 ) ) ;
#18070 = CARTESIAN_POINT ( 'NONE',  ( 77.27749820069621478, -36.02219164018512743, 127.9092550732632816 ) ) ;
#18071 = EDGE_CURVE ( 'NONE', #92046, #57881, #88575, .T. ) ;
#18072 = ORIENTED_EDGE ( 'NONE', *, *, #71479, .T. ) ;
#18073 = CARTESIAN_POINT ( 'NONE',  ( 7.188101187500000933, -22.06250000204838813, -2.977408999572650483 ) ) ;
#18074 =( BOUNDED_SURFACE ( )  B_SPLINE_SURFACE ( 3, 2, ( 
 ( #26068, #43263, #84783 ),
 ( #52399, #68066, #76680 ),
 ( #11402, #77759, #93414 ),
 ( #19032, #76145, #27117 ) ),
 .UNSPECIFIED., .F., .F., .F. ) 
 B_SPLINE_SURFACE_WITH_KNOTS ( ( 4, 4 ),
 ( 3, 3 ),
 ( -2.262729933977247754E-16, 0.0009806926547533787071 ),
 ( 0.000000000000000000, 1.000000000000000000 ),
 .UNSPECIFIED. ) 
 GEOMETRIC_REPRESENTATION_ITEM ( )  RATIONAL_B_SPLINE_SURFACE ( (
 ( 1.000000000000000000, 0.9603284238771497838, 1.000000000000000000),
 ( 1.000000000000000000, 0.9551945799212837596, 1.000000000000000000),
 ( 1.000000000000000000, 0.9458776633876946338, 1.000000000000000000),
 ( 1.000000000000000000, 0.9359444767143315635, 1.000000000000000000) ) ) 
 REPRESENTATION_ITEM ( '' )  SURFACE ( )  );
#18075 = PRESENTATION_LAYER_ASSIGNMENT (  '', '', ( #66318 ) ) ;
#18076 = CARTESIAN_POINT ( 'NONE',  ( -94.13300556333170732, -57.67265947060198528, 21.91134835779649137 ) ) ;
#18077 = VERTEX_POINT ( 'NONE', #28580 ) ;
#18078 = PLANE ( 'NONE',  #97113 ) ;
#18079 = CARTESIAN_POINT ( 'NONE',  ( 105.1830448132046030, -52.71715498403217026, 168.1466463903639976 ) ) ;
#18080 = CARTESIAN_POINT ( 'NONE',  ( 5.290067270632158980, 51.34639538792298197, -8.531152949374604333 ) ) ;
#18081 = DIRECTION ( 'NONE',  ( -1.000000000000000000, -1.224606353822377258E-16, -0.000000000000000000 ) ) ;
#18082 = CARTESIAN_POINT ( 'NONE',  ( -3.313708498984765161, -22.15625000409677270, 7.999999999999998224 ) ) ;
#18083 = DIRECTION ( 'NONE',  ( 0.000000000000000000, 0.000000000000000000, -1.000000000000000000 ) ) ;
#18084 = CARTESIAN_POINT ( 'NONE',  ( 18.58349330513380337, 4.000000000000003553, 0.000000000000000000 ) ) ;
#18085 = DIRECTION ( 'NONE',  ( -1.000000000000000000, -1.224606353822377258E-16, -0.000000000000000000 ) ) ;
#18086 = CARTESIAN_POINT ( 'NONE',  ( 9.381593208289372043, 32.01438638119505953, -3.465401811657802256 ) ) ;
#18087 = CARTESIAN_POINT ( 'NONE',  ( 97.53417911421176711, -56.34822196449098897, 195.8862142079233024 ) ) ;
#18088 = DIRECTION ( 'NONE',  ( 6.938893903907228378E-18, -2.390563456409604733E-25, -1.000000000000000000 ) ) ;
#18089 = CARTESIAN_POINT ( 'NONE',  ( 19.29515645702225868, 1.482358050883964840E-15, 0.000000000000000000 ) ) ;
#18090 = ORIENTED_EDGE ( 'NONE', *, *, #43802, .F. ) ;
#18091 = DIRECTION ( 'NONE',  ( 0.000000000000000000, 0.3049629831704142591, 0.9523642049635221429 ) ) ;
#18092 = PLANE ( 'NONE',  #92195 ) ;
#18093 = EDGE_CURVE ( 'NONE', #17070, #45005, #61468, .T. ) ;
#18094 = CARTESIAN_POINT ( 'NONE',  ( 91.09088295274877112, 6.123233995736568081E-16, -5.000000000000011546 ) ) ;
#18095 = CARTESIAN_POINT ( 'NONE',  ( -84.27187814110018849, -30.00000000000000355, 163.4558213934668061 ) ) ;
#18096 = ADVANCED_FACE ( 'NONE', ( #32818 ), #104032, .T. ) ;
#18097 = AXIS2_PLACEMENT_3D ( 'NONE', #2752, #86368, #93907 ) ;
#18098 = B_SPLINE_CURVE_WITH_KNOTS ( 'NONE', 3,
 ( #68191, #11530, #76275, #60657, #2383, #36408, #35329, #44457, #18607, #51469, #84384, #84914, #85999, #35870, #77352, #3998, #3465, #28302, #10999, #77886, #43917, #19161, #94063, #20228, #60135, #53078, #45001, #69793, #10473, #102688 ),
 .UNSPECIFIED., .F., .F.,
 ( 4, 2, 2, 2, 2, 2, 2, 2, 2, 2, 2, 2, 2, 2, 4 ),
 ( 0.01009607051181166983, 0.01101525429224240425, 0.01193443807267314041, 0.01285362185310387484, 0.01377280563353460927, 0.01423239752374997821, 0.01446219346885766269, 0.01469198941396534716, 0.01492178535907303163, 0.01515158130418071611, 0.01538137724928840058, 0.01561117319439608506, 0.01607076508461143666, 0.01653035697482678826, 0.01744954075525749146 ),
 .UNSPECIFIED. ) ;
#18099 = ORIENTED_EDGE ( 'NONE', *, *, #55769, .F. ) ;
#18100 = ORIENTED_EDGE ( 'NONE', *, *, #43040, .T. ) ;
#18101 = CARTESIAN_POINT ( 'NONE',  ( 4.168229866080995549, -48.49071734043477733, 43.45413307567940819 ) ) ;
#18102 = CARTESIAN_POINT ( 'NONE',  ( 70.53489761712432937, -57.68241810049395468, 158.3663422263703637 ) ) ;
#18103 = EDGE_CURVE ( 'NONE', #58408, #51789, #19716, .T. ) ;
#18105 = CARTESIAN_POINT ( 'NONE',  ( 34.10284876471455817, 5.000000000000003553, 0.000000000000000000 ) ) ;
#18104 = CARTESIAN_POINT ( 'NONE',  ( -15.22818746202957207, 3.929489829918556332, -4.609438620807924103 ) ) ;
#18106 = CARTESIAN_POINT ( 'NONE',  ( 54.68240138874981682, -36.51280362385794120, -35.33638688103538072 ) ) ;
#18107 = PRESENTATION_STYLE_ASSIGNMENT (( #25144 ) ) ;
#18108 = DIRECTION ( 'NONE',  ( -1.000000000000000000, -0.000000000000000000, -0.000000000000000000 ) ) ;
#18109 = CARTESIAN_POINT ( 'NONE',  ( -32.93660888375947593, -60.00000000000000711, 44.79872838179039007 ) ) ;
#18110 = AXIS2_PLACEMENT_3D ( 'NONE', #46666, #95236, #5677 ) ;
#18111 = CIRCLE ( 'NONE', #31892, 0.9999999999999994449 ) ;
#18112 = LINE ( 'NONE', #60178, #14119 ) ;
#18113 = FILL_AREA_STYLE ('',( #36972 ) ) ;
#18114 = COLOUR_RGB ( '', 0.66274510, 0.83137255, 0.94901961) ;
#18115 = CARTESIAN_POINT ( 'NONE',  ( -86.52299692828317745, -31.80693871344314516, 185.9752520618245057 ) ) ;
#18116 = EDGE_LOOP ( 'NONE', ( #87553, #46351, #46931, #1380, #31859, #90225 ) ) ;
#18117 = CARTESIAN_POINT ( 'NONE',  ( -42.50679667587944266, 460.9583926513354868, 2.954705527095128126 ) ) ;
#18118 = CARTESIAN_POINT ( 'NONE',  ( -10.15792624425911050, -29.03126705412632447, 28.73829528188013072 ) ) ;
#18119 = MECHANICAL_DESIGN_GEOMETRIC_PRESENTATION_REPRESENTATION (  '', ( #74972 ), #97317 ) ;
#18120 = FACE_OUTER_BOUND ( 'NONE', #86847, .T. ) ;
#18121 = DIRECTION ( 'NONE',  ( -1.000000000000000000, -1.224606353822377258E-16, -0.000000000000000000 ) ) ;
#18123 = CARTESIAN_POINT ( 'NONE',  ( 4.569677289105409379, -65.67692000944629171, 13.11436000269381985 ) ) ;
#18122 = CARTESIAN_POINT ( 'NONE',  ( -42.71758075471695548, 375.2456527110321076, 18.33958921108564155 ) ) ;
#18124 = ORIENTED_EDGE ( 'NONE', *, *, #23747, .F. ) ;
#18125 = FILL_AREA_STYLE ('',( #100077 ) ) ;
#18126 = CARTESIAN_POINT ( 'NONE',  ( 1.101047506738523696, 27.52289228718336034, 40.11312307701721380 ) ) ;
#18127 = CARTESIAN_POINT ( 'NONE',  ( 94.84444444444443434, -4.171999999999998820, 5.616230220889773285E-16 ) ) ;
#18128 = CARTESIAN_POINT ( 'NONE',  ( 17.79338952166786569, 50.00000000000001421, 62.19549801434460790 ) ) ;
#18129 = CARTESIAN_POINT ( 'NONE',  ( 29.07128654445882887, 296.9339959557834163, -9.548856946219741459 ) ) ;
#18130 = DIRECTION ( 'NONE',  ( -1.000000000000000000, -1.224606353822377258E-16, -0.000000000000000000 ) ) ;
#18131 = ADVANCED_FACE ( 'NONE', ( #7970 ), #40364, .T. ) ;
#18132 = CARTESIAN_POINT ( 'NONE',  ( 106.8726675771063981, -14.21045842199433729, 167.8793401222494595 ) ) ;
#18133 = CARTESIAN_POINT ( 'NONE',  ( -82.67280634349272361, -29.09043949173138444, 151.5834487444393517 ) ) ;
#18134 = ORIENTED_EDGE ( 'NONE', *, *, #65217, .F. ) ;
#18135 = DIRECTION ( 'NONE',  ( 0.000000000000000000, -1.000000000000000000, 0.000000000000000000 ) ) ;
#18136 = FACE_OUTER_BOUND ( 'NONE', #59587, .T. ) ;
#18137 = SURFACE_SIDE_STYLE ('',( #75820 ) ) ;
#18138 = CARTESIAN_POINT ( 'NONE',  ( 19.73463816634110657, 304.7971333121958537, 8.925379062039144884 ) ) ;
#18139 = CARTESIAN_POINT ( 'NONE',  ( -42.48678019891495694, 465.9003906206858119, 13.75832259440540284 ) ) ;
#18140 = EDGE_CURVE ( 'NONE', #100701, #34409, #71318, .T. ) ;
#18141 = CARTESIAN_POINT ( 'NONE',  ( 6.289572920342627604, -6.243622107253693265, 2.843693100100563420 ) ) ;
#18142 = ORIENTED_EDGE ( 'NONE', *, *, #68314, .F. ) ;
#18143 = UNCERTAINTY_MEASURE_WITH_UNIT (LENGTH_MEASURE( 1.000000000000000082E-05 ), #43549, 'distance_accuracy_value', 'NONE');
#18144 = VERTEX_POINT ( 'NONE', #40882 ) ;
#18145 =( NAMED_UNIT ( * ) PLANE_ANGLE_UNIT ( ) SI_UNIT ( $, .RADIAN. ) );
#18146 = VECTOR ( 'NONE', #43939, 1000.000000000000000 ) ;
#18147 = CARTESIAN_POINT ( 'NONE',  ( -89.99999999999997158, -52.00000000000000000, 196.0238439516549818 ) ) ;
#18148 = CARTESIAN_POINT ( 'NONE',  ( 36.97265860262990600, 437.4722588954304570, 4.366279915526031452 ) ) ;
#18149 = ADVANCED_FACE ( 'NONE', ( #25261 ), #65693, .T. ) ;
#18150 = CARTESIAN_POINT ( 'NONE',  ( -5.378041831648492810, 41.50935559050609669, -58.55697846129572071 ) ) ;
#18151 = DIRECTION ( 'NONE',  ( -1.000000000000000000, 0.000000000000000000, 0.000000000000000000 ) ) ;
#18152 = DIRECTION ( 'NONE',  ( 0.000000000000000000, 1.000000000000000000, 0.000000000000000000 ) ) ;
#18153 = VERTEX_POINT ( 'NONE', #57575 ) ;
#18154 = CARTESIAN_POINT ( 'NONE',  ( 99.73874981799322370, -59.99999999999998579, 201.9620565075520062 ) ) ;
#18156 = CARTESIAN_POINT ( 'NONE',  ( 23.68178223146766470, -39.47564461994503660, 31.49583778405278522 ) ) ;
#18155 = CARTESIAN_POINT ( 'NONE',  ( -78.18420296597048491, -29.99999999999999645, 185.0796872551976548 ) ) ;
#18157 = CARTESIAN_POINT ( 'NONE',  ( 13.99999999999998401, 61.49999999999999289, -6.999999999999989342 ) ) ;
#18158 = CARTESIAN_POINT ( 'NONE',  ( 33.00000000000000000, 488.6481008951279250, 3.890293910850408210 ) ) ;
#18159 = CARTESIAN_POINT ( 'NONE',  ( -42.72860860146450790, -29.16005040975862883, 38.64535797928981964 ) ) ;
#18160 = LINE ( 'NONE', #18707, #38522 ) ;
#18161 = UNCERTAINTY_MEASURE_WITH_UNIT (LENGTH_MEASURE( 1.000000000000000082E-05 ), #48351, 'distance_accuracy_value', 'NONE');
#18162 = ORIENTED_EDGE ( 'NONE', *, *, #58820, .F. ) ;
#18163 = CARTESIAN_POINT ( 'NONE',  ( 43.00000000000000000, 500.0000000000002274, 15.00000000000000711 ) ) ;
#18164 = CARTESIAN_POINT ( 'NONE',  ( -43.69697758767997442, 434.4335448986656729, 11.30914782517130668 ) ) ;
#18165 = CARTESIAN_POINT ( 'NONE',  ( 40.07586470527510158, 337.7832441655235129, 20.21182470898328631 ) ) ;
#18166 = SURFACE_STYLE_USAGE ( .BOTH. , #91517 ) ;
#18167 = DIRECTION ( 'NONE',  ( 0.000000000000000000, -1.000000000000000000, 0.000000000000000000 ) ) ;
#18168 = CARTESIAN_POINT ( 'NONE',  ( -32.15166163075724626, 486.0589784586660471, 5.199393881400879103 ) ) ;
#18169 = ORIENTED_EDGE ( 'NONE', *, *, #648, .F. ) ;
#18170 = ORIENTED_EDGE ( 'NONE', *, *, #21665, .F. ) ;
#18171 = STYLED_ITEM ( 'NONE', ( #84412 ), #64682 ) ;
#18172 = CARTESIAN_POINT ( 'NONE',  ( 79.32260940021335216, -29.99999999999999289, -14.62515576484859459 ) ) ;
#18173 = CARTESIAN_POINT ( 'NONE',  ( 47.24099558602568294, 11.75653836616716141, 16.58383527959104242 ) ) ;
#18174 = LINE ( 'NONE', #58626, #27266 ) ;
#18175 = DIRECTION ( 'NONE',  ( -0.000000000000000000, 1.000000000000000000, -0.000000000000000000 ) ) ;
#18176 = CARTESIAN_POINT ( 'NONE',  ( 80.76767570714686428, -30.00000000000000355, 10.72804306168430344 ) ) ;
#18177 = EDGE_CURVE ( 'NONE', #81125, #27380, #16607, .T. ) ;
#18178 = CARTESIAN_POINT ( 'NONE',  ( -31.69405040003880814, 348.1944610541558518, 20.16544092466686777 ) ) ;
#18179 = ORIENTED_EDGE ( 'NONE', *, *, #75852, .T. ) ;
#18180 = CONICAL_SURFACE ( 'NONE', #64655, 3.309500000000001663, 0.9599310885968770357 ) ;
#18181 = ORIENTED_EDGE ( 'NONE', *, *, #381, .T. ) ;
#18182 = ORIENTED_EDGE ( 'NONE', *, *, #87129, .T. ) ;
#18183 = CARTESIAN_POINT ( 'NONE',  ( -32.71046359557016103, 465.7618366408448765, 11.82978892796183246 ) ) ;
#18184 =( NAMED_UNIT ( * ) PLANE_ANGLE_UNIT ( ) SI_UNIT ( $, .RADIAN. ) );
#18185 = CARTESIAN_POINT ( 'NONE',  ( -36.81189781133993932, 25.99449293029668340, -11.20643870584772550 ) ) ;
#18186 = CIRCLE ( 'NONE', #57704, 3.000000000000019096 ) ;
#18187 = CARTESIAN_POINT ( 'NONE',  ( 36.53955443788006363, 439.8193023638518753, 24.21875945428991272 ) ) ;
#18188 = ADVANCED_FACE ( 'NONE', ( #65154 ), #59326, .T. ) ;
#18189 = CARTESIAN_POINT ( 'NONE',  ( -32.13665136737670736, 374.7280873276972102, 24.09185903376077320 ) ) ;
#18190 = DIRECTION ( 'NONE',  ( -0.5735764363510494901, -0.8191520442889894671, 0.000000000000000000 ) ) ;
#18191 = EDGE_LOOP ( 'NONE', ( #104893, #69116 ) ) ;
#18192 = CARTESIAN_POINT ( 'NONE',  ( -6.145467200823436116, 49.99999999999999289, -92.99666842290275781 ) ) ;
#18193 = ORIENTED_EDGE ( 'NONE', *, *, #85036, .T. ) ;
#18194 = DIRECTION ( 'NONE',  ( 0.000000000000000000, -1.000000000000000000, 0.000000000000000000 ) ) ;
#18195 = CARTESIAN_POINT ( 'NONE',  ( 69.20520435146650584, -38.33177068396069131, 130.8227709917701986 ) ) ;
#18196 = CARTESIAN_POINT ( 'NONE',  ( 6.333820801331835781, 4.275724398228168965, -5.594228103108450867 ) ) ;
#18197 =( GEOMETRIC_REPRESENTATION_CONTEXT ( 3 ) GLOBAL_UNCERTAINTY_ASSIGNED_CONTEXT ( ( #19654 ) ) GLOBAL_UNIT_ASSIGNED_CONTEXT ( ( #16646, #41449, #101295 ) ) REPRESENTATION_CONTEXT ( 'NONE', 'WORKASPACE' ) );
#18198 = ADVANCED_FACE ( 'NONE', ( #6376 ), #105097, .T. ) ;
#18199 = STYLED_ITEM ( 'NONE', ( #39130 ), #22488 ) ;
#18200 = CARTESIAN_POINT ( 'NONE',  ( 34.73580866203639061, 304.6300892602635031, 12.21738039697267553 ) ) ;
#18201 = AXIS2_PLACEMENT_3D ( 'NONE', #78598, #95332, #79669 ) ;
#18202 = MECHANICAL_DESIGN_GEOMETRIC_PRESENTATION_REPRESENTATION (  '', ( #90537 ), #11291 ) ;
#18203 = CARTESIAN_POINT ( 'NONE',  ( -4.658465013329187165, 248.6763612032690105, 3.783534922165396441 ) ) ;
#18204 = AXIS2_PLACEMENT_3D ( 'NONE', #76398, #101749, #2512 ) ;
#18205 = VERTEX_POINT ( 'NONE', #64123 ) ;
#18206 = AXIS2_PLACEMENT_3D ( 'NONE', #2260, #2804, #34151 ) ;
#18207 = CARTESIAN_POINT ( 'NONE',  ( 17.64253364725055206, 45.32498240469067952, -6.177274125185148179 ) ) ;
#18208 = LINE ( 'NONE', #101758, #12738 ) ;
#18209 = DIRECTION ( 'NONE',  ( 0.000000000000000000, 0.000000000000000000, 1.000000000000000000 ) ) ;
#18210 = CARTESIAN_POINT ( 'NONE',  ( -3.313708498984798467, -21.03124999999998934, -7.999999999999961808 ) ) ;
#18211 = B_SPLINE_CURVE_WITH_KNOTS ( 'NONE', 3,
 ( #33380, #8008, #945, #17718, #99684, #26904, #41447, #82975, #50067, #50579, #66255, #74858, #8542, #9595, #34987, #83496 ),
 .UNSPECIFIED., .F., .F.,
 ( 4, 2, 2, 2, 2, 2, 2, 4 ),
 ( 2.909219710836648185E-18, 0.001212534658634416241, 0.002425069317268828580, 0.004850138634537652822, 0.006062673293172064944, 0.007275207951806477932, 0.008487742610440890054, 0.009700277269075302175 ),
 .UNSPECIFIED. ) ;
#18212 = ORIENTED_EDGE ( 'NONE', *, *, #17907, .F. ) ;
#18213 = CARTESIAN_POINT ( 'NONE',  ( -23.45191171818318665, 303.6749378929117711, 10.11563714018844884 ) ) ;
#18214 = SURFACE_STYLE_FILL_AREA ( #893 ) ;
#18215 = UNCERTAINTY_MEASURE_WITH_UNIT (LENGTH_MEASURE( 1.000000000000000082E-05 ), #20619, 'distance_accuracy_value', 'NONE');
#18216 = DIRECTION ( 'NONE',  ( 1.000000000000000000, 0.000000000000000000, 0.000000000000000000 ) ) ;
#18217 = CARTESIAN_POINT ( 'NONE',  ( -2.411464220262661495, -7.267994521134594876, -7.491772860716523930 ) ) ;
#18218 = DIRECTION ( 'NONE',  ( 0.000000000000000000, -1.000000000000000000, 0.000000000000000000 ) ) ;
#18219 = CARTESIAN_POINT ( 'NONE',  ( 19.50000000000000000, 12.99999999999999289, 0.000000000000000000 ) ) ;
#18220 = CARTESIAN_POINT ( 'NONE',  ( 0.000000000000000000, 70.00000000000000000, 0.000000000000000000 ) ) ;
#18221 = CARTESIAN_POINT ( 'NONE',  ( 85.88695608651612190, -35.61023455811969285, 185.0182596836982043 ) ) ;
#18222 = CARTESIAN_POINT ( 'NONE',  ( -8.067121135846440083, 44.45135178119163299, 0.000000000000000000 ) ) ;
#18223 = ORIENTED_EDGE ( 'NONE', *, *, #93021, .F. ) ;
#18224 = CARTESIAN_POINT ( 'NONE',  ( 90.07482630527962897, -57.66626241257390006, -22.18633397614781799 ) ) ;
#18225 = FACE_BOUND ( 'NONE', #21696, .T. ) ;
#18226 = CARTESIAN_POINT ( 'NONE',  ( 15.64225497181437419, 35.03862301904531762, -22.45844242034788962 ) ) ;
#18227 = CARTESIAN_POINT ( 'NONE',  ( 88.20199406385988539, 5.000000000000020428, 0.000000000000000000 ) ) ;
#18228 = AXIS2_PLACEMENT_3D ( 'NONE', #14472, #63603, #55465 ) ;
#18229 = CARTESIAN_POINT ( 'NONE',  ( -81.90312948688070094, -29.99999999999999645, 32.95728417534301968 ) ) ;
#18230 = EDGE_CURVE ( 'NONE', #38464, #30181, #96998, .T. ) ;
#18231 =( NAMED_UNIT ( * ) PLANE_ANGLE_UNIT ( ) SI_UNIT ( $, .RADIAN. ) );
#18232 = CARTESIAN_POINT ( 'NONE',  ( -6.733158593834142280, 41.46658730094299017, -70.54360490943875561 ) ) ;
#18233 = LINE ( 'NONE', #9040, #91184 ) ;
#18234 = EDGE_CURVE ( 'NONE', #77573, #4416, #31752, .T. ) ;
#18235 = CARTESIAN_POINT ( 'NONE',  ( -9.165151389911699198, 249.9999999999999716, -4.000000000000002665 ) ) ;
#18236 = CARTESIAN_POINT ( 'NONE',  ( -29.50962187807867210, 13.72866526111396546, 42.09567151085925474 ) ) ;
#18237 = CARTESIAN_POINT ( 'NONE',  ( 43.00000000000000000, 487.9285348210859752, 8.903916466042430145 ) ) ;
#18238 = DIRECTION ( 'NONE',  ( 1.000000000000000000, -0.000000000000000000, 0.000000000000000000 ) ) ;
#18239 = B_SPLINE_CURVE_WITH_KNOTS ( 'NONE', 3,
 ( #99898, #26071, #48677, #74553, #40601, #81049, #33595, #66470, #25528, #49213, #23931, #17409, #58927, #15266, #89696, #48150, #7163, #41142, #73484, #72955, #105862, #32004, #15796, #32544, #64879, #81561, #24464, #106382, #65416, #57299, #98310 ),
 .UNSPECIFIED., .F., .F.,
 ( 4, 2, 2, 1, 1, 2, 2, 1, 2, 2, 2, 2, 1, 1, 2, 2, 2, 4 ),
 ( 0.000000000000000000, 0.05356300153016844284, 0.06695375191271055182, 0.08034450229525266773, 0.1071260030603368579, 0.1205167534428789461, 0.1339075038254210204, 0.1606890045905052244, 0.1874705053555893730, 0.2142520061206735493, 0.2410335068857577534, 0.2544242572682998693, 0.2678150076508419297, 0.2945965084159261060, 0.3079872587984681109, 0.3213780091810101158, 0.3749410107111783574, 0.4285040122413465991 ),
 .UNSPECIFIED. ) ;
#18240 = CARTESIAN_POINT ( 'NONE',  ( -22.88866733252017482, 25.33094138452381827, 33.17289542880824627 ) ) ;
#18241 = CARTESIAN_POINT ( 'NONE',  ( 0.000000000000000000, -5.629165124598853431, -3.249999999999994227 ) ) ;
#18242 = CARTESIAN_POINT ( 'NONE',  ( 12.17407353652991908, -16.62868128721872196, -34.62501512136454807 ) ) ;
#18243 = CIRCLE ( 'NONE', #61356, 4.000000000000007105 ) ;
#18244 = CARTESIAN_POINT ( 'NONE',  ( -24.11972882727333456, -53.39844759095379345, 33.93414205717319732 ) ) ;
#18245 = VERTEX_POINT ( 'NONE', #48431 ) ;
#18246 = CARTESIAN_POINT ( 'NONE',  ( 5.919343243681500333, 11.56755076042193764, 3.736960138817876143 ) ) ;
#18247 = CARTESIAN_POINT ( 'NONE',  ( 0.000000000000000000, -50.00000000000000000, 112.0000000000000000 ) ) ;
#18248 = CARTESIAN_POINT ( 'NONE',  ( -6.928203230275512325, 84.73116675491002070, -4.000000000000000000 ) ) ;
#18249 = CARTESIAN_POINT ( 'NONE',  ( -66.76684803170716975, -29.86276467274606361, -22.29546326141434065 ) ) ;
#18251 = CARTESIAN_POINT ( 'NONE',  ( -65.51163020881617172, -21.77008787170778703, -21.27136415489606236 ) ) ;
#18250 = CARTESIAN_POINT ( 'NONE',  ( -0.7772950121166072313, 27.39127224023426166, 40.48240021764166130 ) ) ;
#18252 = ADVANCED_FACE ( 'NONE', ( #81322 ), #50659, .T. ) ;
#18253 = CIRCLE ( 'NONE', #26826, 7.500000000000000000 ) ;
#18254 = EDGE_LOOP ( 'NONE', ( #46891, #24957 ) ) ;
#18255 = CARTESIAN_POINT ( 'NONE',  ( -36.42556657147747501, 437.5919504960684776, 4.247212042401131704 ) ) ;
#18256 = ORIENTED_EDGE ( 'NONE', *, *, #36894, .F. ) ;
#18257 = FACE_OUTER_BOUND ( 'NONE', #13367, .T. ) ;
#18258 = SURFACE_STYLE_FILL_AREA ( #36591 ) ;
#18259 = EDGE_CURVE ( 'NONE', #21120, #97430, #25820, .T. ) ;
#18260 = AXIS2_PLACEMENT_3D ( 'NONE', #75408, #52192, #2044 ) ;
#18261 = DIRECTION ( 'NONE',  ( 0.000000000000000000, -1.000000000000000000, 0.000000000000000000 ) ) ;
#18262 = ORIENTED_EDGE ( 'NONE', *, *, #55586, .T. ) ;
#18263 = FILL_AREA_STYLE_COLOUR ( '', #53221 ) ;
#18264 = CIRCLE ( 'NONE', #90618, 4.000000000000001776 ) ;
#18265 = DIRECTION ( 'NONE',  ( 0.000000000000000000, -1.000000000000000000, 0.000000000000000000 ) ) ;
#18266 = CARTESIAN_POINT ( 'NONE',  ( 100.1542774294340887, -45.27487897115133109, 192.4539520511120827 ) ) ;
#18267 = VECTOR ( 'NONE', #19087, 1000.000000000000000 ) ;
#18269 = CARTESIAN_POINT ( 'NONE',  ( -7.045755811259134305, -8.696583969864475350, 3.790843699961852664 ) ) ;
#18268 = CARTESIAN_POINT ( 'NONE',  ( 9.091052096490022549, 294.6686584899208583, -4.203955522403658662 ) ) ;
#18270 = VERTEX_POINT ( 'NONE', #68904 ) ;
#18271 = AXIS2_PLACEMENT_3D ( 'NONE', #18546, #41733, #101568 ) ;
#18272 = ORIENTED_EDGE ( 'NONE', *, *, #4552, .T. ) ;
#18273 = PRESENTATION_LAYER_ASSIGNMENT (  '', '', ( #76838 ) ) ;
#18274 = ORIENTED_EDGE ( 'NONE', *, *, #39358, .T. ) ;
#18275 = CARTESIAN_POINT ( 'NONE',  ( 31.43460747645193010, 410.2298262219391063, 24.47801356763874026 ) ) ;
#18276 = CARTESIAN_POINT ( 'NONE',  ( 34.83349330513379982, 4.898587196589405926E-16, -4.000000000000001776 ) ) ;
#18277 = CARTESIAN_POINT ( 'NONE',  ( 9.106558737793045921, 53.52158284938358435, 3.908029755355241441 ) ) ;
#18279 = EDGE_CURVE ( 'NONE', #18574, #35853, #47220, .T. ) ;
#18278 = VERTEX_POINT ( 'NONE', #34429 ) ;
#18280 = CARTESIAN_POINT ( 'NONE',  ( 0.000000000000000000, 0.000000000000000000, -10.00000000000000000 ) ) ;
#18281 = LINE ( 'NONE', #33396, #6672 ) ;
#18282 = CARTESIAN_POINT ( 'NONE',  ( 37.33349330513379982, 4.898587196589411843E-16, -4.000000000000001776 ) ) ;
#18283 = CARTESIAN_POINT ( 'NONE',  ( -49.73192663144240555, -57.67846088945594829, 76.49129250627629517 ) ) ;
#18284 = CARTESIAN_POINT ( 'NONE',  ( -37.56673239365849781, 27.88554838446201600, 10.95617127781066102 ) ) ;
#18285 = AXIS2_PLACEMENT_3D ( 'NONE', #94880, #102422, #78138 ) ;
#18286 = CARTESIAN_POINT ( 'NONE',  ( -31.14694070047868735, 432.3293837220155069, 24.29762062537629319 ) ) ;
#18287 = CARTESIAN_POINT ( 'NONE',  ( 37.61650669486618881, 1.474610560812782335E-15, 0.000000000000000000 ) ) ;
#18288 = CARTESIAN_POINT ( 'NONE',  ( -90.14748428319414586, -30.00000000000004263, -6.309121115244137101 ) ) ;
#18289 = CARTESIAN_POINT ( 'NONE',  ( -43.54570344706616680, 464.5919001249994835, 9.427857144821919277 ) ) ;
#18290 = CARTESIAN_POINT ( 'NONE',  ( -52.30004809150737799, -25.64534318506951038, 49.83580167134282135 ) ) ;
#18291 = CARTESIAN_POINT ( 'NONE',  ( 30.11650669486618881, 1.474610560812782335E-15, 0.000000000000000000 ) ) ;
#18292 = ORIENTED_EDGE ( 'NONE', *, *, #89285, .F. ) ;
#18293 = CARTESIAN_POINT ( 'NONE',  ( 24.05868969682389036, 5.000000000000004441, 6.123233995736770227E-16 ) ) ;
#18294 = CARTESIAN_POINT ( 'NONE',  ( 33.09999999999999432, -3.309499999999999886, 0.000000000000000000 ) ) ;
#18295 = CARTESIAN_POINT ( 'NONE',  ( 10.63911829571853929, -0.9478434794733983093, 20.26887800423669717 ) ) ;
#18296 = ORIENTED_EDGE ( 'NONE', *, *, #74743, .T. ) ;
#18297 = CARTESIAN_POINT ( 'NONE',  ( 4.567209634097043391, 249.0640021391448045, -3.891254717191809931 ) ) ;
#18298 = CARTESIAN_POINT ( 'NONE',  ( 76.35497413732163352, -38.40080420323430133, 180.8501158277027798 ) ) ;
#18299 = FACE_OUTER_BOUND ( 'NONE', #71906, .T. ) ;
#18300 = CARTESIAN_POINT ( 'NONE',  ( -5.290067270634260410, 52.08006895350597176, -6.031152949369843697 ) ) ;
#18301 = CARTESIAN_POINT ( 'NONE',  ( -16.55845859191752112, 294.5717093170194403, 1.877662430929134096 ) ) ;
#18302 = AXIS2_PLACEMENT_3D ( 'NONE', #66545, #99422, #26657 ) ;
#18303 =( NAMED_UNIT ( * ) PLANE_ANGLE_UNIT ( ) SI_UNIT ( $, .RADIAN. ) );
#18304 = CARTESIAN_POINT ( 'NONE',  ( 85.96311599642660894, -30.00000000000000000, 178.3436844846160909 ) ) ;
#18305 = CARTESIAN_POINT ( 'NONE',  ( -3.381870600466846067E-15, 46.21383923812598482, -16.24999999999995026 ) ) ;
#18306 = EDGE_CURVE ( 'NONE', #101891, #33852, #2544, .T. ) ;
#18307 = CARTESIAN_POINT ( 'NONE',  ( -32.87547266101557852, 465.6993878536674742, 10.91512469976539279 ) ) ;
#18308 = B_SPLINE_CURVE_WITH_KNOTS ( 'NONE', 3,
 ( #88366, #62499, #21528, #46308 ),
 .UNSPECIFIED., .F., .F.,
 ( 4, 4 ),
 ( 0.000000000000000000, 1.000000000000000000 ),
 .UNSPECIFIED. ) ;
#18309 = EDGE_LOOP ( 'NONE', ( #93845, #100648, #29032, #6651 ) ) ;
#18310 = ORIENTED_EDGE ( 'NONE', *, *, #44623, .F. ) ;
#18311 = CARTESIAN_POINT ( 'NONE',  ( 53.53308456940848004, -36.03345146573957436, 55.90449180736266044 ) ) ;
#18312 = CARTESIAN_POINT ( 'NONE',  ( -44.23147267340018374, 435.1968787606626847, 14.01185548270382242 ) ) ;
#18313 = DIRECTION ( 'NONE',  ( -1.000000000000000000, -1.224606353822377258E-16, -0.000000000000000000 ) ) ;
#18314 = ADVANCED_FACE ( 'NONE', ( #10629 ), #16193, .T. ) ;
#18315 = VERTEX_POINT ( 'NONE', #76428 ) ;
#18317 = B_SPLINE_CURVE_WITH_KNOTS ( 'NONE', 3,
 ( #97745, #24448, #81545, #82095, #96710, #81031, #6620, #22847 ),
 .UNSPECIFIED., .F., .F.,
 ( 4, 2, 2, 4 ),
 ( -1.044876449520883118E-05, 0.0004743401164197471763, 0.0007167345568772206729, 0.0009591289973346941696 ),
 .UNSPECIFIED. ) ;
#18316 = CARTESIAN_POINT ( 'NONE',  ( -91.45024945953299778, -38.38939539467013873, -7.873147340154297957 ) ) ;
#18318 = ORIENTED_EDGE ( 'NONE', *, *, #65176, .T. ) ;
#18319 = PRESENTATION_STYLE_ASSIGNMENT (( #67388 ) ) ;
#18320 = CARTESIAN_POINT ( 'NONE',  ( 108.5189666034069660, -38.35713193670694210, 191.5735787013350375 ) ) ;
#18321 = CARTESIAN_POINT ( 'NONE',  ( 15.27839008720943781, 22.61312091684385095, 2.812667176176046446 ) ) ;
#18322 = CARTESIAN_POINT ( 'NONE',  ( 84.87915795533969288, -45.28284344526540650, 33.56703465616141102 ) ) ;
#18323 = CARTESIAN_POINT ( 'NONE',  ( -7.996668423981801332, -3.000000000000002665, -78.85453280025087963 ) ) ;
#18324 = CARTESIAN_POINT ( 'NONE',  ( 5.169066395376115786, -13.70246774098871079, -6.130298896213989046 ) ) ;
#18325 = CARTESIAN_POINT ( 'NONE',  ( 0.000000000000000000, -8.000000000000000000, 0.000000000000000000 ) ) ;
#18326 = VECTOR ( 'NONE', #20371, 1000.000000000000341 ) ;
#18327 = ADVANCED_FACE ( 'NONE', ( #19329 ), #43548, .F. ) ;
#18328 = LINE ( 'NONE', #18878, #56075 ) ;
#18329 = EDGE_LOOP ( 'NONE', ( #18009, #91946, #80374, #83191, #98438 ) ) ;
#18330 = CARTESIAN_POINT ( 'NONE',  ( 61.87539551481160771, -29.06099552529470031, 72.15998440305089900 ) ) ;
#18331 = CARTESIAN_POINT ( 'NONE',  ( 0.000000000000000000, 0.000000000000000000, -13.00000000000000000 ) ) ;
#18332 = MECHANICAL_DESIGN_GEOMETRIC_PRESENTATION_REPRESENTATION (  '', ( #51005 ), #33888 ) ;
#18333 = DIRECTION ( 'NONE',  ( 0.000000000000000000, -0.9591753627735369880, 0.2828119931124806197 ) ) ;
#18334 = EDGE_LOOP ( 'NONE', ( #99148, #62887, #14184, #67297, #99997, #23622 ) ) ;
#18335 = DIRECTION ( 'NONE',  ( 0.000000000000000000, 0.4999999999999999445, -0.8660254037844387076 ) ) ;
#18336 = CARTESIAN_POINT ( 'NONE',  ( -42.76735375558020280, 409.2590350599533622, 19.91209603463725131 ) ) ;
#18337 = CARTESIAN_POINT ( 'NONE',  ( 13.58349330513380160, 1.593028355512270567E-15, 0.000000000000000000 ) ) ;
#18338 = CARTESIAN_POINT ( 'NONE',  ( 0.000000000000000000, 0.000000000000000000, 4.000000000000000000 ) ) ;
#18339 = CARTESIAN_POINT ( 'NONE',  ( 5.656854249492378806, -26.18749999999999645, 5.656854249492381470 ) ) ;
#18340 = AXIS2_PLACEMENT_3D ( 'NONE', #98693, #82531, #32945 ) ;
#18341 = CARTESIAN_POINT ( 'NONE',  ( -29.46142920806810395, -21.41144172159147985, 31.99227660533023609 ) ) ;
#18342 = CIRCLE ( 'NONE', #14849, 4.172000000000009479 ) ;
#18343 = COLOUR_RGB ( '', 0.72549020, 0.75294118, 0.79215686) ;
#18344 = DIRECTION ( 'NONE',  ( -1.000000000000000000, -1.224606353822377258E-16, -0.000000000000000000 ) ) ;
#18345 = AXIS2_PLACEMENT_3D ( 'NONE', #38436, #62699, #95591 ) ;
#18346 = VERTEX_POINT ( 'NONE', #44083 ) ;
#18347 = CARTESIAN_POINT ( 'NONE',  ( 85.94436667923068285, -21.71192462058850836, 172.2505468594992806 ) ) ;
#18348 = DIRECTION ( 'NONE',  ( 0.000000000000000000, 0.000000000000000000, -1.000000000000000000 ) ) ;
#18349 = CARTESIAN_POINT ( 'NONE',  ( 0.000000000000000000, 0.000000000000000000, 0.000000000000000000 ) ) ;
#18350 = ORIENTED_EDGE ( 'NONE', *, *, #45887, .T. ) ;
#18351 = CARTESIAN_POINT ( 'NONE',  ( -20.05074616892822803, 67.05096163904791240, -10.02537308446410869 ) ) ;
#18352 = VECTOR ( 'NONE', #21688, 1000.000000000000000 ) ;
#18353 = CARTESIAN_POINT ( 'NONE',  ( 0.000000000000000000, 0.000000000000000000, 5.000000000000000888 ) ) ;
#18354 = CARTESIAN_POINT ( 'NONE',  ( 9.920059540000885079, -3.000000000000002665, -96.33176891504291461 ) ) ;
#18355 = VECTOR ( 'NONE', #31526, 1000.000000000000227 ) ;
#18356 = CARTESIAN_POINT ( 'NONE',  ( -29.75089728405549749, -29.48423827979404876, -38.19276141328201390 ) ) ;
#18357 = EDGE_CURVE ( 'NONE', #81895, #66028, #17981, .T. ) ;
#18359 = AXIS2_PLACEMENT_3D ( 'NONE', #96187, #64353, #55162 ) ;
#18358 = CARTESIAN_POINT ( 'NONE',  ( 43.93350074023148011, -60.00000000000001421, 58.56064191452826151 ) ) ;
#18360 = DIRECTION ( 'NONE',  ( 0.000000000000000000, 0.000000000000000000, -1.000000000000000000 ) ) ;
#18361 = CARTESIAN_POINT ( 'NONE',  ( 10.44871243568134922, -13.87974197187156555, 31.87097697359232740 ) ) ;
#18362 = EDGE_CURVE ( 'NONE', #25464, #98077, #17158, .T. ) ;
#18364 = CARTESIAN_POINT ( 'NONE',  ( -13.08051135748678107, 23.84419156307226118, 4.072937932820233087 ) ) ;
#18363 = CARTESIAN_POINT ( 'NONE',  ( -31.88880264354962435, -33.67810866067220843, 41.75912053304347182 ) ) ;
#18365 = CARTESIAN_POINT ( 'NONE',  ( -9.165151389911681434, 85.26319506294885286, 4.000000000000001776 ) ) ;
#18366 = CARTESIAN_POINT ( 'NONE',  ( 27.18908553330205180, 296.5274986157688772, 10.30015177545897842 ) ) ;
#18367 = CARTESIAN_POINT ( 'NONE',  ( 31.84999999999999787, 1.533819458162526451E-15, 0.000000000000000000 ) ) ;
#18368 = DIRECTION ( 'NONE',  ( -1.000000000000000000, 0.000000000000000000, 0.000000000000000000 ) ) ;
#18369 = ORIENTED_EDGE ( 'NONE', *, *, #7559, .F. ) ;
#18370 = CARTESIAN_POINT ( 'NONE',  ( 3.250000000000015987, -5.629165124598843661, 1.734723475976807094E-15 ) ) ;
#18371 = AXIS2_PLACEMENT_3D ( 'NONE', #12242, #46742, #94249 ) ;
#18372 = CARTESIAN_POINT ( 'NONE',  ( -17.49999999999997513, 52.00000000000000711, 59.86364615470452577 ) ) ;
#18373 = UNCERTAINTY_MEASURE_WITH_UNIT (LENGTH_MEASURE( 1.000000000000000082E-05 ), #3066, 'distance_accuracy_value', 'NONE');
#18374 = DIRECTION ( 'NONE',  ( 0.000000000000000000, 1.000000000000000000, 0.000000000000000000 ) ) ;
#18376 = CARTESIAN_POINT ( 'NONE',  ( 37.82333364650842356, -34.58951055744512360, -29.84593800095458604 ) ) ;
#18375 = CARTESIAN_POINT ( 'NONE',  ( 9.165151389911699198, 250.2673515560711621, -4.000000000000002665 ) ) ;
#18377 = EDGE_CURVE ( 'NONE', #70516, #19922, #24846, .T. ) ;
#18378 = ORIENTED_EDGE ( 'NONE', *, *, #93016, .T. ) ;
#18379 = DIRECTION ( 'NONE',  ( -3.673940397442057649E-17, 0.000000000000000000, -1.000000000000000000 ) ) ;
#18380 = SURFACE_SIDE_STYLE ('',( #9179 ) ) ;
#18381 = VERTEX_POINT ( 'NONE', #100180 ) ;
#18382 = EDGE_CURVE ( 'NONE', #72570, #25185, #68802, .T. ) ;
#18383 = LINE ( 'NONE', #1620, #23127 ) ;
#18384 = CARTESIAN_POINT ( 'NONE',  ( -5.668939695963768344, 41.88723863199725628, -59.02759498664629945 ) ) ;
#18385 = DIRECTION ( 'NONE',  ( 0.000000000000000000, -1.000000000000000000, 0.000000000000000000 ) ) ;
#18386 = CARTESIAN_POINT ( 'NONE',  ( -103.7190351099681891, -59.99999999999999289, 102.7930850803005711 ) ) ;
#18387 =( NAMED_UNIT ( * ) SI_UNIT ( $, .STERADIAN. ) SOLID_ANGLE_UNIT ( ) );
#18388 = LINE ( 'NONE', #49658, #57342 ) ;
#18389 = CARTESIAN_POINT ( 'NONE',  ( 28.76346532419124458, 309.5219921958590135, -8.933260212751790164 ) ) ;
#18390 = CARTESIAN_POINT ( 'NONE',  ( 41.75908120488439579, 460.3944608375876442, 2.386179269085898724 ) ) ;
#18392 =( NAMED_UNIT ( * ) PLANE_ANGLE_UNIT ( ) SI_UNIT ( $, .RADIAN. ) );
#18391 = CARTESIAN_POINT ( 'NONE',  ( -6.145467200824003662, -3.000000000000002665, -92.99666842290695001 ) ) ;
#18393 = B_SPLINE_CURVE_WITH_KNOTS ( 'NONE', 3,
 ( #36488, #68827, #27871, #102235, #60736, #28386, #34350, #59129, #94146, #92011 ),
 .UNSPECIFIED., .F., .F.,
 ( 4, 2, 2, 2, 4 ),
 ( 0.000000000000000000, 0.001118707926289530573, 0.002237415852579061146, 0.003356123778868591936, 0.004474831705158122293 ),
 .UNSPECIFIED. ) ;
#18394 = CARTESIAN_POINT ( 'NONE',  ( -80.66956869714498168, -60.45664881771811139, 181.0067086544060260 ) ) ;
#18395 = VECTOR ( 'NONE', #19164, 1000.000000000000114 ) ;
#18396 = ORIENTED_EDGE ( 'NONE', *, *, #104173, .T. ) ;
#18397 = ORIENTED_EDGE ( 'NONE', *, *, #64416, .F. ) ;
#18398 = VERTEX_POINT ( 'NONE', #93161 ) ;
#18399 = CARTESIAN_POINT ( 'NONE',  ( 0.000000000000000000, 2.999999999999992450, -7.000000000000024869 ) ) ;
#18400 =( BOUNDED_CURVE ( )  B_SPLINE_CURVE ( 2, ( #46773, #5263, #38190, #47292, #63509, #79670, #24129, #13861, #71049 ),
 .UNSPECIFIED., .F., .F. ) 
 B_SPLINE_CURVE_WITH_KNOTS ( ( 3, 2, 2, 2, 3 ),
 ( 0.8088235294117647189, 0.8161764705882352811, 0.8235294117647058432, 0.8308823529411766273, 0.8382352941176471894 ),
 .UNSPECIFIED. ) 
 CURVE ( )  GEOMETRIC_REPRESENTATION_ITEM ( )  RATIONAL_B_SPLINE_CURVE ( ( 1.000000000000000000, 0.9238795325112867385, 1.000000000000000000, 0.9238795325112867385, 1.000000000000000000, 0.9238795325112867385, 1.000000000000000000, 0.9238795325112856283, 1.000000000000001110 ) ) 
 REPRESENTATION_ITEM ( '' )  );
#18401 = CARTESIAN_POINT ( 'NONE',  ( 6.070808553811512019E-16, -8.716842316802404511, -7.700127545397318585 ) ) ;
#18402 = ORIENTED_EDGE ( 'NONE', *, *, #74691, .T. ) ;
#18403 = DIRECTION ( 'NONE',  ( 0.000000000000000000, 0.000000000000000000, -1.000000000000000000 ) ) ;
#18404 = CARTESIAN_POINT ( 'NONE',  ( 27.59999999999999787, 1.411358822780289120E-15, 0.000000000000000000 ) ) ;
#18405 = DIRECTION ( 'NONE',  ( 0.000000000000000000, -1.000000000000000000, 0.000000000000000000 ) ) ;
#18406 = DIRECTION ( 'NONE',  ( -1.000000000000000000, -1.224606353822377258E-16, -0.000000000000000000 ) ) ;
#18407 = CIRCLE ( 'NONE', #28746, 4.172000000000009479 ) ;
#18408 = CARTESIAN_POINT ( 'NONE',  ( -0.7842673370667302413, 54.19802454029581895, 8.013341487591407741 ) ) ;
#18409 = DIRECTION ( 'NONE',  ( 0.000000000000000000, 1.000000000000000000, 0.000000000000000000 ) ) ;
#18410 = CARTESIAN_POINT ( 'NONE',  ( -5.000000000000000000, -14.11579947677662261, 9.475149649641746663 ) ) ;
#18411 = CARTESIAN_POINT ( 'NONE',  ( 99.89428240326108721, -30.00000000000003908, 96.08155976150675315 ) ) ;
#18412 = CARTESIAN_POINT ( 'NONE',  ( -100.5643661290868209, -60.00000000000009237, 204.3458358344470582 ) ) ;
#18413 = CARTESIAN_POINT ( 'NONE',  ( -58.02850647072168755, -42.96756333752487933, 68.81541298771311688 ) ) ;
#18414 = EDGE_LOOP ( 'NONE', ( #77274, #41053, #104085, #73352, #12796 ) ) ;
#18415 = CARTESIAN_POINT ( 'NONE',  ( 5.299999999999999822, 0.000000000000000000, 0.000000000000000000 ) ) ;
#18416 = CARTESIAN_POINT ( 'NONE',  ( 44.67209098260076416, -60.00000000002891198, -41.28851062587111898 ) ) ;
#18418 = EDGE_LOOP ( 'NONE', ( #40968, #101655, #11623, #96639 ) ) ;
#18417 = TOROIDAL_SURFACE ( 'NONE', #76984, 13.00000000000000000, 2.000000000000000000 ) ;
#18419 = CARTESIAN_POINT ( 'NONE',  ( -104.0167802882961610, -45.26538512285915772, 170.3650450961504248 ) ) ;
#18421 = AXIS2_PLACEMENT_3D ( 'NONE', #77156, #26521, #27588 ) ;
#18420 = DIRECTION ( 'NONE',  ( 0.000000000000000000, 0.000000000000000000, 1.000000000000000000 ) ) ;
#18422 = CARTESIAN_POINT ( 'NONE',  ( -5.930617632350569934, 51.27007761046171908, 8.357863051050422598 ) ) ;
#18423 = CARTESIAN_POINT ( 'NONE',  ( 3.822317990709313662, -30.00000000000000000, 6.092126002012808961 ) ) ;
#18424 = EDGE_LOOP ( 'NONE', ( #86864, #39861, #7781, #63691 ) ) ;
#18425 = CARTESIAN_POINT ( 'NONE',  ( 6.931554132387847567, -4.999999999998125055, -71.13906995425121238 ) ) ;
#18427 = VECTOR ( 'NONE', #86604, 1000.000000000000000 ) ;
#18426 = CARTESIAN_POINT ( 'NONE',  ( -79.00733982898046293, -60.00000000000002132, 194.6382242294647824 ) ) ;
#18428 = CARTESIAN_POINT ( 'NONE',  ( 36.36462878256535447, 25.99729457938612143, -12.55876404825913362 ) ) ;
#18429 = CARTESIAN_POINT ( 'NONE',  ( 2.977408999572651815, -21.31250000204838813, 7.188101187500000933 ) ) ;
#18430 = CARTESIAN_POINT ( 'NONE',  ( -1.010844465928027569, 37.02277097779673909, -27.74667697905033492 ) ) ;
#18431 = AXIS2_PLACEMENT_3D ( 'NONE', #105386, #41181, #98857 ) ;
#18432 = CARTESIAN_POINT ( 'NONE',  ( -2.451784423852116035, 21.02359296169644054, -6.560417912171430110 ) ) ;
#18433 = CARTESIAN_POINT ( 'NONE',  ( 81.98192093697382177, -38.00000000001091394, -13.86368299876859567 ) ) ;
#18434 = CARTESIAN_POINT ( 'NONE',  ( 43.27801297234275779, 485.1608390498441850, -2.258185464242984608 ) ) ;
#18435 = SURFACE_STYLE_USAGE ( .BOTH. , #75030 ) ;
#18436 = CARTESIAN_POINT ( 'NONE',  ( -16.64348903516521005, 45.88445698070336221, -4.157797401561533768 ) ) ;
#18437 = EDGE_CURVE ( 'NONE', #54223, #27527, #98860, .T. ) ;
#18438 = CARTESIAN_POINT ( 'NONE',  ( -5.025684061874351016, -6.606954474312070502, -14.98089720656572688 ) ) ;
#18439 = CARTESIAN_POINT ( 'NONE',  ( -31.37200766108269434, -46.43604509162865668, 34.89251725904698276 ) ) ;
#18440 =( NAMED_UNIT ( * ) PLANE_ANGLE_UNIT ( ) SI_UNIT ( $, .RADIAN. ) );
#18441 = CARTESIAN_POINT ( 'NONE',  ( 44.74630639848560065, -39.52738033063129564, 43.35887041975919942 ) ) ;
#18442 = CARTESIAN_POINT ( 'NONE',  ( -32.68648381768493039, 486.2785269687576601, 6.276066868102866181 ) ) ;
#18443 = CARTESIAN_POINT ( 'NONE',  ( -7.618844049274133390, 88.17235898929459381, 2.450177051822846064 ) ) ;
#18444 = EDGE_CURVE ( 'NONE', #53830, #32527, #92618, .T. ) ;
#18445 = CARTESIAN_POINT ( 'NONE',  ( -81.76979430546906258, -38.84151416488224129, 195.6111116689327218 ) ) ;
#18446 = EDGE_LOOP ( 'NONE', ( #62869, #20363, #25232, #26374, #91386 ) ) ;
#18448 = FILL_AREA_STYLE_COLOUR ( '', #62914 ) ;
#18447 = DIRECTION ( 'NONE',  ( -1.000000000000000000, -0.000000000000000000, -0.000000000000000000 ) ) ;
#18449 = CARTESIAN_POINT ( 'NONE',  ( 80.12066730003955684, -60.00000000000016342, 175.6537320670710187 ) ) ;
#18450 = CARTESIAN_POINT ( 'NONE',  ( 0.000000000000000000, 0.000000000000000000, -4.814498510800145681 ) ) ;
#18451 = CARTESIAN_POINT ( 'NONE',  ( -7.130799806110275973, 41.48518899657568682, -59.01258712674732010 ) ) ;
#18452 = FACE_OUTER_BOUND ( 'NONE', #96964, .T. ) ;
#18453 = DIRECTION ( 'NONE',  ( -1.000000000000000000, -1.224606353822377258E-16, -0.000000000000000000 ) ) ;
#18454 = CARTESIAN_POINT ( 'NONE',  ( 42.20540931547681396, 464.9254549434355681, 14.73500713293389985 ) ) ;
#18455 = CARTESIAN_POINT ( 'NONE',  ( 7.500000000000000888, 3.608439182435154269, -7.298562697733107285 ) ) ;
#18456 = CIRCLE ( 'NONE', #97629, 1.000000000000000444 ) ;
#18457 = CARTESIAN_POINT ( 'NONE',  ( 103.6220394604206092, -60.00000000000001421, 102.2245821222708315 ) ) ;
#18458 = DIRECTION ( 'NONE',  ( -1.000000000000000000, -1.224606353822377258E-16, -0.000000000000000000 ) ) ;
#18459 = EDGE_CURVE ( 'NONE', #38799, #17374, #35388, .T. ) ;
#18460 = CONICAL_SURFACE ( 'NONE', #39164, 5.000000000000001776, 0.9599310885968803664 ) ;
#18461 = FILL_AREA_STYLE ('',( #66452 ) ) ;
#18462 = ORIENTED_EDGE ( 'NONE', *, *, #58627, .F. ) ;
#18463 = SURFACE_STYLE_USAGE ( .BOTH. , #11385 ) ;
#18464 = CARTESIAN_POINT ( 'NONE',  ( -81.01065487345596239, -30.00000000000003197, -11.84759136933223012 ) ) ;
#18465 = ORIENTED_EDGE ( 'NONE', *, *, #48848, .F. ) ;
#18466 = CARTESIAN_POINT ( 'NONE',  ( 42.61140200160144786, 465.9030374194822457, 13.21253569360410829 ) ) ;
#18467 = FACE_OUTER_BOUND ( 'NONE', #45649, .T. ) ;
#18468 = CARTESIAN_POINT ( 'NONE',  ( 6.828042838857774299, 41.63841260098274688, -58.95291818684747653 ) ) ;
#18469 = CARTESIAN_POINT ( 'NONE',  ( -5.082755093536325042, -18.96875000204838457, -5.082755093536325930 ) ) ;
#18470 = CARTESIAN_POINT ( 'NONE',  ( -7.500000000000000000, -4.330127018922203419, -0.9999999999999974465 ) ) ;
#18471 = DIRECTION ( 'NONE',  ( -1.000000000000000000, -1.224606353822377258E-16, -0.000000000000000000 ) ) ;
#18473 = ORIENTED_EDGE ( 'NONE', *, *, #51879, .T. ) ;
#18472 =( LENGTH_UNIT ( ) NAMED_UNIT ( * ) SI_UNIT ( .MILLI., .METRE. ) );
#18474 = CARTESIAN_POINT ( 'NONE',  ( 82.82994579733494334, -36.01735634948035170, 162.7126334183690517 ) ) ;
#18475 = DIRECTION ( 'NONE',  ( 0.000000000000000000, -1.000000000000000000, 0.000000000000000000 ) ) ;
#18476 = VECTOR ( 'NONE', #32537, 1000.000000000000000 ) ;
#18477 = SURFACE_SIDE_STYLE ('',( #16320 ) ) ;
#18478 = ORIENTED_EDGE ( 'NONE', *, *, #31670, .F. ) ;
#18479 = CARTESIAN_POINT ( 'NONE',  ( 42.18756898894580587, 484.4522853017719513, -2.425645685620450909 ) ) ;
#18480 = PRESENTATION_STYLE_ASSIGNMENT (( #83185 ) ) ;
#18481 = DIRECTION ( 'NONE',  ( 0.1659550938513567053, -0.9861333108788017388, 0.000000000000000000 ) ) ;
#18482 = FACE_OUTER_BOUND ( 'NONE', #50532, .T. ) ;
#18483 = CARTESIAN_POINT ( 'NONE',  ( -4.656390720430131580, 251.3164618596054254, 3.786082374785823212 ) ) ;
#18484 = CARTESIAN_POINT ( 'NONE',  ( -27.80732017476346130, 308.5520240896025825, 11.27696741942652281 ) ) ;
#18485 = LINE ( 'NONE', #44883, #34850 ) ;
#18486 = ORIENTED_EDGE ( 'NONE', *, *, #3730, .T. ) ;
#18487 = EDGE_CURVE ( 'NONE', #51009, #2998, #67449, .T. ) ;
#18488 = COLOUR_RGB ( '', 0.72549020, 0.75294118, 0.79215686) ;
#18489 = TOROIDAL_SURFACE ( 'NONE', #78729, 7.999999999999983125, 1.000000000000000888 ) ;
#18490 = FACE_OUTER_BOUND ( 'NONE', #60071, .T. ) ;
#18491 = CARTESIAN_POINT ( 'NONE',  ( 87.06637252711929875, -50.08904605173307090, 191.9841204601254958 ) ) ;
#18492 = EDGE_CURVE ( 'NONE', #44460, #18895, #33467, .T. ) ;
#18493 = DIRECTION ( 'NONE',  ( -1.000000000000000000, -0.000000000000000000, -0.000000000000000000 ) ) ;
#18494 = CARTESIAN_POINT ( 'NONE',  ( 2.977408999572650927, -26.37500000204838457, -7.188101187500001821 ) ) ;
#18495 = COLOUR_RGB ( '', 0.09019608, 0.27058824, 0.51372549) ;
#18496 = TOROIDAL_SURFACE ( 'NONE', #87396, 12.00000000000003908, 1.000000000000000000 ) ;
#18497 = CARTESIAN_POINT ( 'NONE',  ( -10.00000000000000178, 0.000000000000000000, -9.999999999999998224 ) ) ;
#18498 = VECTOR ( 'NONE', #91255, 1000.000000000000000 ) ;
#18499 = LINE ( 'NONE', #92887, #96470 ) ;
#18500 = CARTESIAN_POINT ( 'NONE',  ( 37.06438722625302518, 3.851859888774471706E-31, 5.000000000000001776 ) ) ;
#18501 = ORIENTED_EDGE ( 'NONE', *, *, #41539, .T. ) ;
#18502 = DIRECTION ( 'NONE',  ( 0.000000000000000000, 0.000000000000000000, 1.000000000000000000 ) ) ;
#18503 = COLOUR_RGB ( '', 0.72549020, 0.75294118, 0.79215686) ;
#18504 = CARTESIAN_POINT ( 'NONE',  ( -5.859023161960823955, 4.697346715784889604, -4.999999999999999112 ) ) ;
#18505 = AXIS2_PLACEMENT_3D ( 'NONE', #91637, #2603, #100768 ) ;
#18506 = DIRECTION ( 'NONE',  ( -1.000000000000000000, -0.000000000000000000, -0.000000000000000000 ) ) ;
#18507 = EDGE_CURVE ( 'NONE', #54910, #11758, #30039, .T. ) ;
#18508 = VERTEX_POINT ( 'NONE', #61339 ) ;
#18509 = CARTESIAN_POINT ( 'NONE',  ( -30.00000000000000000, 464.1571281261997797, 12.55969758983369822 ) ) ;
#18510 = CARTESIAN_POINT ( 'NONE',  ( -42.89089171642230980, 462.3282028663734877, 4.511925770446329587 ) ) ;
#18511 = EDGE_CURVE ( 'NONE', #12868, #56691, #5736, .T. ) ;
#18512 = CARTESIAN_POINT ( 'NONE',  ( 32.84970661036780371, 435.2659274799900686, 16.49359760587357826 ) ) ;
#18513 = CARTESIAN_POINT ( 'NONE',  ( 4.898587196589412829E-16, -22.81250000409677270, -8.000000000000000000 ) ) ;
#18514 = AXIS2_PLACEMENT_3D ( 'NONE', #64986, #16431, #98923 ) ;
#18515 = DIRECTION ( 'NONE',  ( -1.000000000000000000, -1.224606353822377258E-16, -0.000000000000000000 ) ) ;
#18516 = CARTESIAN_POINT ( 'NONE',  ( 1.128077836147720614, 302.8478239976497548, 9.936168295454386623 ) ) ;
#18517 = CARTESIAN_POINT ( 'NONE',  ( -85.35784636269366388, -60.00000000000000000, 200.2676956853971717 ) ) ;
#18518 = CARTESIAN_POINT ( 'NONE',  ( 9.520703147840279712, 43.48472836740506153, -15.15874889920861968 ) ) ;
#18519 = LINE ( 'NONE', #101003, #82139 ) ;
#18520 = EDGE_CURVE ( 'NONE', #23955, #91293, #86764, .T. ) ;
#18521 = AXIS2_PLACEMENT_3D ( 'NONE', #27064, #9754, #84728 ) ;
#18522 = CARTESIAN_POINT ( 'NONE',  ( -85.13125407531725841, -35.77895824004616543, 181.7330530824042967 ) ) ;
#18523 = CARTESIAN_POINT ( 'NONE',  ( 23.15769230769230802, 4.172000000000003261, 0.000000000000000000 ) ) ;
#18524 = AXIS2_PLACEMENT_3D ( 'NONE', #29449, #36483, #11072 ) ;
#18525 = ORIENTED_EDGE ( 'NONE', *, *, #56843, .T. ) ;
#18526 = FACE_OUTER_BOUND ( 'NONE', #73467, .T. ) ;
#18527 = CARTESIAN_POINT ( 'NONE',  ( 3.753470829068755954, -1.089309597783790551, 104.5911851069063943 ) ) ;
#18528 = CARTESIAN_POINT ( 'NONE',  ( -86.27499340120317584, -60.13461745695511951, 5.971924282842688392 ) ) ;
#18529 = CARTESIAN_POINT ( 'NONE',  ( -5.180156406282273807, -13.23729396337573050, -7.081638082358150399 ) ) ;
#18530 = MECHANICAL_DESIGN_GEOMETRIC_PRESENTATION_REPRESENTATION (  '', ( #1534 ), #83958 ) ;
#18531 = ORIENTED_EDGE ( 'NONE', *, *, #64773, .T. ) ;
#18532 = FACE_OUTER_BOUND ( 'NONE', #74365, .T. ) ;
#18533 = LINE ( 'NONE', #91869, #95856 ) ;
#18535 = CONICAL_SURFACE ( 'NONE', #11572, 8.605212085995399107, 1.221730476396037490 ) ;
#18534 = CARTESIAN_POINT ( 'NONE',  ( 3.386172030103295594, -0.8620675201542831179, 104.0372870256219642 ) ) ;
#18536 = CARTESIAN_POINT ( 'NONE',  ( 51.40679407232553899, -29.99999999999998934, 68.09281640667435909 ) ) ;
#18537 = CARTESIAN_POINT ( 'NONE',  ( -16.32074838266548156, 61.49999999999999289, -8.160374191332742555 ) ) ;
#18538 = CARTESIAN_POINT ( 'NONE',  ( -87.30967359867977962, -14.21045842199447229, 28.19474181966119275 ) ) ;
#18539 = CARTESIAN_POINT ( 'NONE',  ( -76.54952089020632400, -22.13347653070191257, 114.5436684493959660 ) ) ;
#18540 = ORIENTED_EDGE ( 'NONE', *, *, #102819, .F. ) ;
#18541 = CARTESIAN_POINT ( 'NONE',  ( 62.45579587598661675, -29.99999999999998934, 99.43503315974342627 ) ) ;
#18542 = CARTESIAN_POINT ( 'NONE',  ( -61.99911740321165610, 40.83832667049977516, -19.74839170142865541 ) ) ;
#18543 = ORIENTED_EDGE ( 'NONE', *, *, #71778, .F. ) ;
#18544 = CARTESIAN_POINT ( 'NONE',  ( 55.63191178850256335, -57.67115282173337931, -38.73449349589243695 ) ) ;
#18545 = ORIENTED_EDGE ( 'NONE', *, *, #48465, .T. ) ;
#18546 = CARTESIAN_POINT ( 'NONE',  ( 87.04245038058458306, 1.016364837396684119E-14, 0.000000000000000000 ) ) ;
#18547 = CARTESIAN_POINT ( 'NONE',  ( 5.082755093536324154, -27.21875000204838813, 5.082755093536326818 ) ) ;
#18548 = CARTESIAN_POINT ( 'NONE',  ( -5.981118819178463220, -6.028165438199430959, 0.5452870891823657917 ) ) ;
#18549 = ORIENTED_EDGE ( 'NONE', *, *, #1841, .F. ) ;
#18551 = DIRECTION ( 'NONE',  ( 0.5000000000000024425, -0.8660254037844372643, 0.000000000000000000 ) ) ;
#18550 = AXIS2_PLACEMENT_3D ( 'NONE', #44342, #3353, #60020 ) ;
#18552 = EDGE_LOOP ( 'NONE', ( #31046, #59584 ) ) ;
#18553 = CARTESIAN_POINT ( 'NONE',  ( 0.000000000000000000, 0.000000000000000000, 0.000000000000000000 ) ) ;
#18554 = CARTESIAN_POINT ( 'NONE',  ( 46.97732051764557326, 17.75298140206541220, -16.28617214199182328 ) ) ;
#18555 = CARTESIAN_POINT ( 'NONE',  ( -11.06541635813348101, 43.17498430620472760, 15.13886682000006800 ) ) ;
#18556 = CARTESIAN_POINT ( 'NONE',  ( -2.977408999572650039, -12.68750000204838280, -7.188101187500001821 ) ) ;
#18557 = CARTESIAN_POINT ( 'NONE',  ( 91.09088295274877112, 5.000000000000020428, 0.000000000000000000 ) ) ;
#18558 = CARTESIAN_POINT ( 'NONE',  ( 0.000000000000000000, 0.000000000000000000, -3.012075477074183105 ) ) ;
#18559 = CARTESIAN_POINT ( 'NONE',  ( 59.41111111111111143, -3.309500000000000774, 0.000000000000000000 ) ) ;
#18560 = CARTESIAN_POINT ( 'NONE',  ( -9.739726766104316980, 49.99999999999999289, -87.61747884499031613 ) ) ;
#18561 = DIRECTION ( 'NONE',  ( -0.2021170706129989947, -0.9793613683246955581, 0.000000000000000000 ) ) ;
#18562 = FACE_OUTER_BOUND ( 'NONE', #60689, .T. ) ;
#18564 = ADVANCED_FACE ( 'NONE', ( #102311 ), #74842, .T. ) ;
#18563 = UNCERTAINTY_MEASURE_WITH_UNIT (LENGTH_MEASURE( 1.000000000000000082E-05 ), #104499, 'distance_accuracy_value', 'NONE');
#18565 = ORIENTED_EDGE ( 'NONE', *, *, #78028, .F. ) ;
#18566 = CARTESIAN_POINT ( 'NONE',  ( 4.581218816254565063, -2.199133564524530460, 103.5404609598622301 ) ) ;
#18567 = PRESENTATION_LAYER_ASSIGNMENT (  '', '', ( #25419 ) ) ;
#18569 = CARTESIAN_POINT ( 'NONE',  ( 31.61125088838073793, -22.14068077173801541, 30.54052087820161887 ) ) ;
#18568 = SURFACE_STYLE_FILL_AREA ( #66025 ) ;
#18570 = CARTESIAN_POINT ( 'NONE',  ( -32.17646412119387378, 464.6980787822280377, 10.84896803612861227 ) ) ;
#18571 = EDGE_LOOP ( 'NONE', ( #7376, #98151, #74378, #65875 ) ) ;
#18572 = EDGE_CURVE ( 'NONE', #76499, #79477, #93813, .T. ) ;
#18573 = ADVANCED_FACE ( 'NONE', ( #89843 ), #38695, .T. ) ;
#18574 = VERTEX_POINT ( 'NONE', #40748 ) ;
#18576 = DIRECTION ( 'NONE',  ( -0.2246406655633630400, 0.2919586099462053164, 0.9296756108737761481 ) ) ;
#18575 = CARTESIAN_POINT ( 'NONE',  ( 0.000000000000000000, 0.000000000000000000, 0.000000000000000000 ) ) ;
#18577 = VECTOR ( 'NONE', #50316, 1000.000000000000227 ) ;
#18578 = CARTESIAN_POINT ( 'NONE',  ( 4.910934285265537547, 41.41789230214733664, -70.63711736860776114 ) ) ;
#18579 = CARTESIAN_POINT ( 'NONE',  ( -43.59536836168519613, 485.3411848761405736, 3.528079522969483239 ) ) ;
#18580 = MECHANICAL_DESIGN_GEOMETRIC_PRESENTATION_REPRESENTATION (  '', ( #47782 ), #68457 ) ;
#18581 = DIRECTION ( 'NONE',  ( 0.000000000000000000, 1.000000000000000000, 0.000000000000000000 ) ) ;
#18582 = CARTESIAN_POINT ( 'NONE',  ( 0.000000000000000000, -48.79941684889505638, 112.0000000000000000 ) ) ;
#18583 = CARTESIAN_POINT ( 'NONE',  ( -36.57468857844283860, 463.9816243198204688, 19.61678995109673806 ) ) ;
#18584 = ORIENTED_EDGE ( 'NONE', *, *, #18625, .F. ) ;
#18585 = CARTESIAN_POINT ( 'NONE',  ( 82.44953616767962501, -60.00000000000000711, -26.43629379952842839 ) ) ;
#18586 = CARTESIAN_POINT ( 'NONE',  ( 91.09088295274877112, 5.000000000000021316, 0.000000000000000000 ) ) ;
#18587 = EDGE_CURVE ( 'NONE', #57189, #20836, #90346, .T. ) ;
#18588 = DIRECTION ( 'NONE',  ( 0.000000000000000000, 0.000000000000000000, 1.000000000000000000 ) ) ;
#18589 = COLOUR_RGB ( '', 0.08235294, 0.09019608, 0.10196078) ;
#18590 = CARTESIAN_POINT ( 'NONE',  ( -47.78256487607072245, 15.50824688151216257, -16.83670797542569986 ) ) ;
#18591 = ORIENTED_EDGE ( 'NONE', *, *, #57590, .F. ) ;
#18592 = CONICAL_SURFACE ( 'NONE', #78834, 5.000000000000010658, 0.9599310885968697082 ) ;
#18593 = CARTESIAN_POINT ( 'NONE',  ( -42.79755424932065466, 462.9502418795178755, 4.193817862666615603 ) ) ;
#18594 = ORIENTED_EDGE ( 'NONE', *, *, #26377, .F. ) ;
#18595 = EDGE_LOOP ( 'NONE', ( #53307, #94049, #75936, #86484 ) ) ;
#18596 = DIRECTION ( 'NONE',  ( -0.000000000000000000, -0.000000000000000000, -1.000000000000000000 ) ) ;
#18597 = FACE_OUTER_BOUND ( 'NONE', #79359, .T. ) ;
#18598 = CARTESIAN_POINT ( 'NONE',  ( -15.67130090876874604, 34.65698101724829172, -23.70546282029701857 ) ) ;
#18599 = CARTESIAN_POINT ( 'NONE',  ( 10.73176661990081371, 5.000000000000004441, 6.123233995736770227E-16 ) ) ;
#18600 = CARTESIAN_POINT ( 'NONE',  ( 84.20945289264685130, -45.27999795687735940, -10.90044817620680284 ) ) ;
#18601 = CARTESIAN_POINT ( 'NONE',  ( -33.53347886086262264, 315.6494051702701427, -6.932048779613169565 ) ) ;
#18602 = PLANE ( 'NONE',  #33599 ) ;
#18603 = CARTESIAN_POINT ( 'NONE',  ( -17.68672840718395634, 45.00000000000000711, 62.88372900578075075 ) ) ;
#18604 = ORIENTED_EDGE ( 'NONE', *, *, #3236, .T. ) ;
#18605 = CYLINDRICAL_SURFACE ( 'NONE', #54589, 4.000000000000000888 ) ;
#18606 = ORIENTED_EDGE ( 'NONE', *, *, #66304, .F. ) ;
#18607 = CARTESIAN_POINT ( 'NONE',  ( 49.15776748649641092, 8.563726824893073797, -15.04013919214091466 ) ) ;
#18608 = CARTESIAN_POINT ( 'NONE',  ( 30.00000000000000000, 0.000000000000000000, 0.000000000000000000 ) ) ;
#18609 = COLOUR_RGB ( '', 0.08235294, 0.09019608, 0.10196078) ;
#18611 = ORIENTED_EDGE ( 'NONE', *, *, #56229, .F. ) ;
#18610 = DIRECTION ( 'NONE',  ( -0.5735764363510497121, 0.8191520442889892450, 1.003171929053521665E-16 ) ) ;
#18612 = CARTESIAN_POINT ( 'NONE',  ( 70.72083910363338077, -42.95977585387966968, 106.3012996167854141 ) ) ;
#18613 = EDGE_LOOP ( 'NONE', ( #13360, #88594, #54488, #31370, #54443 ) ) ;
#18614 = CARTESIAN_POINT ( 'NONE',  ( 6.670804059825538701, -48.62050409103763116, 39.30984229886809800 ) ) ;
#18615 = DIRECTION ( 'NONE',  ( 0.000000000000000000, -1.000000000000000000, 0.000000000000000000 ) ) ;
#18616 = CARTESIAN_POINT ( 'NONE',  ( 7.188101187499999156, -25.25000000204839168, 2.977408999572654924 ) ) ;
#18617 = CARTESIAN_POINT ( 'NONE',  ( -89.88826151057727998, -57.66708741322880627, -22.42023280972025390 ) ) ;
#18618 = EDGE_LOOP ( 'NONE', ( #36290, #95872, #89039, #102636, #103462, #53697 ) ) ;
#18619 =( NAMED_UNIT ( * ) PLANE_ANGLE_UNIT ( ) SI_UNIT ( $, .RADIAN. ) );
#18620 = CARTESIAN_POINT ( 'NONE',  ( 67.48317336153286305, 6.856755485862130937E-15, 0.000000000000000000 ) ) ;
#18621 = AXIS2_PLACEMENT_3D ( 'NONE', #52035, #84419, #91969 ) ;
#18622 = CARTESIAN_POINT ( 'NONE',  ( 101.9416562456032267, -37.84849355845468466, 184.3864726907910097 ) ) ;
#18623 = AXIS2_PLACEMENT_3D ( 'NONE', #54332, #69496, #103446 ) ;
#18624 = CARTESIAN_POINT ( 'NONE',  ( 6.303135229827225849, 51.28796181275954069, -8.018170099117096328 ) ) ;
#18625 = EDGE_CURVE ( 'NONE', #71083, #58745, #104115, .T. ) ;
#18626 = CARTESIAN_POINT ( 'NONE',  ( 27.33349330513380693, 1.593028355512270962E-15, 0.000000000000000000 ) ) ;
#18627 = CARTESIAN_POINT ( 'NONE',  ( -8.000000000000000000, -15.03125000409677092, -3.313708498984762496 ) ) ;
#18628 = CARTESIAN_POINT ( 'NONE',  ( -6.851679529983103610E-15, 22.97884757028485225, 55.94820918777160301 ) ) ;
#18629 = DIRECTION ( 'NONE',  ( -0.000000000000000000, -0.000000000000000000, -1.000000000000000000 ) ) ;
#18630 = AXIS2_PLACEMENT_3D ( 'NONE', #33521, #18406, #24901 ) ;
#18631 = VECTOR ( 'NONE', #14328, 1000.000000000000000 ) ;
#18632 = CARTESIAN_POINT ( 'NONE',  ( -37.39037644056123355, 437.8315769264678465, 4.421099621100916366 ) ) ;
#18633 = CARTESIAN_POINT ( 'NONE',  ( 3.313708498984800688, -20.28124999999999289, 7.999999999999960032 ) ) ;
#18634 = DIRECTION ( 'NONE',  ( 1.000000000000000000, 6.090313915389453076E-17, 1.194435138363865691E-17 ) ) ;
#18635 = CARTESIAN_POINT ( 'NONE',  ( 4.242317035479241660, -29.99999999999999289, -6.258419296384283292 ) ) ;
#18636 = ORIENTED_EDGE ( 'NONE', *, *, #104075, .T. ) ;
#18637 = CARTESIAN_POINT ( 'NONE',  ( 6.250000000000000000, -5.051814855409235250, -7.198902722707430257 ) ) ;
#18638 =( NAMED_UNIT ( * ) PLANE_ANGLE_UNIT ( ) SI_UNIT ( $, .RADIAN. ) );
#18639 = DIRECTION ( 'NONE',  ( -1.000000000000000000, 0.000000000000000000, 0.000000000000000000 ) ) ;
#18640 = CARTESIAN_POINT ( 'NONE',  ( -88.08998614599749999, -29.99999999999999645, 186.9891332546852141 ) ) ;
#18641 = EDGE_CURVE ( 'NONE', #88306, #29177, #104971, .T. ) ;
#18642 = ORIENTED_EDGE ( 'NONE', *, *, #96032, .F. ) ;
#18643 = PRESENTATION_LAYER_ASSIGNMENT (  '', '', ( #82362 ) ) ;
#18644 = CARTESIAN_POINT ( 'NONE',  ( 4.999999999999995559, -46.00000000000000000, 42.58845726811989607 ) ) ;
#18645 = MECHANICAL_DESIGN_GEOMETRIC_PRESENTATION_REPRESENTATION (  '', ( #66894 ), #84058 ) ;
#18646 = CARTESIAN_POINT ( 'NONE',  ( 70.60288179947629317, -57.68235211279129260, 158.9257230075169502 ) ) ;
#18647 = STYLED_ITEM ( 'NONE', ( #10014 ), #40818 ) ;
#18649 = DIRECTION ( 'NONE',  ( -9.714451465434776236E-14, -1.000000000000000000, -2.768324312120152571E-13 ) ) ;
#18648 = CARTESIAN_POINT ( 'NONE',  ( -14.27029591641818662, 3.391655494167292950, -4.551126452497153529 ) ) ;
#18650 = CARTESIAN_POINT ( 'NONE',  ( 49.88420474661570836, -35.54202973682257038, -36.18076981765180733 ) ) ;
#18651 = CARTESIAN_POINT ( 'NONE',  ( 7.500000000000007105, -3.000000000000000000, -68.91429205785459544 ) ) ;
#18652 = FILL_AREA_STYLE_COLOUR ( '', #106286 ) ;
#18653 = B_SPLINE_CURVE_WITH_KNOTS ( 'NONE', 3,
 ( #25475, #7114, #83139, #40553, #90710, #16819, #33547, #41090 ),
 .UNSPECIFIED., .F., .F.,
 ( 4, 2, 2, 4 ),
 ( 0.02179091314793462492, 0.02376333058066962614, 0.02573574801340463084, 0.02968058287887463328 ),
 .UNSPECIFIED. ) ;
#18654 = CARTESIAN_POINT ( 'NONE',  ( -32.71478493902962725, -59.99999999999998579, 44.64407865478428761 ) ) ;
#18655 = STYLED_ITEM ( 'NONE', ( #60569 ), #59080 ) ;
#18656 = AXIS2_PLACEMENT_3D ( 'NONE', #25633, #101068, #60114 ) ;
#18657 = ADVANCED_FACE ( 'NONE', ( #48299 ), #36815, .F. ) ;
#18658 = FILL_AREA_STYLE_COLOUR ( '', #93383 ) ;
#18659 = EDGE_CURVE ( 'NONE', #54377, #4657, #100510, .T. ) ;
#18660 = SURFACE_STYLE_FILL_AREA ( #18113 ) ;
#18661 = CARTESIAN_POINT ( 'NONE',  ( -85.99455140606450243, -46.52813070295108133, 189.5206154160531185 ) ) ;
#18662 = EDGE_LOOP ( 'NONE', ( #12317, #51319, #70386, #76712, #86545 ) ) ;
#18663 = CARTESIAN_POINT ( 'NONE',  ( 35.44354944450248723, 438.5272207030965887, 4.908769030776976905 ) ) ;
#18664 = CARTESIAN_POINT ( 'NONE',  ( -3.030330602040952392, -39.47594121070261508, 30.46411644868683766 ) ) ;
#18665 = DIRECTION ( 'NONE',  ( 0.000000000000000000, 0.000000000000000000, 1.000000000000000000 ) ) ;
#18666 = CARTESIAN_POINT ( 'NONE',  ( 85.08140087618613734, -52.74747956140128480, 190.3168375061761424 ) ) ;
#18668 = DIRECTION ( 'NONE',  ( 0.000000000000000000, 0.000000000000000000, 1.000000000000000000 ) ) ;
#18667 = CARTESIAN_POINT ( 'NONE',  ( -28.70957337361108230, 297.0740850577855667, 2.420696489529333917 ) ) ;
#18669 = ORIENTED_EDGE ( 'NONE', *, *, #661, .T. ) ;
#18670 = CARTESIAN_POINT ( 'NONE',  ( -36.71681843521122346, 414.0170306961729239, 6.175275802599538899 ) ) ;
#18671 = COLOUR_RGB ( '', 0.40784314, 0.44705882, 0.49803922) ;
#18672 = CARTESIAN_POINT ( 'NONE',  ( -3.999994092537668244, -10.00072617203139380, 6.928206640937044192 ) ) ;
#18673 = CARTESIAN_POINT ( 'NONE',  ( -30.88008372391045242, 8.315965929874618467, -41.22858563418540712 ) ) ;
#18674 = CARTESIAN_POINT ( 'NONE',  ( 17.51571489128689763, 50.00000000000000711, 63.27752882552535851 ) ) ;
#18675 = CARTESIAN_POINT ( 'NONE',  ( 45.48126212248870814, 413.7349014071057240, 8.309231847991947362 ) ) ;
#18676 = CARTESIAN_POINT ( 'NONE',  ( -10.12668159690567826, 1.240160820363494750E-15, -9.226681596905679683 ) ) ;
#18677 = CARTESIAN_POINT ( 'NONE',  ( 96.86866073052655679, 5.000000000000020428, 0.000000000000000000 ) ) ;
#18678 = CONICAL_SURFACE ( 'NONE', #10015, 4.000000000000001776, 0.9599310885968774798 ) ;
#18679 = CARTESIAN_POINT ( 'NONE',  ( 101.4322121444104852, -14.21045842199439235, 121.1820579999150738 ) ) ;
#18680 = CARTESIAN_POINT ( 'NONE',  ( -81.58075026974830735, -36.03152022319830650, 152.4545240145561422 ) ) ;
#18681 = ORIENTED_EDGE ( 'NONE', *, *, #95545, .T. ) ;
#18682 = CARTESIAN_POINT ( 'NONE',  ( 32.04230769230768772, 1.411358822780289120E-15, 0.000000000000000000 ) ) ;
#18683 = CARTESIAN_POINT ( 'NONE',  ( 4.813555570991629118, 251.7947379651731978, -3.584128953194764655 ) ) ;
#18684 = CARTESIAN_POINT ( 'NONE',  ( 47.79234619673301410, -57.68000456042641844, 71.60442412587305228 ) ) ;
#18685 = CARTESIAN_POINT ( 'NONE',  ( -3.750000000000007105, 6.495190528383286477, 1.734723475976807094E-15 ) ) ;
#18686 = DIRECTION ( 'NONE',  ( -1.000000000000000000, -1.224606353822377258E-16, -0.000000000000000000 ) ) ;
#18687 = ORIENTED_EDGE ( 'NONE', *, *, #93217, .F. ) ;
#18688 = CARTESIAN_POINT ( 'NONE',  ( 31.35596682365820342, 438.0939828603633828, 22.55458131664035548 ) ) ;
#18689 = ORIENTED_EDGE ( 'NONE', *, *, #81171, .F. ) ;
#18690 = SURFACE_STYLE_FILL_AREA ( #92010 ) ;
#18691 = CARTESIAN_POINT ( 'NONE',  ( 2.563280883359705609, 15.30085158940939394, 9.673800154114783112 ) ) ;
#18692 = CARTESIAN_POINT ( 'NONE',  ( 4.699999999999999289, 3.752776749732569694, 6.499999999999997335 ) ) ;
#18693 = CARTESIAN_POINT ( 'NONE',  ( -60.62677696746660416, 49.99999999999999289, 24.18439665019479179 ) ) ;
#18694 = CARTESIAN_POINT ( 'NONE',  ( 5.000000000000000000, -15.43644767549559482, 12.61250542912354078 ) ) ;
#18697 = DIRECTION ( 'NONE',  ( 0.000000000000000000, -1.000000000000000000, 0.000000000000000000 ) ) ;
#18696 = B_SPLINE_CURVE_WITH_KNOTS ( 'NONE', 3,
 ( #72542, #104930, #24561, #56339, #7265, #55801, #8333, #89803, #15901, #48255, #81156, #88737, #31071, #57406, #32650, #40176, #33174, #73051, #80624, #105962, #24035, #90322, #7794, #98410, #39667, #41237, #63949, #211 ),
 .UNSPECIFIED., .F., .F.,
 ( 4, 2, 2, 2, 2, 2, 2, 2, 2, 2, 2, 2, 2, 4 ),
 ( 0.002626378601955864887, 0.003560090090687840179, 0.004493801579419815471, 0.005427513068151789896, 0.006361224556883765188, 0.006828080301249753702, 0.007061508173432749259, 0.007294936045615743950, 0.007528363917798739507, 0.007761791789981735065, 0.008228647534347722711, 0.008695503278713710357, 0.009162359023079696269, 0.01009607051181166983 ),
 .UNSPECIFIED. ) ;
#18695 = CIRCLE ( 'NONE', #73773, 4.000000000000000888 ) ;
#18698 = ORIENTED_EDGE ( 'NONE', *, *, #10560, .T. ) ;
#18699 = CARTESIAN_POINT ( 'NONE',  ( 96.25432131042047956, -59.99999999999998579, 57.89339241846288076 ) ) ;
#18701 = CARTESIAN_POINT ( 'NONE',  ( 21.32256896959740899, -39.47421529476722668, 31.13554192005910792 ) ) ;
#18700 = CARTESIAN_POINT ( 'NONE',  ( -84.52733067048065152, -59.99999999999991473, 202.7036346196431111 ) ) ;
#18703 = CARTESIAN_POINT ( 'NONE',  ( 82.11590029501883237, -38.00000000000000000, -13.62443290218705627 ) ) ;
#18702 = UNCERTAINTY_MEASURE_WITH_UNIT (LENGTH_MEASURE( 1.000000000000000082E-05 ), #68023, 'distance_accuracy_value', 'NONE');
#18704 = CARTESIAN_POINT ( 'NONE',  ( 37.58431281695580140, 369.0522562676452480, 4.070271502429146260 ) ) ;
#18705 =( GEOMETRIC_REPRESENTATION_CONTEXT ( 3 ) GLOBAL_UNCERTAINTY_ASSIGNED_CONTEXT ( ( #26548 ) ) GLOBAL_UNIT_ASSIGNED_CONTEXT ( ( #51975, #67651, #76785 ) ) REPRESENTATION_CONTEXT ( 'NONE', 'WORKASPACE' ) );
#18706 = CARTESIAN_POINT ( 'NONE',  ( -39.71717478528384504, -29.14735779400208671, 36.19107066650675364 ) ) ;
#18707 = CARTESIAN_POINT ( 'NONE',  ( 54.52222222222221859, -3.309500000000000774, 0.000000000000000000 ) ) ;
#18708 = UNCERTAINTY_MEASURE_WITH_UNIT (LENGTH_MEASURE( 1.000000000000000082E-05 ), #90504, 'distance_accuracy_value', 'NONE');
#18709 = VERTEX_POINT ( 'NONE', #63465 ) ;
#18710 = CARTESIAN_POINT ( 'NONE',  ( -11.17734400176827414, -4.285714285714296246, 22.67073868809948678 ) ) ;
#18711 = DIRECTION ( 'NONE',  ( 0.000000000000000000, -1.000000000000000000, 0.000000000000000000 ) ) ;
#18712 = CARTESIAN_POINT ( 'NONE',  ( -3.400000000000000355, 4.163799117101001052E-16, -8.000000000000000000 ) ) ;
#18713 = CIRCLE ( 'NONE', #68665, 5.000000000000010658 ) ;
#18714 = CARTESIAN_POINT ( 'NONE',  ( 43.00000000000000000, 450.0000000000002274, 28.20242257375372219 ) ) ;
#18715 = CARTESIAN_POINT ( 'NONE',  ( 7.934914944860278041, -61.13154352799890034, -1.051261972695690217 ) ) ;
#18716 = CARTESIAN_POINT ( 'NONE',  ( -30.00000000000000355, 488.8442721620238558, 4.433647275927455667 ) ) ;
#18717 = VERTEX_POINT ( 'NONE', #55843 ) ;
#18718 = CARTESIAN_POINT ( 'NONE',  ( -15.50007054317033628, 37.03005157377465650, -23.01145510268015926 ) ) ;
#18719 = AXIS2_PLACEMENT_3D ( 'NONE', #3884, #12481, #37876 ) ;
#18720 = ORIENTED_EDGE ( 'NONE', *, *, #73191, .F. ) ;
#18721 = CARTESIAN_POINT ( 'NONE',  ( 96.97070535361069687, -30.00000000000008882, 191.0996011186520320 ) ) ;
#18722 = DIRECTION ( 'NONE',  ( -1.000000000000000000, -1.224606353822377258E-16, -0.000000000000000000 ) ) ;
#18723 = CARTESIAN_POINT ( 'NONE',  ( -5.646888413699858944, -81.55025844029613324, 2.040714635159925905 ) ) ;
#18724 = EDGE_CURVE ( 'NONE', #48174, #25868, #47244, .T. ) ;
#18725 = CARTESIAN_POINT ( 'NONE',  ( 81.98815504130990917, -30.00000000000000355, 33.82435566842140418 ) ) ;
#18726 =( BOUNDED_CURVE ( )  B_SPLINE_CURVE ( 2, ( #28671, #100391, #44292, #26553, #45362, #1685, #10312, #92288, #61556 ),
 .UNSPECIFIED., .F., .F. ) 
 B_SPLINE_CURVE_WITH_KNOTS ( ( 3, 2, 2, 2, 3 ),
 ( 0.8088235294117648300, 0.8161764705882353921, 0.8235294117647060652, 0.8308823529411767383, 0.8382352941176473005 ),
 .UNSPECIFIED. ) 
 CURVE ( )  GEOMETRIC_REPRESENTATION_ITEM ( )  RATIONAL_B_SPLINE_CURVE ( ( 0.9999999999999988898, 0.9238795325112878487, 1.000000000000000000, 0.9238795325112867385, 1.000000000000000000, 0.9238795325112867385, 1.000000000000000000, 0.9238795325112844070, 1.000000000000002220 ) ) 
 REPRESENTATION_ITEM ( '' )  );
#18727 = EDGE_CURVE ( 'NONE', #19102, #31789, #80146, .T. ) ;
#18728 = CARTESIAN_POINT ( 'NONE',  ( -30.17217689282319881, 323.8004284941208653, 14.85062082350430046 ) ) ;
#18729 = EDGE_LOOP ( 'NONE', ( #71859, #89614, #95140, #45752 ) ) ;
#18730 = ORIENTED_EDGE ( 'NONE', *, *, #79476, .F. ) ;
#18731 = EDGE_LOOP ( 'NONE', ( #12275, #5892, #16432, #71187 ) ) ;
#18732 = VECTOR ( 'NONE', #38077, 1000.000000000000000 ) ;
#18734 = EDGE_LOOP ( 'NONE', ( #37082, #81278, #35987, #67741, #9028 ) ) ;
#18733 = CARTESIAN_POINT ( 'NONE',  ( -47.29503607946688248, 13.12332669628135484, -14.58854632476132629 ) ) ;
#18735 = FILL_AREA_STYLE ('',( #3042 ) ) ;
#18736 = CARTESIAN_POINT ( 'NONE',  ( -36.94914368061458987, 25.95618448055659755, -11.11629759539213502 ) ) ;
#18737 = VECTOR ( 'NONE', #83242, 1000.000000000000114 ) ;
#18738 = CARTESIAN_POINT ( 'NONE',  ( 5.727189096784631950, -13.57869875248741387, -1.806430436190354705 ) ) ;
#18740 = CONICAL_SURFACE ( 'NONE', #89382, 8.000000000000000000, 1.047197551196600296 ) ;
#18739 = CARTESIAN_POINT ( 'NONE',  ( -31.04379474421510920, 362.9620158108600094, 22.40809114958081238 ) ) ;
#18741 = CARTESIAN_POINT ( 'NONE',  ( 36.84999999999999432, -3.309499999999999886, 0.000000000000000000 ) ) ;
#18742 = VERTEX_POINT ( 'NONE', #74699 ) ;
#18743 = CARTESIAN_POINT ( 'NONE',  ( -5.036189802309416486, 49.99999999999999289, -76.26213611588271135 ) ) ;
#18744 = ORIENTED_EDGE ( 'NONE', *, *, #44473, .T. ) ;
#18745 = CARTESIAN_POINT ( 'NONE',  ( 35.90484354297773706, 0.000000000000000000, 5.000000000000002665 ) ) ;
#18746 = CARTESIAN_POINT ( 'NONE',  ( 74.34077940264843676, -38.32857108130681922, 163.3424694308657763 ) ) ;
#18747 = CARTESIAN_POINT ( 'NONE',  ( 31.88024914789805564, 435.8785884660822489, 17.60509251234928030 ) ) ;
#18748 = CARTESIAN_POINT ( 'NONE',  ( 31.56243845224520683, 299.8233007605157354, 11.05572696249486064 ) ) ;
#18749 = VECTOR ( 'NONE', #52947, 1000.000000000000000 ) ;
#18750 = CARTESIAN_POINT ( 'NONE',  ( -4.656749229489890674, 248.6823959187356365, -3.785628640239142584 ) ) ;
#18751 = ORIENTED_EDGE ( 'NONE', *, *, #92804, .T. ) ;
#18752 = DIRECTION ( 'NONE',  ( -1.000000000000000000, 0.000000000000000000, 0.000000000000000000 ) ) ;
#18753 = CARTESIAN_POINT ( 'NONE',  ( 0.000000000000000000, 152.0000000000000000, -5.000000000000000000 ) ) ;
#18754 = CARTESIAN_POINT ( 'NONE',  ( 38.23020739000291712, 310.6548857871646305, 5.705730873200064224 ) ) ;
#18755 = DIRECTION ( 'NONE',  ( 0.000000000000000000, 0.000000000000000000, 1.000000000000000000 ) ) ;
#18756 = CARTESIAN_POINT ( 'NONE',  ( 14.46174234134069359, 2.926873011494404597, 3.961839331259466856 ) ) ;
#18757 = ORIENTED_EDGE ( 'NONE', *, *, #102694, .T. ) ;
#18758 = CIRCLE ( 'NONE', #25611, 0.5000000000000004441 ) ;
#18759 = CARTESIAN_POINT ( 'NONE',  ( 7.414580834929599185, -87.64656280281482736, 3.010264818013836052 ) ) ;
#18760 = DIRECTION ( 'NONE',  ( -1.000000000000000000, -0.000000000000000000, -0.000000000000000000 ) ) ;
#18761 = CARTESIAN_POINT ( 'NONE',  ( 0.000000000000000000, 0.000000000000000000, -1.971869939371574620 ) ) ;
#18762 = CARTESIAN_POINT ( 'NONE',  ( 43.54152071275301239, 464.9591243512723509, 12.86066780444667579 ) ) ;
#18763 = AXIS2_PLACEMENT_3D ( 'NONE', #56108, #98702, #24857 ) ;
#18764 = CARTESIAN_POINT ( 'NONE',  ( 2.477036783837432310, 294.8392925584320210, 1.934412769351830041 ) ) ;
#18765 = CONICAL_SURFACE ( 'NONE', #34470, 4.172000000000001485, 0.9599310885968750373 ) ;
#18766 = CARTESIAN_POINT ( 'NONE',  ( 3.400000000000000355, 0.000000000000000000, -1.876475477074182940 ) ) ;
#18767 = EDGE_CURVE ( 'NONE', #85790, #84655, #94604, .T. ) ;
#18768 = CIRCLE ( 'NONE', #70392, 0.9999999999999986677 ) ;
#18769 = DIRECTION ( 'NONE',  ( 0.000000000000000000, -0.5000000000000016653, -0.8660254037844375974 ) ) ;
#18770 = CARTESIAN_POINT ( 'NONE',  ( 86.16337931003708661, -28.29594558851139041, 183.0065083202355538 ) ) ;
#18771 = AXIS2_PLACEMENT_3D ( 'NONE', #75871, #51045, #51587 ) ;
#18772 = PRESENTATION_STYLE_ASSIGNMENT (( #10101 ) ) ;
#18773 = CARTESIAN_POINT ( 'NONE',  ( -2.883864260984685401, 61.94980599433312562, 5.000000000000000000 ) ) ;
#18774 = ORIENTED_EDGE ( 'NONE', *, *, #83208, .F. ) ;
#18775 = CARTESIAN_POINT ( 'NONE',  ( 2.435347819570957628E-07, -57.67120202539301488, -44.61186700419775519 ) ) ;
#18776 = DIRECTION ( 'NONE',  ( 0.000000000000000000, 1.000000000000000000, 0.000000000000000000 ) ) ;
#18777 = CARTESIAN_POINT ( 'NONE',  ( 15.66935158561425290, 34.65848964118274012, -23.70178274125795070 ) ) ;
#18778 = PRESENTATION_STYLE_ASSIGNMENT (( #68364 ) ) ;
#18779 = CARTESIAN_POINT ( 'NONE',  ( -81.82247036775113713, -30.00000000000000355, 32.11225174614141054 ) ) ;
#18780 = EDGE_CURVE ( 'NONE', #60267, #105843, #58470, .T. ) ;
#18781 =( GEOMETRIC_REPRESENTATION_CONTEXT ( 3 ) GLOBAL_UNCERTAINTY_ASSIGNED_CONTEXT ( ( #92027 ) ) GLOBAL_UNIT_ASSIGNED_CONTEXT ( ( #82656, #74023, #32001 ) ) REPRESENTATION_CONTEXT ( 'NONE', 'WORKASPACE' ) );
#18782 = PRESENTATION_STYLE_ASSIGNMENT (( #43020 ) ) ;
#18783 = CARTESIAN_POINT ( 'NONE',  ( 46.85000000000000142, 5.616230220889764410E-16, -4.171999999999999709 ) ) ;
#18784 = DIRECTION ( 'NONE',  ( -1.000000000000000000, 0.000000000000000000, 0.000000000000000000 ) ) ;
#18786 = DIRECTION ( 'NONE',  ( 0.000000000000000000, 0.000000000000000000, 1.000000000000000000 ) ) ;
#18785 = CARTESIAN_POINT ( 'NONE',  ( -7.894787914004607998, -0.7661396099416337702, -7.591390474663430865 ) ) ;
#18787 = CARTESIAN_POINT ( 'NONE',  ( 6.999999999999995559, -46.00000000000000000, 39.12435565298213902 ) ) ;
#18788 = CARTESIAN_POINT ( 'NONE',  ( -47.03242928956601787, -37.42254165723339554, 45.62446206611129895 ) ) ;
#18789 = CARTESIAN_POINT ( 'NONE',  ( -36.66272501223257052, 491.8430924522253349, 12.58828741394581030 ) ) ;
#18790 = LINE ( 'NONE', #11702, #28823 ) ;
#18791 = CARTESIAN_POINT ( 'NONE',  ( 0.5805565836007648972, -7.505553499465138501, -1.190388518514737689E-16 ) ) ;
#18792 = PRESENTATION_LAYER_ASSIGNMENT (  '', '', ( #94619 ) ) ;
#18793 = CARTESIAN_POINT ( 'NONE',  ( 54.41739748717052549, -28.39686699294333749, -26.76204183714953544 ) ) ;
#18794 = EDGE_CURVE ( 'NONE', #19034, #22906, #84411, .T. ) ;
#18795 = AXIS2_PLACEMENT_3D ( 'NONE', #30987, #46603, #79501 ) ;
#18796 = CARTESIAN_POINT ( 'NONE',  ( -22.40161616653207233, -35.99812881269021148, 30.71311989447094959 ) ) ;
#18797 = ORIENTED_EDGE ( 'NONE', *, *, #13177, .T. ) ;
#18798 = DIRECTION ( 'NONE',  ( -0.000000000000000000, 1.000000000000000000, -0.000000000000000000 ) ) ;
#18799 = CARTESIAN_POINT ( 'NONE',  ( -9.644834624769973885, 108.0089050020577446, 2.648308524638421702 ) ) ;
#18800 = CARTESIAN_POINT ( 'NONE',  ( -16.95911990754058607, -49.92065424304449550, 32.46463353416660880 ) ) ;
#18801 = CARTESIAN_POINT ( 'NONE',  ( -47.26583134274487463, -26.85017121223957659, -28.66095955266838757 ) ) ;
#18802 = EDGE_CURVE ( 'NONE', #5164, #75282, #91895, .T. ) ;
#18804 = CARTESIAN_POINT ( 'NONE',  ( -72.96315109214474148, -34.58961219393635389, -20.39832908442921422 ) ) ;
#18803 = CARTESIAN_POINT ( 'NONE',  ( -0.1698221021441387313, 27.29656849860388235, 40.74999999999998579 ) ) ;
#18805 = ORIENTED_EDGE ( 'NONE', *, *, #19305, .T. ) ;
#18806 = CARTESIAN_POINT ( 'NONE',  ( 74.56127108291157413, 4.000000000000014211, 0.000000000000000000 ) ) ;
#18807 = ORIENTED_EDGE ( 'NONE', *, *, #85584, .F. ) ;
#18808 = LINE ( 'NONE', #85096, #56768 ) ;
#18809 = EDGE_CURVE ( 'NONE', #87281, #12410, #30209, .T. ) ;
#18810 = FACE_OUTER_BOUND ( 'NONE', #60437, .T. ) ;
#18811 = CARTESIAN_POINT ( 'NONE',  ( 32.82691535583474973, 485.1045372766795367, 1.724905475515037701 ) ) ;
#18813 = EDGE_CURVE ( 'NONE', #62559, #37271, #103973, .T. ) ;
#18812 = ORIENTED_EDGE ( 'NONE', *, *, #87659, .T. ) ;
#18814 = CARTESIAN_POINT ( 'NONE',  ( 34.42407431220851066, 1.340359594676612611E-15, 0.000000000000000000 ) ) ;
#18815 = CARTESIAN_POINT ( 'NONE',  ( -8.239065070776058874, 53.79488990884892274, -3.999784715952824143 ) ) ;
#18816 = CIRCLE ( 'NONE', #79071, 3.309500000000001663 ) ;
#18817 = CARTESIAN_POINT ( 'NONE',  ( 99.43428100118596547, -37.82682717057377886, 191.4305896544213681 ) ) ;
#18819 = CARTESIAN_POINT ( 'NONE',  ( -7.212994264445060644, -7.982886556599625649, 3.463766307298585811 ) ) ;
#18818 = CARTESIAN_POINT ( 'NONE',  ( 11.37552658721364196, -21.18656163614519627, 27.44809313948756113 ) ) ;
#18820 = EDGE_LOOP ( 'NONE', ( #74209, #53660, #865, #20708, #86154, #47691 ) ) ;
#18821 = EDGE_CURVE ( 'NONE', #26612, #105826, #10955, .T. ) ;
#18822 = VERTEX_POINT ( 'NONE', #1872 ) ;
#18823 = VERTEX_POINT ( 'NONE', #34292 ) ;
#18824 = CARTESIAN_POINT ( 'NONE',  ( 26.43220986894085911, 308.0179851418885164, 10.90514003825779099 ) ) ;
#18825 = CYLINDRICAL_SURFACE ( 'NONE', #35461, 4.250000000000000000 ) ;
#18826 = CARTESIAN_POINT ( 'NONE',  ( 15.70492864000501143, 46.17438344839472819, 4.577980962366692275 ) ) ;
#18827 = ORIENTED_EDGE ( 'NONE', *, *, #88118, .T. ) ;
#18828 = DIRECTION ( 'NONE',  ( -1.000000000000000000, -0.000000000000000000, -0.000000000000000000 ) ) ;
#18829 = DIRECTION ( 'NONE',  ( -0.000000000000000000, 1.000000000000000000, -0.000000000000000000 ) ) ;
#18830 = FACE_OUTER_BOUND ( 'NONE', #83502, .T. ) ;
#18831 = CARTESIAN_POINT ( 'NONE',  ( -94.82011412385188009, -59.99999999999028688, -11.94472248813712589 ) ) ;
#18832 = DIRECTION ( 'NONE',  ( -0.000000000000000000, -1.000000000000000000, -0.000000000000000000 ) ) ;
#18833 = CARTESIAN_POINT ( 'NONE',  ( -30.35537264529554946, 338.7115663565144246, 18.05293407820170515 ) ) ;
#18834 = CARTESIAN_POINT ( 'NONE',  ( -6.970005740671308736, 41.38563782891063880, -58.64823611141540027 ) ) ;
#18835 = CARTESIAN_POINT ( 'NONE',  ( -84.89308075164642275, -60.00000000000002842, -27.59301604020478038 ) ) ;
#18836 = CARTESIAN_POINT ( 'NONE',  ( -44.11327388758688528, 464.4313852428373934, 9.822198357558601600 ) ) ;
#18837 = AXIS2_PLACEMENT_3D ( 'NONE', #37434, #13631, #95636 ) ;
#18838 = CARTESIAN_POINT ( 'NONE',  ( -50.73354104550973886, -60.30528530471388393, 59.32307533831818347 ) ) ;
#18839 = ORIENTED_EDGE ( 'NONE', *, *, #10442, .F. ) ;
#18840 = CARTESIAN_POINT ( 'NONE',  ( 0.000000000000000000, -0.5000000000000000000, 8.500000000000000000 ) ) ;
#18841 = EDGE_LOOP ( 'NONE', ( #39873, #87752, #94070 ) ) ;
#18842 = CARTESIAN_POINT ( 'NONE',  ( -94.84365371199864114, -45.25270723803333084, 194.1674599023730536 ) ) ;
#18843 = DIRECTION ( 'NONE',  ( -1.000000000000000000, -1.224606353822377258E-16, -0.000000000000000000 ) ) ;
#18844 = CIRCLE ( 'NONE', #46367, 3.309499999999999886 ) ;
#18845 = CARTESIAN_POINT ( 'NONE',  ( 6.207999833770304399, 1.336757187206296660, 6.499999999999700684 ) ) ;
#18846 = EDGE_LOOP ( 'NONE', ( #86724, #75867 ) ) ;
#18847 =( NAMED_UNIT ( * ) PLANE_ANGLE_UNIT ( ) SI_UNIT ( $, .RADIAN. ) );
#18848 = CARTESIAN_POINT ( 'NONE',  ( 102.9968910219542693, -38.42918772397359817, 199.1158771562406571 ) ) ;
#18849 = CYLINDRICAL_SURFACE ( 'NONE', #14112, 9.999999999999994671 ) ;
#18850 = CARTESIAN_POINT ( 'NONE',  ( 3.718188220750195505, -48.95098499554293880, 104.2423402216923591 ) ) ;
#18851 = CARTESIAN_POINT ( 'NONE',  ( -17.49999999999996803, 47.99999999999997868, 64.09949417230998847 ) ) ;
#18852 = CARTESIAN_POINT ( 'NONE',  ( -90.56128410203886858, 42.00000000000000000, 11.85444436786840328 ) ) ;
#18853 = CARTESIAN_POINT ( 'NONE',  ( 85.96011442332530805, -30.00000000000000000, 178.3233229589895643 ) ) ;
#18854 = CARTESIAN_POINT ( 'NONE',  ( 0.000000000000000000, 0.000000000000000000, -8.000000000000000000 ) ) ;
#18855 = ADVANCED_FACE ( 'NONE', ( #76302 ), #60933, .F. ) ;
#18856 = CARTESIAN_POINT ( 'NONE',  ( 37.54559764570182523, 464.1143081516207189, 19.43664670202678835 ) ) ;
#18857 = CONICAL_SURFACE ( 'NONE', #61959, 7.500000000000000888, 0.8594454914424817238 ) ;
#18858 = ORIENTED_EDGE ( 'NONE', *, *, #76250, .T. ) ;
#18859 = ORIENTED_EDGE ( 'NONE', *, *, #81367, .F. ) ;
#18860 = CARTESIAN_POINT ( 'NONE',  ( 52.27629109544965758, -56.83866631114189971, 61.26715463662765870 ) ) ;
#18861 = CARTESIAN_POINT ( 'NONE',  ( -46.00000000000000000, 436.0273486662516689, 12.60673985408120323 ) ) ;
#18862 = EDGE_CURVE ( 'NONE', #87871, #101395, #69503, .T. ) ;
#18863 = CARTESIAN_POINT ( 'NONE',  ( -5.500000000000007994, 42.00000000000000000, -70.16688272716517361 ) ) ;
#18864 = EDGE_LOOP ( 'NONE', ( #2040, #102228, #106497, #2757 ) ) ;
#18865 = CARTESIAN_POINT ( 'NONE',  ( -85.43365283625350060, -38.35985798731113050, -22.44808446743328290 ) ) ;
#18866 = AXIS2_PLACEMENT_3D ( 'NONE', #55127, #29320, #46004 ) ;
#18867 = ORIENTED_EDGE ( 'NONE', *, *, #76842, .F. ) ;
#18868 = CARTESIAN_POINT ( 'NONE',  ( 3.313708498984753170, -29.46875000409677980, 8.000000000000008882 ) ) ;
#18869 = CARTESIAN_POINT ( 'NONE',  ( 106.8967157683483720, -38.36539324343537061, 195.0206876434428409 ) ) ;
#18870 = CARTESIAN_POINT ( 'NONE',  ( 13.42061381376756835, 24.46452927392946464, -2.387491988728646763 ) ) ;
#18871 = CARTESIAN_POINT ( 'NONE',  ( 86.56679986176000341, -60.14582403643369446, 24.17458394031839930 ) ) ;
#18872 = DIRECTION ( 'NONE',  ( 0.000000000000000000, 1.000000000000000000, 0.000000000000000000 ) ) ;
#18873 = CARTESIAN_POINT ( 'NONE',  ( -21.91220694774618849, 304.0706505179387023, -9.953496567762948999 ) ) ;
#18874 = DIRECTION ( 'NONE',  ( 0.000000000000000000, -1.000000000000000000, 0.000000000000000000 ) ) ;
#18875 = EDGE_CURVE ( 'NONE', #35853, #65774, #79797, .T. ) ;
#18876 = AXIS2_PLACEMENT_3D ( 'NONE', #39977, #31900, #65312 ) ;
#18877 = CARTESIAN_POINT ( 'NONE',  ( 105.5353273971932140, 1.030564683017419500E-14, 0.000000000000000000 ) ) ;
#18878 = CARTESIAN_POINT ( 'NONE',  ( 6.936184427528457874, 1.053834543709838281E-15, 8.605212085995399107 ) ) ;
#18879 = CARTESIAN_POINT ( 'NONE',  ( 2.849089834145952516, 81.66538534281866646, 5.000000000000000000 ) ) ;
#18880 = ORIENTED_EDGE ( 'NONE', *, *, #91198, .F. ) ;
#18881 = ADVANCED_FACE ( 'NONE', ( #25130 ), #85168, .F. ) ;
#18882 = CARTESIAN_POINT ( 'NONE',  ( 0.6452391198540656791, 36.35841920418370421, 29.58352460202021206 ) ) ;
#18883 = DIRECTION ( 'NONE',  ( 0.000000000000000000, -1.000000000000000000, 0.000000000000000000 ) ) ;
#18884 = ORIENTED_EDGE ( 'NONE', *, *, #106116, .F. ) ;
#18885 = CARTESIAN_POINT ( 'NONE',  ( -4.205728106920963327, 53.86358984174591313, 7.922788842214678162 ) ) ;
#18886 = CARTESIAN_POINT ( 'NONE',  ( -28.87333700207125986, 311.5295170219202419, 12.02128803619848263 ) ) ;
#18887 = DIRECTION ( 'NONE',  ( 0.000000000000000000, -1.000000000000000000, 0.000000000000000000 ) ) ;
#18888 = CARTESIAN_POINT ( 'NONE',  ( 0.000000000000000000, -80.00000000000000000, 27.00000000000000000 ) ) ;
#18889 = CARTESIAN_POINT ( 'NONE',  ( -3.313708498984760720, -30.03124999999999645, -8.000000000000000000 ) ) ;
#18890 =( GEOMETRIC_REPRESENTATION_CONTEXT ( 3 ) GLOBAL_UNCERTAINTY_ASSIGNED_CONTEXT ( ( #48500 ) ) GLOBAL_UNIT_ASSIGNED_CONTEXT ( ( #82929, #80796, #37872 ) ) REPRESENTATION_CONTEXT ( 'NONE', 'WORKASPACE' ) );
#18891 = EDGE_CURVE ( 'NONE', #8366, #101089, #19582, .T. ) ;
#18892 = PRESENTATION_LAYER_ASSIGNMENT (  '', '', ( #89460 ) ) ;
#18893 = CIRCLE ( 'NONE', #11919, 5.000000000000002665 ) ;
#18894 = CARTESIAN_POINT ( 'NONE',  ( 49.01201108414410612, 48.00000000000000000, 43.00492839360018849 ) ) ;
#18895 = VERTEX_POINT ( 'NONE', #71391 ) ;
#18896 = CARTESIAN_POINT ( 'NONE',  ( 81.41390920051752289, -60.59005278335753530, 185.5272298782579128 ) ) ;
#18897 = CARTESIAN_POINT ( 'NONE',  ( -15.45347762069378383, 46.21495662470459820, 5.015962831654086074 ) ) ;
#18898 = EDGE_LOOP ( 'NONE', ( #34128, #37497 ) ) ;
#18899 = CARTESIAN_POINT ( 'NONE',  ( -86.56297675702614924, -52.70887369560592361, 37.65507028047760940 ) ) ;
#18900 = CARTESIAN_POINT ( 'NONE',  ( -32.95589646111152149, 464.8957215206404499, 10.75300444715534987 ) ) ;
#18901 = DIRECTION ( 'NONE',  ( -1.000000000000000000, 0.000000000000000000, 1.096832036894112098E-16 ) ) ;
#18902 = CARTESIAN_POINT ( 'NONE',  ( 13.16264097910227981, 304.5561373339386932, 8.874147965172166863 ) ) ;
#18903 = CARTESIAN_POINT ( 'NONE',  ( -22.71182892702813660, -26.84646812124476156, -38.43211124454622762 ) ) ;
#18904 = EDGE_CURVE ( 'NONE', #99736, #8297, #16120, .T. ) ;
#18905 =( NAMED_UNIT ( * ) PLANE_ANGLE_UNIT ( ) SI_UNIT ( $, .RADIAN. ) );
#18906 = CIRCLE ( 'NONE', #3388, 5.000000000000010658 ) ;
#18907 = CARTESIAN_POINT ( 'NONE',  ( 41.69006022411431189, -59.99999999999999289, 54.65678614846827088 ) ) ;
#18908 = CONICAL_SURFACE ( 'NONE', #80916, 3.309500000000001663, 0.9599310885968770357 ) ;
#18909 = CARTESIAN_POINT ( 'NONE',  ( 25.87313031554646514, -29.63673128196639084, 38.60121535671525095 ) ) ;
#18910 = CARTESIAN_POINT ( 'NONE',  ( -30.00000000000000000, -54.00000000000000711, 27.11721482942554928 ) ) ;
#18911 = DIRECTION ( 'NONE',  ( 0.000000000000000000, 0.000000000000000000, 1.000000000000000000 ) ) ;
#18914 = VECTOR ( 'NONE', #76653, 1000.000000000000000 ) ;
#18913 = CARTESIAN_POINT ( 'NONE',  ( -11.82957429177135289, 21.33083118278957713, -7.415650228056600568 ) ) ;
#18912 = CARTESIAN_POINT ( 'NONE',  ( -29.99396172607142574, -32.44667869317692777, 40.57082760664052756 ) ) ;
#18915 = B_SPLINE_CURVE_WITH_KNOTS ( 'NONE', 3,
 ( #97125, #54523, #15147, #96081 ),
 .UNSPECIFIED., .F., .F.,
 ( 4, 4 ),
 ( 0.0007388461703411279557, 0.02697940549969501944 ),
 .UNSPECIFIED. ) ;
#18916 = CARTESIAN_POINT ( 'NONE',  ( 0.5082004253310246078, 295.8543628272474280, -10.00017741440575669 ) ) ;
#18917 = CARTESIAN_POINT ( 'NONE',  ( 35.76379064120181539, 307.0162303970107587, 12.81051142610679960 ) ) ;
#18918 = FACE_BOUND ( 'NONE', #1463, .T. ) ;
#18919 = DIRECTION ( 'NONE',  ( 0.000000000000000000, 1.000000000000000000, 0.000000000000000000 ) ) ;
#18920 = CIRCLE ( 'NONE', #8546, 5.000000000000010658 ) ;
#18921 = VERTEX_POINT ( 'NONE', #105883 ) ;
#18922 = DIRECTION ( 'NONE',  ( -0.5735764363510510444, -0.8191520442889883569, 0.000000000000000000 ) ) ;
#18923 = FACE_OUTER_BOUND ( 'NONE', #17279, .T. ) ;
#18924 = FACE_OUTER_BOUND ( 'NONE', #80716, .T. ) ;
#18925 = FACE_OUTER_BOUND ( 'NONE', #71968, .T. ) ;
#18926 = EDGE_CURVE ( 'NONE', #105869, #81361, #24775, .T. ) ;
#18928 = CARTESIAN_POINT ( 'NONE',  ( 15.77584606617254614, -34.58953296166827585, -32.12825160005380098 ) ) ;
#18927 = CARTESIAN_POINT ( 'NONE',  ( 9.253817200599849357, 251.2999272991685586, -3.791916801615176080 ) ) ;
#18929 = ORIENTED_EDGE ( 'NONE', *, *, #32172, .T. ) ;
#18930 = PRESENTATION_LAYER_ASSIGNMENT (  '', '', ( #80935 ) ) ;
#18931 = CARTESIAN_POINT ( 'NONE',  ( 9.881544152755356691, 294.6462802181998200, 1.569702982030937610 ) ) ;
#18932 = CARTESIAN_POINT ( 'NONE',  ( -43.47539510892337944, 487.0683238468439527, 3.561594968384696802 ) ) ;
#18933 = ORIENTED_EDGE ( 'NONE', *, *, #37057, .F. ) ;
#18934 = EDGE_CURVE ( 'NONE', #103450, #48691, #59191, .T. ) ;
#18935 = DIRECTION ( 'NONE',  ( 0.000000000000000000, -1.000000000000000000, -0.000000000000000000 ) ) ;
#18936 = FACE_OUTER_BOUND ( 'NONE', #20170, .T. ) ;
#18937 = CONICAL_SURFACE ( 'NONE', #96445, 45.10524579772351217, 0.3972631705159501148 ) ;
#18938 = LINE ( 'NONE', #51236, #39036 ) ;
#18939 = CARTESIAN_POINT ( 'NONE',  ( -92.23598523486838019, -60.00000000000001421, 2.395111321838569118 ) ) ;
#18940 = CARTESIAN_POINT ( 'NONE',  ( -34.16642289233710983, 463.8422268500497125, 18.98106911353875148 ) ) ;
#18941 = CARTESIAN_POINT ( 'NONE',  ( 35.59667163540026280, 463.9592197885497171, -0.04846191499040426731 ) ) ;
#18942 = CARTESIAN_POINT ( 'NONE',  ( 39.17204790861331531, 459.8623611124623949, 1.900463024344650087 ) ) ;
#18944 = CARTESIAN_POINT ( 'NONE',  ( 38.86638200451619696, 1.340359594676612611E-15, 0.000000000000000000 ) ) ;
#18943 = CARTESIAN_POINT ( 'NONE',  ( 6.145467200819017428, -3.000000000000002665, -77.00333157708807619 ) ) ;
#18945 = STYLED_ITEM ( 'NONE', ( #35515 ), #69567 ) ;
#18946 = CARTESIAN_POINT ( 'NONE',  ( -81.53213380329533777, -53.46540947967974233, 178.0948321718499017 ) ) ;
#18947 = EDGE_LOOP ( 'NONE', ( #18972, #96319, #12033, #18636, #51189 ) ) ;
#18948 = SURFACE_STYLE_FILL_AREA ( #100873 ) ;
#18949 = EDGE_CURVE ( 'NONE', #12439, #17653, #44340, .T. ) ;
#18950 = ORIENTED_EDGE ( 'NONE', *, *, #88246, .F. ) ;
#18951 = ORIENTED_EDGE ( 'NONE', *, *, #1900, .T. ) ;
#18952 = CARTESIAN_POINT ( 'NONE',  ( -19.53131398207814939, 303.7300551578738919, -10.02587845849555492 ) ) ;
#18953 = CARTESIAN_POINT ( 'NONE',  ( 7.811152745362717198, -4.332661967060489339, -16.03212449091516945 ) ) ;
#18954 = DIRECTION ( 'NONE',  ( 0.000000000000000000, -1.000000000000000000, 0.000000000000000000 ) ) ;
#18955 = ORIENTED_EDGE ( 'NONE', *, *, #56125, .T. ) ;
#18956 = CARTESIAN_POINT ( 'NONE',  ( 0.000000000000000000, -30.00000000000000000, 8.000000000000000000 ) ) ;
#18957 = CARTESIAN_POINT ( 'NONE',  ( 2.435348425596516081E-07, -57.67120202539301488, -44.61186700419774098 ) ) ;
#18958 = CARTESIAN_POINT ( 'NONE',  ( 7.150931910075644105, -11.78625798522264390, -3.588457848165354402 ) ) ;
#18959 = CARTESIAN_POINT ( 'NONE',  ( -7.897196874019790869, -61.20872795832194413, -1.302055520192090476 ) ) ;
#18960 = CYLINDRICAL_SURFACE ( 'NONE', #6632, 4.000000000000000888 ) ;
#18961 = CARTESIAN_POINT ( 'NONE',  ( 0.000000000000000000, 30.00000000000000000, 0.000000000000000000 ) ) ;
#18962 = FACE_OUTER_BOUND ( 'NONE', #24028, .T. ) ;
#18963 = CARTESIAN_POINT ( 'NONE',  ( 97.37780541404315215, -14.21045842199443143, 96.97658560636448044 ) ) ;
#18964 = CARTESIAN_POINT ( 'NONE',  ( -75.52856519143354319, -59.99999999999994316, 193.8568173627997737 ) ) ;
#18965 = CARTESIAN_POINT ( 'NONE',  ( -60.37025287372667748, -29.06875052076281563, 68.28797770161614267 ) ) ;
#18966 = ORIENTED_EDGE ( 'NONE', *, *, #39887, .F. ) ;
#18967 = CYLINDRICAL_SURFACE ( 'NONE', #2392, 1.250000000000001110 ) ;
#18968 = ORIENTED_EDGE ( 'NONE', *, *, #4409, .T. ) ;
#18969 = CARTESIAN_POINT ( 'NONE',  ( -106.0471509648365043, -60.15506806661914396, 181.9131953650650360 ) ) ;
#18970 = DIRECTION ( 'NONE',  ( 1.000000000000000000, 0.000000000000000000, 0.000000000000000000 ) ) ;
#18971 = DIRECTION ( 'NONE',  ( -1.000000000000000000, -1.224606353822377258E-16, -0.000000000000000000 ) ) ;
#18972 = ORIENTED_EDGE ( 'NONE', *, *, #10494, .F. ) ;
#18973 = CARTESIAN_POINT ( 'NONE',  ( 19.49977600865978289, 50.00000000000003553, 59.92175665475047452 ) ) ;
#18974 = CARTESIAN_POINT ( 'NONE',  ( -48.42784265545724764, -59.99999999999998579, 67.95292345526354438 ) ) ;
#18975 = CARTESIAN_POINT ( 'NONE',  ( -5.000000000000000888, 6.123233995736767268E-16, -10.00000000000000000 ) ) ;
#18976 = CARTESIAN_POINT ( 'NONE',  ( 4.401442555609581635E-16, -22.15625000204838457, -7.188101187500000044 ) ) ;
#18977 = CARTESIAN_POINT ( 'NONE',  ( -0.7864879193441504102, 36.39291929247367818, -29.48511154656912936 ) ) ;
#18978 = CYLINDRICAL_SURFACE ( 'NONE', #94289, 1.250000000000001110 ) ;
#18979 = CARTESIAN_POINT ( 'NONE',  ( 16.90642566761063748, 0.000000000000000000, -2.220638482676887460 ) ) ;
#18980 = CARTESIAN_POINT ( 'NONE',  ( 103.5111111111111057, 1.023464760207051730E-14, 0.000000000000000000 ) ) ;
#18981 = CARTESIAN_POINT ( 'NONE',  ( 0.000000000000000000, 0.000000000000000000, 0.000000000000000000 ) ) ;
#18982 = CARTESIAN_POINT ( 'NONE',  ( -16.48315964343910167, 45.94107222901597964, -4.157797401561528439 ) ) ;
#18983 = ADVANCED_FACE ( 'NONE', ( #5432 ), #60884, .T. ) ;
#18984 = CARTESIAN_POINT ( 'NONE',  ( 0.000000000000000000, -50.00000000000000000, 27.00000000000000000 ) ) ;
#18985 = UNCERTAINTY_MEASURE_WITH_UNIT (LENGTH_MEASURE( 1.000000000000000082E-05 ), #16984, 'distance_accuracy_value', 'NONE');
#18986 = B_SPLINE_CURVE_WITH_KNOTS ( 'NONE', 3,
 ( #104665, #45389, #30817, #36793, #69660, #61583, #94475, #20633, #53473, #86393, #78270, #4382 ),
 .UNSPECIFIED., .F., .F.,
 ( 4, 2, 2, 2, 2, 4 ),
 ( 2.255140518769849223E-17, 0.001518988062909442825, 0.002278482094364125531, 0.003037976125818808455, 0.004556964188728219838, 0.006075952251637632522 ),
 .UNSPECIFIED. ) ;
#18987 = CARTESIAN_POINT ( 'NONE',  ( -29.28896430935111184, -29.06400796251119445, 31.04148615219279250 ) ) ;
#18988 = CIRCLE ( 'NONE', #13770, 8.000000000000000000 ) ;
#18989 = CARTESIAN_POINT ( 'NONE',  ( 3.972708858246882357, 18.38910731443329638, 5.763820867899048572 ) ) ;
#18990 = UNCERTAINTY_MEASURE_WITH_UNIT (LENGTH_MEASURE( 1.000000000000000082E-05 ), #69023, 'distance_accuracy_value', 'NONE');
#18991 = CARTESIAN_POINT ( 'NONE',  ( 45.59211296353198861, -46.43827376306629162, 46.30565985479245228 ) ) ;
#18992 = CARTESIAN_POINT ( 'NONE',  ( 5.947762761376478302, 6.880090707843046438, 1.083333333333333481 ) ) ;
#18993 = EDGE_CURVE ( 'NONE', #88199, #60134, #12652, .T. ) ;
#18994 = CARTESIAN_POINT ( 'NONE',  ( -1.093451710897897389, 45.52449153923928549, 18.11105145254594007 ) ) ;
#18995 = VECTOR ( 'NONE', #81330, 1000.000000000000000 ) ;
#18996 = CARTESIAN_POINT ( 'NONE',  ( -97.05521031604199322, -38.48254110268376849, 201.1230655224092629 ) ) ;
#18997 = ORIENTED_EDGE ( 'NONE', *, *, #47328, .T. ) ;
#18999 = CARTESIAN_POINT ( 'NONE',  ( -28.35333406767821884, 36.33371803105157483, 8.700175216043216864 ) ) ;
#18998 = CARTESIAN_POINT ( 'NONE',  ( -16.11142072793864699, 21.68022463236556163, 1.737955725777517779 ) ) ;
#19000 = CARTESIAN_POINT ( 'NONE',  ( 74.61050274188295361, -60.00000000000002132, 134.6572766532755452 ) ) ;
#19001 = CARTESIAN_POINT ( 'NONE',  ( -48.15042790184227073, 11.33351092753205336, -14.35535821593460071 ) ) ;
#19002 = FACE_OUTER_BOUND ( 'NONE', #26650, .T. ) ;
#19003 = CARTESIAN_POINT ( 'NONE',  ( 9.981544566921639827, 15.23274035658502079, -0.7016502453917061732 ) ) ;
#19004 = DIRECTION ( 'NONE',  ( 0.000000000000000000, 1.000000000000000000, 0.000000000000000000 ) ) ;
#19005 = CARTESIAN_POINT ( 'NONE',  ( -19.73463816634111012, 304.7971333121958537, 8.925379062039116462 ) ) ;
#19006 = DIRECTION ( 'NONE',  ( 0.000000000000000000, -1.000000000000000000, 0.000000000000000000 ) ) ;
#19007 = CARTESIAN_POINT ( 'NONE',  ( 112.1757562388903722, -59.99999999999998579, 169.0180869050140302 ) ) ;
#19008 = CARTESIAN_POINT ( 'NONE',  ( 6.289692432696817548, -6.589071317540659223, 2.245373559999283231 ) ) ;
#19009 = COLOUR_RGB ( '', 0.72549020, 0.75294118, 0.79215686) ;
#19010 = B_SPLINE_CURVE_WITH_KNOTS ( 'NONE', 3,
 ( #20345, #11644, #45111, #43501, #12705, #61284, #53191, #20875, #86108, #28961 ),
 .UNSPECIFIED., .F., .F.,
 ( 4, 2, 2, 2, 4 ),
 ( -2.000195913693527015E-05, 0.001085800244612924580, 0.002191602448362784360, 0.003297404652112644139, 0.004403206855862503918 ),
 .UNSPECIFIED. ) ;
#19011 = LINE ( 'NONE', #101482, #25028 ) ;
#19012 = VERTEX_POINT ( 'NONE', #87948 ) ;
#19013 = ADVANCED_FACE ( 'NONE', ( #78252 ), #103071, .T. ) ;
#19014 = CARTESIAN_POINT ( 'NONE',  ( 1.257641187044677311, -49.99999999632648695, 101.3278948775254094 ) ) ;
#19015 = CARTESIAN_POINT ( 'NONE',  ( -80.36397934127951714, -30.00000000000006040, -13.26667358045050271 ) ) ;
#19016 = ORIENTED_EDGE ( 'NONE', *, *, #33459, .F. ) ;
#19017 = CIRCLE ( 'NONE', #99948, 5.000000000000000000 ) ;
#19019 = CARTESIAN_POINT ( 'NONE',  ( 43.04469050570450150, 434.7734435962914290, 9.248231035223298591 ) ) ;
#19018 = CARTESIAN_POINT ( 'NONE',  ( -80.12540570148722452, -38.79873096281602329, 193.2784058327983416 ) ) ;
#19020 = CARTESIAN_POINT ( 'NONE',  ( 43.71037717921926458, 462.3391554988761527, 4.824299547763559737 ) ) ;
#19021 = CARTESIAN_POINT ( 'NONE',  ( 22.71376002812208839, 304.4529191814661431, 10.06675239557364065 ) ) ;
#19022 = CARTESIAN_POINT ( 'NONE',  ( 13.86650669486618881, -3.999999999999998224, 0.000000000000000000 ) ) ;
#19023 = CARTESIAN_POINT ( 'NONE',  ( -7.188101187500000044, -17.28125000204838813, -8.802885111219163269E-16 ) ) ;
#19024 = CARTESIAN_POINT ( 'NONE',  ( -11.68767211932356531, -5.000000000000002665, -81.85902538601600043 ) ) ;
#19025 = CIRCLE ( 'NONE', #67271, 4.000000000000001776 ) ;
#19026 = UNCERTAINTY_MEASURE_WITH_UNIT (LENGTH_MEASURE( 1.000000000000000082E-05 ), #30713, 'distance_accuracy_value', 'NONE');
#19027 = CARTESIAN_POINT ( 'NONE',  ( 30.93146042459050804, 14.42085588385340778, -40.69811146320466833 ) ) ;
#19029 = EDGE_LOOP ( 'NONE', ( #57133, #55745, #80034 ) ) ;
#19028 = SURFACE_SIDE_STYLE ('',( #91815 ) ) ;
#19030 = CARTESIAN_POINT ( 'NONE',  ( 82.39744891461782572, -39.49350758968277830, 164.1889903970027262 ) ) ;
#19031 = CIRCLE ( 'NONE', #94770, 10.00000000000003730 ) ;
#19032 = CARTESIAN_POINT ( 'NONE',  ( -4.551587301587303180, -1.200583151104949176, 104.4018401814738155 ) ) ;
#19033 = FACE_OUTER_BOUND ( 'NONE', #103270, .T. ) ;
#19034 = VERTEX_POINT ( 'NONE', #12443 ) ;
#19035 = CARTESIAN_POINT ( 'NONE',  ( -32.15166163075724626, 486.0589784586661040, 5.199393881400821371 ) ) ;
#19036 = CARTESIAN_POINT ( 'NONE',  ( -47.78396355473400803, 15.50490861890658323, 16.83695313132053428 ) ) ;
#19037 = CARTESIAN_POINT ( 'NONE',  ( 1.429841143546225365E-15, 35.00000000000000000, 11.18527996897366528 ) ) ;
#19038 = CARTESIAN_POINT ( 'NONE',  ( 33.86650669486618881, -3.999999999999998224, 0.000000000000000000 ) ) ;
#19039 = CARTESIAN_POINT ( 'NONE',  ( -5.999787407977320797, 253.9996811118444668, 0.2740427891042886976 ) ) ;
#19040 = CARTESIAN_POINT ( 'NONE',  ( 1.107728337459903178, 17.28511502408344214, 49.90434249749426954 ) ) ;
#19041 = CARTESIAN_POINT ( 'NONE',  ( 10.59869873574526267, 2.545575842793166732, 14.78270473238058891 ) ) ;
#19042 = ORIENTED_EDGE ( 'NONE', *, *, #37624, .T. ) ;
#19043 = SURFACE_SIDE_STYLE ('',( #50810 ) ) ;
#19044 = LINE ( 'NONE', #92878, #90542 ) ;
#19045 = CIRCLE ( 'NONE', #72344, 3.309500000000001663 ) ;
#19046 = CARTESIAN_POINT ( 'NONE',  ( 87.13380744255303512, -42.76071740017988532, 190.1415511809839245 ) ) ;
#19047 = CARTESIAN_POINT ( 'NONE',  ( 18.09999999999999787, -3.309499999999999886, 0.000000000000000000 ) ) ;
#19048 = CARTESIAN_POINT ( 'NONE',  ( -5.082755093536326818, -24.21875000204838813, 5.082755093536325042 ) ) ;
#19049 = CARTESIAN_POINT ( 'NONE',  ( -42.08762648273019380, 487.0030674539067945, 9.106351919860287580 ) ) ;
#19050 = DIRECTION ( 'NONE',  ( 1.000000000000000000, 0.000000000000000000, 0.000000000000000000 ) ) ;
#19051 = DIRECTION ( 'NONE',  ( 0.000000000000000000, 0.000000000000000000, 1.000000000000000000 ) ) ;
#19052 = ORIENTED_EDGE ( 'NONE', *, *, #47504, .T. ) ;
#19053 = CARTESIAN_POINT ( 'NONE',  ( 4.250000000000000000, 0.000000000000000000, -6.606815774914157835 ) ) ;
#19054 = DIRECTION ( 'NONE',  ( 0.000000000000000000, 1.000000000000000000, 0.000000000000000000 ) ) ;
#19055 = CARTESIAN_POINT ( 'NONE',  ( -6.232788007775230454, 4.162902319565254139, -5.000000000000000000 ) ) ;
#19056 =( BOUNDED_SURFACE ( )  B_SPLINE_SURFACE ( 3, 2, ( 
 ( #13455, #70653, #46892 ),
 ( #45849, #21084, #30752 ),
 ( #39879, #88958, #13987 ),
 ( #72239, #78722, #5895 ) ),
 .UNSPECIFIED., .F., .F., .F. ) 
 B_SPLINE_SURFACE_WITH_KNOTS ( ( 4, 4 ),
 ( 3, 3 ),
 ( 0.1191486731993773723, 0.1451922720400707911 ),
 ( 0.000000000000000000, 0.6299180599692617566 ),
 .UNSPECIFIED. ) 
 GEOMETRIC_REPRESENTATION_ITEM ( )  RATIONAL_B_SPLINE_SURFACE ( (
 ( 1.000000000000000000, 0.8155016339198950526, 0.8634409734971468797),
 ( 1.000000000000000000, 0.8155019444343304391, 0.8634412033287162114),
 ( 1.000000000000000000, 0.8155018689791531106, 0.8634411474795193886),
 ( 1.000000000000000000, 0.8155015613424223542, 0.8634409197779229217) ) ) 
 REPRESENTATION_ITEM ( '' )  SURFACE ( )  );
#19057 = FACE_OUTER_BOUND ( 'NONE', #95103, .T. ) ;
#19058 = ADVANCED_FACE ( 'NONE', ( #37302 ), #55677, .T. ) ;
#19059 = ADVANCED_BREP_SHAPE_REPRESENTATION ( '', ( #51736, #10728 ), #21183 ) ;
#19060 = CONICAL_SURFACE ( 'NONE', #51727, 3.309500000000001663, 0.9599310885968770357 ) ;
#19061 = ORIENTED_EDGE ( 'NONE', *, *, #71525, .F. ) ;
#19062 = CARTESIAN_POINT ( 'NONE',  ( 34.86931356687689032, 472.8464800566460440, 16.94524670509526132 ) ) ;
#19063 = CARTESIAN_POINT ( 'NONE',  ( 4.707696486723893514, 49.99999999999999289, -99.43546650846349166 ) ) ;
#19064 = VERTEX_POINT ( 'NONE', #62101 ) ;
#19065 = EDGE_CURVE ( 'NONE', #81772, #2138, #86284, .T. ) ;
#19066 = EDGE_CURVE ( 'NONE', #10651, #36077, #95451, .T. ) ;
#19067 = CARTESIAN_POINT ( 'NONE',  ( 31.55511120193260055, 436.6792952284608873, 19.27130410701429852 ) ) ;
#19068 = CARTESIAN_POINT ( 'NONE',  ( -0.9537700198956184927, 8.769399064309570946, -51.31178202143230749 ) ) ;
#19069 = LINE ( 'NONE', #10903, #1025 ) ;
#19070 = CARTESIAN_POINT ( 'NONE',  ( -17.08200492518427183, 36.32755554593312297, 24.26548702208081565 ) ) ;
#19071 = CARTESIAN_POINT ( 'NONE',  ( -111.0088745510421262, -60.00000000000000000, 187.2406379443718833 ) ) ;
#19072 = CARTESIAN_POINT ( 'NONE',  ( -45.49982102694234953, 388.3127959276886827, 7.886590035822850453 ) ) ;
#19073 = SURFACE_SIDE_STYLE ('',( #69192 ) ) ;
#19074 = DIRECTION ( 'NONE',  ( 0.8191520442889974607, 1.003171929053531649E-16, -0.5735764363510380548 ) ) ;
#19075 = CARTESIAN_POINT ( 'NONE',  ( -85.67509731226019198, -28.57511156689592724, 179.3357466346379852 ) ) ;
#19076 = CARTESIAN_POINT ( 'NONE',  ( 0.000000000000000000, 0.5000000000000000000, 0.000000000000000000 ) ) ;
#19078 = ADVANCED_FACE ( 'NONE', ( #61518 ), #3658, .T. ) ;
#19077 = AXIS2_PLACEMENT_3D ( 'NONE', #68736, #50385, #10990 ) ;
#19079 = ORIENTED_EDGE ( 'NONE', *, *, #79075, .F. ) ;
#19080 = CARTESIAN_POINT ( 'NONE',  ( 5.656854249492380582, -25.81249999999999645, -5.656854249492379694 ) ) ;
#19081 = CARTESIAN_POINT ( 'NONE',  ( 41.08349330513380693, 1.593028355512270567E-15, 0.000000000000000000 ) ) ;
#19082 = CARTESIAN_POINT ( 'NONE',  ( -85.20477662574127464, -52.70491138971408418, 3.232116785323828623 ) ) ;
#19083 = AXIS2_PLACEMENT_3D ( 'NONE', #7979, #40891, #73777 ) ;
#19084 =( NAMED_UNIT ( * ) SI_UNIT ( $, .STERADIAN. ) SOLID_ANGLE_UNIT ( ) );
#19085 = CARTESIAN_POINT ( 'NONE',  ( 0.000000000000000000, 45.00000000000000711, 57.21727615095610275 ) ) ;
#19086 = DIRECTION ( 'NONE',  ( 1.000000000000000000, 0.000000000000000000, 0.000000000000000000 ) ) ;
#19087 = DIRECTION ( 'NONE',  ( -1.000000000000000000, -0.000000000000000000, -0.000000000000000000 ) ) ;
#19088 = CARTESIAN_POINT ( 'NONE',  ( 23.70422451876635250, 42.00000000000004263, -88.20421627930062414 ) ) ;
#19089 = CARTESIAN_POINT ( 'NONE',  ( 57.26188992556405566, -30.00000000000000355, 83.64747613098029433 ) ) ;
#19090 = VECTOR ( 'NONE', #14055, 1000.000000000000000 ) ;
#19091 = CARTESIAN_POINT ( 'NONE',  ( -85.55948822751662419, -29.99999999999991829, -20.40846083852196813 ) ) ;
#19092 = CARTESIAN_POINT ( 'NONE',  ( -72.46402628313448702, -18.64347544987403182, 97.55464540977230570 ) ) ;
#19093 = ORIENTED_EDGE ( 'NONE', *, *, #44441, .T. ) ;
#19094 = CARTESIAN_POINT ( 'NONE',  ( 100.7999351731576354, -29.99999999999990763, 198.8735152728553999 ) ) ;
#19095 = CARTESIAN_POINT ( 'NONE',  ( 64.56046279400122501, 40.83886016323774726, -8.108302868572121014 ) ) ;
#19096 = CARTESIAN_POINT ( 'NONE',  ( 38.84142322586829721, -60.00000000000980549, 54.50522279198219167 ) ) ;
#19097 = ORIENTED_EDGE ( 'NONE', *, *, #71252, .T. ) ;
#19098 = CARTESIAN_POINT ( 'NONE',  ( 13.51445589115056833, -9.121446783585646756, 11.91887821639477707 ) ) ;
#19099 = CARTESIAN_POINT ( 'NONE',  ( -2.977408999572650039, -28.06250000204838813, -7.188101187500000933 ) ) ;
#19100 = AXIS2_PLACEMENT_3D ( 'NONE', #30205, #23174, #97551 ) ;
#19101 = FACE_OUTER_BOUND ( 'NONE', #17589, .T. ) ;
#19102 = VERTEX_POINT ( 'NONE', #93868 ) ;
#19103 = PRODUCT ( '1. Base', '1. Base', '', ( #74044 ) ) ;
#19104 = DIRECTION ( 'NONE',  ( 0.000000000000000000, -1.000000000000000000, 0.000000000000000000 ) ) ;
#19105 = ORIENTED_EDGE ( 'NONE', *, *, #59012, .F. ) ;
#19106 = CARTESIAN_POINT ( 'NONE',  ( -8.087340429040079215, 41.99999999999999289, -69.98180430517560069 ) ) ;
#19107 =( NAMED_UNIT ( * ) PLANE_ANGLE_UNIT ( ) SI_UNIT ( $, .RADIAN. ) );
#19108 = CARTESIAN_POINT ( 'NONE',  ( -36.33885736213258610, -59.99999999999506173, 51.14030269516670302 ) ) ;
#19109 = CARTESIAN_POINT ( 'NONE',  ( 33.09767504420651818, 317.8536043559706741, -6.616321532221737911 ) ) ;
#19110 = CARTESIAN_POINT ( 'NONE',  ( 7.188101187499999156, -13.25000000204838280, 2.977408999572654924 ) ) ;
#19111 = CARTESIAN_POINT ( 'NONE',  ( 4.898587196589412829E-16, -18.31250000409676915, -8.000000000000000000 ) ) ;
#19112 = CARTESIAN_POINT ( 'NONE',  ( 23.09999999999999432, 3.309500000000003439, 4.052968581778167743E-16 ) ) ;
#19113 = PRESENTATION_STYLE_ASSIGNMENT (( #35823 ) ) ;
#19114 = CARTESIAN_POINT ( 'NONE',  ( 1.224646799147352073E-15, 49.99999999999999289, -75.00000000000001421 ) ) ;
#19115 = CARTESIAN_POINT ( 'NONE',  ( 15.05785784214676326, 3.824195276769950969, 4.604276673498415740 ) ) ;
#19116 = CARTESIAN_POINT ( 'NONE',  ( 40.95645226493660118, 436.0015890305569428, 6.362679593776062070 ) ) ;
#19117 = ADVANCED_FACE ( 'NONE', ( #20027 ), #75938, .T. ) ;
#19118 = EDGE_LOOP ( 'NONE', ( #84459, #65015, #48206, #56433 ) ) ;
#19119 = CARTESIAN_POINT ( 'NONE',  ( 5.000000000092883035, -3.772466818847466818, 103.2791840072271015 ) ) ;
#19121 = CARTESIAN_POINT ( 'NONE',  ( 33.60426306485480552, -53.36599767116988602, 37.21245143418115475 ) ) ;
#19120 = CARTESIAN_POINT ( 'NONE',  ( -3.841398122528037806, -48.92777529680780901, 104.5835869663331295 ) ) ;
#19122 = CONICAL_SURFACE ( 'NONE', #95, 4.000000000000002665, 0.9599310885968824758 ) ;
#19123 = CARTESIAN_POINT ( 'NONE',  ( 12.70248734011628500, -4.285714285714347760, 22.03900363279280583 ) ) ;
#19124 = VERTEX_POINT ( 'NONE', #30207 ) ;
#19125 = ADVANCED_FACE ( 'NONE', ( #70119 ), #74234, .T. ) ;
#19126 = ADVANCED_FACE ( 'NONE', ( #44257 ), #32933, .T. ) ;
#19127 = FACE_OUTER_BOUND ( 'NONE', #72231, .T. ) ;
#19128 = COLOUR_RGB ( '', 0.09019608, 0.27058824, 0.51372549) ;
#19129 = VERTEX_POINT ( 'NONE', #69599 ) ;
#19131 = DIRECTION ( 'NONE',  ( 0.000000000000000000, -0.9540597841379402366, 0.2996163017772344728 ) ) ;
#19130 = CARTESIAN_POINT ( 'NONE',  ( 0.000000000000000000, 0.000000000000000000, 0.000000000000000000 ) ) ;
#19132 = CARTESIAN_POINT ( 'NONE',  ( 11.72694920408448560, 302.5954528286877689, -10.05449594607857655 ) ) ;
#19133 = CARTESIAN_POINT ( 'NONE',  ( 3.313708498984762496, -23.46875000409677980, 7.999999999999998224 ) ) ;
#19134 = CARTESIAN_POINT ( 'NONE',  ( 34.83349330513379982, 1.593028355512270567E-15, 0.000000000000000000 ) ) ;
#19135 = CARTESIAN_POINT ( 'NONE',  ( 0.7145311798163271888, -9.237604307034018802, 8.246630900752838649E-17 ) ) ;
#19136 = ORIENTED_EDGE ( 'NONE', *, *, #98957, .F. ) ;
#19137 = CARTESIAN_POINT ( 'NONE',  ( 92.56598272418166573, -60.00000000000000000, -2.244544293399764356 ) ) ;
#19138 = SURFACE_STYLE_USAGE ( .BOTH. , #20747 ) ;
#19139 = CARTESIAN_POINT ( 'NONE',  ( -4.854898768586437541, 40.57568730855741990, -70.80100296729774811 ) ) ;
#19140 = DIRECTION ( 'NONE',  ( -1.000000000000000000, -1.224606353822377258E-16, -0.000000000000000000 ) ) ;
#19141 = VERTEX_POINT ( 'NONE', #28636 ) ;
#19142 = ADVANCED_FACE ( 'NONE', ( #13984 ), #105656, .F. ) ;
#19143 = AXIS2_PLACEMENT_3D ( 'NONE', #80221, #6325, #62472 ) ;
#19144 = CARTESIAN_POINT ( 'NONE',  ( -107.8347873283999263, -30.00000000001003997, 189.1745601741373264 ) ) ;
#19145 = EDGE_LOOP ( 'NONE', ( #32458, #18611, #79259, #85408 ) ) ;
#19146 = ORIENTED_EDGE ( 'NONE', *, *, #9803, .T. ) ;
#19147 = AXIS2_PLACEMENT_3D ( 'NONE', #89262, #25074, #41228 ) ;
#19148 = DIRECTION ( 'NONE',  ( -0.000000000000000000, 1.000000000000000000, -0.000000000000000000 ) ) ;
#19149 = DIRECTION ( 'NONE',  ( -1.000000000000000000, -0.000000000000000000, -0.000000000000000000 ) ) ;
#19150 = CARTESIAN_POINT ( 'NONE',  ( 7.894787914004607998, 0.7661396099416308836, -7.591390474663430865 ) ) ;
#19151 = SURFACE_SIDE_STYLE ('',( #745 ) ) ;
#19152 = CARTESIAN_POINT ( 'NONE',  ( 82.54631802247214978, -37.80417153317709023, -12.53333535189654846 ) ) ;
#19153 = CARTESIAN_POINT ( 'NONE',  ( -37.72597192858580684, 305.1524505036002211, -7.625521618108728639 ) ) ;
#19154 = FACE_OUTER_BOUND ( 'NONE', #81621, .T. ) ;
#19155 = CARTESIAN_POINT ( 'NONE',  ( -17.54117848700256488, 45.00000000000000711, 63.36500943357729909 ) ) ;
#19156 = CARTESIAN_POINT ( 'NONE',  ( -13.16254534550195565, 304.5561388177458184, 8.874148279916250104 ) ) ;
#19157 = ORIENTED_EDGE ( 'NONE', *, *, #4122, .T. ) ;
#19158 = ADVANCED_FACE ( 'NONE', ( #64680 ), #81902, .F. ) ;
#19159 = CARTESIAN_POINT ( 'NONE',  ( 0.000000000000000000, 0.000000000000000000, 0.000000000000000000 ) ) ;
#19160 = ORIENTED_EDGE ( 'NONE', *, *, #17089, .F. ) ;
#19161 = CARTESIAN_POINT ( 'NONE',  ( 48.91361122442920362, 8.059984797525084232, -16.48958644079329972 ) ) ;
#19162 = CARTESIAN_POINT ( 'NONE',  ( 0.000000000000000000, 48.00000000000000000, 61.50000000000000000 ) ) ;
#19163 = EDGE_CURVE ( 'NONE', #104988, #94131, #77641, .T. ) ;
#19165 = ORIENTED_EDGE ( 'NONE', *, *, #6203, .F. ) ;
#19164 = DIRECTION ( 'NONE',  ( 0.5735764363510462704, 0.8191520442889915765, 0.000000000000000000 ) ) ;
#19166 = CARTESIAN_POINT ( 'NONE',  ( 74.77612988998848209, -18.65171555483784971, 105.3432223141187762 ) ) ;
#19167 = CIRCLE ( 'NONE', #69095, 6.500000000000000000 ) ;
#19168 = ORIENTED_EDGE ( 'NONE', *, *, #22963, .T. ) ;
#19169 = AXIS2_PLACEMENT_3D ( 'NONE', #26973, #9667, #17268 ) ;
#19170 = CARTESIAN_POINT ( 'NONE',  ( 3.438608821155801021, -49.17330182167980013, 44.01479443626973875 ) ) ;
#19171 = DIRECTION ( 'NONE',  ( -1.000000000000000000, -1.224606353822377258E-16, -0.000000000000000000 ) ) ;
#19172 = CARTESIAN_POINT ( 'NONE',  ( -5.082755093536326818, -27.21875000204838813, 5.082755093536325042 ) ) ;
#19173 = CARTESIAN_POINT ( 'NONE',  ( -95.95698421656685184, -57.67166530053860640, 41.39248336299490916 ) ) ;
#19174 = ORIENTED_EDGE ( 'NONE', *, *, #101889, .F. ) ;
#19175 = MECHANICAL_DESIGN_GEOMETRIC_PRESENTATION_REPRESENTATION (  '', ( #15715 ), #26098 ) ;
#19176 = CARTESIAN_POINT ( 'NONE',  ( -24.92095225878771458, 43.66054905306249623, -76.23935496511737142 ) ) ;
#19178 = CARTESIAN_POINT ( 'NONE',  ( 104.3768403531009881, -52.71698490578736340, 184.8465504898348968 ) ) ;
#19177 = STYLED_ITEM ( 'NONE', ( #4322 ), #19117 ) ;
#19179 = CARTESIAN_POINT ( 'NONE',  ( -80.00000000000000000, -52.00000000000000000, -21.09707704303352926 ) ) ;
#19180 = CARTESIAN_POINT ( 'NONE',  ( 0.000000000000000000, 0.000000000000000000, 0.000000000000000000 ) ) ;
#19181 = CARTESIAN_POINT ( 'NONE',  ( -5.656854249492379694, -19.62500000409677270, -5.656854249492380582 ) ) ;
#19182 = CARTESIAN_POINT ( 'NONE',  ( -52.44185982314375849, -29.98747349849042720, 50.93426759498176182 ) ) ;
#19183 = DIRECTION ( 'NONE',  ( -1.000000000000000000, -1.224606353822377258E-16, -0.000000000000000000 ) ) ;
#19184 = CARTESIAN_POINT ( 'NONE',  ( -37.29743189576421258, 437.4067884073531332, 4.451016994673306471 ) ) ;
#19185 = DIRECTION ( 'NONE',  ( 0.000000000000000000, -1.000000000000000000, 0.000000000000000000 ) ) ;
#19186 = DIRECTION ( 'NONE',  ( 1.387778780781445676E-16, -0.6840875820779008798, -0.7293998766429913294 ) ) ;
#19187 = CARTESIAN_POINT ( 'NONE',  ( 33.77559172535811172, 464.7834715296606873, 7.192701217093182997 ) ) ;
#19188 = VERTEX_POINT ( 'NONE', #63093 ) ;
#19189 = CARTESIAN_POINT ( 'NONE',  ( 86.75754961941542831, 1.030564683017419500E-14, 0.000000000000000000 ) ) ;
#19190 = DIRECTION ( 'NONE',  ( 0.000000000000000000, 0.000000000000000000, 1.000000000000000000 ) ) ;
#19191 = CARTESIAN_POINT ( 'NONE',  ( 0.8433902809040685344, 8.501990100278735696, 51.42592703772288587 ) ) ;
#19192 = CARTESIAN_POINT ( 'NONE',  ( -87.08109489273023485, -30.00000000000000000, 184.1098654863104400 ) ) ;
#19193 = EDGE_CURVE ( 'NONE', #41746, #9858, #105208, .T. ) ;
#19194 = B_SPLINE_CURVE_WITH_KNOTS ( 'NONE', 3,
 ( #55090, #45969, #45442, #61640, #47005, #14098, #6013, #38937, #30869, #86450, #63749, #96636, #85912, #11987, #44917, #77801, #94532, #69712, #102605, #20683 ),
 .UNSPECIFIED., .F., .F.,
 ( 4, 2, 2, 2, 2, 2, 2, 2, 2, 4 ),
 ( 0.003623855290150441045, 0.004630762948664648646, 0.005134216777921752663, 0.005637670607178856680, 0.005889397521807407387, 0.006141124436435958095, 0.006644578265693064714, 0.006896305180321615422, 0.007148032094950166129, 0.007651485924207265810 ),
 .UNSPECIFIED. ) ;
#19195 = AXIS2_PLACEMENT_3D ( 'NONE', #25720, #65595, #58580 ) ;
#19196 = ORIENTED_EDGE ( 'NONE', *, *, #18659, .F. ) ;
#19197 = EDGE_CURVE ( 'NONE', #80498, #44793, #5891, .T. ) ;
#19198 = CARTESIAN_POINT ( 'NONE',  ( 38.56636269275068685, 25.18999535537753331, -12.97483823376252410 ) ) ;
#19199 = CARTESIAN_POINT ( 'NONE',  ( 73.91422987116176557, -57.61663468891570972, 186.6107994588369081 ) ) ;
#19200 = AXIS2_PLACEMENT_3D ( 'NONE', #73023, #66546, #83257 ) ;
#19202 = CARTESIAN_POINT ( 'NONE',  ( 46.00000000000004263, 436.1058985003094222, 16.82352493621293377 ) ) ;
#19201 = CARTESIAN_POINT ( 'NONE',  ( -14.97109678640281594, 2.057467188490503585, 0.8486206380284277984 ) ) ;
#19203 = ADVANCED_FACE ( 'NONE', ( #30750 ), #98342, .T. ) ;
#19204 = EDGE_CURVE ( 'NONE', #31268, #21775, #55494, .T. ) ;
#19205 = CARTESIAN_POINT ( 'NONE',  ( 27.28396264558442752, -28.56679706456900902, -38.29477899011715891 ) ) ;
#19206 =( GEOMETRIC_REPRESENTATION_CONTEXT ( 3 ) GLOBAL_UNCERTAINTY_ASSIGNED_CONTEXT ( ( #90381 ) ) GLOBAL_UNIT_ASSIGNED_CONTEXT ( ( #69919, #102279, #13254 ) ) REPRESENTATION_CONTEXT ( 'NONE', 'WORKASPACE' ) );
#19207 = CARTESIAN_POINT ( 'NONE',  ( 7.500000000000000000, -3.000000000000000000, -20.99851272547260095 ) ) ;
#19208 =( LENGTH_UNIT ( ) NAMED_UNIT ( * ) SI_UNIT ( .MILLI., .METRE. ) );
#19209 = PRODUCT ( 'hex bolt gradeab_din_DIN EN 24014 - M8 x 70 x 22-S', 'hex bolt gradeab_din_DIN EN 24014 - M8 x 70 x 22-S', '', ( #14211 ) ) ;
#19210 = CARTESIAN_POINT ( 'NONE',  ( -36.17094327262719844, -60.00000000000000000, 47.52071233496300096 ) ) ;
#19211 = EDGE_CURVE ( 'NONE', #40814, #73170, #72473, .T. ) ;
#19212 = CARTESIAN_POINT ( 'NONE',  ( -86.32881076508184037, -46.50315659945954394, 190.0124563228725378 ) ) ;
#19213 = EDGE_CURVE ( 'NONE', #10685, #100984, #21260, .T. ) ;
#19214 = VERTEX_POINT ( 'NONE', #59791 ) ;
#19215 = CARTESIAN_POINT ( 'NONE',  ( -42.16858620285800185, 461.4629983908308191, 3.513115262080999557 ) ) ;
#19216 = CARTESIAN_POINT ( 'NONE',  ( -1.007163654173327982, -42.95772940445374388, 31.04927152701133153 ) ) ;
#19217 = EDGE_CURVE ( 'NONE', #104354, #69179, #26033, .T. ) ;
#19218 = EDGE_CURVE ( 'NONE', #1105, #98286, #66806, .T. ) ;
#19219 = FACE_OUTER_BOUND ( 'NONE', #40365, .T. ) ;
#19220 = CARTESIAN_POINT ( 'NONE',  ( 83.88447113947664491, -60.00000000000000000, 191.6821499555289847 ) ) ;
#19222 = FILL_AREA_STYLE_COLOUR ( '', #56011 ) ;
#19221 = CARTESIAN_POINT ( 'NONE',  ( -42.11927462130235966, 344.1102093767603947, 13.55314436600152739 ) ) ;
#19223 = VERTEX_POINT ( 'NONE', #58721 ) ;
#19224 = STYLED_ITEM ( 'NONE', ( #9516 ), #47680 ) ;
#19225 = CARTESIAN_POINT ( 'NONE',  ( 24.33159596665262470, 34.19642918197134662, 12.16579798332630880 ) ) ;
#19226 = DIRECTION ( 'NONE',  ( -0.5735764363510497121, 0.8191520442889892450, 1.003171929053521665E-16 ) ) ;
#19227 = CARTESIAN_POINT ( 'NONE',  ( -9.574280356041013462, -5.000000000000002665, -20.99850713196553187 ) ) ;
#19228 = DIRECTION ( 'NONE',  ( 0.5735764363510466035, -0.8191520442889914655, 1.003171929053524500E-16 ) ) ;
#19229 = CARTESIAN_POINT ( 'NONE',  ( 23.58450237658830417, 303.4694747804686017, -9.867290210144552987 ) ) ;
#19230 = CARTESIAN_POINT ( 'NONE',  ( 43.74855578046756222, 328.6220886837048170, -1.765109843966993441 ) ) ;
#19231 = SHAPE_REPRESENTATION ( '4. Handle', ( #10728 ), #60740 ) ;
#19232 = DIRECTION ( 'NONE',  ( 1.000000000000000000, 0.000000000000000000, 0.000000000000000000 ) ) ;
#19233 = CARTESIAN_POINT ( 'NONE',  ( 9.533652678419262116, 53.58338683237839462, -1.993657782990515992 ) ) ;
#19234 = CARTESIAN_POINT ( 'NONE',  ( 109.5930103617047422, -60.00000000000001421, 123.9179654958789456 ) ) ;
#19235 = CARTESIAN_POINT ( 'NONE',  ( -83.58713925656184074, -18.68419755623315126, 145.1655856526831201 ) ) ;
#19236 = ORIENTED_EDGE ( 'NONE', *, *, #8594, .F. ) ;
#19237 = CARTESIAN_POINT ( 'NONE',  ( -3.294249609603391082, -3.000000000000002665, -70.27378291343094929 ) ) ;
#19238 = CARTESIAN_POINT ( 'NONE',  ( 5.093234209762004916, 252.4446777346490194, 3.176141468578033145 ) ) ;
#19239 = CARTESIAN_POINT ( 'NONE',  ( 27.41618788073706270, -57.67796933674075177, 43.99820381704387984 ) ) ;
#19240 = CARTESIAN_POINT ( 'NONE',  ( -4.472135954999579610, -85.00000000000000000, 4.000000000000001776 ) ) ;
#19241 = CARTESIAN_POINT ( 'NONE',  ( 43.81783411079661050, 329.5522331351167509, -1.551972439396806402 ) ) ;
#19242 = DIRECTION ( 'NONE',  ( 0.000000000000000000, -1.000000000000000000, 0.000000000000000000 ) ) ;
#19243 = EDGE_LOOP ( 'NONE', ( #73220, #23908, #4901, #21364 ) ) ;
#19244 = UNCERTAINTY_MEASURE_WITH_UNIT (LENGTH_MEASURE( 1.000000000000000082E-05 ), #68826, 'distance_accuracy_value', 'NONE');
#19245 = LINE ( 'NONE', #76883, #56431 ) ;
#19246 = CIRCLE ( 'NONE', #62322, 15.00000000000000711 ) ;
#19247 = STYLED_ITEM ( 'NONE', ( #106653 ), #82163 ) ;
#19248 = CARTESIAN_POINT ( 'NONE',  ( 31.29338602784115864, 439.6455612451725870, 23.30856287163057772 ) ) ;
#19249 = ORIENTED_EDGE ( 'NONE', *, *, #13580, .T. ) ;
#19250 = DIRECTION ( 'NONE',  ( 0.000000000000000000, 1.000000000000000000, 0.000000000000000000 ) ) ;
#19251 = AXIS2_PLACEMENT_3D ( 'NONE', #77347, #84908, #76271 ) ;
#19252 = DIRECTION ( 'NONE',  ( -0.5000000000000008882, 0.8660254037844381525, 0.000000000000000000 ) ) ;
#19253 = FACE_OUTER_BOUND ( 'NONE', #89720, .T. ) ;
#19254 = CARTESIAN_POINT ( 'NONE',  ( -28.89099332391479535, 50.00000000002003731, 58.53034795348396813 ) ) ;
#19255 = CARTESIAN_POINT ( 'NONE',  ( 4.277266239492808708, -9.465691673376495530, -11.68615649787714972 ) ) ;
#19257 = B_SPLINE_CURVE_WITH_KNOTS ( 'NONE', 3,
 ( #66111, #24622, #40769, #58009, #97947, #56939, #74719, #82290, #99530, #58569, #40241, #89861, #15968, #32168, #73660, #73117, #15432, #90934, #82829, #91466, #48846, #16497 ),
 .UNSPECIFIED., .F., .F.,
 ( 4, 2, 2, 2, 2, 2, 2, 2, 2, 2, 4 ),
 ( 0.001294468792936987779, 0.002255807329995941028, 0.003217145867054894276, 0.005139822941172805110, 0.006101161478231762261, 0.007062500015290718546, 0.008985177089408637185, 0.01090785416352655843, 0.01283053123764447967, 0.01475320831176240091, 0.01667588538588031868 ),
 .UNSPECIFIED. ) ;
#19256 = VECTOR ( 'NONE', #61840, 1000.000000000000000 ) ;
#19258 =( NAMED_UNIT ( * ) SI_UNIT ( $, .STERADIAN. ) SOLID_ANGLE_UNIT ( ) );
#19259 = ORIENTED_EDGE ( 'NONE', *, *, #103826, .T. ) ;
#19260 = DIRECTION ( 'NONE',  ( -1.000000000000000000, -0.000000000000000000, -0.000000000000000000 ) ) ;
#19261 = AXIS2_PLACEMENT_3D ( 'NONE', #85661, #4731, #85113 ) ;
#19263 = CARTESIAN_POINT ( 'NONE',  ( 19.90934191524716468, -29.03263091507375648, 29.21916946763769829 ) ) ;
#19262 = CARTESIAN_POINT ( 'NONE',  ( -83.90898588706018302, -30.00000000000009592, 196.6629347554013520 ) ) ;
#19264 = CARTESIAN_POINT ( 'NONE',  ( -6.011841252072294266E-15, 27.55047179872464724, 49.09040922050319011 ) ) ;
#19265 = DIRECTION ( 'NONE',  ( -1.000000000000000000, -1.224606353822377258E-16, -0.000000000000000000 ) ) ;
#19266 = EDGE_CURVE ( 'NONE', #8468, #47738, #33003, .T. ) ;
#19267 = CARTESIAN_POINT ( 'NONE',  ( -33.47853446770369601, -18.69755159962205227, 30.56496980470470604 ) ) ;
#19268 = CIRCLE ( 'NONE', #50217, 35.82893434829263413 ) ;
#19269 = UNCERTAINTY_MEASURE_WITH_UNIT (LENGTH_MEASURE( 1.000000000000000082E-05 ), #67332, 'distance_accuracy_value', 'NONE');
#19270 = EDGE_LOOP ( 'NONE', ( #54047, #40537 ) ) ;
#19271 = PRODUCT_DEFINITION_SHAPE ( 'NONE', 'NONE',  #106810 ) ;
#19272 = CYLINDRICAL_SURFACE ( 'NONE', #3086, 5.000000000000000888 ) ;
#19273 = CARTESIAN_POINT ( 'NONE',  ( -48.02835407290516656, 11.61227450977240494, 14.35535821593516559 ) ) ;
#19274 = CARTESIAN_POINT ( 'NONE',  ( 5.075566108724593128, -4.332661967060489339, -17.09624963492156269 ) ) ;
#19275 = CARTESIAN_POINT ( 'NONE',  ( 7.999912353029504430, -61.00017529396908600, -0.2691822806795002299 ) ) ;
#19276 = CARTESIAN_POINT ( 'NONE',  ( -14.95236164054199257, 4.204970931333630091, 5.179833178273279159 ) ) ;
#19278 = EDGE_CURVE ( 'NONE', #20459, #103579, #12230, .T. ) ;
#19277 = EDGE_LOOP ( 'NONE', ( #6830, #27357, #64753, #36146, #45848 ) ) ;
#19279 = CARTESIAN_POINT ( 'NONE',  ( -15.73424097804746324, 37.19149822104526493, -22.31191215652655657 ) ) ;
#19280 = ORIENTED_EDGE ( 'NONE', *, *, #39543, .T. ) ;
#19281 = CARTESIAN_POINT ( 'NONE',  ( 98.93841510732947597, -30.00000000000001066, 144.4000381891304130 ) ) ;
#19282 = CARTESIAN_POINT ( 'NONE',  ( 32.85077815300981285, 40.72790403658980551, -62.46656677406199520 ) ) ;
#19283 = CARTESIAN_POINT ( 'NONE',  ( -4.567209634097050497, -84.06400213914488972, -3.891254717191802381 ) ) ;
#19284 = CARTESIAN_POINT ( 'NONE',  ( 80.76542010163649365, -30.00000000000000355, 13.70105158619666419 ) ) ;
#19285 = CARTESIAN_POINT ( 'NONE',  ( -32.01437930851541580, 362.7125307742095970, 22.60227621942590304 ) ) ;
#19286 = VERTEX_POINT ( 'NONE', #82450 ) ;
#19287 = VECTOR ( 'NONE', #8160, 1000.000000000000000 ) ;
#19288 = ORIENTED_EDGE ( 'NONE', *, *, #88722, .T. ) ;
#19289 = ORIENTED_EDGE ( 'NONE', *, *, #30933, .F. ) ;
#19290 = CARTESIAN_POINT ( 'NONE',  ( -31.99294114632805019, 464.8457910465705822, 12.87241426108672826 ) ) ;
#19291 = CARTESIAN_POINT ( 'NONE',  ( 0.000000000000000000, 0.000000000000000000, -8.553285714285713937 ) ) ;
#19292 = CARTESIAN_POINT ( 'NONE',  ( 8.000000000000000000, -15.40624999999999289, -3.313708498984761164 ) ) ;
#19293 = AXIS2_PLACEMENT_3D ( 'NONE', #49570, #73299, #81391 ) ;
#19294 = CARTESIAN_POINT ( 'NONE',  ( 5.649205854336971200, -13.45354532811516179, -2.034449005107564545 ) ) ;
#19295 = FACE_OUTER_BOUND ( 'NONE', #85775, .T. ) ;
#19296 = FILL_AREA_STYLE ('',( #60256 ) ) ;
#19297 = ORIENTED_EDGE ( 'NONE', *, *, #103347, .F. ) ;
#19298 = EDGE_CURVE ( 'NONE', #71455, #2681, #32865, .T. ) ;
#19299 = CARTESIAN_POINT ( 'NONE',  ( 6.043427762770655853, 50.00000000000000000, -74.51456333905269958 ) ) ;
#19300 = ORIENTED_EDGE ( 'NONE', *, *, #3549, .T. ) ;
#19301 = CARTESIAN_POINT ( 'NONE',  ( 37.33349330513379982, 1.593028355512270567E-15, 0.000000000000000000 ) ) ;
#19302 = CARTESIAN_POINT ( 'NONE',  ( 71.49141929022891873, -38.32768232336286474, 142.8628847782384810 ) ) ;
#19303 = FACE_OUTER_BOUND ( 'NONE', #34166, .T. ) ;
#19304 = CARTESIAN_POINT ( 'NONE',  ( 25.78003121851679680, 295.8949495087512673, 2.161690327135773693 ) ) ;
#19305 = EDGE_CURVE ( 'NONE', #22672, #83885, #98387, .T. ) ;
#19306 = FACE_BOUND ( 'NONE', #71634, .T. ) ;
#19307 = ORIENTED_EDGE ( 'NONE', *, *, #89799, .T. ) ;
#19308 = CARTESIAN_POINT ( 'NONE',  ( 0.000000000000000000, 6.123233995736770227E-16, -5.000000000000002665 ) ) ;
#19309 = CARTESIAN_POINT ( 'NONE',  ( 35.59999999999999432, -3.309499999999999886, 0.000000000000000000 ) ) ;
#19310 = CARTESIAN_POINT ( 'NONE',  ( 21.09715123528542691, -5.000000000000000000, 0.000000000000000000 ) ) ;
#19311 = DIRECTION ( 'NONE',  ( 0.000000000000000000, 1.000000000000000000, 0.000000000000000000 ) ) ;
#19312 = CARTESIAN_POINT ( 'NONE',  ( 14.89969599197393002, 1.346844969883137511, 1.740400043388351081 ) ) ;
#19313 = EDGE_LOOP ( 'NONE', ( #61054, #37164, #27980, #29933 ) ) ;
#19314 =( NAMED_UNIT ( * ) PLANE_ANGLE_UNIT ( ) SI_UNIT ( $, .RADIAN. ) );
#19315 = LINE ( 'NONE', #43535, #45154 ) ;
#19316 = CARTESIAN_POINT ( 'NONE',  ( 21.84999999999999787, 3.309500000000003439, 4.052968581778167743E-16 ) ) ;
#19317 = CARTESIAN_POINT ( 'NONE',  ( 0.000000000000000000, 0.000000000000000000, 0.000000000000000000 ) ) ;
#19318 = FACE_OUTER_BOUND ( 'NONE', #15810, .T. ) ;
#19319 = FACE_BOUND ( 'NONE', #18898, .T. ) ;
#19320 = PRODUCT_DEFINITION ( 'UNKNOWN', '', #25007, #99571 ) ;
#19321 = CARTESIAN_POINT ( 'NONE',  ( 6.878751942472531411, 3.924677726130916255, -6.573129608219089093 ) ) ;
#19322 = CARTESIAN_POINT ( 'NONE',  ( 84.56215681354241553, -57.45443045189220754, 191.5346530351454533 ) ) ;
#19323 = CARTESIAN_POINT ( 'NONE',  ( 17.77146113466383426, 36.31761464240111081, -23.79974184213102362 ) ) ;
#19324 = CARTESIAN_POINT ( 'NONE',  ( -2.844355883296552090, 79.52658463821998680, 5.000000000000000000 ) ) ;
#19325 = VERTEX_POINT ( 'NONE', #83505 ) ;
#19326 = PRESENTATION_STYLE_ASSIGNMENT (( #93159 ) ) ;
#19327 = AXIS2_PLACEMENT_3D ( 'NONE', #60536, #27124, #34681 ) ;
#19328 = DIRECTION ( 'NONE',  ( 0.000000000000000000, -1.000000000000000000, 0.000000000000000000 ) ) ;
#19329 = FACE_OUTER_BOUND ( 'NONE', #97031, .T. ) ;
#19330 = CARTESIAN_POINT ( 'NONE',  ( 55.74444444444444713, 6.915964383211875250E-15, 0.000000000000000000 ) ) ;
#19331 = CARTESIAN_POINT ( 'NONE',  ( -83.18363256083800650, -30.00000000000000355, 44.37128110272426795 ) ) ;
#19332 = FILL_AREA_STYLE_COLOUR ( '', #46838 ) ;
#19333 = AXIS2_PLACEMENT_3D ( 'NONE', #89246, #95744, #14272 ) ;
#19334 = CARTESIAN_POINT ( 'NONE',  ( 32.95144866765099323, -57.69153774002047186, 47.28118679687395343 ) ) ;
#19335 = MANIFOLD_SOLID_BREP ( 'Chamfer1', #56606 ) ;
#19337 = DIRECTION ( 'NONE',  ( -0.000000000000000000, -1.000000000000000000, -0.000000000000000000 ) ) ;
#19336 = CARTESIAN_POINT ( 'NONE',  ( 36.63387181268254977, 490.9973753891291040, 12.47313570402020666 ) ) ;
#19338 = ADVANCED_FACE ( 'NONE', ( #86728 ), #29555, .T. ) ;
#19339 = CARTESIAN_POINT ( 'NONE',  ( -51.20800334721975133, -38.00000000000002132, 52.28430389016808988 ) ) ;
#19340 = CARTESIAN_POINT ( 'NONE',  ( -37.51625577700188074, 491.7333577044544768, 12.51656167145504384 ) ) ;
#19341 = CARTESIAN_POINT ( 'NONE',  ( -9.090909090909089940, 16.00000000000000000, 4.165977904505306029 ) ) ;
#19342 = DIRECTION ( 'NONE',  ( 0.000000000000000000, -1.000000000000000000, 0.000000000000000000 ) ) ;
#19343 = CARTESIAN_POINT ( 'NONE',  ( 39.82383024057768495, -24.81360042265481169, -30.33102204919740785 ) ) ;
#19344 = CARTESIAN_POINT ( 'NONE',  ( -26.88564424253746665, -60.35060106910436417, 35.78314768987581118 ) ) ;
#19345 = ORIENTED_EDGE ( 'NONE', *, *, #27636, .F. ) ;
#19346 = CARTESIAN_POINT ( 'NONE',  ( 19.00000000000000711, 4.000000000000000888, -1.500000000000001332 ) ) ;
#19347 = SURFACE_STYLE_USAGE ( .BOTH. , #93181 ) ;
#19348 = CARTESIAN_POINT ( 'NONE',  ( -17.95371827100986195, -42.95797721961560001, 31.37255097494336908 ) ) ;
#19349 = EDGE_CURVE ( 'NONE', #11179, #67595, #89811, .T. ) ;
#19350 = EDGE_CURVE ( 'NONE', #92807, #39874, #38174, .T. ) ;
#19352 = CARTESIAN_POINT ( 'NONE',  ( 40.17970824403359842, 485.1790858365317263, -4.313947164402517132 ) ) ;
#19351 = CARTESIAN_POINT ( 'NONE',  ( -14.75116209839011994, 43.55504285526384933, -90.22050492866908655 ) ) ;
#19353 = ORIENTED_EDGE ( 'NONE', *, *, #98620, .T. ) ;
#19354 = ORIENTED_EDGE ( 'NONE', *, *, #45773, .F. ) ;
#19355 = CARTESIAN_POINT ( 'NONE',  ( 0.000000000000000000, 0.000000000000000000, 0.000000000000000000 ) ) ;
#19356 = CIRCLE ( 'NONE', #33107, 4.000000000000001776 ) ;
#19357 = CIRCLE ( 'NONE', #12361, 5.000000000000000000 ) ;
#19358 = SURFACE_SIDE_STYLE ('',( #18258 ) ) ;
#19359 = CARTESIAN_POINT ( 'NONE',  ( 92.82022815836235452, 1.016364837396684119E-14, 0.000000000000000000 ) ) ;
#19360 = ORIENTED_EDGE ( 'NONE', *, *, #15864, .T. ) ;
#19361 = FACE_OUTER_BOUND ( 'NONE', #98927, .T. ) ;
#19362 = CARTESIAN_POINT ( 'NONE',  ( 101.4140146818485988, -52.73191828097732525, 192.9060813891788655 ) ) ;
#19364 = LINE ( 'NONE', #100744, #22040 ) ;
#19363 = DIRECTION ( 'NONE',  ( -0.000000000000000000, 1.000000000000000000, -0.000000000000000000 ) ) ;
#19365 = ORIENTED_EDGE ( 'NONE', *, *, #35280, .T. ) ;
#19366 = ORIENTED_EDGE ( 'NONE', *, *, #77728, .T. ) ;
#19367 = ORIENTED_EDGE ( 'NONE', *, *, #80978, .T. ) ;
#19369 =( BOUNDED_SURFACE ( )  B_SPLINE_SURFACE ( 3, 2, ( 
 ( #20608, #3298, #60498 ),
 ( #59424, #69635, #27618 ),
 ( #11910, #61020, #44839 ),
 ( #92829, #51835, #85834 ),
 ( #93381, #52367, #77726 ),
 ( #34641, #18442, #85278 ),
 ( #100920, #51298, #84217 ),
 ( #68027, #36769, #84750 ) ),
 .UNSPECIFIED., .F., .F., .F. ) 
 B_SPLINE_SURFACE_WITH_KNOTS ( ( 4, 2, 2, 4 ),
 ( 3, 3 ),
 ( 2.732189474663471174E-17, 0.002319727980540720394, 0.003479591970811066713, 0.004639455961081413032 ),
 ( 0.000000000000000000, 1.000000000000000000 ),
 .UNSPECIFIED. ) 
 GEOMETRIC_REPRESENTATION_ITEM ( )  RATIONAL_B_SPLINE_SURFACE ( (
 ( 1.000000000000000000, 0.8162384603571204433, 1.000000000000000000),
 ( 1.000000000000000000, 0.8233098591466496696, 1.000000000000000000),
 ( 1.000000000000000000, 0.8247006568295612849, 1.000000000000000000),
 ( 1.000000000000000000, 0.8207129887246857880, 1.000000000000000000),
 ( 1.000000000000000000, 0.8182997519107459983, 1.000000000000000000),
 ( 1.000000000000000000, 0.8111528056794476971, 1.000000000000000000),
 ( 1.000000000000000000, 0.8064385712637164305, 1.000000000000000000),
 ( 1.000000000000000000, 0.8001746426091337350, 1.000000000000000000) ) ) 
 REPRESENTATION_ITEM ( '' )  SURFACE ( )  );
#19368 = CARTESIAN_POINT ( 'NONE',  ( 23.79145413011031351, 304.9699511662212785, 10.18164519790058442 ) ) ;
#19370 = CARTESIAN_POINT ( 'NONE',  ( 64.29999999999999716, 6.915964383211875250E-15, 0.000000000000000000 ) ) ;
#19371 = DIRECTION ( 'NONE',  ( -0.2517716543986441846, 0.000000000000000000, 0.9677866676294779591 ) ) ;
#19372 = VERTEX_POINT ( 'NONE', #93741 ) ;
#19373 = DIRECTION ( 'NONE',  ( 1.224646799147351482E-16, 0.000000000000000000, -1.000000000000000000 ) ) ;
#19374 = DIRECTION ( 'NONE',  ( 0.000000000000000000, 0.000000000000000000, 1.000000000000000000 ) ) ;
#19375 = DIRECTION ( 'NONE',  ( -1.000000000000000000, -1.224606353822377258E-16, -0.000000000000000000 ) ) ;
#19376 = CARTESIAN_POINT ( 'NONE',  ( -90.68113043260497363, -59.99999999999998579, -22.06029277779147790 ) ) ;
#19377 = CARTESIAN_POINT ( 'NONE',  ( 14.27307692307692299, 1.411358822780289120E-15, 0.000000000000000000 ) ) ;
#19378 = CARTESIAN_POINT ( 'NONE',  ( -35.76482652855951017, 405.2378813769876729, 6.148826621638260548 ) ) ;
#19379 = CARTESIAN_POINT ( 'NONE',  ( -6.516859558828629773, 41.40454146154883830, -58.45803901209384179 ) ) ;
#19380 = CARTESIAN_POINT ( 'NONE',  ( -93.94019401501873290, -59.99999999999992895, -15.95863606727341022 ) ) ;
#19381 = FACE_OUTER_BOUND ( 'NONE', #20191, .T. ) ;
#19382 = EDGE_CURVE ( 'NONE', #28486, #15372, #70867, .T. ) ;
#19383 = CARTESIAN_POINT ( 'NONE',  ( -48.50691641643196306, -53.36615341440958105, 52.77268722834218551 ) ) ;
#19384 = ORIENTED_EDGE ( 'NONE', *, *, #76408, .F. ) ;
#19385 = CARTESIAN_POINT ( 'NONE',  ( 0.000000000000000000, 16.00000000000000000, 0.000000000000000000 ) ) ;
#19386 = ORIENTED_EDGE ( 'NONE', *, *, #88444, .T. ) ;
#19387 = CARTESIAN_POINT ( 'NONE',  ( -1.469576158976823947E-15, -12.87499999999999467, 8.000000000000000000 ) ) ;
#19388 = CARTESIAN_POINT ( 'NONE',  ( -4.023953349588704320, 300.5162199157759915, -10.00978861085819460 ) ) ;
#19389 = CARTESIAN_POINT ( 'NONE',  ( 6.098403338276324526, 3.412123303361987325, 6.499999999999997335 ) ) ;
#19390 = ORIENTED_EDGE ( 'NONE', *, *, #97343, .F. ) ;
#19391 = CARTESIAN_POINT ( 'NONE',  ( 4.904566723942675566, 247.9775729752925315, 3.460360782932712986 ) ) ;
#19392 = CARTESIAN_POINT ( 'NONE',  ( 79.62312256247624020, -29.99999999999502975, -25.10596286033261748 ) ) ;
#19393 = CARTESIAN_POINT ( 'NONE',  ( 2.599973688629601546E-12, 9.016154170237600241, -7.999534413642741093 ) ) ;
#19394 = CARTESIAN_POINT ( 'NONE',  ( 3.459690225506051320, -48.89101625908396898, 104.5059395991323470 ) ) ;
#19395 = MECHANICAL_DESIGN_GEOMETRIC_PRESENTATION_REPRESENTATION (  '', ( #102020 ), #15944 ) ;
#19396 = CARTESIAN_POINT ( 'NONE',  ( 33.86650669486618881, 4.000000000000003553, 4.898587196589414801E-16 ) ) ;
#19397 = CARTESIAN_POINT ( 'NONE',  ( 38.36535705883633796, 18.64316884711713840, 5.022013495247446890 ) ) ;
#19398 = CARTESIAN_POINT ( 'NONE',  ( 87.75391236170332832, -30.00000000000000000, 186.1424029422745434 ) ) ;
#19399 = AXIS2_PLACEMENT_3D ( 'NONE', #62781, #40081, #63841 ) ;
#19400 = CARTESIAN_POINT ( 'NONE',  ( 43.22624402987835879, 434.6924416827904452, 9.644670084733055759 ) ) ;
#19401 = EDGE_CURVE ( 'NONE', #51545, #40845, #59822, .T. ) ;
#19402 = CARTESIAN_POINT ( 'NONE',  ( -30.00000000000000000, 450.0000000000002274, 13.20242257375370976 ) ) ;
#19403 = ORIENTED_EDGE ( 'NONE', *, *, #22339, .F. ) ;
#19404 = ORIENTED_EDGE ( 'NONE', *, *, #106008, .T. ) ;
#19405 = CARTESIAN_POINT ( 'NONE',  ( 53.66335548193523408, -32.56571110302638772, 54.84416711442435144 ) ) ;
#19406 = CARTESIAN_POINT ( 'NONE',  ( 7.026865755812575998, 41.28180827239863504, -58.57604196968413390 ) ) ;
#19407 =( GEOMETRIC_REPRESENTATION_CONTEXT ( 3 ) GLOBAL_UNCERTAINTY_ASSIGNED_CONTEXT ( ( #59158 ) ) GLOBAL_UNIT_ASSIGNED_CONTEXT ( ( #69373, #77456, #4100 ) ) REPRESENTATION_CONTEXT ( 'NONE', 'WORKASPACE' ) );
#19408 = CARTESIAN_POINT ( 'NONE',  ( 37.33349330513379982, -4.000000000000000888, 4.898587196589416773E-16 ) ) ;
#19409 = ORIENTED_EDGE ( 'NONE', *, *, #20951, .T. ) ;
#19410 = CARTESIAN_POINT ( 'NONE',  ( -85.36887401862720992, -38.35973107371995638, -22.50894793657372261 ) ) ;
#19411 = ORIENTED_EDGE ( 'NONE', *, *, #30939, .T. ) ;
#19412 = CARTESIAN_POINT ( 'NONE',  ( 110.4849111511414606, -38.35604559967232774, 182.5406385957329292 ) ) ;
#19413 = CARTESIAN_POINT ( 'NONE',  ( 13.04450623576480872, 19.29496049036926308, 7.774814228663267102 ) ) ;
#19414 = CARTESIAN_POINT ( 'NONE',  ( 85.24431148756310961, -52.71368398924936827, 22.59386177874363710 ) ) ;
#19415 = CARTESIAN_POINT ( 'NONE',  ( -0.6457278711330333154, 45.36073317496411050, -18.58332603715044584 ) ) ;
#19416 = DIRECTION ( 'NONE',  ( -1.000000000000000000, 0.000000000000000000, 0.000000000000000000 ) ) ;
#19417 = CARTESIAN_POINT ( 'NONE',  ( 5.180156406282274695, -13.23729396337629538, -7.081638082359322794 ) ) ;
#19418 = EDGE_CURVE ( 'NONE', #66185, #16979, #81165, .T. ) ;
#19419 = CARTESIAN_POINT ( 'NONE',  ( -24.44510943275183124, 25.27280235212049675, -32.24409512226776542 ) ) ;
#19420 = CARTESIAN_POINT ( 'NONE',  ( -43.81062608880512244, 434.3289934330967981, 12.63519120573293542 ) ) ;
#19421 = CARTESIAN_POINT ( 'NONE',  ( 2.869473476665008516, 87.32989181417194402, 5.000000000000000000 ) ) ;
#19422 = ORIENTED_EDGE ( 'NONE', *, *, #8414, .F. ) ;
#19423 =( GEOMETRIC_REPRESENTATION_CONTEXT ( 3 ) GLOBAL_UNCERTAINTY_ASSIGNED_CONTEXT ( ( #60002 ) ) GLOBAL_UNIT_ASSIGNED_CONTEXT ( ( #2939, #43941, #27810 ) ) REPRESENTATION_CONTEXT ( 'NONE', 'WORKASPACE' ) );
#19424 = EDGE_CURVE ( 'NONE', #64980, #86482, #96739, .T. ) ;
#19425 = CARTESIAN_POINT ( 'NONE',  ( -4.000000000000000000, 17.85270131633358659, -5.744562646538044604 ) ) ;
#19426 = CARTESIAN_POINT ( 'NONE',  ( 15.73298926836839229, 37.19132885152138357, -22.31337215277972419 ) ) ;
#19427 = PRESENTATION_LAYER_ASSIGNMENT (  '', '', ( #79728 ) ) ;
#19428 = CARTESIAN_POINT ( 'NONE',  ( -32.45536069360919385, 439.3279843089443943, 23.70254088333128450 ) ) ;
#19429 = ORIENTED_EDGE ( 'NONE', *, *, #24809, .T. ) ;
#19430 = CARTESIAN_POINT ( 'NONE',  ( -32.23866588128408495, 319.2897111165075898, -5.491189000399069542 ) ) ;
#19431 = CARTESIAN_POINT ( 'NONE',  ( -29.01992505677934275, 312.0266740597124340, 12.14665302515488143 ) ) ;
#19432 = CARTESIAN_POINT ( 'NONE',  ( 21.36650669486618881, 1.474610560812782335E-15, 0.000000000000000000 ) ) ;
#19433 = DIRECTION ( 'NONE',  ( -1.000000000000000000, -1.224606353822377258E-16, -0.000000000000000000 ) ) ;
#19434 = CARTESIAN_POINT ( 'NONE',  ( -3.313708498984760720, -19.53124999999999289, -8.000000000000000000 ) ) ;
#19435 = CARTESIAN_POINT ( 'NONE',  ( -9.393209957245337804, -13.60606480366886473, 31.92530073092069642 ) ) ;
#19436 = LINE ( 'NONE', #92734, #62192 ) ;
#19437 = CIRCLE ( 'NONE', #40018, 0.9999999999999965583 ) ;
#19438 = ORIENTED_EDGE ( 'NONE', *, *, #98033, .F. ) ;
#19439 = CARTESIAN_POINT ( 'NONE',  ( 83.68344101230451315, -53.75102016957082895, 188.1393155033960056 ) ) ;
#19440 = CARTESIAN_POINT ( 'NONE',  ( -10.00000000000000178, -15.00000000000000000, -9.999999999999998224 ) ) ;
#19441 = CARTESIAN_POINT ( 'NONE',  ( -86.23550558450645553, -45.41061243867311958, 189.5308106279269396 ) ) ;
#19442 = ORIENTED_EDGE ( 'NONE', *, *, #81070, .T. ) ;
#19443 = ADVANCED_FACE ( 'NONE', ( #95333 ), #52737, .T. ) ;
#19444 = CARTESIAN_POINT ( 'NONE',  ( -86.15561449557901597, -37.82113771879615172, 53.97651405801602209 ) ) ;
#19445 = CARTESIAN_POINT ( 'NONE',  ( -6.503518969018518003E-15, -5.948846446048894343, 2.696295709017757947 ) ) ;
#19446 = CARTESIAN_POINT ( 'NONE',  ( 46.00000000000000000, 500.0000000000002274, 0.000000000000000000 ) ) ;
#19447 = CARTESIAN_POINT ( 'NONE',  ( -16.64348903516521005, -1.200000000000000030E-05, -4.157797401561533768 ) ) ;
#19448 = CARTESIAN_POINT ( 'NONE',  ( -13.98520082896717653, -23.75605607105831396, -38.53473594684242443 ) ) ;
#19449 = CARTESIAN_POINT ( 'NONE',  ( 39.83354149937073174, -60.00000000000000711, 51.86226764490275087 ) ) ;
#19450 = CARTESIAN_POINT ( 'NONE',  ( 29.71740142289437614, -32.26218012251615619, 40.41358957572558808 ) ) ;
#19451 = CARTESIAN_POINT ( 'NONE',  ( 7.046357527897573192, 106.3061565060100548, -3.789683693877204274 ) ) ;
#19452 = CARTESIAN_POINT ( 'NONE',  ( 10.38014692360259872, -13.86296647480986977, 31.87445430327215234 ) ) ;
#19454 = CARTESIAN_POINT ( 'NONE',  ( -14.51986452503335734, 21.59086984591841940, 5.125738280916170453 ) ) ;
#19453 = CARTESIAN_POINT ( 'NONE',  ( -2.499999999999996447, -13.08383949353407516, -21.61544600755649626 ) ) ;
#19455 = CARTESIAN_POINT ( 'NONE',  ( 7.886225516951638426, 296.0473068317901379, -10.02775466922195413 ) ) ;
#19456 = CARTESIAN_POINT ( 'NONE',  ( -3.594033448928638741, -9.156975712238445197, 6.225088131883842912 ) ) ;
#19457 = SURFACE_STYLE_USAGE ( .BOTH. , #20534 ) ;
#19458 = AXIS2_PLACEMENT_3D ( 'NONE', #93881, #34614, #76087 ) ;
#19459 = CARTESIAN_POINT ( 'NONE',  ( 7.000000000000000000, 0.000000000000000000, -8.125150395352576993 ) ) ;
#19460 = MECHANICAL_DESIGN_GEOMETRIC_PRESENTATION_REPRESENTATION (  '', ( #98616 ), #93496 ) ;
#19461 = CARTESIAN_POINT ( 'NONE',  ( -2.106019827721631099, -60.00000000000000000, 39.63609690567994903 ) ) ;
#19462 = ORIENTED_EDGE ( 'NONE', *, *, #106511, .T. ) ;
#19463 = CARTESIAN_POINT ( 'NONE',  ( 65.52222222222222570, 3.309500000000014541, 4.052968581778174646E-16 ) ) ;
#19464 = AXIS2_PLACEMENT_3D ( 'NONE', #63611, #65178, #99120 ) ;
#19465 = CARTESIAN_POINT ( 'NONE',  ( -42.76230833568499179, 461.1825766694569211, 3.198895819599639978 ) ) ;
#19466 = EDGE_CURVE ( 'NONE', #16013, #20391, #35535, .T. ) ;
#19468 = CARTESIAN_POINT ( 'NONE',  ( -12.61036987039059909, -34.58958934473714208, -32.31355602543667516 ) ) ;
#19467 = CARTESIAN_POINT ( 'NONE',  ( 9.333892298909278296, 251.7827573162502688, -3.590295303293472795 ) ) ;
#19469 = ORIENTED_EDGE ( 'NONE', *, *, #53088, .T. ) ;
#19470 = CARTESIAN_POINT ( 'NONE',  ( 9.789044728060087408, 294.6486233851415477, -2.043184600578025201 ) ) ;
#19471 = DIRECTION ( 'NONE',  ( 0.000000000000000000, -1.000000000000000000, 0.000000000000000000 ) ) ;
#19473 = ORIENTED_EDGE ( 'NONE', *, *, #84004, .F. ) ;
#19472 = TOROIDAL_SURFACE ( 'NONE', #79706, 57.86910460382442523, 0.5000000000000000000 ) ;
#19474 = EDGE_CURVE ( 'NONE', #9776, #102391, #84653, .T. ) ;
#19475 = LINE ( 'NONE', #96387, #16228 ) ;
#19476 = CYLINDRICAL_SURFACE ( 'NONE', #3562, 4.000000000000000000 ) ;
#19477 = CARTESIAN_POINT ( 'NONE',  ( -91.89519763986371004, -59.99999999999999289, 15.53214387827562248 ) ) ;
#19478 = FACE_OUTER_BOUND ( 'NONE', #67777, .T. ) ;
#19479 = CARTESIAN_POINT ( 'NONE',  ( -8.000000000000000000, -11.74999999999999289, -9.797174393178825657E-16 ) ) ;
#19480 = CARTESIAN_POINT ( 'NONE',  ( 38.98764044590114963, 460.2978347093389289, 2.283752696535007232 ) ) ;
#19481 = CARTESIAN_POINT ( 'NONE',  ( -35.23234612623826223, 435.7070084737468392, 6.197831874882719916 ) ) ;
#19482 = CARTESIAN_POINT ( 'NONE',  ( -80.87283484261959643, -53.41399119864235701, 172.1343020383144449 ) ) ;
#19483 = EDGE_LOOP ( 'NONE', ( #19995, #41372, #49539, #25761 ) ) ;
#19484 = CARTESIAN_POINT ( 'NONE',  ( 8.559508646656407649, -1.200000000000000030E-05, 2.781152949374444461 ) ) ;
#19485 = ORIENTED_EDGE ( 'NONE', *, *, #9204, .F. ) ;
#19486 = EDGE_LOOP ( 'NONE', ( #98849, #19795, #12833, #57901 ) ) ;
#19487 = CARTESIAN_POINT ( 'NONE',  ( -4.460266806907394077, -1.165284401735731112, 104.3906379647731910 ) ) ;
#19488 = CARTESIAN_POINT ( 'NONE',  ( -15.73927229776775150, -4.999999999999999112, -7.856667017201005798 ) ) ;
#19489 = CIRCLE ( 'NONE', #62564, 4.000000000000000888 ) ;
#19490 = SURFACE_STYLE_FILL_AREA ( #100879 ) ;
#19491 = DIRECTION ( 'NONE',  ( 0.000000000000000000, 0.000000000000000000, 1.000000000000000000 ) ) ;
#19492 = ORIENTED_EDGE ( 'NONE', *, *, #6680, .T. ) ;
#19493 =( GEOMETRIC_REPRESENTATION_CONTEXT ( 3 ) GLOBAL_UNCERTAINTY_ASSIGNED_CONTEXT ( ( #30564 ) ) GLOBAL_UNIT_ASSIGNED_CONTEXT ( ( #46710, #104407, #3611 ) ) REPRESENTATION_CONTEXT ( 'NONE', 'WORKASPACE' ) );
#19494 = CARTESIAN_POINT ( 'NONE',  ( 24.83349330513380337, 1.593028355512270567E-15, 0.000000000000000000 ) ) ;
#19495 = CARTESIAN_POINT ( 'NONE',  ( -61.29065067449151627, -57.67115771167040350, -37.35479649122906665 ) ) ;
#19496 = LINE ( 'NONE', #69603, #11151 ) ;
#19497 = CARTESIAN_POINT ( 'NONE',  ( 14.34999999999999787, 3.309500000000003439, 0.000000000000000000 ) ) ;
#19498 = PRESENTATION_LAYER_ASSIGNMENT (  '', '', ( #40086 ) ) ;
#19499 = CARTESIAN_POINT ( 'NONE',  ( 24.46190898409538406, 27.53854914924986730, 31.75601090834086904 ) ) ;
#19500 = CARTESIAN_POINT ( 'NONE',  ( 52.56483885390523625, -79.93083296558610584, -38.23529411764706509 ) ) ;
#19501 = DIRECTION ( 'NONE',  ( 0.000000000000000000, -1.000000000000000000, 0.000000000000000000 ) ) ;
#19502 = MANIFOLD_SOLID_BREP ( 'ThdSchPat', #98043 ) ;
#19503 = CARTESIAN_POINT ( 'NONE',  ( 89.60175727050132366, -14.21045842199443143, 48.51353285324994147 ) ) ;
#19504 = CARTESIAN_POINT ( 'NONE',  ( -88.91591484687975822, -30.00000000000007105, 199.0554621605764680 ) ) ;
#19505 = EDGE_CURVE ( 'NONE', #26189, #63565, #46756, .T. ) ;
#19506 = CARTESIAN_POINT ( 'NONE',  ( -57.09409901914469998, -60.33378115074653891, 74.31118004153825041 ) ) ;
#19507 = ORIENTED_EDGE ( 'NONE', *, *, #94232, .F. ) ;
#19508 = FILL_AREA_STYLE ('',( #28120 ) ) ;
#19509 = ORIENTED_EDGE ( 'NONE', *, *, #98874, .T. ) ;
#19510 = CARTESIAN_POINT ( 'NONE',  ( -101.3127191661065893, -37.82044097410556560, 187.1967937974196445 ) ) ;
#19511 = CARTESIAN_POINT ( 'NONE',  ( 70.89460441624491693, 4.898587196589294500E-16, -4.000000000000007105 ) ) ;
#19512 = DIRECTION ( 'NONE',  ( 1.000000000000000000, 0.000000000000000000, 0.000000000000000000 ) ) ;
#19513 = EDGE_CURVE ( 'NONE', #7688, #76929, #69183, .T. ) ;
#19514 = SURFACE_STYLE_USAGE ( .BOTH. , #27601 ) ;
#19515 = ORIENTED_EDGE ( 'NONE', *, *, #53580, .T. ) ;
#19516 = CARTESIAN_POINT ( 'NONE',  ( 4.205882352941162416, -4.999999999999998224, -72.69916451482997388 ) ) ;
#19517 = CARTESIAN_POINT ( 'NONE',  ( -3.558939058151737722, -1.060970281106035751, 104.4181685828941966 ) ) ;
#19518 = CARTESIAN_POINT ( 'NONE',  ( -1.320432766682874540E-15, -15.40625000204838635, 7.188101187500000044 ) ) ;
#19519 = CARTESIAN_POINT ( 'NONE',  ( 41.85000000000000142, 1.533819458162526451E-15, 0.000000000000000000 ) ) ;
#19520 = CARTESIAN_POINT ( 'NONE',  ( 0.000000000000000000, 29.56666008184760130, -34.51297463494397988 ) ) ;
#19521 = CARTESIAN_POINT ( 'NONE',  ( 16.46930219882285584, 0.000000000000000000, 4.418206560245473646 ) ) ;
#19522 = CARTESIAN_POINT ( 'NONE',  ( -29.01988888469873018, 321.8047804620298393, 14.12772110426748284 ) ) ;
#19523 = CARTESIAN_POINT ( 'NONE',  ( 11.13412560657217654, -11.04925094343736269, 10.14712091588952347 ) ) ;
#19524 = EDGE_CURVE ( 'NONE', #71082, #10644, #53612, .T. ) ;
#19525 = CARTESIAN_POINT ( 'NONE',  ( 4.898587196589412829E-16, -15.31250000409677092, -8.000000000000000000 ) ) ;
#19526 = CARTESIAN_POINT ( 'NONE',  ( -7.500000000000000000, -6.192646671729328922, -14.54134196042664229 ) ) ;
#19527 = CARTESIAN_POINT ( 'NONE',  ( -31.88729338067515684, -56.85255422488128829, 36.98592566769335832 ) ) ;
#19528 =( NAMED_UNIT ( * ) SI_UNIT ( $, .STERADIAN. ) SOLID_ANGLE_UNIT ( ) );
#19529 = CARTESIAN_POINT ( 'NONE',  ( 44.90564540012300654, -49.89129374844679177, 46.32480369452557767 ) ) ;
#19530 = LINE ( 'NONE', #101984, #5894 ) ;
#19531 = CARTESIAN_POINT ( 'NONE',  ( -5.763785242774021711, 13.53591622817248563, 3.972758706198395551 ) ) ;
#19532 = CARTESIAN_POINT ( 'NONE',  ( -98.37152973009548873, -38.47865734070185084, 200.9152500599649613 ) ) ;
#19533 = ORIENTED_EDGE ( 'NONE', *, *, #87071, .F. ) ;
#19535 = CARTESIAN_POINT ( 'NONE',  ( 10.73176661990081371, 6.123233995736770227E-16, -5.000000000000002665 ) ) ;
#19534 = CARTESIAN_POINT ( 'NONE',  ( 42.69811214730273718, 434.9611672192513652, 18.34625614733210242 ) ) ;
#19536 = CARTESIAN_POINT ( 'NONE',  ( 11.55846695675572455, 7.296715529366291975, -9.344306654786388222 ) ) ;
#19537 = CARTESIAN_POINT ( 'NONE',  ( -49.03380706566419889, 8.971284072415123489, -14.85953237006457783 ) ) ;
#19538 = CARTESIAN_POINT ( 'NONE',  ( -7.425374667685089136, 41.07993512976541695, -59.67056295168852387 ) ) ;
#19539 = CARTESIAN_POINT ( 'NONE',  ( 6.190137450539002550, 41.32597165365250191, -70.92513721826038875 ) ) ;
#19540 = CARTESIAN_POINT ( 'NONE',  ( 1.592040838891563829E-15, -100.0000000000000000, 13.00000000000003730 ) ) ;
#19542 = CARTESIAN_POINT ( 'NONE',  ( 42.18756898894580587, 484.4522853017719513, -2.425645685620450909 ) ) ;
#19541 = AXIS2_PLACEMENT_3D ( 'NONE', #48891, #73163, #8447 ) ;
#19543 = CARTESIAN_POINT ( 'NONE',  ( 0.000000000000000000, 0.000000000000000000, 0.000000000000000000 ) ) ;
#19544 = CARTESIAN_POINT ( 'NONE',  ( 111.2710224913295605, -59.99999999999998579, 185.8464216051011135 ) ) ;
#19545 = AXIS2_PLACEMENT_3D ( 'NONE', #5378, #69060, #79252 ) ;
#19546 = AXIS2_PLACEMENT_3D ( 'NONE', #19076, #36326, #26115 ) ;
#19547 = FACE_OUTER_BOUND ( 'NONE', #55005, .T. ) ;
#19548 = ORIENTED_EDGE ( 'NONE', *, *, #72802, .F. ) ;
#19549 = EDGE_CURVE ( 'NONE', #102469, #65829, #18400, .T. ) ;
#19550 = CARTESIAN_POINT ( 'NONE',  ( 3.052800042147939319, -49.15628846935693730, 104.0321489743691501 ) ) ;
#19551 = CARTESIAN_POINT ( 'NONE',  ( -81.58798209278842251, -30.00000000000000000, -7.591802554973769546 ) ) ;
#19552 = ORIENTED_EDGE ( 'NONE', *, *, #65922, .F. ) ;
#19554 = CARTESIAN_POINT ( 'NONE',  ( -9.113097280746996987, -54.00000000000000711, 31.11721482942554928 ) ) ;
#19553 = SURFACE_STYLE_USAGE ( .BOTH. , #102007 ) ;
#19555 = CARTESIAN_POINT ( 'NONE',  ( 12.48544000261163944, -3.553614324104685807, -13.69205050333947327 ) ) ;
#19556 = CARTESIAN_POINT ( 'NONE',  ( -8.000000000000001776, -3.000000000000000444, 1.047197551196596077 ) ) ;
#19557 = DIRECTION ( 'NONE',  ( 1.000000000000000000, 1.224606353822377258E-16, 0.000000000000000000 ) ) ;
#19558 = AXIS2_PLACEMENT_3D ( 'NONE', #90471, #32793, #65132 ) ;
#19559 = CARTESIAN_POINT ( 'NONE',  ( -7.188101187500000044, -14.28125000204838457, -8.802885111219163269E-16 ) ) ;
#19560 = CARTESIAN_POINT ( 'NONE',  ( 11.99999999999999467, -5.000000000000002665, -86.57079632498522415 ) ) ;
#19561 = EDGE_CURVE ( 'NONE', #60305, #84586, #14923, .T. ) ;
#19562 = PLANE ( 'NONE',  #81011 ) ;
#19564 = ORIENTED_EDGE ( 'NONE', *, *, #55334, .T. ) ;
#19563 = CARTESIAN_POINT ( 'NONE',  ( 0.000000000000000000, 45.00000000000000711, 0.000000000000000000 ) ) ;
#19565 = CARTESIAN_POINT ( 'NONE',  ( 83.69477321491778810, -29.06518311407809563, 159.7595627650821655 ) ) ;
#19566 = CARTESIAN_POINT ( 'NONE',  ( 83.86866073052654258, -5.000000000000000000, 6.123233995736778115E-16 ) ) ;
#19567 = LINE ( 'NONE', #29250, #5813 ) ;
#19568 = ORIENTED_EDGE ( 'NONE', *, *, #5278, .F. ) ;
#19569 = ADVANCED_FACE ( 'NONE', ( #39759 ), #56975, .T. ) ;
#19570 = CARTESIAN_POINT ( 'NONE',  ( -32.92521947952602090, 485.8269030686984706, 5.191998501979409930 ) ) ;
#19572 = EDGE_CURVE ( 'NONE', #29309, #99399, #74307, .T. ) ;
#19571 = AXIS2_PLACEMENT_3D ( 'NONE', #56907, #89830, #23531 ) ;
#19573 = CARTESIAN_POINT ( 'NONE',  ( 17.51155336591212830, 34.75093603301226608, 22.05173959547846252 ) ) ;
#19574 =( NAMED_UNIT ( * ) PLANE_ANGLE_UNIT ( ) SI_UNIT ( $, .RADIAN. ) );
#19575 = CARTESIAN_POINT ( 'NONE',  ( 0.5805565836007618996, 3.752776749732569250, 6.499999999999997335 ) ) ;
#19576 = CARTESIAN_POINT ( 'NONE',  ( -4.472135954999578722, 250.2707722006736049, 3.999999999999999112 ) ) ;
#19578 = CARTESIAN_POINT ( 'NONE',  ( 0.8348441572799575328, 18.10288867187672324, 49.56646071010256094 ) ) ;
#19577 = CONICAL_SURFACE ( 'NONE', #76324, 4.000000000000007105, 0.9599310885968835860 ) ;
#19579 = DIRECTION ( 'NONE',  ( -1.000000000000000000, -1.224606353822377258E-16, -0.000000000000000000 ) ) ;
#19580 = ORIENTED_EDGE ( 'NONE', *, *, #41468, .F. ) ;
#19581 =( GEOMETRIC_REPRESENTATION_CONTEXT ( 3 ) GLOBAL_UNCERTAINTY_ASSIGNED_CONTEXT ( ( #81258 ) ) GLOBAL_UNIT_ASSIGNED_CONTEXT ( ( #96212, #14728, #15275 ) ) REPRESENTATION_CONTEXT ( 'NONE', 'WORKASPACE' ) );
#19582 = CIRCLE ( 'NONE', #64350, 9.999999999999994671 ) ;
#19583 = CARTESIAN_POINT ( 'NONE',  ( -3.042178694127982475, 300.3091518900824326, 9.528975082528521767 ) ) ;
#19584 = CARTESIAN_POINT ( 'NONE',  ( 2.245730763532626462, 18.64284798592908032, 38.36507033181725035 ) ) ;
#19585 = CARTESIAN_POINT ( 'NONE',  ( 86.89309887720403935, -60.97679280612473462, 194.8801408971697811 ) ) ;
#19587 = CARTESIAN_POINT ( 'NONE',  ( -13.02995514262170396, 6.128988252786461643, -7.304746880288981892 ) ) ;
#19586 = DIRECTION ( 'NONE',  ( -1.000000000000000000, -0.000000000000000000, -0.000000000000000000 ) ) ;
#19588 = CARTESIAN_POINT ( 'NONE',  ( -7.188101187500000044, -27.40625000204838813, -8.802885111219163269E-16 ) ) ;
#19589 = DIRECTION ( 'NONE',  ( 0.2270551762890646308, 0.1092888915761187629, 0.9677302749725282816 ) ) ;
#19590 = CARTESIAN_POINT ( 'NONE',  ( 16.08349330513380337, 1.593028355512270962E-15, 0.000000000000000000 ) ) ;
#19591 = SURFACE_STYLE_USAGE ( .BOTH. , #101523 ) ;
#19592 = CONTEXT_DEPENDENT_SHAPE_REPRESENTATION ( #101770, #21029 ) ;
#19593 = ORIENTED_EDGE ( 'NONE', *, *, #2047, .T. ) ;
#19594 = CARTESIAN_POINT ( 'NONE',  ( 46.84999999999999432, -3.309499999999999886, 0.000000000000000000 ) ) ;
#19595 = CARTESIAN_POINT ( 'NONE',  ( -10.16823181764058859, 7.259740064965935602, 0.000000000000000000 ) ) ;
#19596 = DIRECTION ( 'NONE',  ( -1.000000000000000000, -1.224606353822377258E-16, -0.000000000000000000 ) ) ;
#19597 = ADVANCED_FACE ( 'NONE', ( #95871 ), #104474, .F. ) ;
#19598 = B_SPLINE_CURVE_WITH_KNOTS ( 'NONE', 3,
 ( #37273, #15474, #48887, #31171, #7904, #48366, #24142, #30631, #16010, #64055, #28652, #20591, #31688, #56984, #53430, #72648, #86348, #40809, #61538, #70139, #12414, #81259, #55391, #88321, #7372, #64574, #14934, #47827, #106062, #94430, #45345, #78224, #23066, #72121, #6849, #23601, #81780, #73704, #63521, #65091, #96418, #14394, #22549, #32212, #47306, #80202, #80732, #97988, #39247, #89900, #105030, #97440, #96930, #55904, #88840, #39773, #56450, #89383, #42405, #58053, #66690, #50483, #92554, #1393, #51559, #99032, #90976, #25750, #18703, #1937 ),
 .UNSPECIFIED., .F., .F.,
 ( 4, 2, 2, 2, 2, 2, 2, 2, 2, 2, 2, 2, 2, 2, 2, 2, 2, 2, 2, 2, 2, 2, 2, 2, 2, 2, 2, 2, 2, 2, 2, 2, 2, 2, 4 ),
 ( 0.1516340706156730500, 0.1524580149623166181, 0.1532819593089602139, 0.1541059036556037820, 0.1549298480022473501, 0.1565777366955345140, 0.1582256253888216779, 0.1598735140821088418, 0.1615214027753959780, 0.1648171801619703891, 0.1714087349351192668, 0.1780002897082681723, 0.1845918444814170500, 0.1911833992545659555, 0.2043665088008637110, 0.2175496183471614942, 0.2307327278934592774, 0.2570989469860547327, 0.2834651660786502436, 0.2966482756249478880, 0.3098313851712456435, 0.3230144947175433434, 0.3296060494906922211, 0.3361976042638411544, 0.3394933816504155377, 0.3427891590369899766, 0.3460849364235644154, 0.3493807138101388543, 0.3526764911967132932, 0.3559722685832876765, 0.3576201572765749237, 0.3592680459698621709, 0.3609159346631494181, 0.3617398790097929862, 0.3625638233564366097 ),
 .UNSPECIFIED. ) ;
#19599 = VERTEX_POINT ( 'NONE', #105018 ) ;
#19600 = CARTESIAN_POINT ( 'NONE',  ( -7.346560218009842380, 52.17944658692381665, -2.467458042133138907 ) ) ;
#19601 = CARTESIAN_POINT ( 'NONE',  ( 8.904581707872910812, 48.00000000000000000, -97.29851715190937966 ) ) ;
#19602 = ADVANCED_FACE ( 'NONE', ( #64044 ), #26102, .F. ) ;
#19603 = CARTESIAN_POINT ( 'NONE',  ( 32.82178245385870952, 434.5289685218765499, 16.70197725476643313 ) ) ;
#19604 = CARTESIAN_POINT ( 'NONE',  ( -1.469576158976823947E-15, -22.06250000409676915, 8.000000000000000000 ) ) ;
#19605 = CARTESIAN_POINT ( 'NONE',  ( 46.36650669486618881, -3.999999999999998224, 0.000000000000000000 ) ) ;
#19606 = CARTESIAN_POINT ( 'NONE',  ( -17.77146113466401545, 36.31761464240112502, 23.79974184213090638 ) ) ;
#19607 = CARTESIAN_POINT ( 'NONE',  ( -98.33757392241099637, -59.99999999999999289, 202.2807768545189901 ) ) ;
#19608 = CYLINDRICAL_SURFACE ( 'NONE', #60018, 10.00000000000000178 ) ;
#19609 = MECHANICAL_DESIGN_GEOMETRIC_PRESENTATION_REPRESENTATION (  '', ( #12612 ), #83222 ) ;
#19610 = DIRECTION ( 'NONE',  ( 0.5735764363510442720, -0.8191520442889930198, 1.003171929053526349E-16 ) ) ;
#19611 = FACE_OUTER_BOUND ( 'NONE', #62640, .T. ) ;
#19612 = DIRECTION ( 'NONE',  ( 0.000000000000000000, -0.8813945903476978483, 0.4723807533185641061 ) ) ;
#19613 = B_SPLINE_CURVE_WITH_KNOTS ( 'NONE', 3,
 ( #19534, #83672, #43235, #9780 ),
 .UNSPECIFIED., .F., .F.,
 ( 4, 4 ),
 ( 1.868354362588067661E-17, 0.001851782051266549116 ),
 .UNSPECIFIED. ) ;
#19614 = CARTESIAN_POINT ( 'NONE',  ( -86.40361593247554595, -17.81809089641515698, 175.1979029344232401 ) ) ;
#19615 = STYLED_ITEM ( 'NONE', ( #30192 ), #84617 ) ;
#19616 = AXIS2_PLACEMENT_3D ( 'NONE', #33791, #74738, #67213 ) ;
#19617 = EDGE_LOOP ( 'NONE', ( #52323, #74745, #71035, #73224, #20201 ) ) ;
#19618 = CARTESIAN_POINT ( 'NONE',  ( -19.96162532426521352, 302.8116070918646301, 9.928455558879880627 ) ) ;
#19619 = EDGE_CURVE ( 'NONE', #27686, #5290, #94985, .T. ) ;
#19620 = CARTESIAN_POINT ( 'NONE',  ( 0.9999999999999997780, -51.24679913438006196, 3.817907945688783666 ) ) ;
#19621 = CARTESIAN_POINT ( 'NONE',  ( -85.02495788024697276, -52.70069914093267016, 6.451521919501416846 ) ) ;
#19622 = FACE_OUTER_BOUND ( 'NONE', #67272, .T. ) ;
#19623 = FILL_AREA_STYLE_COLOUR ( '', #51310 ) ;
#19624 = CARTESIAN_POINT ( 'NONE',  ( 4.322723262674379896, 141.1105290361839479, -4.999999999999999112 ) ) ;
#19625 = CARTESIAN_POINT ( 'NONE',  ( -6.437509419382472231, -11.87447412552791448, 10.48822171390120950 ) ) ;
#19626 = CARTESIAN_POINT ( 'NONE',  ( -51.76085035121451483, 41.99999999999999289, -29.83308852628634966 ) ) ;
#19627 = CARTESIAN_POINT ( 'NONE',  ( 74.83543306973328413, -14.21045842199438347, 137.5190812362815791 ) ) ;
#19628 = CARTESIAN_POINT ( 'NONE',  ( -33.83237027343564307, 58.72416816948007323, 16.91618513671782154 ) ) ;
#19629 = CARTESIAN_POINT ( 'NONE',  ( -89.66619014120909981, -60.00000000000001421, -23.31631894612182521 ) ) ;
#19630 = CARTESIAN_POINT ( 'NONE',  ( -73.98086237266396381, -29.07117432108940491, 109.2040377524712937 ) ) ;
#19631 = ORIENTED_EDGE ( 'NONE', *, *, #85297, .F. ) ;
#19632 = CARTESIAN_POINT ( 'NONE',  ( 103.2152402541460248, -59.99999999999995026, 203.2731761476304655 ) ) ;
#19633 = CARTESIAN_POINT ( 'NONE',  ( -64.12663816132096883, 40.83928107889916959, -11.02910957313798868 ) ) ;
#19634 = CARTESIAN_POINT ( 'NONE',  ( 77.07421096609712663, -57.67120363626943202, -31.72031775925474761 ) ) ;
#19635 = VERTEX_POINT ( 'NONE', #75290 ) ;
#19636 = CARTESIAN_POINT ( 'NONE',  ( 14.32310282642602850, -7.975991125463504083, 12.70685702462689193 ) ) ;
#19637 = CARTESIAN_POINT ( 'NONE',  ( 7.188101187500000933, -25.43750000204838457, -2.977408999572650483 ) ) ;
#19638 = DIRECTION ( 'NONE',  ( -1.000000000000000000, -1.224606353822377258E-16, -0.000000000000000000 ) ) ;
#19639 = ORIENTED_EDGE ( 'NONE', *, *, #72345, .T. ) ;
#19640 = CARTESIAN_POINT ( 'NONE',  ( 26.08349330513380337, -4.000000000000000000, 4.898587196589415787E-16 ) ) ;
#19641 = ORIENTED_EDGE ( 'NONE', *, *, #16241, .T. ) ;
#19642 = CARTESIAN_POINT ( 'NONE',  ( 61.37206225042174879, 6.856755485862130937E-15, 0.000000000000000000 ) ) ;
#19643 = MECHANICAL_DESIGN_GEOMETRIC_PRESENTATION_REPRESENTATION (  '', ( #14410 ), #95422 ) ;
#19644 = CARTESIAN_POINT ( 'NONE',  ( 46.86921974295913884, 18.15560460139400689, -16.08157171274295649 ) ) ;
#19645 = CARTESIAN_POINT ( 'NONE',  ( -29.73016315324071712, -60.00000000000618172, 45.54566534438918524 ) ) ;
#19646 = LINE ( 'NONE', #36879, #31263 ) ;
#19647 = CARTESIAN_POINT ( 'NONE',  ( 5.082755093536324154, -30.21875000204838813, 5.082755093536326818 ) ) ;
#19648 = CARTESIAN_POINT ( 'NONE',  ( -49.27995299967503939, 13.03636147101657983, 15.63012893016903249 ) ) ;
#19649 = CARTESIAN_POINT ( 'NONE',  ( 16.66764709352487728, -4.285714285714295357, -19.00223544648543950 ) ) ;
#19650 = CARTESIAN_POINT ( 'NONE',  ( -9.596002107488990518, 50.00000000000000000, -92.37456064098950037 ) ) ;
#19651 = DIRECTION ( 'NONE',  ( 1.000000000000000000, 1.224606353822377258E-16, 0.000000000000000000 ) ) ;
#19652 = EDGE_CURVE ( 'NONE', #26711, #66185, #54408, .T. ) ;
#19653 = SURFACE_SIDE_STYLE ('',( #87010 ) ) ;
#19654 = UNCERTAINTY_MEASURE_WITH_UNIT (LENGTH_MEASURE( 1.000000000000000082E-05 ), #16646, 'distance_accuracy_value', 'NONE');
#19655 = CIRCLE ( 'NONE', #78183, 6.999999999999992895 ) ;
#19656 = ORIENTED_EDGE ( 'NONE', *, *, #102470, .T. ) ;
#19657 = CARTESIAN_POINT ( 'NONE',  ( 4.750186375024371799, -1.378107633083520911, 104.3180500829679289 ) ) ;
#19658 = AXIS2_PLACEMENT_3D ( 'NONE', #5969, #22732, #13533 ) ;
#19660 = CARTESIAN_POINT ( 'NONE',  ( 30.72324318598429116, -22.13081174256386419, 30.23699920491905857 ) ) ;
#19659 = CARTESIAN_POINT ( 'NONE',  ( -3.460324465703970453, -48.83451908470669878, 104.5902739980974161 ) ) ;
#19661 = FACE_OUTER_BOUND ( 'NONE', #21259, .T. ) ;
#19662 = ORIENTED_EDGE ( 'NONE', *, *, #77900, .F. ) ;
#19663 = DIRECTION ( 'NONE',  ( 0.000000000000000000, 1.000000000000000000, 0.000000000000000000 ) ) ;
#19664 = CARTESIAN_POINT ( 'NONE',  ( -35.69739812508499455, 430.4862580793411553, 4.964222856391316441 ) ) ;
#19665 = FACE_OUTER_BOUND ( 'NONE', #16995, .T. ) ;
#19666 = CARTESIAN_POINT ( 'NONE',  ( -43.09948196127317033, 484.9577458347782226, -0.8563396247089051228 ) ) ;
#19667 = CARTESIAN_POINT ( 'NONE',  ( 32.65804572401750505, 465.7880960007718727, 12.84163515238255826 ) ) ;
#19668 = CARTESIAN_POINT ( 'NONE',  ( -34.63438812788589871, 463.6460534741191282, 19.43326544948470769 ) ) ;
#19669 = VERTEX_POINT ( 'NONE', #50475 ) ;
#19670 = CARTESIAN_POINT ( 'NONE',  ( 92.60551233582847885, -60.00000000000001421, -2.887494206137121822 ) ) ;
#19671 = DIRECTION ( 'NONE',  ( -0.5735764363510461594, 0.8191520442889916875, 1.003171929053524870E-16 ) ) ;
#19672 = CARTESIAN_POINT ( 'NONE',  ( 17.35892867067943257, 294.5707697310705839, -10.05973541782409342 ) ) ;
#19673 = CARTESIAN_POINT ( 'NONE',  ( -5.548191825034886726, 40.55407105498441211, -71.04437881643139008 ) ) ;
#19674 = CARTESIAN_POINT ( 'NONE',  ( -47.29386731606042815, 18.29473622529003762, -14.58939859131310790 ) ) ;
#19675 = ORIENTED_EDGE ( 'NONE', *, *, #28448, .T. ) ;
#19676 = ADVANCED_FACE ( 'NONE', ( #58596 ), #58387, .F. ) ;
#19677 = CARTESIAN_POINT ( 'NONE',  ( -108.1305341385797192, -30.00000000011948842, 149.1718095810573459 ) ) ;
#19678 = ORIENTED_EDGE ( 'NONE', *, *, #25782, .T. ) ;
#19679 = CARTESIAN_POINT ( 'NONE',  ( 0.000000000000000000, 2.253471898105741801E-15, 6.500000000000000000 ) ) ;
#19680 = PRESENTATION_STYLE_ASSIGNMENT (( #29356 ) ) ;
#19681 = DIRECTION ( 'NONE',  ( 0.000000000000000000, 0.000000000000000000, 1.000000000000000000 ) ) ;
#19682 = CARTESIAN_POINT ( 'NONE',  ( 16.10370002540634360, 21.82456013744149814, 0.8668566225193951036 ) ) ;
#19683 = CARTESIAN_POINT ( 'NONE',  ( 84.43992632049143765, -45.28489048329945632, -8.688217668655392245 ) ) ;
#19684 = CARTESIAN_POINT ( 'NONE',  ( -38.86088754547002111, 310.5264066565887333, 1.725813668771058351 ) ) ;
#19685 = DIRECTION ( 'NONE',  ( 0.000000000000000000, 0.000000000000000000, -1.000000000000000000 ) ) ;
#19686 = EDGE_CURVE ( 'NONE', #44057, #97033, #48878, .T. ) ;
#19687 = CARTESIAN_POINT ( 'NONE',  ( -17.52413350827921690, 45.00000000000000000, 63.50693744801557017 ) ) ;
#19688 =( LENGTH_UNIT ( ) NAMED_UNIT ( * ) SI_UNIT ( .MILLI., .METRE. ) );
#19689 = VERTEX_POINT ( 'NONE', #41864 ) ;
#19691 = EDGE_CURVE ( 'NONE', #59863, #65026, #82706, .T. ) ;
#19690 = CARTESIAN_POINT ( 'NONE',  ( -6.499999999998818723, -2.692912473540151286, -6.218066308271905207 ) ) ;
#19692 = EDGE_LOOP ( 'NONE', ( #78633, #93442, #76260, #94962 ) ) ;
#19693 = CARTESIAN_POINT ( 'NONE',  ( 17.50000000000002842, 46.00000000000000000, 64.09953197959339377 ) ) ;
#19694 = FACE_OUTER_BOUND ( 'NONE', #49191, .T. ) ;
#19695 =( GEOMETRIC_REPRESENTATION_CONTEXT ( 3 ) GLOBAL_UNCERTAINTY_ASSIGNED_CONTEXT ( ( #29806 ) ) GLOBAL_UNIT_ASSIGNED_CONTEXT ( ( #47658, #100995, #85351 ) ) REPRESENTATION_CONTEXT ( 'NONE', 'WORKASPACE' ) );
#19697 = ORIENTED_EDGE ( 'NONE', *, *, #24682, .T. ) ;
#19696 = CARTESIAN_POINT ( 'NONE',  ( 6.068575646150123681, 51.26875262032900338, 8.262755242866147043 ) ) ;
#19698 = CARTESIAN_POINT ( 'NONE',  ( 72.46319062493193996, -18.64354067297488626, 97.55174160385824678 ) ) ;
#19699 = EDGE_LOOP ( 'NONE', ( #8936, #54347, #12773, #34922, #35928 ) ) ;
#19700 = EDGE_CURVE ( 'NONE', #54845, #56071, #28387, .T. ) ;
#19701 = CARTESIAN_POINT ( 'NONE',  ( 3.638102518737710955, -49.00949705677293622, 43.87169722584302889 ) ) ;
#19702 = CARTESIAN_POINT ( 'NONE',  ( -5.082755093536325042, -23.09375000204838457, -5.082755093536325930 ) ) ;
#19703 = CARTESIAN_POINT ( 'NONE',  ( -82.32950074003311158, -57.52534511946047502, 200.7509962287250573 ) ) ;
#19704 = ORIENTED_EDGE ( 'NONE', *, *, #21526, .F. ) ;
#19705 = CARTESIAN_POINT ( 'NONE',  ( 0.000000000000000000, 0.000000000000000000, 0.000000000000000000 ) ) ;
#19706 = CARTESIAN_POINT ( 'NONE',  ( 105.2866863118581904, -52.71709848458299064, 172.7927270732103011 ) ) ;
#19707 = CARTESIAN_POINT ( 'NONE',  ( -29.68315524076957246, 18.29184282782463455, 39.60535821593508388 ) ) ;
#19708 = DIRECTION ( 'NONE',  ( 0.000000000000000000, 1.000000000000000000, 0.000000000000000000 ) ) ;
#19709 = CARTESIAN_POINT ( 'NONE',  ( 8.000000000000000000, -20.18750000409677270, 0.000000000000000000 ) ) ;
#19710 = CARTESIAN_POINT ( 'NONE',  ( -49.54953808143496730, -29.59979831508751502, 45.90118066601930735 ) ) ;
#19711 = CARTESIAN_POINT ( 'NONE',  ( 9.797936955406328252, 246.5332831022951154, -2.012343231877608218 ) ) ;
#19712 = CARTESIAN_POINT ( 'NONE',  ( 0.000000000000000000, 0.000000000000000000, -13.00000000000000000 ) ) ;
#19713 = CARTESIAN_POINT ( 'NONE',  ( 9.165151389911681434, 30.00000000000000000, -4.000000000000000000 ) ) ;
#19714 = DIRECTION ( 'NONE',  ( -1.000000000000000000, 0.000000000000000000, 0.000000000000000000 ) ) ;
#19716 = CIRCLE ( 'NONE', #105806, 8.000000000000007105 ) ;
#19715 = DIRECTION ( 'NONE',  ( 1.000000000000000000, 0.000000000000000000, 0.000000000000000000 ) ) ;
#19717 = CYLINDRICAL_SURFACE ( 'NONE', #71141, 15.00000000000000711 ) ;
#19718 = ORIENTED_EDGE ( 'NONE', *, *, #21824, .T. ) ;
#19719 = CARTESIAN_POINT ( 'NONE',  ( -3.737791945709141306, -48.91906356597342409, 43.79597853662111362 ) ) ;
#19720 = CARTESIAN_POINT ( 'NONE',  ( 72.11682663846713126, 6.975173280561618775E-15, 0.000000000000000000 ) ) ;
#19721 = DIRECTION ( 'NONE',  ( -1.000000000000000000, -1.224606353822377258E-16, -0.000000000000000000 ) ) ;
#19722 = CIRCLE ( 'NONE', #60952, 3.000000000000000000 ) ;
#19723 = CARTESIAN_POINT ( 'NONE',  ( -87.78673640380277732, -29.99999999999999645, 186.2301084186935043 ) ) ;
#19724 = EDGE_CURVE ( 'NONE', #54493, #12412, #69357, .T. ) ;
#19725 = AXIS2_PLACEMENT_3D ( 'NONE', #106655, #105597, #88894 ) ;
#19726 = ORIENTED_EDGE ( 'NONE', *, *, #93469, .F. ) ;
#19727 = DIRECTION ( 'NONE',  ( 0.000000000000000000, 0.000000000000000000, 1.000000000000000000 ) ) ;
#19728 = CARTESIAN_POINT ( 'NONE',  ( 75.21600497976655220, -57.56879808408343990, 191.2544865931707818 ) ) ;
#19729 = CARTESIAN_POINT ( 'NONE',  ( 9.739726766683153514, 47.99999999999999289, -82.38252115640719353 ) ) ;
#19730 = ADVANCED_FACE ( 'NONE', ( #19253 ), #39387, .T. ) ;
#19731 = EDGE_CURVE ( 'NONE', #67017, #5193, #50291, .T. ) ;
#19732 = CARTESIAN_POINT ( 'NONE',  ( 46.86030329039765974, -34.82990584059800909, -36.63149063538335781 ) ) ;
#19733 = DIRECTION ( 'NONE',  ( 0.000000000000000000, -1.000000000000000000, 0.000000000000000000 ) ) ;
#19734 = CARTESIAN_POINT ( 'NONE',  ( 9.739726766683153514, -3.000000000000002665, -87.61747884359279226 ) ) ;
#19735 = CARTESIAN_POINT ( 'NONE',  ( -71.71190387867660831, -60.00000000000000711, 152.1791357730885181 ) ) ;
#19736 = CARTESIAN_POINT ( 'NONE',  ( -23.99113157947469332, 50.00000000000000000, -74.11764705882353610 ) ) ;
#19737 =( NAMED_UNIT ( * ) PLANE_ANGLE_UNIT ( ) SI_UNIT ( $, .RADIAN. ) );
#19738 = CARTESIAN_POINT ( 'NONE',  ( -86.65346022717083940, -42.80895526278556673, 189.4114321490026782 ) ) ;
#19739 = EDGE_LOOP ( 'NONE', ( #61165, #82720, #3370, #69486, #98137 ) ) ;
#19740 = CARTESIAN_POINT ( 'NONE',  ( 30.64007947709951196, 12.99638611018202283, 41.66214316769377746 ) ) ;
#19741 = CARTESIAN_POINT ( 'NONE',  ( -0.9879027795118733302, -22.06787372868864594, 27.56762891438381402 ) ) ;
#19742 = CARTESIAN_POINT ( 'NONE',  ( -6.434577627411612433, 41.95046723496767527, -59.72043439058787584 ) ) ;
#19743 = PRESENTATION_STYLE_ASSIGNMENT (( #25710 ) ) ;
#19744 = B_SPLINE_SURFACE_WITH_KNOTS ( 'NONE', 1, 3, ( 
 ( #60428, #93306, #61483, #100317, #20539, #59353, #101915, #36701 ),
 ( #69564, #11293, #60944, #76569, #26478, #2682, #36173, #67961 ) ),
 .UNSPECIFIED., .F., .F., .F.,
 ( 2, 2 ),
 ( 4, 2, 2, 4 ),
 ( 0.000000000000000000, 1.000000000000000000 ),
 ( 0.000000000000000000, 0.04450745600790868145, 0.06676118401186306728, 0.08901491201581737678 ),
 .UNSPECIFIED. ) ;
#19746 = CARTESIAN_POINT ( 'NONE',  ( 55.74444444444444713, 3.309500000000014541, 0.000000000000000000 ) ) ;
#19745 = CARTESIAN_POINT ( 'NONE',  ( -33.70641995125998136, 301.3514140349557238, 3.410652409991425049 ) ) ;
#19747 = ORIENTED_EDGE ( 'NONE', *, *, #95409, .F. ) ;
#19748 = EDGE_CURVE ( 'NONE', #43603, #100209, #95716, .T. ) ;
#19750 = CARTESIAN_POINT ( 'NONE',  ( 32.61650669486618881, -3.851859888774471706E-31, 4.000000000000000888 ) ) ;
#19749 = AXIS2_PLACEMENT_3D ( 'NONE', #33556, #25484, #9245 ) ;
#19751 = CARTESIAN_POINT ( 'NONE',  ( 6.162888688655346670, -3.752776749732575468, -6.499999999999999112 ) ) ;
#19752 = CARTESIAN_POINT ( 'NONE',  ( 0.4142243125050798502, 28.18107813451710442, 38.31766717693767532 ) ) ;
#19753 = CARTESIAN_POINT ( 'NONE',  ( 62.59428447264396311, 6.856755485862130937E-15, 0.000000000000000000 ) ) ;
#19754 = CARTESIAN_POINT ( 'NONE',  ( 25.63523488843089737, 295.8087761051020834, -1.794239459488054633 ) ) ;
#19755 = CARTESIAN_POINT ( 'NONE',  ( 42.09210974227526947, 317.4093497706929270, -4.557617623460385126 ) ) ;
#19756 = EDGE_CURVE ( 'NONE', #78368, #71944, #93034, .T. ) ;
#19757 = CARTESIAN_POINT ( 'NONE',  ( 10.50000000000000711, -5.000000000000000000, -77.33514508527181874 ) ) ;
#19758 = FILL_AREA_STYLE_COLOUR ( '', #4836 ) ;
#19759 = CARTESIAN_POINT ( 'NONE',  ( 104.0150978814680940, -30.00000000000001421, 120.6686366764556766 ) ) ;
#19760 = CARTESIAN_POINT ( 'NONE',  ( -82.07466008940585311, -29.09322732867462946, 147.4984060422640368 ) ) ;
#19761 = CONICAL_SURFACE ( 'NONE', #79984, 3.309500000000001663, 0.9599310885968770357 ) ;
#19762 = VERTEX_POINT ( 'NONE', #64445 ) ;
#19763 = CARTESIAN_POINT ( 'NONE',  ( -5.000000000000000000, 0.000000000000000000, -7.131971428571428184 ) ) ;
#19764 = CYLINDRICAL_SURFACE ( 'NONE', #53966, 8.000000000000000000 ) ;
#19765 = FILL_AREA_STYLE_COLOUR ( '', #85087 ) ;
#19766 = PRESENTATION_LAYER_ASSIGNMENT (  '', '', ( #88623 ) ) ;
#19767 = AXIS2_PLACEMENT_3D ( 'NONE', #7068, #63743, #96629 ) ;
#19768 =( REPRESENTATION_RELATIONSHIP ('NONE','NONE', #69581, #55690 ) REPRESENTATION_RELATIONSHIP_WITH_TRANSFORMATION ( #2813 )SHAPE_REPRESENTATION_RELATIONSHIP( ) );
#19769 = CARTESIAN_POINT ( 'NONE',  ( 6.562874270078300043, -3.301808241302750080, -6.845811579416826831 ) ) ;
#19770 = CARTESIAN_POINT ( 'NONE',  ( 39.80833478160801064, 313.8620429462365564, 2.567395400256364812 ) ) ;
#19771 = DIRECTION ( 'NONE',  ( 0.000000000000000000, 0.000000000000000000, -1.000000000000000000 ) ) ;
#19772 = ORIENTED_EDGE ( 'NONE', *, *, #103415, .T. ) ;
#19773 = CARTESIAN_POINT ( 'NONE',  ( -3.587928128302542596, 304.8518027750386636, 9.936999415048941131 ) ) ;
#19774 = FACE_BOUND ( 'NONE', #13396, .T. ) ;
#19775 = CARTESIAN_POINT ( 'NONE',  ( -7.188101187500002709, -28.81250000204838457, 2.977408999572648707 ) ) ;
#19776 = ORIENTED_EDGE ( 'NONE', *, *, #72763, .F. ) ;
#19777 = CARTESIAN_POINT ( 'NONE',  ( 6.123233995736772199E-16, 15.00000000000000000, 9.999999999999998224 ) ) ;
#19778 = CARTESIAN_POINT ( 'NONE',  ( -10.00000000000000355, 85.00000000000000000, -4.000000000000000000 ) ) ;
#19779 = CARTESIAN_POINT ( 'NONE',  ( 43.69716417795766006, 49.99999999997997691, 48.48761666245326296 ) ) ;
#19780 = CARTESIAN_POINT ( 'NONE',  ( -8.000000000000001776, -17.65624999999999645, 3.313708498984759387 ) ) ;
#19781 = FACE_OUTER_BOUND ( 'NONE', #79494, .T. ) ;
#19782 = EDGE_LOOP ( 'NONE', ( #19869, #23699, #58552, #95624, #1932, #56352 ) ) ;
#19783 = CARTESIAN_POINT ( 'NONE',  ( 91.19629277837930204, -59.99999999999997868, -16.43493217179371513 ) ) ;
#19785 = CARTESIAN_POINT ( 'NONE',  ( 22.19785761497768917, -29.03579384637624372, 29.50662452699125993 ) ) ;
#19784 = CARTESIAN_POINT ( 'NONE',  ( -39.04695011312426800, -60.00000000000001421, 54.77420429098338417 ) ) ;
#19786 = CARTESIAN_POINT ( 'NONE',  ( 6.819038153627915297E-15, 51.11204936430951307, -27.84083606136722366 ) ) ;
#19787 = CARTESIAN_POINT ( 'NONE',  ( -36.97264161332481791, -39.51093519734542525, 36.52640270433840186 ) ) ;
#19788 = ORIENTED_EDGE ( 'NONE', *, *, #88459, .F. ) ;
#19789 = DIRECTION ( 'NONE',  ( 0.000000000000000000, 0.000000000000000000, 1.000000000000000000 ) ) ;
#19790 = CARTESIAN_POINT ( 'NONE',  ( -33.00000000000000000, 500.0000000000002274, 0.000000000000000000 ) ) ;
#19791 = CARTESIAN_POINT ( 'NONE',  ( -43.03357534758770697, 463.2291678140051658, 4.675918524147543387 ) ) ;
#19792 = FILL_AREA_STYLE_COLOUR ( '', #4445 ) ;
#19793 = CARTESIAN_POINT ( 'NONE',  ( 7.619701877737479201, -61.82557840467232069, -2.447562251315979154 ) ) ;
#19794 = CARTESIAN_POINT ( 'NONE',  ( 11.16512584324286728, -1.276815909463798526, 20.44381853242944302 ) ) ;
#19795 = ORIENTED_EDGE ( 'NONE', *, *, #5532, .T. ) ;
#19796 = CARTESIAN_POINT ( 'NONE',  ( 17.50000000000002132, 45.90000000000000568, 64.09953197957062798 ) ) ;
#19797 = ORIENTED_EDGE ( 'NONE', *, *, #90712, .F. ) ;
#19798 = CARTESIAN_POINT ( 'NONE',  ( 94.09021974688658929, -30.00000000000000000, 191.2958226932782395 ) ) ;
#19799 = CARTESIAN_POINT ( 'NONE',  ( 49.99533400023343432, 38.95362648028734043, -39.50304336076459322 ) ) ;
#19800 = PRESENTATION_LAYER_ASSIGNMENT (  '', '', ( #24920 ) ) ;
#19801 = CARTESIAN_POINT ( 'NONE',  ( 38.86650669486618881, 1.474610560812782335E-15, 0.000000000000000000 ) ) ;
#19802 = CARTESIAN_POINT ( 'NONE',  ( 79.66186223668852051, -30.00000000000000000, -14.34090231030551443 ) ) ;
#19803 = CARTESIAN_POINT ( 'NONE',  ( -23.71062927693709099, 304.9117331807381106, 10.16837944912345648 ) ) ;
#19804 = ORIENTED_EDGE ( 'NONE', *, *, #88910, .F. ) ;
#19805 = ADVANCED_FACE ( 'NONE', ( #47699 ), #48228, .T. ) ;
#19806 = VECTOR ( 'NONE', #63577, 1000.000000000000000 ) ;
#19807 = EDGE_LOOP ( 'NONE', ( #91930, #4123, #14845, #49665 ) ) ;
#19808 = ORIENTED_EDGE ( 'NONE', *, *, #89592, .T. ) ;
#19809 = CARTESIAN_POINT ( 'NONE',  ( 4.250000000000000000, 0.000000000000000000, -10.00000000000000000 ) ) ;
#19810 = FACE_BOUND ( 'NONE', #89145, .T. ) ;
#19811 = LINE ( 'NONE', #101739, #53463 ) ;
#19812 = CARTESIAN_POINT ( 'NONE',  ( 6.000208918519489565, -14.00031337789968333, -0.2646532170642350024 ) ) ;
#19813 = DIRECTION ( 'NONE',  ( -0.000000000000000000, -1.000000000000000000, -0.000000000000000000 ) ) ;
#19814 = EDGE_CURVE ( 'NONE', #7327, #66563, #85406, .T. ) ;
#19815 = CARTESIAN_POINT ( 'NONE',  ( 5.689121120886425409, 54.09406011002712944, 6.093839483979978766 ) ) ;
#19816 = ADVANCED_FACE ( 'NONE', ( #70932 ), #22763, .T. ) ;
#19817 = VERTEX_POINT ( 'NONE', #103825 ) ;
#19819 = EDGE_CURVE ( 'NONE', #21338, #1507, #62334, .T. ) ;
#19818 = CARTESIAN_POINT ( 'NONE',  ( 9.596002107493083244, 50.00000000000000000, -92.37456064097861486 ) ) ;
#19820 = ORIENTED_EDGE ( 'NONE', *, *, #104594, .F. ) ;
#19821 = CARTESIAN_POINT ( 'NONE',  ( -5.909155701201248334, -61.13738319811270827, 1.073778020691675161 ) ) ;
#19822 = CARTESIAN_POINT ( 'NONE',  ( 77.52501956836729846, -38.51633467271251732, 186.5635750154488903 ) ) ;
#19823 = DIRECTION ( 'NONE',  ( -1.000000000000000000, 0.000000000000000000, 0.000000000000000000 ) ) ;
#19824 = CARTESIAN_POINT ( 'NONE',  ( 22.31492703060326477, 303.2773340566886304, 10.02844635004729135 ) ) ;
#19825 = ADVANCED_FACE ( 'NONE', ( #87661 ), #7172, .F. ) ;
#19826 = CARTESIAN_POINT ( 'NONE',  ( -4.815811321232733810, 248.1992329230262158, 3.581116321197045593 ) ) ;
#19827 = B_SPLINE_CURVE_WITH_KNOTS ( 'NONE', 3,
 ( #3417, #52479, #76757, #102097, #77836, #10426, #59538, #92947, #94017, #92406, #18555, #93499, #9893, #34751, #3947, #11480 ),
 .UNSPECIFIED., .F., .F.,
 ( 4, 2, 2, 2, 2, 2, 2, 4 ),
 ( 0.006919675597518590293, 0.007926800617648671263, 0.008933925637778750498, 0.009437488147843788380, 0.009941050657908824528, 0.01019283191294134347, 0.01044461316797386241, 0.01094817567803889682 ),
 .UNSPECIFIED. ) ;
#19828 = ORIENTED_EDGE ( 'NONE', *, *, #68519, .T. ) ;
#19829 = ADVANCED_FACE ( 'NONE', ( #80073 ), #59003, .T. ) ;
#19830 = CARTESIAN_POINT ( 'NONE',  ( 29.59437054465009354, 13.24940423479646157, -39.60535821593528283 ) ) ;
#19831 = CARTESIAN_POINT ( 'NONE',  ( -30.00000000000000000, 500.0000000000002274, 0.000000000000000000 ) ) ;
#19832 = CARTESIAN_POINT ( 'NONE',  ( 22.76441849112663007, 295.0913517417525895, 1.987917119805708843 ) ) ;
#19833 = CARTESIAN_POINT ( 'NONE',  ( -4.852941176470586093, 40.00000000000132871, -70.80672828634229177 ) ) ;
#19834 = ORIENTED_EDGE ( 'NONE', *, *, #23013, .F. ) ;
#19835 = SURFACE_STYLE_USAGE ( .BOTH. , #85602 ) ;
#19836 = DIRECTION ( 'NONE',  ( -1.000000000000000000, -0.000000000000000000, -0.000000000000000000 ) ) ;
#19837 = DIRECTION ( 'NONE',  ( 1.000000000000000000, 0.000000000000000000, -0.000000000000000000 ) ) ;
#19838 = DIRECTION ( 'NONE',  ( -1.000000000000000000, -0.000000000000000000, -0.000000000000000000 ) ) ;
#19839 = CARTESIAN_POINT ( 'NONE',  ( -7.619753052866897747, 101.8254849719282760, -2.447276542590448578 ) ) ;
#19840 = AXIS2_PLACEMENT_3D ( 'NONE', #91747, #67475, #1095 ) ;
#19841 = FACE_OUTER_BOUND ( 'NONE', #27244, .T. ) ;
#19842 = AXIS2_PLACEMENT_3D ( 'NONE', #50981, #59641, #36982 ) ;
#19843 = CARTESIAN_POINT ( 'NONE',  ( 86.49248487488796400, -20.77465731842720231, 183.3202939029210370 ) ) ;
#19844 = CIRCLE ( 'NONE', #2537, 4.000000000000000888 ) ;
#19845 = CARTESIAN_POINT ( 'NONE',  ( 17.15361759915018425, 37.01177862285504716, -21.87054431129734411 ) ) ;
#19846 = CARTESIAN_POINT ( 'NONE',  ( -7.856156674180255983, 67.82625813595271325, 5.000000000000000000 ) ) ;
#19847 = ORIENTED_EDGE ( 'NONE', *, *, #72729, .F. ) ;
#19848 = CARTESIAN_POINT ( 'NONE',  ( 39.18061350182468772, -57.67079139730139303, -41.79049676620926590 ) ) ;
#19849 = CARTESIAN_POINT ( 'NONE',  ( -1.531369966231251212, -15.38254760766061580, -35.23445425113402507 ) ) ;
#19850 = DIRECTION ( 'NONE',  ( -1.000000000000000000, -0.000000000000000000, -0.000000000000000000 ) ) ;
#19851 = CARTESIAN_POINT ( 'NONE',  ( 13.99726531479253566, -50.00011198987433403, 27.38140257663831889 ) ) ;
#19852 = CARTESIAN_POINT ( 'NONE',  ( 5.000000000000000000, -14.08057492516784670, 11.76246841892764827 ) ) ;
#19853 = PRESENTATION_LAYER_ASSIGNMENT (  '', '', ( #85236 ) ) ;
#19854 = CARTESIAN_POINT ( 'NONE',  ( -94.05566740925665670, -30.00000000000000711, 112.3003052795253751 ) ) ;
#19855 = EDGE_CURVE ( 'NONE', #22140, #97138, #3806, .T. ) ;
#19856 = DIRECTION ( 'NONE',  ( 1.000000000000000000, 1.224606353822377258E-16, 0.000000000000000000 ) ) ;
#19857 = CARTESIAN_POINT ( 'NONE',  ( 33.93441569500630095, -57.69361011669973749, 48.11240463317153626 ) ) ;
#19858 = MANIFOLD_SOLID_BREP ( 'Cut-Extrude1', #34330 ) ;
#19860 = CARTESIAN_POINT ( 'NONE',  ( 19.70764564238367100, 304.7954121406193053, 9.925013215726757210 ) ) ;
#19859 = CARTESIAN_POINT ( 'NONE',  ( -9.698972129396532083, 246.8237028725805828, -2.445345647270314782 ) ) ;
#19861 = ADVANCED_FACE ( 'NONE', ( #17489 ), #279, .T. ) ;
#19862 = CARTESIAN_POINT ( 'NONE',  ( -45.37589591933651434, 39.17805190087540979, -45.78237796162623141 ) ) ;
#19863 = CARTESIAN_POINT ( 'NONE',  ( -46.26773511477994560, -37.24076651715746777, 44.57266266732312943 ) ) ;
#19864 = CARTESIAN_POINT ( 'NONE',  ( 0.000000000000000000, 4.898587196589412829E-16, -4.000000000000000000 ) ) ;
#19865 = CARTESIAN_POINT ( 'NONE',  ( -10.00000000000000000, 15.00000000000000000, 4.582575694955833612 ) ) ;
#19866 = LINE ( 'NONE', #28474, #68377 ) ;
#19867 = CARTESIAN_POINT ( 'NONE',  ( 64.03281346377859506, -29.67188817540662171, -23.46043575699671635 ) ) ;
#19868 = CARTESIAN_POINT ( 'NONE',  ( -23.12949768660158156, -22.07965379576427978, 28.45208980778609131 ) ) ;
#19869 = ORIENTED_EDGE ( 'NONE', *, *, #78532, .F. ) ;
#19870 =( LENGTH_UNIT ( ) NAMED_UNIT ( * ) SI_UNIT ( .MILLI., .METRE. ) );
#19871 = DIRECTION ( 'NONE',  ( 0.000000000000000000, 0.000000000000000000, 1.000000000000000000 ) ) ;
#19872 = CARTESIAN_POINT ( 'NONE',  ( -19.40877383843934822, -56.88258129937103291, 33.84440115307146613 ) ) ;
#19873 = AXIS2_PLACEMENT_3D ( 'NONE', #101376, #21038, #70603 ) ;
#19874 = EDGE_CURVE ( 'NONE', #91446, #53134, #707, .T. ) ;
#19876 = CARTESIAN_POINT ( 'NONE',  ( 0.8406291878555783859, 36.41282694755211224, -29.42872758306872427 ) ) ;
#19875 = CARTESIAN_POINT ( 'NONE',  ( -1.250030556990739061, 27.68693347593793774, 39.65778548936075509 ) ) ;
#19877 = PRODUCT_DEFINITION_FORMATION_WITH_SPECIFIED_SOURCE ( 'ANY', '', #84520, .NOT_KNOWN. ) ;
#19878 = ORIENTED_EDGE ( 'NONE', *, *, #96851, .F. ) ;
#19879 = DIRECTION ( 'NONE',  ( -0.000000000000000000, 1.000000000000000000, -0.000000000000000000 ) ) ;
#19880 = ORIENTED_EDGE ( 'NONE', *, *, #28617, .T. ) ;
#19881 = DIRECTION ( 'NONE',  ( 0.000000000000000000, -3.755786496842903988E-16, -1.000000000000000000 ) ) ;
#19882 = CARTESIAN_POINT ( 'NONE',  ( -2.629942617601558563, -60.00000000000000000, -42.63907760742034014 ) ) ;
#19883 = EDGE_LOOP ( 'NONE', ( #54757, #74515, #6207, #53340 ) ) ;
#19884 = DIRECTION ( 'NONE',  ( 0.000000000000000000, 0.000000000000000000, -1.000000000000000000 ) ) ;
#19885 = CARTESIAN_POINT ( 'NONE',  ( 11.69538631874992696, 50.00000000000001421, -88.12269504201513826 ) ) ;
#19886 = CARTESIAN_POINT ( 'NONE',  ( 102.2172463571572081, -52.72165632411573455, 191.7000982784959717 ) ) ;
#19888 = DIRECTION ( 'NONE',  ( -1.000000000000000000, 0.000000000000000000, 0.000000000000000000 ) ) ;
#19887 = DIRECTION ( 'NONE',  ( 1.000000000000000000, 1.224606353822377258E-16, 0.000000000000000000 ) ) ;
#19889 = EDGE_CURVE ( 'NONE', #14645, #68407, #73563, .T. ) ;
#19890 = ORIENTED_EDGE ( 'NONE', *, *, #52061, .T. ) ;
#19891 = CIRCLE ( 'NONE', #30420, 4.000000000000000888 ) ;
#19892 = ORIENTED_EDGE ( 'NONE', *, *, #41496, .T. ) ;
#19893 = EDGE_LOOP ( 'NONE', ( #65662, #18162 ) ) ;
#19894 = CARTESIAN_POINT ( 'NONE',  ( 22.39167605158363372, 305.3927309438643078, 9.053801646461055341 ) ) ;
#19895 = CARTESIAN_POINT ( 'NONE',  ( -19.99999999999999289, 5.000000000000000888, 25.00000000000000000 ) ) ;
#19896 = SURFACE_STYLE_FILL_AREA ( #87251 ) ;
#19897 = ORIENTED_EDGE ( 'NONE', *, *, #35011, .F. ) ;
#19898 = DIRECTION ( 'NONE',  ( 0.000000000000000000, 0.000000000000000000, 1.000000000000000000 ) ) ;
#19899 = CARTESIAN_POINT ( 'NONE',  ( -5.687763048235635388, 41.86978728324998400, -70.29636412762722841 ) ) ;
#19900 = CARTESIAN_POINT ( 'NONE',  ( -76.26250048646183188, -60.00000000000972733, -32.52427117533751755 ) ) ;
#19901 = CARTESIAN_POINT ( 'NONE',  ( 7.897196874019792645, -68.79127204167807008, -1.302055520192085813 ) ) ;
#19902 = CARTESIAN_POINT ( 'NONE',  ( -14.78920111284466010, -5.000000000000000000, 7.149758979994854435 ) ) ;
#19903 = CARTESIAN_POINT ( 'NONE',  ( -6.348225762706512398, 41.72645165896221897, -58.84140311374890331 ) ) ;
#19904 = VECTOR ( 'NONE', #1423, 1000.000000000000000 ) ;
#19906 = CARTESIAN_POINT ( 'NONE',  ( 4.046579032613510485, -39.47243836725472477, 30.46108599521819826 ) ) ;
#19905 = CARTESIAN_POINT ( 'NONE',  ( -103.8766418169371093, -14.21045842199435860, 137.3606855625607182 ) ) ;
#19907 = DIRECTION ( 'NONE',  ( 0.000000000000000000, 0.000000000000000000, -1.000000000000000000 ) ) ;
#19908 = CARTESIAN_POINT ( 'NONE',  ( -48.55441502850074897, -49.90519047855075740, 51.74626393089475584 ) ) ;
#19909 = ORIENTED_EDGE ( 'NONE', *, *, #103082, .T. ) ;
#19910 = CARTESIAN_POINT ( 'NONE',  ( -1.798493680560833141, 21.43522084520895277, 6.769567297170397957 ) ) ;
#19911 = AXIS2_PLACEMENT_3D ( 'NONE', #89482, #39350, #32324 ) ;
#19912 = ORIENTED_EDGE ( 'NONE', *, *, #106389, .F. ) ;
#19913 = AXIS2_PLACEMENT_3D ( 'NONE', #34235, #99448, #25623 ) ;
#19914 = CARTESIAN_POINT ( 'NONE',  ( -3.313708498984765161, -12.96874999999999289, 7.999999999999998224 ) ) ;
#19915 = CONICAL_SURFACE ( 'NONE', #102477, 3.309500000000001663, 0.9599310885968770357 ) ;
#19916 = TOROIDAL_SURFACE ( 'NONE', #9444, 13.99700487351915612, 1.000000000000000000 ) ;
#19917 = CARTESIAN_POINT ( 'NONE',  ( -6.930002047141902821, 302.1778385080101543, -10.02505617572823304 ) ) ;
#19918 = CARTESIAN_POINT ( 'NONE',  ( 0.000000000000000000, 0.000000000000000000, 0.000000000000000000 ) ) ;
#19919 = ORIENTED_EDGE ( 'NONE', *, *, #47799, .T. ) ;
#19920 = CARTESIAN_POINT ( 'NONE',  ( 5.191472769733068482, 247.3590842328105168, -3.014900733016769863 ) ) ;
#19921 = AXIS2_PLACEMENT_3D ( 'NONE', #65665, #40848, #73741 ) ;
#19922 = VERTEX_POINT ( 'NONE', #82734 ) ;
#19923 = CARTESIAN_POINT ( 'NONE',  ( 89.30802776495242767, -29.99999999999331379, 17.92124857685668360 ) ) ;
#19924 = CARTESIAN_POINT ( 'NONE',  ( 56.48317336153285595, -1.232595164407830946E-29, 4.000000000000007105 ) ) ;
#19925 = CARTESIAN_POINT ( 'NONE',  ( -52.56483885390523625, 48.00000000000000000, -38.23529411764706509 ) ) ;
#19926 = CARTESIAN_POINT ( 'NONE',  ( 6.648506486173414665, 41.85229613648736091, -59.35075371410250256 ) ) ;
#19927 = AXIS2_PLACEMENT_3D ( 'NONE', #28717, #5465, #61599 ) ;
#19928 = CARTESIAN_POINT ( 'NONE',  ( -57.69562748396144514, 41.99999999999999289, -15.50526908263377734 ) ) ;
#19929 = CARTESIAN_POINT ( 'NONE',  ( 86.39127330366721935, -29.99999999999999645, 181.0099429049296589 ) ) ;
#19930 = ORIENTED_EDGE ( 'NONE', *, *, #24353, .T. ) ;
#19931 = EDGE_CURVE ( 'NONE', #72021, #93003, #40425, .T. ) ;
#19932 = EDGE_CURVE ( 'NONE', #66410, #21651, #66551, .T. ) ;
#19933 = ORIENTED_EDGE ( 'NONE', *, *, #62351, .F. ) ;
#19934 = ORIENTED_EDGE ( 'NONE', *, *, #29209, .T. ) ;
#19935 = CARTESIAN_POINT ( 'NONE',  ( 53.46816772670749884, -49.90459927595630063, 61.13385163798207600 ) ) ;
#19936 = CARTESIAN_POINT ( 'NONE',  ( 6.661867388682258806, 41.56276662288188817, -58.70509931710797247 ) ) ;
#19937 = DIRECTION ( 'NONE',  ( -1.000000000000000000, -1.224606353822377258E-16, -0.000000000000000000 ) ) ;
#19938 = EDGE_CURVE ( 'NONE', #6815, #39498, #87878, .T. ) ;
#19939 = ORIENTED_EDGE ( 'NONE', *, *, #74472, .F. ) ;
#19941 = EDGE_CURVE ( 'NONE', #97355, #14483, #26147, .T. ) ;
#19940 = CARTESIAN_POINT ( 'NONE',  ( -90.95001345222152622, -38.40481687849002412, -12.83308699341175618 ) ) ;
#19942 = EDGE_LOOP ( 'NONE', ( #7513, #84045, #55652, #83560, #56139, #98132 ) ) ;
#19943 = DIRECTION ( 'NONE',  ( 0.5735764363510468256, 0.8191520442889913545, 0.000000000000000000 ) ) ;
#19944 = CARTESIAN_POINT ( 'NONE',  ( 110.2491967804197657, -38.35601177350259405, 184.3369562795453476 ) ) ;
#19945 = CARTESIAN_POINT ( 'NONE',  ( 12.87241103463997050, 21.40694261541543497, 5.440169305117485976 ) ) ;
#19946 = CARTESIAN_POINT ( 'NONE',  ( 86.14744280574011270, -60.13430353365158254, 9.937224624942581741 ) ) ;
#19947 = CARTESIAN_POINT ( 'NONE',  ( 41.62074773851009724, 334.2059636480821609, 11.44767655643080140 ) ) ;
#19948 = CARTESIAN_POINT ( 'NONE',  ( 4.805888432416990597, -14.59013712844782340, -7.778733730875278418 ) ) ;
#19949 = FACE_OUTER_BOUND ( 'NONE', #75333, .T. ) ;
#19950 = ADVANCED_FACE ( 'NONE', ( #49287 ), #103753, .T. ) ;
#19951 = CARTESIAN_POINT ( 'NONE',  ( 4.681380154937406779, 0.7378729568059335664, 103.7259032015043232 ) ) ;
#19952 = CARTESIAN_POINT ( 'NONE',  ( 8.986804597164578468, 136.5680015418715811, 8.673617379999392574E-16 ) ) ;
#19953 = ORIENTED_EDGE ( 'NONE', *, *, #29868, .T. ) ;
#19954 = FILL_AREA_STYLE ('',( #29115 ) ) ;
#19955 = DIRECTION ( 'NONE',  ( -1.000000000000000000, -0.000000000000000000, -0.000000000000000000 ) ) ;
#19956 = CARTESIAN_POINT ( 'NONE',  ( -33.07276483573514980, 438.9325140356083352, 23.89537236861354685 ) ) ;
#19957 = ORIENTED_EDGE ( 'NONE', *, *, #101233, .F. ) ;
#19958 = CARTESIAN_POINT ( 'NONE',  ( -26.15748752718828385, 306.9073039913806156, -8.546226797207475911 ) ) ;
#19959 = CARTESIAN_POINT ( 'NONE',  ( -40.84349315627966348, 325.1007658372994911, 9.312971402044151858 ) ) ;
#19960 = CARTESIAN_POINT ( 'NONE',  ( 19.61638200451619696, 1.340359594676612611E-15, 0.000000000000000000 ) ) ;
#19961 = CARTESIAN_POINT ( 'NONE',  ( -5.656854249492381470, -22.06249999999999289, 5.656854249492379694 ) ) ;
#19962 = CARTESIAN_POINT ( 'NONE',  ( 14.83349330513380337, 1.593028355512270567E-15, 0.000000000000000000 ) ) ;
#19963 = ORIENTED_EDGE ( 'NONE', *, *, #47214, .T. ) ;
#19964 = CARTESIAN_POINT ( 'NONE',  ( 84.89452607104252024, -35.82308226578413013, 180.4058047747997762 ) ) ;
#19965 = CARTESIAN_POINT ( 'NONE',  ( 97.15356149169568312, 1.016364837396684119E-14, 0.000000000000000000 ) ) ;
#19966 = B_SPLINE_CURVE_WITH_KNOTS ( 'NONE', 3,
 ( #56711, #15733, #65354, #98245, #93360, #44276, #92812, #61540, #85259, #68561, #59947, #18422, #52892, #100370, #3816, #28653 ),
 .UNSPECIFIED., .F., .F.,
 ( 4, 2, 2, 2, 2, 2, 2, 4 ),
 ( 0.006917039672641533445, 0.007923839859808178010, 0.008930640046974823443, 0.009434040140558146159, 0.009937440234141472345, 0.01018914028093313197, 0.01044084032772479333, 0.01094424042130811431 ),
 .UNSPECIFIED. ) ;
#19967 = CONICAL_SURFACE ( 'NONE', #76721, 4.000000000000007105, 0.9599310885968835860 ) ;
#19968 = CARTESIAN_POINT ( 'NONE',  ( 0.000000000000000000, -6.928203230275509661, -3.999999999999999112 ) ) ;
#19969 = ORIENTED_EDGE ( 'NONE', *, *, #100235, .T. ) ;
#19970 = CARTESIAN_POINT ( 'NONE',  ( -89.14489647802798800, -52.70987939842911629, 57.40709364672285631 ) ) ;
#19971 = CARTESIAN_POINT ( 'NONE',  ( 0.06809871960542722424, 7.710219529346608702, -2.645508037661881584 ) ) ;
#19972 = CARTESIAN_POINT ( 'NONE',  ( 12.12626197893011515, -5.000000000000005329, -94.24800833403364209 ) ) ;
#19973 = CARTESIAN_POINT ( 'NONE',  ( 18.09733584172112231, 304.6346571588649681, 8.890781977549927717 ) ) ;
#19974 = CARTESIAN_POINT ( 'NONE',  ( -6.469245887355936198, -21.86882241383921155, -38.54580312982461265 ) ) ;
#19975 = COLOUR_RGB ( '', 0.66274510, 0.83137255, 0.94901961) ;
#19976 = CARTESIAN_POINT ( 'NONE',  ( 39.13724550554672987, -60.00000000000000000, 50.92405014926310969 ) ) ;
#19977 = AXIS2_PLACEMENT_3D ( 'NONE', #50367, #18576, #19131 ) ;
#19978 = CARTESIAN_POINT ( 'NONE',  ( 42.00932080603077168, -38.13850585723300668, 52.74428052397462352 ) ) ;
#19979 = CARTESIAN_POINT ( 'NONE',  ( 2.068673967786806678, -0.1361670080194822274, 102.1191603897975284 ) ) ;
#19980 = CARTESIAN_POINT ( 'NONE',  ( 45.12088577198531425, -28.33719382385789842, 40.20412836573458293 ) ) ;
#19982 = CARTESIAN_POINT ( 'NONE',  ( -10.93523035535289978, 16.60435489604227044, 9.334902641144335433 ) ) ;
#19981 = CARTESIAN_POINT ( 'NONE',  ( -36.74903329801482244, -36.38333104526201822, 45.94992449520283628 ) ) ;
#19983 = ADVANCED_FACE ( 'NONE', ( #38979 ), #24474, .T. ) ;
#19984 = CARTESIAN_POINT ( 'NONE',  ( 4.544092624809295877, 294.7929985550215974, -8.922686206446940105 ) ) ;
#19985 = STYLED_ITEM ( 'NONE', ( #49835 ), #88434 ) ;
#19986 = CARTESIAN_POINT ( 'NONE',  ( 22.91651842568168362, 295.0901107613288445, -9.949346074078583513 ) ) ;
#19987 = CONICAL_SURFACE ( 'NONE', #83594, 5.000000000000010658, 0.9599310885968697082 ) ;
#19988 = FACE_OUTER_BOUND ( 'NONE', #71564, .T. ) ;
#19989 = CIRCLE ( 'NONE', #47489, 3.309500000000001663 ) ;
#19990 = VERTEX_POINT ( 'NONE', #103180 ) ;
#19991 = LINE ( 'NONE', #19459, #67437 ) ;
#19992 = PRODUCT_DEFINITION_SHAPE ( 'NONE', 'NONE',  #106788 ) ;
#19993 = PLANE ( 'NONE',  #80258 ) ;
#19994 = CIRCLE ( 'NONE', #71594, 3.000000000000024425 ) ;
#19995 = ORIENTED_EDGE ( 'NONE', *, *, #59964, .F. ) ;
#19996 = CARTESIAN_POINT ( 'NONE',  ( -12.08879135166870888, -2.338888145639765881, 20.67789593137304749 ) ) ;
#19997 = DIRECTION ( 'NONE',  ( 0.000000000000000000, 1.000000000000000000, 0.000000000000000000 ) ) ;
#19998 = CIRCLE ( 'NONE', #33753, 5.000000000000003553 ) ;
#19999 = CARTESIAN_POINT ( 'NONE',  ( -43.00000000000000000, 461.4080316921935605, 3.462976341553817949 ) ) ;
#20000 =( BOUNDED_CURVE ( )  B_SPLINE_CURVE ( 2, ( #6571, #55636, #88572, #54581, #62205, #21223, #70796, #39503, #38968 ),
 .UNSPECIFIED., .F., .T. ) 
 B_SPLINE_CURVE_WITH_KNOTS ( ( 3, 2, 2, 2, 3 ),
 ( 0.2500000000000000555, 0.2573529411764705621, 0.2647058823529411797, 0.2720588235294116863, 0.2794117647058823040 ),
 .UNSPECIFIED. ) 
 CURVE ( )  GEOMETRIC_REPRESENTATION_ITEM ( )  RATIONAL_B_SPLINE_CURVE ( ( 0.9999999999999994449, 0.9238795325112872936, 1.000000000000000000, 0.9238795325112867385, 1.000000000000000000, 0.9238795325112867385, 1.000000000000000000, 0.9238795325112872936, 0.9999999999999994449 ) ) 
 REPRESENTATION_ITEM ( '' )  );
#20001 = EDGE_CURVE ( 'NONE', #75344, #43310, #77879, .T. ) ;
#20002 = ADVANCED_FACE ( 'NONE', ( #95098 ), #84717, .T. ) ;
#20003 = CARTESIAN_POINT ( 'NONE',  ( -8.066124028907301735, -60.22817720597890911, -36.77925220922959682 ) ) ;
#20004 = ORIENTED_EDGE ( 'NONE', *, *, #23013, .T. ) ;
#20005 = CARTESIAN_POINT ( 'NONE',  ( 4.000000000000001776, 0.000000000000000000, -8.000000000000000000 ) ) ;
#20006 = CARTESIAN_POINT ( 'NONE',  ( -3.999997374469381750, -9.125726201419798400, 6.928204746136267467 ) ) ;
#20007 = ORIENTED_EDGE ( 'NONE', *, *, #67614, .T. ) ;
#20008 = DIRECTION ( 'NONE',  ( 0.000000000000000000, 0.000000000000000000, -1.000000000000000000 ) ) ;
#20009 = CYLINDRICAL_SURFACE ( 'NONE', #57948, 1.250000000000001110 ) ;
#20010 = CARTESIAN_POINT ( 'NONE',  ( -91.86514296420848780, -60.00000000000002132, 10.95446608244987097 ) ) ;
#20011 = VERTEX_POINT ( 'NONE', #33027 ) ;
#20012 = CARTESIAN_POINT ( 'NONE',  ( 30.00000000000000000, 488.6481008951278113, 3.890293910850189274 ) ) ;
#20013 = DIRECTION ( 'NONE',  ( 0.000000000000000000, 0.000000000000000000, -1.000000000000000000 ) ) ;
#20014 = LINE ( 'NONE', #52858, #27144 ) ;
#20016 = CARTESIAN_POINT ( 'NONE',  ( 27.10511071441197117, -1.200000000000000030E-05, 8.806984339685705265 ) ) ;
#20015 = CARTESIAN_POINT ( 'NONE',  ( 8.000000000000000000, 9.797174393178825657E-16, -1.875285714285714445 ) ) ;
#20017 = EDGE_CURVE ( 'NONE', #97524, #57259, #83140, .T. ) ;
#20018 = CARTESIAN_POINT ( 'NONE',  ( -82.06274044418753988, -46.46213096741415427, 172.2108392399005652 ) ) ;
#20019 = VERTEX_POINT ( 'NONE', #56723 ) ;
#20020 = B_SPLINE_CURVE_WITH_KNOTS ( 'NONE', 3,
 ( #50416, #17019, #49894, #83326, #1866, #8903, #41804, #34824 ),
 .UNSPECIFIED., .F., .F.,
 ( 4, 2, 2, 4 ),
 ( 0.000000000000000000, 0.5000000000000000000, 0.7500000000000000000, 1.000000000000000000 ),
 .UNSPECIFIED. ) ;
#20021 = CARTESIAN_POINT ( 'NONE',  ( -14.76977913854937796, -0.000000000000000000, -8.521464936439098636 ) ) ;
#20022 = VERTEX_POINT ( 'NONE', #81001 ) ;
#20023 = ORIENTED_EDGE ( 'NONE', *, *, #43928, .T. ) ;
#20024 = CARTESIAN_POINT ( 'NONE',  ( -7.157960986248002477, -5.000000000000000000, -14.69147069243657100 ) ) ;
#20025 = EDGE_CURVE ( 'NONE', #28073, #54015, #27951, .T. ) ;
#20026 = DIRECTION ( 'NONE',  ( -1.000000000000000000, -1.224606353822377258E-16, -0.000000000000000000 ) ) ;
#20027 = FACE_OUTER_BOUND ( 'NONE', #25986, .T. ) ;
#20028 = EDGE_LOOP ( 'NONE', ( #25129, #52113, #36960, #9075 ) ) ;
#20029 = DIRECTION ( 'NONE',  ( -1.000000000000000000, -1.224606353822377258E-16, -0.000000000000000000 ) ) ;
#20030 = CARTESIAN_POINT ( 'NONE',  ( -93.81425292840387442, -57.67376786465794680, 13.59058164905135513 ) ) ;
#20031 = CARTESIAN_POINT ( 'NONE',  ( 7.045755811259135193, -11.30341603013554064, 3.790843699961852664 ) ) ;
#20032 = CARTESIAN_POINT ( 'NONE',  ( -8.000000000000000000, 0.000000000000000000, -12.97459999999999525 ) ) ;
#20033 = CARTESIAN_POINT ( 'NONE',  ( -9.334514330295428763, 103.2137726231821233, -3.588704711590612995 ) ) ;
#20034 = DIRECTION ( 'NONE',  ( -0.000000000000000000, 1.000000000000000000, -0.000000000000000000 ) ) ;
#20035 = CARTESIAN_POINT ( 'NONE',  ( 3.884543032214245351, 15.13241195026108166, -9.216463528758918500 ) ) ;
#20036 = CARTESIAN_POINT ( 'NONE',  ( 94.85921371064608820, -60.00000000000004263, 26.66736809083038651 ) ) ;
#20037 = CARTESIAN_POINT ( 'NONE',  ( -99.17463707058834643, -30.00000000000003908, 199.4944348318372818 ) ) ;
#20038 = CARTESIAN_POINT ( 'NONE',  ( -56.18806491820092930, -29.08722365262319087, 58.61279431429321818 ) ) ;
#20039 = ORIENTED_EDGE ( 'NONE', *, *, #68616, .T. ) ;
#20040 = DIRECTION ( 'NONE',  ( 0.000000000000000000, -0.9221233147934838614, -0.3868961001538753219 ) ) ;
#20041 = EDGE_LOOP ( 'NONE', ( #7519, #52811 ) ) ;
#20042 = CARTESIAN_POINT ( 'NONE',  ( -102.7148152195156143, -37.82052743781596860, 177.0099866061467822 ) ) ;
#20043 = CARTESIAN_POINT ( 'NONE',  ( -3.672464763049774796E-06, -18.02989419364509516, 35.00496915990722613 ) ) ;
#20044 = EDGE_LOOP ( 'NONE', ( #10413, #26305 ) ) ;
#20045 = CARTESIAN_POINT ( 'NONE',  ( 19.49193093582640302, 49.99898248078959284, 60.07857787404169159 ) ) ;
#20046 = B_SPLINE_CURVE_WITH_KNOTS ( 'NONE', 3,
 ( #98832, #22874, #57841, #32556, #47629, #39576, #90768, #80531, #6648, #56784, #72450, #81062, #7701, #49765, #82669, #11416, #52413, #100973, #66480, #2805, #99357, #42741, #77236, #67562, #93431, #10885, #43799, #85331, #75633, #100444, #27132, #51883, #19584, #101512 ),
 .UNSPECIFIED., .F., .F.,
 ( 4, 2, 2, 2, 2, 2, 2, 2, 2, 2, 2, 2, 2, 2, 2, 2, 4 ),
 ( 0.000000000000000000, 0.03124999999999548625, 0.06249999999999097250, 0.09374999999998642752, 0.1249999999999818895, 0.1562499999999773237, 0.1874999999999727995, 0.2187499999999682476, 0.2499999999999637235, 0.2812499999999591993, 0.3124999999999546474, 0.3437499999999502065, 0.3749999999999456546, 0.4062499999999411582, 0.4374999999999366063, 0.4687499999999321654, 0.4999999999999275579 ),
 .UNSPECIFIED. ) ;
#20047 = CARTESIAN_POINT ( 'NONE',  ( -18.32916183804282895, -60.00000000000000000, 40.02166413529950262 ) ) ;
#20048 = CARTESIAN_POINT ( 'NONE',  ( -3.626288723285919779, -1.044241108143933339, 104.3502830461760880 ) ) ;
#20049 = CARTESIAN_POINT ( 'NONE',  ( -5.082755093536325042, -17.46875000204838813, -5.082755093536325930 ) ) ;
#20050 = CARTESIAN_POINT ( 'NONE',  ( 27.18908553330205180, 296.5274986157688772, 10.30015177545897842 ) ) ;
#20051 = LINE ( 'NONE', #52900, #87508 ) ;
#20052 = CARTESIAN_POINT ( 'NONE',  ( -31.00389226249483698, 502.9289871839745842, 8.047326149841639520 ) ) ;
#20053 = CARTESIAN_POINT ( 'NONE',  ( 35.00384615384614762, 4.172000000000003261, 0.000000000000000000 ) ) ;
#20054 = CARTESIAN_POINT ( 'NONE',  ( -7.865987974594087717, 86.57916236585580805, 1.301042606982605124E-15 ) ) ;
#20055 = CARTESIAN_POINT ( 'NONE',  ( 41.50669491856072568, 1.482358050883964840E-15, 0.000000000000000000 ) ) ;
#20056 = VECTOR ( 'NONE', #26348, 1000.000000000000000 ) ;
#20057 = CARTESIAN_POINT ( 'NONE',  ( -5.369174336198356379, 44.20122194677738037, -60.96850753999265748 ) ) ;
#20058 = UNCERTAINTY_MEASURE_WITH_UNIT (LENGTH_MEASURE( 1.000000000000000082E-05 ), #69265, 'distance_accuracy_value', 'NONE');
#20059 = CARTESIAN_POINT ( 'NONE',  ( -32.05612036281008415, -60.32439009662663665, 37.68584545065578340 ) ) ;
#20060 = CARTESIAN_POINT ( 'NONE',  ( -42.20041562234357002, 435.2369744135583574, 7.788607701745487333 ) ) ;
#20061 = CARTESIAN_POINT ( 'NONE',  ( 48.11622830880407520, -29.14282674110490134, 44.62614721453967093 ) ) ;
#20062 = AXIS2_PLACEMENT_3D ( 'NONE', #98854, #74588, #664 ) ;
#20063 = CARTESIAN_POINT ( 'NONE',  ( 43.30868969682389036, 1.340359594676612611E-15, 0.000000000000000000 ) ) ;
#20064 = DIRECTION ( 'NONE',  ( 0.000000000000000000, -1.000000000000000000, 0.000000000000000000 ) ) ;
#20065 = CARTESIAN_POINT ( 'NONE',  ( -86.06810362144429405, -38.63750899286093698, 199.0947428394257486 ) ) ;
#20066 = AXIS2_PLACEMENT_3D ( 'NONE', #38112, #70969, #93122 ) ;
#20067 = EDGE_LOOP ( 'NONE', ( #38961, #52517, #30654, #8458, #30001 ) ) ;
#20068 = CARTESIAN_POINT ( 'NONE',  ( 22.33349330513380337, 1.593028355512270567E-15, 0.000000000000000000 ) ) ;
#20069 = CARTESIAN_POINT ( 'NONE',  ( 12.54481040020086802, 5.202751164716101329, -8.103389815076774028 ) ) ;
#20070 = CARTESIAN_POINT ( 'NONE',  ( -19.33400676013704000, 49.88855074631516828, 61.23237481859990794 ) ) ;
#20071 = CONICAL_SURFACE ( 'NONE', #51024, 4.174999999999998934, 0.9599310885968824758 ) ;
#20072 = CARTESIAN_POINT ( 'NONE',  ( 6.280866958221838381, 40.29318264226383661, -71.19386870237659082 ) ) ;
#20073 = CARTESIAN_POINT ( 'NONE',  ( -32.82923042684467418, 434.9827582799806009, 12.60815599139151111 ) ) ;
#20074 = VECTOR ( 'NONE', #35122, 1000.000000000000000 ) ;
#20075 = CARTESIAN_POINT ( 'NONE',  ( 42.61140200160144076, 465.9030374194823594, 13.21253569360416691 ) ) ;
#20076 = FACE_OUTER_BOUND ( 'NONE', #95199, .T. ) ;
#20077 = CARTESIAN_POINT ( 'NONE',  ( 111.4401660675299865, -59.99999999999997868, 184.8140296056671730 ) ) ;
#20078 = CIRCLE ( 'NONE', #87242, 5.000000000000001776 ) ;
#20079 = MECHANICAL_DESIGN_GEOMETRIC_PRESENTATION_REPRESENTATION (  '', ( #76838 ), #38976 ) ;
#20080 = ADVANCED_FACE ( 'NONE', ( #25476 ), #63121, .F. ) ;
#20081 = DIRECTION ( 'NONE',  ( 0.000000000000000000, -1.000000000000000000, 0.000000000000000000 ) ) ;
#20082 = ORIENTED_EDGE ( 'NONE', *, *, #50364, .T. ) ;
#20083 = EDGE_CURVE ( 'NONE', #66067, #89428, #74506, .T. ) ;
#20084 = CARTESIAN_POINT ( 'NONE',  ( 2.806188179629718782, -49.57861714546726972, 102.9366787940491861 ) ) ;
#20085 = CARTESIAN_POINT ( 'NONE',  ( -98.73364301279765698, -29.99999999999999645, 142.5754916489613322 ) ) ;
#20086 = ORIENTED_EDGE ( 'NONE', *, *, #12577, .F. ) ;
#20087 = CARTESIAN_POINT ( 'NONE',  ( 5.248477453467016218, 10.42489023671462611, -30.57443130249296459 ) ) ;
#20088 = CARTESIAN_POINT ( 'NONE',  ( 17.33349330513380693, 4.000000000000003553, 0.000000000000000000 ) ) ;
#20089 = CARTESIAN_POINT ( 'NONE',  ( 43.02661387979727436, 465.7449615347604208, 11.43319743843670544 ) ) ;
#20090 = CIRCLE ( 'NONE', #33846, 1.000000000000000888 ) ;
#20091 = CARTESIAN_POINT ( 'NONE',  ( 47.33349330513379982, 1.593028355512270567E-15, 0.000000000000000000 ) ) ;
#20092 = CARTESIAN_POINT ( 'NONE',  ( -7.188101187500001821, -15.87500000204838635, -2.977408999572651371 ) ) ;
#20093 = CARTESIAN_POINT ( 'NONE',  ( 3.140974613990258568, -5.000000000000002665, -73.31232788067565309 ) ) ;
#20094 = PRODUCT_DEFINITION_SHAPE ( 'NONE', 'NONE',  #76584 ) ;
#20095 =( NAMED_UNIT ( * ) PLANE_ANGLE_UNIT ( ) SI_UNIT ( $, .RADIAN. ) );
#20097 = ORIENTED_EDGE ( 'NONE', *, *, #71259, .F. ) ;
#20096 = DIRECTION ( 'NONE',  ( 0.000000000000000000, -1.000000000000000000, 0.000000000000000000 ) ) ;
#20098 = CARTESIAN_POINT ( 'NONE',  ( 81.84886303975771682, -49.95657649133486444, 175.6591428596718174 ) ) ;
#20100 = AXIS2_PLACEMENT_3D ( 'NONE', #93616, #43993, #35404 ) ;
#20099 = CARTESIAN_POINT ( 'NONE',  ( -6.499999999999999112, -3.752776749732595452, -0.7999999999999977129 ) ) ;
#20101 = CARTESIAN_POINT ( 'NONE',  ( 9.381593208289377372, 87.01438638119508084, -3.465401811657801368 ) ) ;
#20102 = VERTEX_POINT ( 'NONE', #56 ) ;
#20103 = DIRECTION ( 'NONE',  ( 0.000000000000000000, -1.000000000000000000, 0.000000000000000000 ) ) ;
#20104 = DIRECTION ( 'NONE',  ( 0.000000000000000000, 0.000000000000000000, 1.000000000000000000 ) ) ;
#20105 = AXIS2_PLACEMENT_3D ( 'NONE', #40670, #73556, #106459 ) ;
#20106 = CARTESIAN_POINT ( 'NONE',  ( -29.33008799483348028, 13.53038725678829124, -39.65490270820011887 ) ) ;
#20107 = DIRECTION ( 'NONE',  ( 0.000000000000000000, 1.000000000000000000, 0.000000000000000000 ) ) ;
#20108 = DIRECTION ( 'NONE',  ( -1.000000000000000000, -0.000000000000000000, -0.000000000000000000 ) ) ;
#20109 = ORIENTED_EDGE ( 'NONE', *, *, #91136, .T. ) ;
#20110 = CARTESIAN_POINT ( 'NONE',  ( -4.302752950498814677, -48.89765970236341985, 104.4121132197325466 ) ) ;
#20111 = DIRECTION ( 'NONE',  ( -1.000000000000000000, -1.224606353822377258E-16, -0.000000000000000000 ) ) ;
#20112 = DIRECTION ( 'NONE',  ( 0.000000000000000000, 0.000000000000000000, 1.000000000000000000 ) ) ;
#20114 = CARTESIAN_POINT ( 'NONE',  ( -12.80252612773492693, 6.537496074479076213, -7.668719352993321969 ) ) ;
#20113 = DIRECTION ( 'NONE',  ( 0.000000000000000000, -1.000000000000000000, 0.000000000000000000 ) ) ;
#20115 = ADVANCED_FACE ( 'NONE', ( #42143 ), #92088, .T. ) ;
#20116 = CARTESIAN_POINT ( 'NONE',  ( 5.082755093536324154, -28.34375000204838813, 5.082755093536326818 ) ) ;
#20117 = CARTESIAN_POINT ( 'NONE',  ( 16.25962063600091412, 302.5670250583751795, -10.06049463409325107 ) ) ;
#20118 = DIRECTION ( 'NONE',  ( -0.000000000000000000, -1.000000000000000000, -0.000000000000000000 ) ) ;
#20119 = DIRECTION ( 'NONE',  ( 1.000000000000000000, -0.000000000000000000, -0.000000000000000000 ) ) ;
#20120 = ORIENTED_EDGE ( 'NONE', *, *, #104818, .F. ) ;
#20121 = LINE ( 'NONE', #76704, #78424 ) ;
#20122 = CARTESIAN_POINT ( 'NONE',  ( 5.799999999999999822, -4.618802153516994302, 8.000000000000000000 ) ) ;
#20123 = CARTESIAN_POINT ( 'NONE',  ( -3.830996925285758525, 18.06395145735098140, -5.000000000000000000 ) ) ;
#20124 = ADVANCED_FACE ( 'NONE', ( #48629 ), #91775, .F. ) ;
#20125 = SURFACE_STYLE_FILL_AREA ( #101529 ) ;
#20126 = AXIS2_PLACEMENT_3D ( 'NONE', #46726, #32151, #80670 ) ;
#20127 = B_SPLINE_CURVE_WITH_KNOTS ( 'NONE', 3,
 ( #69025, #10227, #26463, #52277 ),
 .UNSPECIFIED., .F., .F.,
 ( 4, 4 ),
 ( 0.000000000000000000, 0.0002485318720385933230 ),
 .UNSPECIFIED. ) ;
#20128 = VERTEX_POINT ( 'NONE', #20053 ) ;
#20129 = CARTESIAN_POINT ( 'NONE',  ( 36.01601968523547015, 463.8931034503634692, 20.04842029783048929 ) ) ;
#20130 = CARTESIAN_POINT ( 'NONE',  ( 5.656854249492378806, -21.87500000409676915, 5.656854249492381470 ) ) ;
#20131 = ORIENTED_EDGE ( 'NONE', *, *, #29706, .F. ) ;
#20132 = CARTESIAN_POINT ( 'NONE',  ( -9.169574833318794305, 51.60709747164507633, -1.678735602677582373 ) ) ;
#20133 = CARTESIAN_POINT ( 'NONE',  ( 9.918010731619574472, 101.2084831515677337, -1.300854425901575739 ) ) ;
#20134 = FILL_AREA_STYLE ('',( #43823 ) ) ;
#20135 = UNCERTAINTY_MEASURE_WITH_UNIT (LENGTH_MEASURE( 1.000000000000000082E-05 ), #62164, 'distance_accuracy_value', 'NONE');
#20136 = CARTESIAN_POINT ( 'NONE',  ( -105.9855091700707703, -60.00000000000000000, 198.2901911838892488 ) ) ;
#20137 = AXIS2_PLACEMENT_3D ( 'NONE', #22632, #61480, #104030 ) ;
#20138 = VECTOR ( 'NONE', #84234, 1000.000000000000000 ) ;
#20139 = CONICAL_SURFACE ( 'NONE', #80361, 3.309500000000001663, 0.9599310885968770357 ) ;
#20140 = CARTESIAN_POINT ( 'NONE',  ( 4.358513833876418886, 4.989164364209876190, -0.07763482564820534115 ) ) ;
#20141 = LINE ( 'NONE', #1212, #8077 ) ;
#20142 = EDGE_CURVE ( 'NONE', #93551, #22579, #12031, .T. ) ;
#20143 = CARTESIAN_POINT ( 'NONE',  ( -85.81946245793210437, -25.08273551360057141, 176.6337755868447061 ) ) ;
#20144 = CARTESIAN_POINT ( 'NONE',  ( -4.448391904179714196, 54.30568176866136554, -6.353132081348096705 ) ) ;
#20145 = CIRCLE ( 'NONE', #83843, 5.000000000000001776 ) ;
#20146 = AXIS2_PLACEMENT_3D ( 'NONE', #47137, #95185, #87094 ) ;
#20147 = ORIENTED_EDGE ( 'NONE', *, *, #88714, .T. ) ;
#20148 = CARTESIAN_POINT ( 'NONE',  ( -9.067083174484388053, 46.09712060844259440, -13.87005886985725667 ) ) ;
#20149 = ADVANCED_FACE ( 'NONE', ( #51826 ), #86438, .T. ) ;
#20150 = CARTESIAN_POINT ( 'NONE',  ( 3.384215095276188023, -0.8669809812617773614, 104.0501775326196281 ) ) ;
#20151 = CARTESIAN_POINT ( 'NONE',  ( -82.52728043534214919, -37.83368342240796522, 6.799488428291162734 ) ) ;
#20152 = CARTESIAN_POINT ( 'NONE',  ( -32.00946877229060306, 486.4631725509864850, 6.108882930589409455 ) ) ;
#20153 = CARTESIAN_POINT ( 'NONE',  ( -3.625560833898588964, 129.4090813058823812, -5.000000000000000888 ) ) ;
#20154 = CARTESIAN_POINT ( 'NONE',  ( 3.225593670032574689, 115.6483099733404458, -5.000000000000000000 ) ) ;
#20155 = CARTESIAN_POINT ( 'NONE',  ( 28.10498339410670354, 36.32170307983790991, -9.575481939047044477 ) ) ;
#20156 = DIRECTION ( 'NONE',  ( -1.000000000000000000, -1.224646799147353207E-16, 0.000000000000000000 ) ) ;
#20157 = EDGE_CURVE ( 'NONE', #17481, #72013, #44134, .T. ) ;
#20158 = CARTESIAN_POINT ( 'NONE',  ( 74.38357847894150154, -30.00000000000000711, 152.0601407382578429 ) ) ;
#20159 = CARTESIAN_POINT ( 'NONE',  ( -90.14748428319414586, -30.00000000000004263, -6.309121115244137101 ) ) ;
#20160 = CARTESIAN_POINT ( 'NONE',  ( -65.36515674848668311, -29.05609114770573953, 81.83284678706763771 ) ) ;
#20161 = ORIENTED_EDGE ( 'NONE', *, *, #22034, .F. ) ;
#20162 = CARTESIAN_POINT ( 'NONE',  ( 78.25600647866326653, -14.21045842199443499, 182.3349015425907851 ) ) ;
#20163 = CARTESIAN_POINT ( 'NONE',  ( -59.26346722528342781, 40.83785626851633310, 26.86426695247594409 ) ) ;
#20164 = CARTESIAN_POINT ( 'NONE',  ( 40.95489678083415441, -59.99999999999998579, 57.97946709036114044 ) ) ;
#20165 = ADVANCED_FACE ( 'NONE', ( #85271 ), #77180, .T. ) ;
#20166 = EDGE_LOOP ( 'NONE', ( #92144, #20316, #50562, #64207, #27230, #7143 ) ) ;
#20167 = CARTESIAN_POINT ( 'NONE',  ( 13.87407757772530736, -57.47192967781523976, 25.11348823608586400 ) ) ;
#20168 = CARTESIAN_POINT ( 'NONE',  ( -7.188101187500000044, -26.28125000204838813, -8.802885111219163269E-16 ) ) ;
#20169 = CARTESIAN_POINT ( 'NONE',  ( -0.6461882397993791161, 28.14391481035789155, -38.41680952378990099 ) ) ;
#20170 = EDGE_LOOP ( 'NONE', ( #51516, #96686, #92414 ) ) ;
#20171 = CIRCLE ( 'NONE', #6317, 4.000000000000007105 ) ;
#20172 = DIRECTION ( 'NONE',  ( 0.000000000000000000, 1.000000000000000000, 0.000000000000000000 ) ) ;
#20173 = ORIENTED_EDGE ( 'NONE', *, *, #87420, .T. ) ;
#20174 = CARTESIAN_POINT ( 'NONE',  ( 25.11650669486618881, -3.851859888774471706E-31, 4.000000000000000888 ) ) ;
#20175 = CARTESIAN_POINT ( 'NONE',  ( 32.12958771267400948, 464.7275665249413237, 11.12424126545837133 ) ) ;
#20176 = CARTESIAN_POINT ( 'NONE',  ( -92.81214216858748500, -60.00000000000000000, 30.43431760843921907 ) ) ;
#20177 = CARTESIAN_POINT ( 'NONE',  ( 86.75754961941542831, 1.030564683017419500E-14, 0.000000000000000000 ) ) ;
#20178 = CARTESIAN_POINT ( 'NONE',  ( -2.977408999572654480, -33.50000000204838813, 7.188101187499999156 ) ) ;
#20179 = LINE ( 'NONE', #102099, #34420 ) ;
#20180 = VECTOR ( 'NONE', #7499, 1000.000000000000000 ) ;
#20181 = FILL_AREA_STYLE ('',( #85953 ) ) ;
#20182 = CARTESIAN_POINT ( 'NONE',  ( 28.58349330513380337, -4.000000000000000888, 4.898587196589416773E-16 ) ) ;
#20183 = CARTESIAN_POINT ( 'NONE',  ( 10.48543666094731996, 50.00000000000000000, -91.04342776276723725 ) ) ;
#20184 = CARTESIAN_POINT ( 'NONE',  ( -7.934883677559676940, 108.8683917793755001, 1.051380792122693419 ) ) ;
#20185 = CARTESIAN_POINT ( 'NONE',  ( 38.69545490169056023, 437.5444261471850496, 4.829293893634224233 ) ) ;
#20186 = EDGE_LOOP ( 'NONE', ( #71839, #7962, #42258, #10191 ) ) ;
#20187 = CARTESIAN_POINT ( 'NONE',  ( 4.928386788250423756, -1.571875576847029388, 104.2441249819466833 ) ) ;
#20189 = CARTESIAN_POINT ( 'NONE',  ( 35.43533760671546418, -53.35864796427840417, 38.23550249976548798 ) ) ;
#20188 = CARTESIAN_POINT ( 'NONE',  ( -3.753470829068717762, -48.91069040221621123, 104.5911851069064085 ) ) ;
#20190 = CARTESIAN_POINT ( 'NONE',  ( -22.03900363278799190, -4.285714285715346072, 12.70248734012972669 ) ) ;
#20191 = EDGE_LOOP ( 'NONE', ( #52124, #7045, #68536, #46885 ) ) ;
#20192 = CARTESIAN_POINT ( 'NONE',  ( -22.65226583814422057, 26.07318025823565577, -30.83806826229820075 ) ) ;
#20194 = CARTESIAN_POINT ( 'NONE',  ( 52.81650669486619165, 6.856755485862130937E-15, 0.000000000000000000 ) ) ;
#20193 = PRESENTATION_STYLE_ASSIGNMENT (( #28816 ) ) ;
#20195 = CARTESIAN_POINT ( 'NONE',  ( 8.143901214329899974E-15, 49.00000000000000000, -66.50000000000000000 ) ) ;
#20196 = CARTESIAN_POINT ( 'NONE',  ( -43.39367449997198634, 484.9145775485452532, -0.08602995367264502924 ) ) ;
#20197 = FACE_OUTER_BOUND ( 'NONE', #77913, .T. ) ;
#20198 = DIRECTION ( 'NONE',  ( -1.000000000000000000, -0.000000000000000000, -0.000000000000000000 ) ) ;
#20199 = DIRECTION ( 'NONE',  ( 0.000000000000000000, 0.000000000000000000, 1.000000000000000000 ) ) ;
#20200 = DIRECTION ( 'NONE',  ( -1.000000000000000000, -1.224606353822377258E-16, -0.000000000000000000 ) ) ;
#20201 = ORIENTED_EDGE ( 'NONE', *, *, #15164, .T. ) ;
#20202 = CARTESIAN_POINT ( 'NONE',  ( 92.70591394858523415, -60.00000000000000711, -4.971626050221717996 ) ) ;
#20203 = CIRCLE ( 'NONE', #97572, 8.500000000000000000 ) ;
#20204 = CARTESIAN_POINT ( 'NONE',  ( -10.91073407590445932, 45.93358294599330804, -13.06300009034441523 ) ) ;
#20205 = CARTESIAN_POINT ( 'NONE',  ( 51.01037695545453232, 450.0000000000002274, 13.20242257375370976 ) ) ;
#20206 = CARTESIAN_POINT ( 'NONE',  ( 32.82691535583475684, 485.1045372766794799, 1.724905475515027264 ) ) ;
#20207 = CARTESIAN_POINT ( 'NONE',  ( -6.097206778545145589, 40.29241581810332207, -71.16079338543529786 ) ) ;
#20208 = DIRECTION ( 'NONE',  ( -0.000000000000000000, -1.000000000000000000, -0.000000000000000000 ) ) ;
#20209 = EDGE_LOOP ( 'NONE', ( #56510, #97625, #40502, #87143 ) ) ;
#20210 = ADVANCED_FACE ( 'NONE', ( #11902 ), #86527, .T. ) ;
#20211 = B_SPLINE_CURVE_WITH_KNOTS ( 'NONE', 3,
 ( #50715, #83628, #42648, #2173, #34600, #2716, #92246, #51254 ),
 .UNSPECIFIED., .F., .F.,
 ( 4, 2, 2, 4 ),
 ( 0.003797433802554431997, 0.004743183970586231819, 0.005688934138618031641, 0.007580434474681628683 ),
 .UNSPECIFIED. ) ;
#20212 = CARTESIAN_POINT ( 'NONE',  ( -83.01077121088147237, -30.00000000006739143, 195.4859236386342332 ) ) ;
#20213 = VERTEX_POINT ( 'NONE', #43220 ) ;
#20214 = CARTESIAN_POINT ( 'NONE',  ( -9.226722513859208163, -54.52964393432027634, 23.14374324513729064 ) ) ;
#20215 = CARTESIAN_POINT ( 'NONE',  ( 4.463429423125059081, -13.01149508916979336, -12.86120860535740462 ) ) ;
#20216 = DIRECTION ( 'NONE',  ( -1.000000000000000000, -0.000000000000000000, -0.000000000000000000 ) ) ;
#20217 = CARTESIAN_POINT ( 'NONE',  ( 15.66336674558382569, 21.48481246047165172, -5.205033774743918151 ) ) ;
#20219 = CARTESIAN_POINT ( 'NONE',  ( 86.84721542904824787, -60.22473763668222091, -10.54107096568754365 ) ) ;
#20218 = CIRCLE ( 'NONE', #66658, 4.000000000000007105 ) ;
#20220 = AXIS2_PLACEMENT_3D ( 'NONE', #22391, #65470, #55234 ) ;
#20221 = CARTESIAN_POINT ( 'NONE',  ( -7.188101187500000044, -32.28125000204838813, -8.802885111219163269E-16 ) ) ;
#20223 = EDGE_CURVE ( 'NONE', #41303, #65608, #27076, .T. ) ;
#20222 = CARTESIAN_POINT ( 'NONE',  ( -17.51626200557882029, 45.00000000000000711, 63.59143666326379218 ) ) ;
#20224 = DIRECTION ( 'NONE',  ( 0.000000000000000000, -1.000000000000000000, 0.000000000000000000 ) ) ;
#20225 = ORIENTED_EDGE ( 'NONE', *, *, #71259, .T. ) ;
#20226 = CARTESIAN_POINT ( 'NONE',  ( 32.83963058357245046, 487.9259959563239022, 4.912446691208849359 ) ) ;
#20227 = VERTEX_POINT ( 'NONE', #3827 ) ;
#20228 = CARTESIAN_POINT ( 'NONE',  ( 48.76594521878717359, 8.294242253543416155, -16.61919356891331745 ) ) ;
#20229 = DIRECTION ( 'NONE',  ( 0.000000000000000000, 0.000000000000000000, -1.000000000000000000 ) ) ;
#20230 = MECHANICAL_DESIGN_GEOMETRIC_PRESENTATION_REPRESENTATION (  '', ( #33902 ), #87314 ) ;
#20231 = B_SPLINE_CURVE_WITH_KNOTS ( 'NONE', 3,
 ( #45697, #78059, #44649, #85092, #102335, #76454, #44105, #37110, #19352, #54283, #28483, #4176, #2563, #20942 ),
 .UNSPECIFIED., .F., .F.,
 ( 4, 2, 2, 2, 2, 2, 4 ),
 ( 2.934965519869990483E-17, 0.0003840169304677532383, 0.0007680338609354772032, 0.001152050791403200951, 0.001536067721870924916, 0.002304101582806372412, 0.003072135443741819474 ),
 .UNSPECIFIED. ) ;
#20232 = COLOUR_RGB ( '', 0.40784314, 0.44705882, 0.49803922) ;
#20234 = ORIENTED_EDGE ( 'NONE', *, *, #100379, .F. ) ;
#20233 = DIRECTION ( 'NONE',  ( 0.000000000000000000, -1.000000000000000000, 0.000000000000000000 ) ) ;
#20235 = CARTESIAN_POINT ( 'NONE',  ( 78.49326029233736790, -53.37114656867112217, 151.3752469050666889 ) ) ;
#20236 = PRESENTATION_LAYER_ASSIGNMENT (  '', '', ( #76988 ) ) ;
#20237 = EDGE_LOOP ( 'NONE', ( #77700, #54186, #32076 ) ) ;
#20238 = CARTESIAN_POINT ( 'NONE',  ( 5.029581416257693505, -51.84653879358399564, 40.06623209565592703 ) ) ;
#20239 = CIRCLE ( 'NONE', #83917, 4.000000000000001776 ) ;
#20240 = CARTESIAN_POINT ( 'NONE',  ( 7.188101187500000933, -19.06250000204838102, -2.977408999572650483 ) ) ;
#20241 = CARTESIAN_POINT ( 'NONE',  ( -112.4426759231622270, -57.67115411723771956, 189.8075418672916044 ) ) ;
#20242 = VERTEX_POINT ( 'NONE', #101458 ) ;
#20243 = CARTESIAN_POINT ( 'NONE',  ( 3.757221660946450825, 19.36720549871765940, 4.999999999999998224 ) ) ;
#20244 = CARTESIAN_POINT ( 'NONE',  ( -9.646032546913147598, 81.98719671525634567, 2.644051433538244122 ) ) ;
#20245 = CARTESIAN_POINT ( 'NONE',  ( 24.63846153846153797, 1.411358822780289120E-15, 0.000000000000000000 ) ) ;
#20246 = ADVANCED_FACE ( 'NONE', ( #101974 ), #74723, .F. ) ;
#20247 = CARTESIAN_POINT ( 'NONE',  ( 8.000000000000000000, -20.09375000409677270, -3.313708498984761608 ) ) ;
#20248 = CARTESIAN_POINT ( 'NONE',  ( -49.59036903429539933, -29.60824657159849238, 45.96457809154073004 ) ) ;
#20249 = DIRECTION ( 'NONE',  ( -1.000000000000000000, -0.000000000000000000, -0.000000000000000000 ) ) ;
#20250 = LINE ( 'NONE', #27808, #3458 ) ;
#20251 = MECHANICAL_DESIGN_GEOMETRIC_PRESENTATION_REPRESENTATION (  '', ( #66702 ), #56358 ) ;
#20252 = CARTESIAN_POINT ( 'NONE',  ( -36.97265860262993442, 437.4722588954306843, 4.366279915526011024 ) ) ;
#20253 = PLANE ( 'NONE',  #56806 ) ;
#20254 = PRODUCT_CONTEXT ( 'NONE', #106482, 'mechanical' ) ;
#20255 = CYLINDRICAL_SURFACE ( 'NONE', #76378, 4.000000000000000000 ) ;
#20256 = EDGE_LOOP ( 'NONE', ( #46826, #71166, #21765, #84031, #47579 ) ) ;
#20257 = CARTESIAN_POINT ( 'NONE',  ( -1.197355913555570028, -53.99999999817047325, 40.95503241349764778 ) ) ;
#20258 = CARTESIAN_POINT ( 'NONE',  ( 11.04679971567022712, -4.985848584336745937, -12.57695644737852092 ) ) ;
#20259 = AXIS2_PLACEMENT_3D ( 'NONE', #5306, #80765, #70031 ) ;
#20260 = CARTESIAN_POINT ( 'NONE',  ( 6.337538409676599689E-15, 7.746009256456446224, 51.75000000000000711 ) ) ;
#20261 = CARTESIAN_POINT ( 'NONE',  ( 24.13407075184041872, -22.09882246145749818, -37.53491456946041893 ) ) ;
#20262 = CARTESIAN_POINT ( 'NONE',  ( -62.54040768055548227, -29.99999999999999645, 73.45737685867385380 ) ) ;
#20263 = ADVANCED_FACE ( 'NONE', ( #45357, #72659, #7382, #79689, #5798 ), #106074, .F. ) ;
#20264 = ORIENTED_EDGE ( 'NONE', *, *, #17966, .T. ) ;
#20265 = B_SPLINE_CURVE_WITH_KNOTS ( 'NONE', 3,
 ( #106728, #32878, #65753, #98634 ),
 .UNSPECIFIED., .F., .F.,
 ( 4, 4 ),
 ( 1.734723475976807094E-18, 0.0001964870061279678343 ),
 .UNSPECIFIED. ) ;
#20266 = CARTESIAN_POINT ( 'NONE',  ( 67.22793774957824553, 6.975173280561618775E-15, 0.000000000000000000 ) ) ;
#20267 = CARTESIAN_POINT ( 'NONE',  ( 75.26462255869792273, -57.56720986738325507, 191.3862757953040443 ) ) ;
#20268 = CARTESIAN_POINT ( 'NONE',  ( 6.249999999999998224, 0.000000000000000000, 0.000000000000000000 ) ) ;
#20269 = VECTOR ( 'NONE', #59413, 999.9999999999998863 ) ;
#20270 = CARTESIAN_POINT ( 'NONE',  ( 53.08967281450005515, -36.21579350601970759, -35.63781967302410436 ) ) ;
#20271 = DIRECTION ( 'NONE',  ( -0.5516836157922502260, -0.3133352674422915096, 0.7729593768389489972 ) ) ;
#20272 = CARTESIAN_POINT ( 'NONE',  ( -19.50000000000000000, 12.99999999999999467, 7.500000000000000000 ) ) ;
#20273 = CARTESIAN_POINT ( 'NONE',  ( -56.23870092848233071, -59.99999999999999289, 88.88512022102443666 ) ) ;
#20274 = CARTESIAN_POINT ( 'NONE',  ( -5.727634848077227225, 4.575561887448870380, -6.326622577870805841 ) ) ;
#20275 = VECTOR ( 'NONE', #15261, 999.9999999999998863 ) ;
#20276 = CARTESIAN_POINT ( 'NONE',  ( -86.39046867320946888, -17.31727863270868895, 180.1964746379083522 ) ) ;
#20277 = ORIENTED_EDGE ( 'NONE', *, *, #100533, .T. ) ;
#20278 = DIRECTION ( 'NONE',  ( 0.000000000000000000, -1.000000000000000000, 0.000000000000000000 ) ) ;
#20279 = CARTESIAN_POINT ( 'NONE',  ( -4.128997488399893889, -60.36574394313192471, 33.94255568994992700 ) ) ;
#20280 = CARTESIAN_POINT ( 'NONE',  ( -5.947849941369417692, 41.98179909877737259, -59.44139789967899645 ) ) ;
#20281 = DIRECTION ( 'NONE',  ( -1.000000000000000000, 0.000000000000000000, 0.000000000000000000 ) ) ;
#20282 = CARTESIAN_POINT ( 'NONE',  ( -7.808575906223166108, 53.96872104851095742, 3.793266769575681430 ) ) ;
#20283 = EDGE_CURVE ( 'NONE', #8439, #88628, #104493, .T. ) ;
#20284 = ORIENTED_EDGE ( 'NONE', *, *, #38678, .T. ) ;
#20285 = CARTESIAN_POINT ( 'NONE',  ( 7.500000000000007105, 25.66666666666802854, -68.91429205785459544 ) ) ;
#20286 = DIRECTION ( 'NONE',  ( -0.5735764363510497121, 0.8191520442889892450, 1.003171929053521665E-16 ) ) ;
#20287 = FILL_AREA_STYLE_COLOUR ( '', #45955 ) ;
#20288 = CARTESIAN_POINT ( 'NONE',  ( -30.25697458664245687, 12.04847113665175584, -39.73669343589890701 ) ) ;
#20289 = AXIS2_PLACEMENT_3D ( 'NONE', #103028, #37258, #100484 ) ;
#20290 = ORIENTED_EDGE ( 'NONE', *, *, #63763, .T. ) ;
#20291 = AXIS2_PLACEMENT_3D ( 'NONE', #47149, #89751, #15847 ) ;
#20292 = CARTESIAN_POINT ( 'NONE',  ( 17.50837830432311293, 50.00000000000002132, 63.40454194101801022 ) ) ;
#20293 = CARTESIAN_POINT ( 'NONE',  ( 90.51111111111110574, -4.171999999999998820, 0.000000000000000000 ) ) ;
#20294 = EDGE_CURVE ( 'NONE', #57566, #23889, #47316, .T. ) ;
#20295 = CARTESIAN_POINT ( 'NONE',  ( -11.19959342722916951, 9.651029144387260302E-13, -19.43146043915260179 ) ) ;
#20296 = LINE ( 'NONE', #44527, #37611 ) ;
#20297 = CARTESIAN_POINT ( 'NONE',  ( 94.55541571559547265, -59.99999999999990763, 22.40038052076814878 ) ) ;
#20298 = CARTESIAN_POINT ( 'NONE',  ( -81.03537519357652741, -42.97169953517784080, 157.4357695269996213 ) ) ;
#20299 = ORIENTED_EDGE ( 'NONE', *, *, #45458, .T. ) ;
#20300 = DIRECTION ( 'NONE',  ( 0.000000000000000000, -0.000000000000000000, 1.000000000000000000 ) ) ;
#20301 = CARTESIAN_POINT ( 'NONE',  ( 41.50669491856072568, 1.482358050883964840E-15, 0.000000000000000000 ) ) ;
#20302 = CIRCLE ( 'NONE', #35762, 6.500000000000000000 ) ;
#20303 = CARTESIAN_POINT ( 'NONE',  ( 31.44210964184475898, -57.68773756896033689, 46.15593347035913041 ) ) ;
#20304 = CIRCLE ( 'NONE', #96009, 4.172000000000001485 ) ;
#20305 = CIRCLE ( 'NONE', #65043, 4.000000000000007105 ) ;
#20306 = MECHANICAL_DESIGN_GEOMETRIC_PRESENTATION_REPRESENTATION (  '', ( #85713 ), #82210 ) ;
#20307 = CARTESIAN_POINT ( 'NONE',  ( 0.000000000000000000, 5.629165124598848102, 3.250000000000005329 ) ) ;
#20308 = CARTESIAN_POINT ( 'NONE',  ( 37.12174742129960947, 348.0611237983079036, 0.6179234092325384120 ) ) ;
#20309 = CARTESIAN_POINT ( 'NONE',  ( 43.55333112596304090, 465.2342844084865874, 9.238213423009668190 ) ) ;
#20310 = VERTEX_POINT ( 'NONE', #6316 ) ;
#20311 = CARTESIAN_POINT ( 'NONE',  ( 5.125709143870056828, 54.24787127484101035, -6.031152949374436467 ) ) ;
#20313 = EDGE_CURVE ( 'NONE', #94433, #91201, #9021, .T. ) ;
#20312 = B_SPLINE_CURVE_WITH_KNOTS ( 'NONE', 3,
 ( #5922, #22684, #105163, #38850 ),
 .UNSPECIFIED., .F., .F.,
 ( 4, 4 ),
 ( 5.386030058153475923E-17, 0.0001964870061225198268 ),
 .UNSPECIFIED. ) ;
#20314 = CARTESIAN_POINT ( 'NONE',  ( 31.36162942603217019, 438.6301898249564601, 22.30086042418462711 ) ) ;
#20315 = CARTESIAN_POINT ( 'NONE',  ( 4.401442555609581635E-16, -24.78125000204838813, -7.188101187500000044 ) ) ;
#20316 = ORIENTED_EDGE ( 'NONE', *, *, #14379, .T. ) ;
#20317 = SURFACE_STYLE_FILL_AREA ( #60214 ) ;
#20318 = CIRCLE ( 'NONE', #37472, 5.000000000000000888 ) ;
#20319 = FACE_OUTER_BOUND ( 'NONE', #12908, .T. ) ;
#20320 = CARTESIAN_POINT ( 'NONE',  ( 6.101170550526181735, 41.83126063020969099, -70.32427471769284466 ) ) ;
#20321 = CARTESIAN_POINT ( 'NONE',  ( -54.34415824576156950, 50.00000000000000000, -32.38913437803946493 ) ) ;
#20322 = DIRECTION ( 'NONE',  ( -1.000000000000000000, -0.000000000000000000, -0.000000000000000000 ) ) ;
#20323 = AXIS2_PLACEMENT_3D ( 'NONE', #77786, #4958, #95558 ) ;
#20324 = CARTESIAN_POINT ( 'NONE',  ( 6.249999999999998224, -9.237604307034018802, 3.355146209984123968E-17 ) ) ;
#20325 = ORIENTED_EDGE ( 'NONE', *, *, #83854, .T. ) ;
#20326 = CARTESIAN_POINT ( 'NONE',  ( 78.09008153237981276, -60.00000000000002132, -28.99347257546710210 ) ) ;
#20328 = CARTESIAN_POINT ( 'NONE',  ( 20.95262001139231600, -25.55370161815428176, 28.74710842965579261 ) ) ;
#20327 = CARTESIAN_POINT ( 'NONE',  ( -73.77866262884730020, -30.00000000000000711, 147.9509455049667395 ) ) ;
#20329 = CARTESIAN_POINT ( 'NONE',  ( 40.11650669486618881, 4.898587196589411843E-16, -4.000000000000000888 ) ) ;
#20330 = CARTESIAN_POINT ( 'NONE',  ( -36.40588522426740070, -29.12245875214614088, 34.06417451330221269 ) ) ;
#20331 = UNCERTAINTY_MEASURE_WITH_UNIT (LENGTH_MEASURE( 1.000000000000000082E-05 ), #54050, 'distance_accuracy_value', 'NONE');
#20332 = ORIENTED_EDGE ( 'NONE', *, *, #44424, .F. ) ;
#20333 = CARTESIAN_POINT ( 'NONE',  ( 33.50665702490327647, 462.9566363596913448, 5.621882783608548984 ) ) ;
#20334 = CARTESIAN_POINT ( 'NONE',  ( 0.000000000000000000, -50.00000000000000000, 112.0000000000000000 ) ) ;
#20335 = DIRECTION ( 'NONE',  ( 0.000000000000000000, 0.000000000000000000, 1.000000000000000000 ) ) ;
#20336 = CARTESIAN_POINT ( 'NONE',  ( 4.699999999999999289, 1.502314598737160215E-15, -6.499999999999999112 ) ) ;
#20337 = CARTESIAN_POINT ( 'NONE',  ( 5.975663821520835306, 7.000939006314205848, 0.8740179403730332641 ) ) ;
#20338 = CARTESIAN_POINT ( 'NONE',  ( 12.40471543347789485, -3.812522371550363331, 20.50938476615066719 ) ) ;
#20340 = ORIENTED_EDGE ( 'NONE', *, *, #68519, .F. ) ;
#20339 = CIRCLE ( 'NONE', #90884, 2.000000000000001776 ) ;
#20341 = CARTESIAN_POINT ( 'NONE',  ( -75.97346622875217292, -38.37623792979642445, 178.1546702465331862 ) ) ;
#20342 = FACE_OUTER_BOUND ( 'NONE', #35292, .T. ) ;
#20343 = CARTESIAN_POINT ( 'NONE',  ( 97.84284621570628815, -29.99999999999976907, 190.6742164480843087 ) ) ;
#20344 = CARTESIAN_POINT ( 'NONE',  ( -11.77939662183895386, 6.782627062745584468, -9.100507241011085213 ) ) ;
#20345 = CARTESIAN_POINT ( 'NONE',  ( 0.000000000000000000, 15.00000000000000000, 10.00000000000000000 ) ) ;
#20346 = CIRCLE ( 'NONE', #25473, 4.250000000000000000 ) ;
#20347 = CARTESIAN_POINT ( 'NONE',  ( 81.30983963799556591, -30.00000000000000355, -0.6510870460054363207 ) ) ;
#20348 =( BOUNDED_SURFACE ( )  B_SPLINE_SURFACE ( 3, 2, ( 
 ( #21218, #29310, #37403 ),
 ( #54048, #4462, #53016 ),
 ( #62200, #61669, #46510 ),
 ( #70264, #95086, #86993 ) ),
 .UNSPECIFIED., .F., .F., .T. ) 
 B_SPLINE_SURFACE_WITH_KNOTS ( ( 4, 4 ),
 ( 3, 3 ),
 ( 1.934216675714139910E-16, 0.0007499009164755209749 ),
 ( 0.000000000000000000, 1.000000000000000000 ),
 .UNSPECIFIED. ) 
 GEOMETRIC_REPRESENTATION_ITEM ( )  RATIONAL_B_SPLINE_SURFACE ( (
 ( 1.000000000000000000, 0.7301269460247277188, 1.000000000000000000),
 ( 1.000000000000000000, 0.7327382575064924630, 1.000000000000000000),
 ( 1.000000000000000000, 0.7350727526496084741, 1.000000000000000000),
 ( 1.000000000000000000, 0.7370557512816053869, 1.000000000000000000) ) ) 
 REPRESENTATION_ITEM ( '' )  SURFACE ( )  );
#20349 = DIRECTION ( 'NONE',  ( -1.000000000000000000, -1.224606353822377258E-16, -0.000000000000000000 ) ) ;
#20350 = ORIENTED_EDGE ( 'NONE', *, *, #69888, .T. ) ;
#20351 = EDGE_CURVE ( 'NONE', #36441, #99443, #368, .T. ) ;
#20352 = EDGE_LOOP ( 'NONE', ( #102665, #21127, #16785, #103335 ) ) ;
#20353 = ORIENTED_EDGE ( 'NONE', *, *, #11957, .F. ) ;
#20354 = DIRECTION ( 'NONE',  ( -0.000000000000000000, 0.000000000000000000, -1.000000000000000000 ) ) ;
#20355 = SURFACE_STYLE_FILL_AREA ( #95780 ) ;
#20356 = CARTESIAN_POINT ( 'NONE',  ( -4.999999999999993783, -46.00000000000000000, 103.3397459621556180 ) ) ;
#20357 = CARTESIAN_POINT ( 'NONE',  ( -3.313708498984722528, -16.71875000409677270, -8.000000000000040856 ) ) ;
#20358 = CARTESIAN_POINT ( 'NONE',  ( -0.8750000000010113022, -70.58759490697451611, 13.02737050516266493 ) ) ;
#20359 = CARTESIAN_POINT ( 'NONE',  ( 12.37144696128342147, -4.000000000000003553, 20.44658103856077602 ) ) ;
#20361 = EDGE_CURVE ( 'NONE', #86195, #72492, #10674, .T. ) ;
#20360 =( NAMED_UNIT ( * ) SI_UNIT ( $, .STERADIAN. ) SOLID_ANGLE_UNIT ( ) );
#20362 = VECTOR ( 'NONE', #32773, 1000.000000000000000 ) ;
#20363 = ORIENTED_EDGE ( 'NONE', *, *, #101815, .T. ) ;
#20364 = CARTESIAN_POINT ( 'NONE',  ( -1.570796324980112679, 50.00000000000000000, -97.00000000000000000 ) ) ;
#20365 = ORIENTED_EDGE ( 'NONE', *, *, #21824, .F. ) ;
#20366 = CARTESIAN_POINT ( 'NONE',  ( -4.904566723942681783, -62.97757297529252440, 3.460360782932704549 ) ) ;
#20367 = DIRECTION ( 'NONE',  ( -1.000000000000000000, -0.000000000000000000, -0.000000000000000000 ) ) ;
#20368 = CARTESIAN_POINT ( 'NONE',  ( -41.31161337382455656, 484.8232235214489378, -3.619187650532241562 ) ) ;
#20369 = B_SPLINE_CURVE_WITH_KNOTS ( 'NONE', 3,
 ( #46599, #21831, #14216, #39059, #54670, #88654, #103251, #21302, #70879, #80546, #62799, #47649, #29396, #55725, #103773, #94650, #79497, #95687 ),
 .UNSPECIFIED., .F., .F.,
 ( 4, 2, 2, 2, 2, 2, 2, 2, 4 ),
 ( 0.01279774649274978589, 0.01359624981427548680, 0.01439475313580118598, 0.01519325645732688690, 0.01599175977885258781, 0.01679026310037829567, 0.01758876642190399311, 0.01838726974342969403, 0.01918577306495539495 ),
 .UNSPECIFIED. ) ;
#20370 = CARTESIAN_POINT ( 'NONE',  ( 24.65765876571508031, 295.6277211468342898, 10.10369318520652193 ) ) ;
#20371 = DIRECTION ( 'NONE',  ( 0.5735764363510490460, 0.8191520442889896891, 0.000000000000000000 ) ) ;
#20372 = CARTESIAN_POINT ( 'NONE',  ( 58.58033085486675162, -60.33174129239029782, 78.30550325338386131 ) ) ;
#20373 = VERTEX_POINT ( 'NONE', #33829 ) ;
#20374 = CARTESIAN_POINT ( 'NONE',  ( 28.58246259357159857, 11.06567680426941713, -41.45945986390915294 ) ) ;
#20375 = DIRECTION ( 'NONE',  ( 0.000000000000000000, 0.000000000000000000, 1.000000000000000000 ) ) ;
#20376 = CARTESIAN_POINT ( 'NONE',  ( -6.705020855549795655, 9.539818418972618730, -2.023228926981749609 ) ) ;
#20377 = CARTESIAN_POINT ( 'NONE',  ( -9.317927955922566952, 51.34044562560666236, 3.778188453665225932 ) ) ;
#20378 = EDGE_CURVE ( 'NONE', #103206, #91640, #7246, .T. ) ;
#20379 = ORIENTED_EDGE ( 'NONE', *, *, #1198, .T. ) ;
#20380 = SURFACE_SIDE_STYLE ('',( #102835 ) ) ;
#20381 = CARTESIAN_POINT ( 'NONE',  ( 0.000000000000000000, 48.00000000000000000, 0.000000000000000000 ) ) ;
#20382 = AXIS2_PLACEMENT_3D ( 'NONE', #11735, #35538, #12277 ) ;
#20383 = AXIS2_PLACEMENT_3D ( 'NONE', #17865, #50208, #66940 ) ;
#20384 = CARTESIAN_POINT ( 'NONE',  ( -7.934996450857311423, 101.1313754352746912, -1.050865690281777676 ) ) ;
#20385 = AXIS2_PLACEMENT_3D ( 'NONE', #11715, #25845, #100208 ) ;
#20386 = LINE ( 'NONE', #78030, #70945 ) ;
#20387 = CIRCLE ( 'NONE', #80586, 13.99700487351915612 ) ;
#20388 = CARTESIAN_POINT ( 'NONE',  ( 85.76763381879807469, -50.17746128774981429, 190.4771001175396634 ) ) ;
#20389 = CARTESIAN_POINT ( 'NONE',  ( 44.28985889617170102, 463.6758032475478899, 7.532946519189393619 ) ) ;
#20390 = CARTESIAN_POINT ( 'NONE',  ( -7.989648714934757479, 50.29308867530622251, 5.000000000000000888 ) ) ;
#20391 = VERTEX_POINT ( 'NONE', #67245 ) ;
#20392 = CARTESIAN_POINT ( 'NONE',  ( -7.500000000000000000, 4.330127018922188320, -7.422398894150033399 ) ) ;
#20393 = DIRECTION ( 'NONE',  ( 0.000000000000000000, 0.000000000000000000, 1.000000000000000000 ) ) ;
#20394 = CARTESIAN_POINT ( 'NONE',  ( 27.59999999999999787, 4.172000000000003261, 5.109226446042759579E-16 ) ) ;
#20395 = CARTESIAN_POINT ( 'NONE',  ( 0.000000000000000000, 0.000000000000000000, -0.02540000000000007530 ) ) ;
#20396 = CARTESIAN_POINT ( 'NONE',  ( -89.87360357950815626, -30.00000000000000355, 87.74932085497819401 ) ) ;
#20397 = CIRCLE ( 'NONE', #34150, 4.000000000000000888 ) ;
#20398 = CARTESIAN_POINT ( 'NONE',  ( -2.133938722758583761, -6.273523403446334079, -0.09463688534108292971 ) ) ;
#20399 = CARTESIAN_POINT ( 'NONE',  ( 28.45062504421127869, -57.68029023625437191, 44.48305370826658844 ) ) ;
#20401 = FILL_AREA_STYLE_COLOUR ( '', #89557 ) ;
#20400 = CARTESIAN_POINT ( 'NONE',  ( 11.66726770654783252, 11.72242249675092474, -9.937599956974251469 ) ) ;
#20402 = COLOUR_RGB ( '', 0.72549020, 0.75294118, 0.79215686) ;
#20403 = FACE_OUTER_BOUND ( 'NONE', #27021, .T. ) ;
#20404 = CARTESIAN_POINT ( 'NONE',  ( -50.55323482659543544, -37.96401913402925032, 51.13833031541544472 ) ) ;
#20405 = CARTESIAN_POINT ( 'NONE',  ( 5.000000000000000000, -15.62228920881129390, 12.61250543006183378 ) ) ;
#20406 = SURFACE_STYLE_FILL_AREA ( #78049 ) ;
#20407 = CARTESIAN_POINT ( 'NONE',  ( 3.778422651548691391, -1.120239677707988823, 103.2432416460067657 ) ) ;
#20408 = CARTESIAN_POINT ( 'NONE',  ( 15.53065903970252037, -17.36263754172462015, -34.27975487217998563 ) ) ;
#20409 = COLOUR_RGB ( '', 0.40784314, 0.44705882, 0.49803922) ;
#20410 = PRESENTATION_STYLE_ASSIGNMENT (( #69963 ) ) ;
#20411 = CARTESIAN_POINT ( 'NONE',  ( -26.29831070025733553, -29.04849030947340793, 30.24692729650839951 ) ) ;
#20412 = ORIENTED_EDGE ( 'NONE', *, *, #99802, .F. ) ;
#20413 = CARTESIAN_POINT ( 'NONE',  ( 39.65885301127772067, 485.6927826267698833, -4.533530942913213124 ) ) ;
#20414 = CARTESIAN_POINT ( 'NONE',  ( 0.000000000000000000, 0.000000000000000000, 0.000000000000000000 ) ) ;
#20415 = CARTESIAN_POINT ( 'NONE',  ( -17.81292157518379327, -35.99535881907262080, 30.19758427183107230 ) ) ;
#20417 = LINE ( 'NONE', #3108, #78379 ) ;
#20416 = DIRECTION ( 'NONE',  ( -1.000000000000000000, -1.224606353822377258E-16, -0.000000000000000000 ) ) ;
#20418 = EDGE_CURVE ( 'NONE', #96607, #17199, #98565, .T. ) ;
#20419 = ORIENTED_EDGE ( 'NONE', *, *, #86848, .T. ) ;
#20420 = AXIS2_PLACEMENT_3D ( 'NONE', #256, #58554, #25137 ) ;
#20421 = EDGE_LOOP ( 'NONE', ( #7195, #67081, #50496, #67939, #6862 ) ) ;
#20422 = CARTESIAN_POINT ( 'NONE',  ( 10.51296777078104050, 50.00000000000000000, -92.64705882352942012 ) ) ;
#20423 = EDGE_CURVE ( 'NONE', #71461, #71251, #75059, .T. ) ;
#20424 = CARTESIAN_POINT ( 'NONE',  ( 13.69330508143927538, 5.000000000000004441, 6.123233995736770227E-16 ) ) ;
#20425 = CARTESIAN_POINT ( 'NONE',  ( -8.979652892184141422, -60.00000000000000711, -42.45601304278074650 ) ) ;
#20426 = ORIENTED_EDGE ( 'NONE', *, *, #29916, .F. ) ;
#20427 = DIRECTION ( 'NONE',  ( 0.000000000000000000, 0.000000000000000000, 1.000000000000000000 ) ) ;
#20428 = CARTESIAN_POINT ( 'NONE',  ( 11.99986829839305535, 50.00000000000000711, -86.59063654372916119 ) ) ;
#20429 = CARTESIAN_POINT ( 'NONE',  ( 101.4379291727228036, -37.84844671077693334, 186.7608123887999909 ) ) ;
#20430 = EDGE_CURVE ( 'NONE', #66070, #21786, #52058, .T. ) ;
#20431 = VECTOR ( 'NONE', #44804, 1000.000000000000000 ) ;
#20433 = CARTESIAN_POINT ( 'NONE',  ( 35.00384615384614762, -4.171999999999999709, 5.616230220889763424E-16 ) ) ;
#20432 = CARTESIAN_POINT ( 'NONE',  ( 44.66113381551566874, -36.82664275380086139, 42.44229676395095652 ) ) ;
#20434 = CIRCLE ( 'NONE', #18719, 4.000000000000007105 ) ;
#20435 = ORIENTED_EDGE ( 'NONE', *, *, #29726, .F. ) ;
#20436 = ADVANCED_FACE ( 'NONE', ( #850 ), #95561, .T. ) ;
#20437 = EDGE_LOOP ( 'NONE', ( #59810, #89478, #19442, #74789 ) ) ;
#20438 = EDGE_LOOP ( 'NONE', ( #101159, #29953, #74118, #106170 ) ) ;
#20439 = CARTESIAN_POINT ( 'NONE',  ( 22.75333575518925855, 305.5577985524777773, 10.09022899150792973 ) ) ;
#20440 = CARTESIAN_POINT ( 'NONE',  ( -18.00000000000000355, 12.99999999999999289, 9.500000000000000000 ) ) ;
#20441 = ORIENTED_EDGE ( 'NONE', *, *, #68612, .T. ) ;
#20442 = DIRECTION ( 'NONE',  ( -1.000000000000000000, -1.224606353822377258E-16, -0.000000000000000000 ) ) ;
#20443 = CARTESIAN_POINT ( 'NONE',  ( -6.159997634473088013, 41.93068719192066141, -70.02314903893139331 ) ) ;
#20444 = CARTESIAN_POINT ( 'NONE',  ( -93.72600522304895776, -59.99999999999028688, -16.51119016088236080 ) ) ;
#20445 = CARTESIAN_POINT ( 'NONE',  ( 0.000000000000000000, 50.00000000000000000, 0.000000000000000000 ) ) ;
#20446 = AXIS2_PLACEMENT_3D ( 'NONE', #103827, #29971, #80074 ) ;
#20447 = CARTESIAN_POINT ( 'NONE',  ( 91.37614370737277625, -59.99999999998070876, -21.18689035136125298 ) ) ;
#20448 = DIRECTION ( 'NONE',  ( 0.000000000000000000, 0.000000000000000000, -1.000000000000000000 ) ) ;
#20449 = PRESENTATION_LAYER_ASSIGNMENT (  '', '', ( #66894 ) ) ;
#20450 = CARTESIAN_POINT ( 'NONE',  ( -6.373568580003205142, 41.63985673647684393, -58.70717887382906497 ) ) ;
#20451 = AXIS2_PLACEMENT_3D ( 'NONE', #102999, #62032, #94924 ) ;
#20453 = CARTESIAN_POINT ( 'NONE',  ( 6.163491381871265773, -49.91567759485347011, 32.19897774480319441 ) ) ;
#20452 = CARTESIAN_POINT ( 'NONE',  ( -102.4477130004285499, -30.00000000000004974, 111.1018478433771151 ) ) ;
#20454 = AXIS2_PLACEMENT_3D ( 'NONE', #56074, #106233, #32393 ) ;
#20455 = CARTESIAN_POINT ( 'NONE',  ( 29.34999999999999787, 1.533819458162526451E-15, 0.000000000000000000 ) ) ;
#20456 = CARTESIAN_POINT ( 'NONE',  ( -49.59501341947334652, -22.20558386076936941, 44.49776195370446885 ) ) ;
#20457 = ORIENTED_EDGE ( 'NONE', *, *, #91027, .F. ) ;
#20458 = CARTESIAN_POINT ( 'NONE',  ( 4.117685099651370528, -69.22520594386868709, 13.61356083086173285 ) ) ;
#20459 = VERTEX_POINT ( 'NONE', #50495 ) ;
#20460 = DIRECTION ( 'NONE',  ( -0.5735764363510494901, -0.8191520442889894671, 0.000000000000000000 ) ) ;
#20461 = VECTOR ( 'NONE', #78280, 1000.000000000000000 ) ;
#20462 = CARTESIAN_POINT ( 'NONE',  ( 5.725004243152316263, -6.424808517446342293, -1.812899781754680362 ) ) ;
#20463 = ORIENTED_EDGE ( 'NONE', *, *, #76970, .T. ) ;
#20464 = CARTESIAN_POINT ( 'NONE',  ( -15.90614609307868577, -3.157894736842101757, 14.66382285868950852 ) ) ;
#20465 = ORIENTED_EDGE ( 'NONE', *, *, #27705, .T. ) ;
#20466 = CARTESIAN_POINT ( 'NONE',  ( 100.1190857666780261, -30.00000000013407586, 97.11980566123828851 ) ) ;
#20467 = CARTESIAN_POINT ( 'NONE',  ( 0.000000000000000000, 0.000000000000000000, 0.000000000000000000 ) ) ;
#20468 = CARTESIAN_POINT ( 'NONE',  ( 3.534854069001187593, -48.92952247113088760, 104.4405781011833483 ) ) ;
#20469 = DIRECTION ( 'NONE',  ( 0.000000000000000000, 1.000000000000000000, 0.000000000000000000 ) ) ;
#20470 = CARTESIAN_POINT ( 'NONE',  ( -1.233923992984923027E-14, 18.64316884711714195, -38.36535705883633085 ) ) ;
#20471 = CARTESIAN_POINT ( 'NONE',  ( 98.43868682546687410, -30.00000000000000355, 189.9420339001966340 ) ) ;
#20472 = DIRECTION ( 'NONE',  ( 0.000000000000000000, 0.000000000000000000, 1.000000000000000000 ) ) ;
#20473 = ORIENTED_EDGE ( 'NONE', *, *, #55290, .F. ) ;
#20474 = EDGE_CURVE ( 'NONE', #76724, #88866, #77559, .T. ) ;
#20475 = CIRCLE ( 'NONE', #39362, 15.00000000000001243 ) ;
#20476 = ORIENTED_EDGE ( 'NONE', *, *, #44063, .T. ) ;
#20477 = B_SPLINE_CURVE_WITH_KNOTS ( 'NONE', 3,
 ( #57192, #73912, #89057, #90643, #39457, #98712, #99243, #88529, #56116, #105239, #90108, #106272, #64261, #520, #65309, #24349, #9408, #16752, #16213, #33484, #15154, #81461, #49099, #72843, #49642, #97652 ),
 .UNSPECIFIED., .F., .F.,
 ( 4, 2, 2, 2, 2, 2, 2, 2, 2, 2, 2, 2, 4 ),
 ( 0.001419956731861227216, 0.001671840766058725310, 0.001923724800256223404, 0.002175608834453721715, 0.002427492868651219375, 0.002931260937046222936, 0.003183144971243733173, 0.003435029005441242976, 0.004442565142231283924, 0.004694449176428796763, 0.004946333210626309602, 0.005198217244823822442, 0.005450101279021335281 ),
 .UNSPECIFIED. ) ;
#20478 = ORIENTED_EDGE ( 'NONE', *, *, #49670, .F. ) ;
#20479 = CARTESIAN_POINT ( 'NONE',  ( 54.35033192401171931, -39.49854378541087385, 58.91923346858290245 ) ) ;
#20480 = DIRECTION ( 'NONE',  ( -1.000000000000000000, -1.224606353822377258E-16, -0.000000000000000000 ) ) ;
#20481 = CARTESIAN_POINT ( 'NONE',  ( -5.500000000000006217, 42.00000000000000000, -59.28631038546422616 ) ) ;
#20482 = EDGE_CURVE ( 'NONE', #52131, #19034, #33155, .T. ) ;
#20483 = EDGE_CURVE ( 'NONE', #93666, #32543, #36543, .T. ) ;
#20485 = ORIENTED_EDGE ( 'NONE', *, *, #93507, .F. ) ;
#20484 = PRESENTATION_LAYER_ASSIGNMENT (  '', '', ( #80921 ) ) ;
#20486 = CARTESIAN_POINT ( 'NONE',  ( -88.47893304564723849, -38.37741962354056824, -18.89372368499410371 ) ) ;
#20487 = CIRCLE ( 'NONE', #77242, 4.000000000000000888 ) ;
#20488 = ORIENTED_EDGE ( 'NONE', *, *, #82996, .T. ) ;
#20489 = DIRECTION ( 'NONE',  ( 1.000000000000000000, 0.000000000000000000, 0.000000000000000000 ) ) ;
#20490 = CARTESIAN_POINT ( 'NONE',  ( 101.6090991099778336, -38.45020037725543460, 199.8721891155738035 ) ) ;
#20491 = CARTESIAN_POINT ( 'NONE',  ( 12.69346561929714490, 18.63831398217661928, 8.263378152524056830 ) ) ;
#20492 = CARTESIAN_POINT ( 'NONE',  ( 86.60698052122229740, -60.14205719110204029, 0.8374838849679312469 ) ) ;
#20493 = CARTESIAN_POINT ( 'NONE',  ( 40.93034849641253459, 415.5868670752544176, 27.59989424832417626 ) ) ;
#20494 = CARTESIAN_POINT ( 'NONE',  ( 1.916513513605337504, -7.172711491783059223, -13.28747680017345623 ) ) ;
#20495 = CARTESIAN_POINT ( 'NONE',  ( -43.80679553850465169, 434.9371637098606698, 12.86766421698907514 ) ) ;
#20496 = CARTESIAN_POINT ( 'NONE',  ( 0.9999999999999940048, 0.000000000000000000, 101.0455488498966758 ) ) ;
#20497 = EDGE_LOOP ( 'NONE', ( #105389, #50923, #102566, #30499, #100608, #47452 ) ) ;
#20498 = CARTESIAN_POINT ( 'NONE',  ( -12.44963615905739474, -4.333246069852321192, -12.76855431059839141 ) ) ;
#20499 = ADVANCED_FACE ( 'NONE', ( #12700 ), #92719, .T. ) ;
#20500 = CARTESIAN_POINT ( 'NONE',  ( 0.000000000000000000, 4.898587196589412829E-16, -4.000000000000000000 ) ) ;
#20501 = DIRECTION ( 'NONE',  ( 0.000000000000000000, -1.000000000000000000, 0.000000000000000000 ) ) ;
#20502 = ORIENTED_EDGE ( 'NONE', *, *, #71393, .T. ) ;
#20503 = CARTESIAN_POINT ( 'NONE',  ( -20.96340531204895186, 304.9350079645578262, -8.982323148433966509 ) ) ;
#20504 = AXIS2_PLACEMENT_3D ( 'NONE', #55600, #95566, #87484 ) ;
#20505 = CARTESIAN_POINT ( 'NONE',  ( -39.21858437040845757, 325.7412493439550758, 17.46750275458761692 ) ) ;
#20506 = CARTESIAN_POINT ( 'NONE',  ( 31.08349330513380693, -4.000000000000000888, 4.898587196589416773E-16 ) ) ;
#20507 = CARTESIAN_POINT ( 'NONE',  ( -12.13034742782246767, 42.00000000000000000, -93.82352941176338845 ) ) ;
#20508 = CARTESIAN_POINT ( 'NONE',  ( 8.000000000000000000, -19.90624999999999289, -3.313708498984761608 ) ) ;
#20509 = CARTESIAN_POINT ( 'NONE',  ( -30.81281672544767858, -32.99113872632139532, 41.04263858266035214 ) ) ;
#20510 =( BOUNDED_SURFACE ( )  B_SPLINE_SURFACE ( 3, 2, ( 
 ( #71410, #38034, #30459 ),
 ( #62814, #37508, #28343 ),
 ( #70896, #61769, #21315 ),
 ( #36970, #103785, #70371 ),
 ( #47136, #29928, #20274 ),
 ( #77929, #94665, #53125 ) ),
 .UNSPECIFIED., .F., .F., .F. ) 
 B_SPLINE_SURFACE_WITH_KNOTS ( ( 4, 2, 4 ),
 ( 3, 3 ),
 ( 0.003190620565844210377, 0.007281897438794483236, 0.01137317431174475653 ),
 ( 0.000000000000000000, 1.000000000000000000 ),
 .UNSPECIFIED. ) 
 GEOMETRIC_REPRESENTATION_ITEM ( )  RATIONAL_B_SPLINE_SURFACE ( (
 ( 1.000000000000000000, 0.8047731410850398337, 1.000000000000000000),
 ( 1.000000000000000000, 0.8125552299157385860, 1.000000000000000000),
 ( 1.000000000000000000, 0.8191520442888333697, 1.000000000000000000),
 ( 1.000000000000000000, 0.8191520442891397913, 1.000000000000000000),
 ( 1.000000000000000000, 0.8125552299155083258, 1.000000000000000000),
 ( 1.000000000000000000, 0.8047731410850402778, 1.000000000000000000) ) ) 
 REPRESENTATION_ITEM ( '' )  SURFACE ( )  );
#20511 = EDGE_CURVE ( 'NONE', #19922, #77684, #52628, .T. ) ;
#20512 = DIRECTION ( 'NONE',  ( -1.000000000000000000, -1.224606353822377258E-16, -0.000000000000000000 ) ) ;
#20513 = VERTEX_POINT ( 'NONE', #14287 ) ;
#20514 = CARTESIAN_POINT ( 'NONE',  ( 86.06137632241674851, -21.58008244112160057, 174.3352827979300912 ) ) ;
#20515 = EDGE_CURVE ( 'NONE', #35550, #14924, #72534, .T. ) ;
#20516 = CARTESIAN_POINT ( 'NONE',  ( -49.19520577559744368, 7.745679164654304394, 16.05969994618030228 ) ) ;
#20517 = VECTOR ( 'NONE', #76708, 1000.000000000000000 ) ;
#20518 = CARTESIAN_POINT ( 'NONE',  ( -86.96108843841854252, -39.85768485184852494, 189.1641270546835187 ) ) ;
#20519 = EDGE_LOOP ( 'NONE', ( #46549, #22760, #52869, #25629 ) ) ;
#20520 = CARTESIAN_POINT ( 'NONE',  ( -96.80243442732822245, -45.26554055243965280, 111.1114493365296454 ) ) ;
#20521 = CARTESIAN_POINT ( 'NONE',  ( 6.162888688655347558, -3.752776749732574135, -6.500000000000001776 ) ) ;
#20522 = CARTESIAN_POINT ( 'NONE',  ( 5.385673916453011856, 3.999999999999999112, 18.57417562100670949 ) ) ;
#20523 = CARTESIAN_POINT ( 'NONE',  ( -30.36574723454835478, 11.76891213769395428, 39.80121650896526120 ) ) ;
#20524 =( NAMED_UNIT ( * ) SI_UNIT ( $, .STERADIAN. ) SOLID_ANGLE_UNIT ( ) );
#20525 = CARTESIAN_POINT ( 'NONE',  ( 32.53666910739249829, -59.99999999999999289, 44.50982780536016037 ) ) ;
#20526 = CARTESIAN_POINT ( 'NONE',  ( 18.87214478678923157, -24.99265787794756477, 36.59434658705920640 ) ) ;
#20527 = PRESENTATION_STYLE_ASSIGNMENT (( #54388 ) ) ;
#20528 = CARTESIAN_POINT ( 'NONE',  ( 33.61216083118301157, -23.40945894981453534, 33.02634255258320195 ) ) ;
#20529 = CIRCLE ( 'NONE', #34276, 4.000000000000007105 ) ;
#20531 = CARTESIAN_POINT ( 'NONE',  ( -12.68594940236797797, 18.62354890192223422, 8.273500667382888807 ) ) ;
#20530 = CARTESIAN_POINT ( 'NONE',  ( -29.99900812854675891, -32.45003448039427951, 40.57373401099567900 ) ) ;
#20532 = CARTESIAN_POINT ( 'NONE',  ( 8.984970058459877507, 294.6717433611685237, -4.394086705239145907 ) ) ;
#20533 = DIRECTION ( 'NONE',  ( 0.000000000000000000, 0.000000000000000000, 1.000000000000000000 ) ) ;
#20534 = SURFACE_SIDE_STYLE ('',( #3765 ) ) ;
#20535 = DIRECTION ( 'NONE',  ( 1.000000000000000000, 1.224606353822377258E-16, 0.000000000000000000 ) ) ;
#20536 = AXIS2_PLACEMENT_3D ( 'NONE', #31363, #64240, #48017 ) ;
#20537 = DIRECTION ( 'NONE',  ( -0.000000000000000000, -0.000000000000000000, -1.000000000000000000 ) ) ;
#20538 = ORIENTED_EDGE ( 'NONE', *, *, #70856, .F. ) ;
#20539 = CARTESIAN_POINT ( 'NONE',  ( -13.68764148674883430, 294.5450735065955996, 9.871802096439328267 ) ) ;
#20540 = DIRECTION ( 'NONE',  ( -1.000000000000000000, -0.000000000000000000, -0.000000000000000000 ) ) ;
#20541 = ORIENTED_EDGE ( 'NONE', *, *, #75555, .F. ) ;
#20542 = CARTESIAN_POINT ( 'NONE',  ( -9.877897116810617106, -2.622329759909478586, 15.38437439719164779 ) ) ;
#20543 = PRESENTATION_STYLE_ASSIGNMENT (( #29153 ) ) ;
#20544 = CARTESIAN_POINT ( 'NONE',  ( 4.497431761510337189, -64.45901875748970156, -3.972160586670089089 ) ) ;
#20546 = CARTESIAN_POINT ( 'NONE',  ( -12.44840434870106449, -21.77031870854123241, -30.18225557512956314 ) ) ;
#20545 =( NAMED_UNIT ( * ) PLANE_ANGLE_UNIT ( ) SI_UNIT ( $, .RADIAN. ) );
#20547 = EDGE_CURVE ( 'NONE', #34601, #23687, #96880, .T. ) ;
#20548 = VERTEX_POINT ( 'NONE', #56332 ) ;
#20549 = B_SPLINE_CURVE_WITH_KNOTS ( 'NONE', 3,
 ( #95541, #37345, #78814, #103109, #79348, #77770, #20110, #3883 ),
 .UNSPECIFIED., .F., .F.,
 ( 4, 2, 2, 4 ),
 ( 8.673617379884035472E-19, 0.0001460451837441968887, 0.0002190677756162943436, 0.0002920903674883918257 ),
 .UNSPECIFIED. ) ;
#20550 = CIRCLE ( 'NONE', #3317, 5.000000000000002665 ) ;
#20551 = DIRECTION ( 'NONE',  ( 0.000000000000000000, 0.000000000000000000, 1.000000000000000000 ) ) ;
#20552 = SURFACE_SIDE_STYLE ('',( #94387 ) ) ;
#20553 = ORIENTED_EDGE ( 'NONE', *, *, #4281, .T. ) ;
#20554 = ADVANCED_FACE ( 'NONE', ( #88731 ), #103842, .F. ) ;
#20555 = AXIS2_PLACEMENT_3D ( 'NONE', #41364, #99592, #90996 ) ;
#20556 = ADVANCED_FACE ( 'NONE', ( #48247 ), #88266, .T. ) ;
#20557 = CARTESIAN_POINT ( 'NONE',  ( 30.48982775277875135, 7.748378201987732972, -41.81310123456357530 ) ) ;
#20558 = AXIS2_PLACEMENT_3D ( 'NONE', #81079, #7189, #105372 ) ;
#20559 = CARTESIAN_POINT ( 'NONE',  ( -93.51973230106480628, -60.00000000000000711, 37.21323270788247584 ) ) ;
#20560 = ORIENTED_EDGE ( 'NONE', *, *, #98343, .T. ) ;
#20561 = CARTESIAN_POINT ( 'NONE',  ( 13.09999999999999787, -3.309499999999999886, 4.475777889183790779E-16 ) ) ;
#20562 = CARTESIAN_POINT ( 'NONE',  ( 25.21823338009918203, 1.482358050883964840E-15, 0.000000000000000000 ) ) ;
#20563 = CARTESIAN_POINT ( 'NONE',  ( 9.819056950928633398, 294.6481068335447731, 1.893705519456528208 ) ) ;
#20564 =( LENGTH_UNIT ( ) NAMED_UNIT ( * ) SI_UNIT ( .MILLI., .METRE. ) );
#20565 = CARTESIAN_POINT ( 'NONE',  ( -81.30226012367107558, -53.44438453014575430, 176.1360694353149938 ) ) ;
#20566 = ORIENTED_EDGE ( 'NONE', *, *, #91617, .T. ) ;
#20567 = CARTESIAN_POINT ( 'NONE',  ( -16.46939662768732049, -0.000000000000000000, 4.418225343323818777 ) ) ;
#20568 = EDGE_CURVE ( 'NONE', #31711, #73538, #99512, .T. ) ;
#20569 = ORIENTED_EDGE ( 'NONE', *, *, #37183, .F. ) ;
#20570 = ADVANCED_FACE ( 'NONE', ( #87681 ), #56869, .F. ) ;
#20571 = ORIENTED_EDGE ( 'NONE', *, *, #99508, .T. ) ;
#20572 = CARTESIAN_POINT ( 'NONE',  ( -5.000000000000080824, -12.34932486159458342, 8.854147762507302843 ) ) ;
#20573 = DIRECTION ( 'NONE',  ( 0.000000000000000000, -1.000000000000000000, 0.000000000000000000 ) ) ;
#20574 = VERTEX_POINT ( 'NONE', #22958 ) ;
#20575 = CARTESIAN_POINT ( 'NONE',  ( -3.068228200247434202E-15, 53.37899725327129374, 25.05398456423234066 ) ) ;
#20576 = CARTESIAN_POINT ( 'NONE',  ( -94.60030117187078247, -57.66721437216608592, -3.115894729640209526 ) ) ;
#20577 = DIRECTION ( 'NONE',  ( -1.000000000000000000, -0.000000000000000000, -0.000000000000000000 ) ) ;
#20578 = AXIS2_PLACEMENT_3D ( 'NONE', #40598, #23928, #58378 ) ;
#20579 = DIRECTION ( 'NONE',  ( 0.5735764363510462704, 0.8191520442889915765, 0.000000000000000000 ) ) ;
#20580 = DIRECTION ( 'NONE',  ( 0.000000000000000000, -1.000000000000000000, 0.000000000000000000 ) ) ;
#20581 = CARTESIAN_POINT ( 'NONE',  ( -13.99719405338373512, -50.00026112179624960, 27.38482409491458114 ) ) ;
#20582 = CARTESIAN_POINT ( 'NONE',  ( 2.802461721337288658, 15.83563386295778308, -9.606080321247290499 ) ) ;
#20583 = CLOSED_SHELL ( 'NONE', ( #78647, #68065, #66973, #20774, #96092, #94732, #10316, #77159, #15527, #66649, #44605, #18564, #185, #93726, #20210, #6131, #24056, #49998, #65823, #36037, #87198, #35733, #65440, #12484, #101096, #10364, #104825, #16653, #99977, #76156, #55728, #11749, #59647, #26717, #82998, #85105, #22388, #27947, #44238, #51679, #60434, #45217, #90435, #100986, #105147, #13402, #17300, #84820, #38990, #44186, #44780, #30042, #15259, #60953, #12305, #98816, #18881, #98511, #59131, #67844, #38054, #21310, #8466, #41599, #14634, #35149, #104485, #13091, #1826, #56475, #57123, #59831, #1568, #19125, #49080, #13526, #42772, #58421, #89040, #29400, #85645, #68261, #2790, #7868, #92949, #76671, #31215, #39165, #97546, #15853, #88446, #55970, #95952, #85431, #58033, #100988, #87112, #86403, #60785, #27809 ) ) ;
#20584 = CARTESIAN_POINT ( 'NONE',  ( 67.59883368830136874, -59.99999999999988631, -35.88524404060949990 ) ) ;
#20585 = CARTESIAN_POINT ( 'NONE',  ( -37.39630343064651186, -60.00000000000003553, 52.44675545814470041 ) ) ;
#20586 = CARTESIAN_POINT ( 'NONE',  ( -55.73313709741204036, -29.08943728207367130, 57.64661559024293780 ) ) ;
#20587 = ORIENTED_EDGE ( 'NONE', *, *, #90249, .F. ) ;
#20588 = ORIENTED_EDGE ( 'NONE', *, *, #84003, .T. ) ;
#20589 = CARTESIAN_POINT ( 'NONE',  ( -99.91311621068668103, -45.25511269195838082, 192.6816207345183614 ) ) ;
#20590 = VECTOR ( 'NONE', #43886, 1000.000000000000341 ) ;
#20591 = CARTESIAN_POINT ( 'NONE',  ( 100.6609828699545091, -38.00000000000000711, 189.2800559844043846 ) ) ;
#20592 = CARTESIAN_POINT ( 'NONE',  ( -0.6440314167888865349, 52.10985070881105941, 7.915853150659584614 ) ) ;
#20593 = ORIENTED_EDGE ( 'NONE', *, *, #35206, .F. ) ;
#20594 = CARTESIAN_POINT ( 'NONE',  ( 19.48812817077294923, 49.99803169766527589, 60.15118601806505438 ) ) ;
#20595 = CARTESIAN_POINT ( 'NONE',  ( -14.10784364328131879, -60.00000000000002132, 39.74721978056663119 ) ) ;
#20596 = FACE_BOUND ( 'NONE', #88468, .T. ) ;
#20597 = CARTESIAN_POINT ( 'NONE',  ( -2.977408999572650039, -17.56250000204838813, -7.188101187500001821 ) ) ;
#20598 = CARTESIAN_POINT ( 'NONE',  ( -5.000000000000000000, -60.71953810597282342, 12.61250543006821978 ) ) ;
#20599 = CARTESIAN_POINT ( 'NONE',  ( 1.040949779275250140E-15, 0.000000000000000000, -8.500000000000000000 ) ) ;
#20600 = CARTESIAN_POINT ( 'NONE',  ( 7.551437640244095917, -81.99127537477087913, -2.648272645923386737 ) ) ;
#20601 = CARTESIAN_POINT ( 'NONE',  ( 60.99018172453023823, -30.00000000000000355, 69.41130770961356689 ) ) ;
#20602 = CARTESIAN_POINT ( 'NONE',  ( 35.59667163540026280, 463.9592197885497171, -0.04846191499040426731 ) ) ;
#20603 = CARTESIAN_POINT ( 'NONE',  ( -9.491976138786448303, 142.3932387565501472, 0.000000000000000000 ) ) ;
#20604 = CARTESIAN_POINT ( 'NONE',  ( 13.50000000000000355, -2.625659737069749422, -12.88678781509933380 ) ) ;
#20605 = CARTESIAN_POINT ( 'NONE',  ( -7.500000000000007105, 44.29449649216757479, -60.86453129175313137 ) ) ;
#20606 = CARTESIAN_POINT ( 'NONE',  ( -27.75390804783276621, -49.91462102057435146, 34.23205770176554097 ) ) ;
#20607 = CARTESIAN_POINT ( 'NONE',  ( 48.17782170722597357, -18.76230026711737509, 41.56796169131970231 ) ) ;
#20608 = CARTESIAN_POINT ( 'NONE',  ( -32.28930913497459443, 488.2717154064632723, 9.213726894912742438 ) ) ;
#20609 = CIRCLE ( 'NONE', #63597, 8.000000000000000000 ) ;
#20610 = CARTESIAN_POINT ( 'NONE',  ( -1.249701656895251700, 45.80093235429502840, 17.33947950171232577 ) ) ;
#20611 = EDGE_CURVE ( 'NONE', #8947, #25938, #69430, .T. ) ;
#20612 = CARTESIAN_POINT ( 'NONE',  ( -91.41481866688960167, -38.50420980943239613, 200.8848493538998525 ) ) ;
#20613 = VERTEX_POINT ( 'NONE', #31064 ) ;
#20614 = CARTESIAN_POINT ( 'NONE',  ( -16.10535093526667438, 21.79478144880857826, 1.090471457014209777 ) ) ;
#20615 = CARTESIAN_POINT ( 'NONE',  ( -18.92793431205891608, 49.05858063650561007, 62.10525169381176624 ) ) ;
#20616 = CARTESIAN_POINT ( 'NONE',  ( 6.654387246717901050, 41.27136532114669620, -70.82047233385743823 ) ) ;
#20617 = COLOUR_RGB ( '', 0.72549020, 0.75294118, 0.79215686) ;
#20618 = CARTESIAN_POINT ( 'NONE',  ( -33.97359119245064107, 434.1099241184709285, 11.80501937577160732 ) ) ;
#20619 =( LENGTH_UNIT ( ) NAMED_UNIT ( * ) SI_UNIT ( .MILLI., .METRE. ) );
#20620 = DIRECTION ( 'NONE',  ( 0.000000000000000000, 0.000000000000000000, 1.000000000000000000 ) ) ;
#20621 = CARTESIAN_POINT ( 'NONE',  ( 111.2626209470261784, -60.00000000000000000, 185.8948156968612864 ) ) ;
#20622 = CARTESIAN_POINT ( 'NONE',  ( -7.551437640244095917, -68.00872462522907824, -2.648272645923388513 ) ) ;
#20623 = VERTEX_POINT ( 'NONE', #62875 ) ;
#20624 = CARTESIAN_POINT ( 'NONE',  ( 7.150931910075640552, 31.78625798522262258, -3.588457848165356623 ) ) ;
#20625 = B_SPLINE_CURVE_WITH_KNOTS ( 'NONE', 3,
 ( #26231, #76317, #77396, #50438, #27297, #3510, #9995, #60699, #75794, #36451, #2429, #43437, #34842, #51514 ),
 .UNSPECIFIED., .F., .F.,
 ( 4, 2, 2, 2, 2, 2, 4 ),
 ( 0.000000000000000000, 0.0003608396711012821904, 0.0007216793422025643808, 0.001082519013303846409, 0.001443358684405128762, 0.002165038026607684143, 0.002886717368810240176 ),
 .UNSPECIFIED. ) ;
#20626 = VECTOR ( 'NONE', #12140, 1000.000000000000000 ) ;
#20627 = LINE ( 'NONE', #43774, #71115 ) ;
#20628 = ORIENTED_EDGE ( 'NONE', *, *, #98167, .F. ) ;
#20630 = CARTESIAN_POINT ( 'NONE',  ( 32.12958771267400948, 464.7275665249413237, 11.12424126545837133 ) ) ;
#20629 = SURFACE_STYLE_FILL_AREA ( #61579 ) ;
#20631 = CARTESIAN_POINT ( 'NONE',  ( 3.313708498984839323, -21.78124999999999645, 7.999999999999921840 ) ) ;
#20632 = CARTESIAN_POINT ( 'NONE',  ( -4.028951842967198438, -3.000000000000000444, 6.990291106834060741 ) ) ;
#20633 = CARTESIAN_POINT ( 'NONE',  ( 40.60713025163710910, 436.1947416310474637, 6.060763751012176570 ) ) ;
#20634 = CARTESIAN_POINT ( 'NONE',  ( -2.977408999572650039, -11.56250000204838635, -7.188101187500001821 ) ) ;
#20635 = CARTESIAN_POINT ( 'NONE',  ( -5.040301471719076609, -5.750234626350522404, -0.09933465333851672352 ) ) ;
#20636 = STYLED_ITEM ( 'NONE', ( #90594 ), #33641 ) ;
#20637 = CARTESIAN_POINT ( 'NONE',  ( 30.93388328643609242, 14.00942575955929748, -40.91282515498054551 ) ) ;
#20638 = AXIS2_PLACEMENT_3D ( 'NONE', #4884, #61011, #38335 ) ;
#20639 = EDGE_LOOP ( 'NONE', ( #60036, #26389, #48259, #6310 ) ) ;
#20640 = CARTESIAN_POINT ( 'NONE',  ( 82.71567603574061422, -42.97295659647987520, 172.7369150664174242 ) ) ;
#20641 = EDGE_CURVE ( 'NONE', #25026, #77058, #90351, .T. ) ;
#20642 = CARTESIAN_POINT ( 'NONE',  ( -46.00000000000000000, 462.6038693158056390, 6.978327855974978178 ) ) ;
#20643 = DIRECTION ( 'NONE',  ( 0.000000000000000000, 1.000000000000000000, -2.311253228826402606E-16 ) ) ;
#20644 = ORIENTED_EDGE ( 'NONE', *, *, #39021, .T. ) ;
#20645 = CARTESIAN_POINT ( 'NONE',  ( -29.60697198811803688, 307.3530822094822952, -8.981721099768231298 ) ) ;
#20646 = CARTESIAN_POINT ( 'NONE',  ( -46.95966155981771095, 18.79500983734985553, 14.95375697514023017 ) ) ;
#20647 = CARTESIAN_POINT ( 'NONE',  ( 0.5805565836007658964, 7.505553499465141165, -3.996997974842411264E-16 ) ) ;
#20648 = FACE_OUTER_BOUND ( 'NONE', #83077, .T. ) ;
#20649 = CARTESIAN_POINT ( 'NONE',  ( 6.999999999999998224, -12.54465221550629472, 8.223849511755000563 ) ) ;
#20650 =( BOUNDED_SURFACE ( )  B_SPLINE_SURFACE ( 2, 3, ( 
 ( #918, #98063, #24214, #57585, #57064, #55984, #82950, #8518 ),
 ( #9045, #73781, #74315, #89457, #74837, #33358, #88921, #15014 ),
 ( #6926, #39848, #15551, #72720, #105622, #31762, #64643, #97515 ) ),
 .UNSPECIFIED., .F., .F., .F. ) 
 B_SPLINE_SURFACE_WITH_KNOTS ( ( 3, 3 ),
 ( 4, 2, 2, 4 ),
 ( 0.000000000000000000, 1.000000000000000000 ),
 ( -0.06656819121499020497, -0.06329489543879425473, 0.001517242213116292218, 0.005444315861320835753 ),
 .UNSPECIFIED. ) 
 GEOMETRIC_REPRESENTATION_ITEM ( )  RATIONAL_B_SPLINE_SURFACE ( (
 ( 1.000000000000000000, 1.000000000000000000, 1.000000000000000000, 1.000000000000000000, 1.000000000000000000, 1.000000000000000000, 1.000000000000000000, 1.000000000000000000),
 ( 1.857142857142858317, 1.857142857142858317, 1.857142857142858317, 1.857142857142858317, 1.857142857142858317, 1.857142857142858317, 1.857142857142858317, 1.857142857142858317),
 ( 1.000000000000000000, 1.000000000000000000, 1.000000000000000000, 1.000000000000000000, 1.000000000000000000, 1.000000000000000000, 1.000000000000000000, 1.000000000000000000) ) ) 
 REPRESENTATION_ITEM ( '' )  SURFACE ( )  );
#20651 = CARTESIAN_POINT ( 'NONE',  ( 16.80337955834833252, 43.42153323332214399, 6.657797401561436068 ) ) ;
#20652 = ORIENTED_EDGE ( 'NONE', *, *, #98633, .T. ) ;
#20653 = AXIS2_PLACEMENT_3D ( 'NONE', #12870, #88382, #94889 ) ;
#20654 = DIRECTION ( 'NONE',  ( 0.000000000000000000, 0.000000000000000000, 1.000000000000000000 ) ) ;
#20655 = FACE_OUTER_BOUND ( 'NONE', #58458, .T. ) ;
#20656 = CARTESIAN_POINT ( 'NONE',  ( -0.4000000000000045186, 1.040949779275250140E-15, -8.500000000000000000 ) ) ;
#20658 = CARTESIAN_POINT ( 'NONE',  ( 9.833493305133805151, 1.593028355512270962E-15, 0.000000000000000000 ) ) ;
#20657 = CARTESIAN_POINT ( 'NONE',  ( -12.49955057333833253, -4.332870170146376765, -12.71907580221295220 ) ) ;
#20659 = VECTOR ( 'NONE', #28799, 1000.000000000000000 ) ;
#20660 = CARTESIAN_POINT ( 'NONE',  ( 7.188101187500001821, -23.56250000204838813, -2.977408999572650483 ) ) ;
#20661 = CARTESIAN_POINT ( 'NONE',  ( 15.42276584910590920, 294.5569213128695196, -2.062679874220467724 ) ) ;
#20662 = CARTESIAN_POINT ( 'NONE',  ( 0.000000000000000000, 45.50000000000000711, 59.50000000000000000 ) ) ;
#20663 = AXIS2_PLACEMENT_3D ( 'NONE', #55428, #52716, #92114 ) ;
#20664 = CARTESIAN_POINT ( 'NONE',  ( -28.28112556431591784, 36.39299121505979429, -8.375380894399709675 ) ) ;
#20665 = ORIENTED_EDGE ( 'NONE', *, *, #5265, .F. ) ;
#20666 = CARTESIAN_POINT ( 'NONE',  ( 2.435347819570957628E-07, -57.67120202539301488, -44.61186700419775519 ) ) ;
#20667 = CARTESIAN_POINT ( 'NONE',  ( 43.64534273044669277, 464.9151781295577734, 12.30378483073953966 ) ) ;
#20668 = CARTESIAN_POINT ( 'NONE',  ( -7.989277284024328019, 50.32447066042715988, 0.000000000000000000 ) ) ;
#20669 = CARTESIAN_POINT ( 'NONE',  ( 16.64348903516512834, 43.75610143575153899, -4.157797401561768247 ) ) ;
#20670 = ORIENTED_EDGE ( 'NONE', *, *, #33068, .F. ) ;
#20671 = CARTESIAN_POINT ( 'NONE',  ( 3.313708498984722972, -16.71874999999999289, -8.000000000000040856 ) ) ;
#20672 = CARTESIAN_POINT ( 'NONE',  ( 10.51296777078104050, 50.00000000000000000, -92.64705882352942012 ) ) ;
#20673 = EDGE_LOOP ( 'NONE', ( #96961, #9076, #46664, #98467, #76703 ) ) ;
#20674 = CIRCLE ( 'NONE', #99827, 8.000000000000000000 ) ;
#20675 = EDGE_CURVE ( 'NONE', #89440, #96838, #8326, .T. ) ;
#20676 = CARTESIAN_POINT ( 'NONE',  ( 44.78945892759311675, 1.340359594676612611E-15, 0.000000000000000000 ) ) ;
#20677 = CARTESIAN_POINT ( 'NONE',  ( -2.706785074969889848, -0.5477000579813379177, 103.4519997648587406 ) ) ;
#20678 = CARTESIAN_POINT ( 'NONE',  ( 9.165151389911679658, 105.0000000000000000, 4.000000000000001776 ) ) ;
#20679 = FACE_OUTER_BOUND ( 'NONE', #4672, .T. ) ;
#20680 = CARTESIAN_POINT ( 'NONE',  ( -97.74358396739806665, -60.00000000000000000, 202.3837098231268499 ) ) ;
#20681 = AXIS2_PLACEMENT_3D ( 'NONE', #67404, #51187, #101355 ) ;
#20682 = FILL_AREA_STYLE_COLOUR ( '', #103520 ) ;
#20683 = CARTESIAN_POINT ( 'NONE',  ( 5.290067270632161645, 53.47475093287481229, -8.531152949374595451 ) ) ;
#20684 = CARTESIAN_POINT ( 'NONE',  ( 16.75187969033515145, 34.99134772383131775, -21.80698433968624528 ) ) ;
#20685 = CARTESIAN_POINT ( 'NONE',  ( -85.08241398762224605, -32.28766595076764645, 178.2151489888117055 ) ) ;
#20686 = CARTESIAN_POINT ( 'NONE',  ( 43.91139751470105779, 41.39507865991506463, -50.13180910527601242 ) ) ;
#20687 = ADVANCED_FACE ( 'NONE', ( #66039 ), #81054, .F. ) ;
#20688 = ORIENTED_EDGE ( 'NONE', *, *, #42908, .T. ) ;
#20689 = CARTESIAN_POINT ( 'NONE',  ( 5.656854249492378806, -26.18749999999999645, 5.656854249492381470 ) ) ;
#20690 = EDGE_CURVE ( 'NONE', #34113, #18346, #53110, .T. ) ;
#20691 = CARTESIAN_POINT ( 'NONE',  ( 4.496882872040832702, -65.53788665489622645, 3.972797206970399397 ) ) ;
#20692 = CARTESIAN_POINT ( 'NONE',  ( -84.09493881211557209, -45.27002118742259995, 1.240083160534475759 ) ) ;
#20693 = PRESENTATION_LAYER_ASSIGNMENT (  '', '', ( #56804 ) ) ;
#20694 = CARTESIAN_POINT ( 'NONE',  ( -2.374770270502819969, -6.910312371743992266, -13.35351085777655733 ) ) ;
#20695 = DIRECTION ( 'NONE',  ( 0.000000000000000000, 0.000000000000000000, -1.000000000000000000 ) ) ;
#20696 = CARTESIAN_POINT ( 'NONE',  ( 9.239881048100823335, 139.9679065713421267, -5.000000000000000888 ) ) ;
#20697 =( NAMED_UNIT ( * ) SI_UNIT ( $, .STERADIAN. ) SOLID_ANGLE_UNIT ( ) );
#20698 = CARTESIAN_POINT ( 'NONE',  ( -10.04205104288555184, 18.64316884714294886, -37.36680950593608230 ) ) ;
#20699 = CARTESIAN_POINT ( 'NONE',  ( 81.96363334812492951, -30.00000000000004263, 194.6668941393791386 ) ) ;
#20700 = AXIS2_PLACEMENT_3D ( 'NONE', #91583, #34439, #41949 ) ;
#20701 = CARTESIAN_POINT ( 'NONE',  ( -13.99999999999998046, 61.49999999999999289, -6.999999999999992895 ) ) ;
#20702 = CARTESIAN_POINT ( 'NONE',  ( -92.19364677446148448, -60.00000000000002842, -19.86446420722052153 ) ) ;
#20703 = CARTESIAN_POINT ( 'NONE',  ( -64.03236696410434092, -39.48531855383056666, 83.36438480388000016 ) ) ;
#20704 = ORIENTED_EDGE ( 'NONE', *, *, #94830, .F. ) ;
#20705 = CARTESIAN_POINT ( 'NONE',  ( 84.52829458723479661, -59.99999999999986500, 202.7046071135156069 ) ) ;
#20706 = CARTESIAN_POINT ( 'NONE',  ( -23.30905507870230053, 39.42442235840471909, 60.74964960281029391 ) ) ;
#20707 = CARTESIAN_POINT ( 'NONE',  ( 39.07151204532090105, -57.67118256652997843, -41.76327104003939183 ) ) ;
#20708 = ORIENTED_EDGE ( 'NONE', *, *, #4616, .T. ) ;
#20709 = CARTESIAN_POINT ( 'NONE',  ( -4.000000000000000000, 0.000000000000000000, -4.567799999999999194 ) ) ;
#20710 = CARTESIAN_POINT ( 'NONE',  ( 4.401442555609581635E-16, -28.15625000204838813, -7.188101187500000044 ) ) ;
#20711 = AXIS2_PLACEMENT_3D ( 'NONE', #49983, #98532, #34909 ) ;
#20712 = CARTESIAN_POINT ( 'NONE',  ( -5.727189096784631950, -6.421301247512601229, -1.806430436190350486 ) ) ;
#20713 = EDGE_LOOP ( 'NONE', ( #17155, #85108, #30282, #28837 ) ) ;
#20714 = ORIENTED_EDGE ( 'NONE', *, *, #48991, .F. ) ;
#20715 = DIRECTION ( 'NONE',  ( -1.000000000000000000, -1.224606353822377258E-16, -0.000000000000000000 ) ) ;
#20716 = CARTESIAN_POINT ( 'NONE',  ( -39.13466327772848530, 485.8437493838396790, -4.960055907049729207 ) ) ;
#20717 = CARTESIAN_POINT ( 'NONE',  ( -90.66602546307569810, -59.99999999999997868, -17.63937689681369392 ) ) ;
#20718 = CARTESIAN_POINT ( 'NONE',  ( 9.113097280746998763, -54.26300649141423804, 31.11721482942554928 ) ) ;
#20719 = CARTESIAN_POINT ( 'NONE',  ( 2.977408999572651815, -33.31250000204838813, 7.188101187500000933 ) ) ;
#20720 = LINE ( 'NONE', #4475, #80861 ) ;
#20721 = CARTESIAN_POINT ( 'NONE',  ( -44.12472801210821416, 485.7238370326489871, 3.975897585127424527 ) ) ;
#20722 = CARTESIAN_POINT ( 'NONE',  ( 3.702395615612342095, -48.95046109946132162, 103.3251893371222394 ) ) ;
#20723 = CIRCLE ( 'NONE', #12025, 1.000000000000000888 ) ;
#20724 = CARTESIAN_POINT ( 'NONE',  ( -11.68767211932355465, 50.00000000000000000, -88.14097461399492772 ) ) ;
#20725 = DIRECTION ( 'NONE',  ( -1.000000000000000000, 0.000000000000000000, 0.000000000000000000 ) ) ;
#20726 = CARTESIAN_POINT ( 'NONE',  ( 40.02090011478166076, 436.4865077410170784, 5.635628130754340326 ) ) ;
#20727 = VERTEX_POINT ( 'NONE', #51970 ) ;
#20728 = DIRECTION ( 'NONE',  ( -1.000000000000000000, -0.000000000000000000, -0.000000000000000000 ) ) ;
#20729 = CARTESIAN_POINT ( 'NONE',  ( 4.680975426248725313, -2.415770170678304130, 103.4780497728483226 ) ) ;
#20731 = CARTESIAN_POINT ( 'NONE',  ( 37.69778303256208574, -53.35051267955863352, 39.83820104574851939 ) ) ;
#20730 = CARTESIAN_POINT ( 'NONE',  ( -3.564365538407123779, -48.86493411501031403, 104.5953911288849412 ) ) ;
#20732 = DIRECTION ( 'NONE',  ( -1.000000000000000000, -1.224606353822377258E-16, -0.000000000000000000 ) ) ;
#20733 = EDGE_LOOP ( 'NONE', ( #58490, #2048 ) ) ;
#20734 = CARTESIAN_POINT ( 'NONE',  ( -21.97738170171518490, 25.77581552988312552, -32.31595285212490865 ) ) ;
#20735 = EDGE_CURVE ( 'NONE', #22409, #78525, #28824, .T. ) ;
#20736 = VECTOR ( 'NONE', #35147, 1000.000000000000000 ) ;
#20738 = CARTESIAN_POINT ( 'NONE',  ( 7.036764705882352366, 40.00000000373363207, -71.06385277390853616 ) ) ;
#20737 = CARTESIAN_POINT ( 'NONE',  ( -27.10511071441192144, 34.47735702144345282, -10.05698433968589178 ) ) ;
#20739 = CYLINDRICAL_SURFACE ( 'NONE', #64665, 1.999999999999998224 ) ;
#20740 = PRESENTATION_STYLE_ASSIGNMENT (( #78907 ) ) ;
#20741 = CARTESIAN_POINT ( 'NONE',  ( -41.61741820144500537, 435.6127172585689777, 7.033059668058291969 ) ) ;
#20742 = CARTESIAN_POINT ( 'NONE',  ( -48.80488232270442239, 14.82891652079445599, -14.61828285348522449 ) ) ;
#20743 = EDGE_LOOP ( 'NONE', ( #9197, #72086 ) ) ;
#20744 = AXIS2_PLACEMENT_3D ( 'NONE', #40655, #51252, #100878 ) ;
#20745 = CARTESIAN_POINT ( 'NONE',  ( 92.54596869004491566, -60.00000000000000711, -1.929604771320055701 ) ) ;
#20746 = LINE ( 'NONE', #18586, #46425 ) ;
#20747 = SURFACE_SIDE_STYLE ('',( #10978 ) ) ;
#20748 = CARTESIAN_POINT ( 'NONE',  ( -6.122245915141247607, 40.00000000007563727, -71.16543060730309378 ) ) ;
#20749 = CARTESIAN_POINT ( 'NONE',  ( -11.89526586238883432, 16.74536500488340351, -9.279214822536506091 ) ) ;
#20750 = ADVANCED_FACE ( 'NONE', ( #77858 ), #95134, .T. ) ;
#20751 = ORIENTED_EDGE ( 'NONE', *, *, #69354, .T. ) ;
#20752 = B_SPLINE_CURVE_WITH_KNOTS ( 'NONE', 3,
 ( #90095, #16198, #97638, #32949 ),
 .UNSPECIFIED., .F., .F.,
 ( 4, 4 ),
 ( 0.000000000000000000, 0.0002045283294089406535 ),
 .UNSPECIFIED. ) ;
#20753 = CARTESIAN_POINT ( 'NONE',  ( -91.34471721603175354, -30.00000000002426148, 199.5624097827029573 ) ) ;
#20754 = ORIENTED_EDGE ( 'NONE', *, *, #8414, .T. ) ;
#20755 = LINE ( 'NONE', #78394, #66092 ) ;
#20756 = CARTESIAN_POINT ( 'NONE',  ( 14.60001457338170461, 22.21450448812595013, 3.985393713008906325 ) ) ;
#20757 = FILL_AREA_STYLE ('',( #12588 ) ) ;
#20758 = CARTESIAN_POINT ( 'NONE',  ( 5.082755093536325930, -34.34375000204838813, -5.082755093536325042 ) ) ;
#20759 = AXIS2_PLACEMENT_3D ( 'NONE', #63327, #55198, #88126 ) ;
#20760 = CARTESIAN_POINT ( 'NONE',  ( -17.59874102159060527, 44.99999999999999289, 63.10646976788801510 ) ) ;
#20761 = CARTESIAN_POINT ( 'NONE',  ( 9.032223969890491588, 46.05502784614110823, -14.03066199895145161 ) ) ;
#20762 = CARTESIAN_POINT ( 'NONE',  ( 31.84798808520906022, 480.8473942020407321, 11.59524609927768957 ) ) ;
#20763 = ORIENTED_EDGE ( 'NONE', *, *, #55871, .T. ) ;
#20764 = FACE_OUTER_BOUND ( 'NONE', #17438, .T. ) ;
#20766 = ORIENTED_EDGE ( 'NONE', *, *, #41092, .F. ) ;
#20765 = DIRECTION ( 'NONE',  ( -1.000000000000000000, -0.000000000000000000, -0.000000000000000000 ) ) ;
#20767 = CARTESIAN_POINT ( 'NONE',  ( 79.67959528545318904, -36.02748385560343536, 140.1370599864249584 ) ) ;
#20768 = EDGE_CURVE ( 'NONE', #60654, #44784, #89953, .T. ) ;
#20769 = B_SPLINE_CURVE_WITH_KNOTS ( 'NONE', 3,
 ( #50279, #32542, #57828, #8760, #83183, #98308, #42191, #24461, #82657, #57297, #41140, #74024, #90754, #33073, #41663, #69151, #69667, #102018, #53985, #76682, #68068, #2793, #11944, #60531, #78278, #85319, #2247, #20101, #70193, #35197, #44873, #86405, #77760, #45401 ),
 .UNSPECIFIED., .F., .F.,
 ( 4, 2, 2, 2, 2, 2, 2, 2, 2, 2, 2, 2, 2, 2, 2, 2, 4 ),
 ( 0.01263889472610567853, 0.01342810546992895433, 0.01421731621375223013, 0.01500652695757550420, 0.01579573770139878000, 0.01658494844522205580, 0.01737415918904533160, 0.01816336993286860740, 0.01895258067669188320, 0.01974179142051515901, 0.02053100216433843481, 0.02132021290816171061, 0.02210942365198498294, 0.02289863439580826221, 0.02368784513963153801, 0.02447705588345481381, 0.02526626662727808961 ),
 .UNSPECIFIED. ) ;
#20770 = VERTEX_POINT ( 'NONE', #12572 ) ;
#20771 = CARTESIAN_POINT ( 'NONE',  ( 0.9263455752254985409, -50.01477469915685248, 40.97011183254556954 ) ) ;
#20772 = CARTESIAN_POINT ( 'NONE',  ( 5.082755093536325930, -20.46875000204838813, -5.082755093536325042 ) ) ;
#20773 = CARTESIAN_POINT ( 'NONE',  ( -77.81697554521740301, -57.51284286114859157, 196.3444844341304929 ) ) ;
#20774 = ADVANCED_FACE ( 'NONE', ( #44433 ), #38391, .T. ) ;
#20775 = ORIENTED_EDGE ( 'NONE', *, *, #37179, .T. ) ;
#20776 = AXIS2_PLACEMENT_3D ( 'NONE', #57514, #48888, #90977 ) ;
#20777 = CARTESIAN_POINT ( 'NONE',  ( -5.980543423763065469, -13.97096407501078374, -0.5500789318242844672 ) ) ;
#20778 = EDGE_CURVE ( 'NONE', #4517, #99732, #84358, .T. ) ;
#20779 = AXIS2_PLACEMENT_3D ( 'NONE', #20268, #9989, #42891 ) ;
#20780 = CARTESIAN_POINT ( 'NONE',  ( 7.182275720338873626, 41.30104542284085767, -58.77094221306448674 ) ) ;
#20781 = FACE_OUTER_BOUND ( 'NONE', #58274, .T. ) ;
#20782 = CARTESIAN_POINT ( 'NONE',  ( 7.999999999999998224, -15.78125000409677092, 3.313708498984766493 ) ) ;
#20783 = CARTESIAN_POINT ( 'NONE',  ( -39.92758536453102636, -26.29482751352448133, 35.91463579594280731 ) ) ;
#20784 = CARTESIAN_POINT ( 'NONE',  ( 9.606080321247342013, 15.83563386295778308, 2.802461721337131451 ) ) ;
#20785 = CARTESIAN_POINT ( 'NONE',  ( 42.19179521601841287, 485.4956273777429487, -3.824025998174274577 ) ) ;
#20786 = CARTESIAN_POINT ( 'NONE',  ( 5.268008033849937100, 13.26688624804745587, -33.14867888032319598 ) ) ;
#20787 = B_SPLINE_CURVE_WITH_KNOTS ( 'NONE', 3,
 ( #60506, #62100, #77734, #12442, #69641, #21129, #102534, #94992, #20615, #45892, #12968, #11916, #86376, #4364, #93391, #2761, #69120, #53958, #3305, #51845, #78770, #45369, #78251, #37835, #100929, #85285, #68590, #27090, #35712, #43758, #85842, #59976, #76650, #52374, #11373, #44300, #77194, #101993, #28151, #61027, #93914, #20070, #52918, #44845, #30795, #104643, #5938, #7003, #55014, #96039, #103590, #79833, #97080, #87946, #38354, #39923, #6469, #49993, #96568, #17117, #31842, #13499, #22703, #87425, #55540, #31328, #46422 ),
 .UNSPECIFIED., .F., .F.,
 ( 4, 2, 2, 2, 2, 1, 2, 2, 2, 2, 2, 2, 1, 1, 2, 2, 2, 2, 1, 2, 2, 2, 2, 1, 1, 2, 2, 2, 2, 1, 1, 1, 2, 2, 2, 2, 2, 4 ),
 ( 0.000000000000000000, 0.06249999999989476474, 0.1249999999997895295, 0.1874999999996843081, 0.2187499999996354583, 0.2343749999996066202, 0.2421874999995970723, 0.2499999999995875521, 0.3124999999995375921, 0.3437499999995161093, 0.3749999999994946265, 0.4374999999994517164, 0.4687499999994302335, 0.4843749999994252375, 0.4921874999994257927, 0.4999999999994263478, 0.5624999999994299005, 0.5937499999994316768, 0.6093749999994333422, 0.6171874999994354516, 0.6249999999994374500, 0.6874999999994867439, 0.7187499999995128341, 0.7343749999995256017, 0.7421874999995317079, 0.7460937499995344835, 0.7499999999995371480, 0.8124999999995893285, 0.8437499999996155298, 0.8593749999996311839, 0.8671874999996388445, 0.8710937499996425082, 0.8730468749996473932, 0.8749999999996523892, 0.9062499999997443156, 0.9218749999997882805, 0.9374999999998322453, 1.000000000000000000 ),
 .UNSPECIFIED. ) ;
#20788 = CARTESIAN_POINT ( 'NONE',  ( 4.206664532338635354, 51.73451848529560237, 7.924518144939897368 ) ) ;
#20790 = EDGE_CURVE ( 'NONE', #81895, #4237, #76252, .T. ) ;
#20789 = CARTESIAN_POINT ( 'NONE',  ( 51.88291765283150880, 324.6183258647171215, 367.1969486012847028 ) ) ;
#20791 = CARTESIAN_POINT ( 'NONE',  ( 4.933445413641555533, -30.00000000000000355, -5.637643499260712510 ) ) ;
#20792 = VERTEX_POINT ( 'NONE', #92972 ) ;
#20793 = CIRCLE ( 'NONE', #93109, 4.000000000000000888 ) ;
#20794 = CARTESIAN_POINT ( 'NONE',  ( 11.11385657980845032, -4.981498555758606450, -12.57747955902696546 ) ) ;
#20795 = DIRECTION ( 'NONE',  ( 0.000000000000000000, 1.000000000000000000, 0.000000000000000000 ) ) ;
#20796 = VECTOR ( 'NONE', #76126, 1000.000000000000000 ) ;
#20797 = CARTESIAN_POINT ( 'NONE',  ( -44.53895079744618357, -26.18090992505588943, -29.32626096537978100 ) ) ;
#20798 = CARTESIAN_POINT ( 'NONE',  ( -70.04522862247988257, -30.00000000000000711, 95.47013614611103094 ) ) ;
#20799 = CYLINDRICAL_SURFACE ( 'NONE', #37740, 5.000000000000000888 ) ;
#20800 = ORIENTED_EDGE ( 'NONE', *, *, #28665, .T. ) ;
#20801 = AXIS2_PLACEMENT_3D ( 'NONE', #62011, #39320, #87336 ) ;
#20802 = CARTESIAN_POINT ( 'NONE',  ( 3.490407211888509836E-12, -4.332980043422162808, 17.83347932686506354 ) ) ;
#20803 = CARTESIAN_POINT ( 'NONE',  ( 79.53896493954057689, -57.50597618960500057, 198.4139380564783437 ) ) ;
#20804 = CARTESIAN_POINT ( 'NONE',  ( 46.00000000000000000, 438.3878896346934653, 16.22878885428544038 ) ) ;
#20806 = FACE_OUTER_BOUND ( 'NONE', #67906, .T. ) ;
#20805 = VECTOR ( 'NONE', #91605, 1000.000000000000341 ) ;
#20807 = CARTESIAN_POINT ( 'NONE',  ( -14.45674127754199390, 21.77180424838195094, -4.838420908141329413 ) ) ;
#20808 = CARTESIAN_POINT ( 'NONE',  ( 0.000000000000000000, 0.000000000000000000, -1.875285714285714445 ) ) ;
#20809 = CARTESIAN_POINT ( 'NONE',  ( -61.33683733235092461, -59.99999999999999289, 104.9969710539504746 ) ) ;
#20810 = FACE_OUTER_BOUND ( 'NONE', #23587, .T. ) ;
#20811 = CARTESIAN_POINT ( 'NONE',  ( 6.249999999999998224, 9.237604307034018802, 0.000000000000000000 ) ) ;
#20812 = CIRCLE ( 'NONE', #19100, 4.000000000000007105 ) ;
#20813 = CARTESIAN_POINT ( 'NONE',  ( -43.69716417793774355, 49.99999999999999289, 48.48761666241306756 ) ) ;
#20814 = CARTESIAN_POINT ( 'NONE',  ( -86.30461461627585606, -24.61979355009274073, 182.2308408382141351 ) ) ;
#20815 = ORIENTED_EDGE ( 'NONE', *, *, #15666, .F. ) ;
#20816 = CARTESIAN_POINT ( 'NONE',  ( 35.73709257329849720, 382.3453677267265221, 5.045156307748890789 ) ) ;
#20817 = DIRECTION ( 'NONE',  ( -1.224646799147351482E-16, 0.000000000000000000, -1.000000000000000000 ) ) ;
#20818 = CARTESIAN_POINT ( 'NONE',  ( -5.916007711650134837, 41.94280317611644193, -59.21688531701510527 ) ) ;
#20819 = CARTESIAN_POINT ( 'NONE',  ( 46.36650669486618881, 1.474610560812782335E-15, 0.000000000000000000 ) ) ;
#20820 = EDGE_CURVE ( 'NONE', #85235, #106160, #67257, .T. ) ;
#20821 = CARTESIAN_POINT ( 'NONE',  ( -32.23979701228631001, 314.7547567211047976, -7.398542135358657568 ) ) ;
#20822 = B_SPLINE_CURVE_WITH_KNOTS ( 'NONE', 3,
 ( #5555, #79444, #8064, #57666, #40976, #4501, #48518, #57141, #89535, #16158, #97595, #7520, #21778, #90589, #87555, #40438, #13103, #38482, #73318, #54091, #72792, #46032, #46552, #105697 ),
 .UNSPECIFIED., .F., .F.,
 ( 4, 2, 2, 2, 2, 2, 2, 2, 2, 2, 2, 4 ),
 ( 0.003189860231642088848, 0.003693490673305733444, 0.004197121114969377606, 0.004448936335801199904, 0.004700751556633022202, 0.004952566777464845367, 0.005204381998296666798, 0.005708012439960319200, 0.005959827660792142365, 0.006211642881623965530, 0.006715273323287604922, 0.007218903764951243446 ),
 .UNSPECIFIED. ) ;
#20823 = CARTESIAN_POINT ( 'NONE',  ( 40.46549058525986453, 490.2743938847165737, 11.42162415461235447 ) ) ;
#20824 = DIRECTION ( 'NONE',  ( 1.000000000000000000, 0.000000000000000000, 0.000000000000000000 ) ) ;
#20825 = DIRECTION ( 'NONE',  ( 0.000000000000000000, -1.000000000000000000, 0.000000000000000000 ) ) ;
#20826 = ORIENTED_EDGE ( 'NONE', *, *, #53764, .F. ) ;
#20827 = CIRCLE ( 'NONE', #34667, 4.000000000000000888 ) ;
#20828 = CARTESIAN_POINT ( 'NONE',  ( 18.82063668069593376, 49.99999999999999289, 60.82877375281272236 ) ) ;
#20829 = EDGE_CURVE ( 'NONE', #77688, #16424, #3958, .T. ) ;
#20830 = CARTESIAN_POINT ( 'NONE',  ( 34.83349330513380693, 1.593028355512270962E-15, 0.000000000000000000 ) ) ;
#20831 = CARTESIAN_POINT ( 'NONE',  ( 25.22241582816893413, -4.285714285714286476, 3.301606509414615420 ) ) ;
#20832 = CARTESIAN_POINT ( 'NONE',  ( 9.554917598412142610, 53.41952622708690512, -3.541854172211333918 ) ) ;
#20833 = CARTESIAN_POINT ( 'NONE',  ( 98.75715858346298148, -14.21045842199428222, 105.0403869495405331 ) ) ;
#20834 =( GEOMETRIC_REPRESENTATION_CONTEXT ( 3 ) GLOBAL_UNCERTAINTY_ASSIGNED_CONTEXT ( ( #62844 ) ) GLOBAL_UNIT_ASSIGNED_CONTEXT ( ( #21511, #11782, #85154 ) ) REPRESENTATION_CONTEXT ( 'NONE', 'WORKASPACE' ) );
#20835 = CARTESIAN_POINT ( 'NONE',  ( -79.23476292317855041, -46.43852501042891134, 148.5225104870177688 ) ) ;
#20836 = VERTEX_POINT ( 'NONE', #88082 ) ;
#20837 = CARTESIAN_POINT ( 'NONE',  ( 24.34999999999999787, 1.533819458162526451E-15, 0.000000000000000000 ) ) ;
#20838 = CARTESIAN_POINT ( 'NONE',  ( 4.589357672516666931, 251.0620603097723063, -3.865585121226750243 ) ) ;
#20839 = SURFACE_STYLE_FILL_AREA ( #37533 ) ;
#20840 = CARTESIAN_POINT ( 'NONE',  ( 41.05732475771431211, 50.00000000000000711, 48.04410276558757431 ) ) ;
#20841 = CARTESIAN_POINT ( 'NONE',  ( 37.50518029089035821, 362.5804478665973534, 3.197089636230608267 ) ) ;
#20842 = CARTESIAN_POINT ( 'NONE',  ( 43.63213036654197197, 464.4895599185542210, 9.038982508271296012 ) ) ;
#20843 = ORIENTED_EDGE ( 'NONE', *, *, #44168, .T. ) ;
#20844 = CARTESIAN_POINT ( 'NONE',  ( 4.044483942431806867, 54.03592768539738955, -7.472348141917804831 ) ) ;
#20845 = CARTESIAN_POINT ( 'NONE',  ( 31.67687266298273130, 439.4050284403294881, 23.39876501491971439 ) ) ;
#20846 = CARTESIAN_POINT ( 'NONE',  ( -2.977408999572650039, -26.18750000204838813, -7.188101187500001821 ) ) ;
#20847 = CARTESIAN_POINT ( 'NONE',  ( 5.656854249492378806, -20.37500000409677270, 5.656854249492381470 ) ) ;
#20848 = CARTESIAN_POINT ( 'NONE',  ( 4.898587196589412829E-16, -24.12499999999999289, -8.000000000000000000 ) ) ;
#20849 = CARTESIAN_POINT ( 'NONE',  ( 6.639655237817898126, 41.83126053442604331, -69.93930111382492498 ) ) ;
#20850 = ADVANCED_FACE ( 'NONE', ( #39536 ), #88605, .F. ) ;
#20851 = CARTESIAN_POINT ( 'NONE',  ( 0.000000000000000000, -6.928203230275509661, -3.999999999999999112 ) ) ;
#20852 = CARTESIAN_POINT ( 'NONE',  ( -8.000000000000000000, -17.84374999999999645, -3.313708498984762496 ) ) ;
#20853 = AXIS2_PLACEMENT_3D ( 'NONE', #4889, #62600, #30782 ) ;
#20854 = CARTESIAN_POINT ( 'NONE',  ( -30.00000000000000000, 0.000000000000000000, 0.000000000000000000 ) ) ;
#20855 = ORIENTED_EDGE ( 'NONE', *, *, #55828, .F. ) ;
#20856 = VECTOR ( 'NONE', #63939, 1000.000000000000000 ) ;
#20857 = CARTESIAN_POINT ( 'NONE',  ( 92.65361671693909784, -60.00000000000000000, -3.623317284051360776 ) ) ;
#20859 = CARTESIAN_POINT ( 'NONE',  ( 28.17714236523514515, -60.33865966952142657, 36.15954811534652436 ) ) ;
#20858 = CARTESIAN_POINT ( 'NONE',  ( -70.80424915565322408, -29.99999999999997513, 131.6008933728038528 ) ) ;
#20860 = CARTESIAN_POINT ( 'NONE',  ( -2.399209547574901823E-15, 57.18445727710329862, 19.59103268995865221 ) ) ;
#20861 = ORIENTED_EDGE ( 'NONE', *, *, #86571, .T. ) ;
#20862 = ADVANCED_FACE ( 'NONE', ( #22306 ), #55152, .T. ) ;
#20863 = ORIENTED_EDGE ( 'NONE', *, *, #25458, .T. ) ;
#20864 = PRESENTATION_LAYER_ASSIGNMENT (  '', '', ( #79541 ) ) ;
#20865 = CARTESIAN_POINT ( 'NONE',  ( 35.23463026195637582, 462.2854383349875320, 4.568931904893218210 ) ) ;
#20866 = CARTESIAN_POINT ( 'NONE',  ( -5.371950044183563477, -47.79483119409569269, 104.0625755208173331 ) ) ;
#20867 = CARTESIAN_POINT ( 'NONE',  ( -13.45079846400083312, -54.00000000000000711, 23.11721482942554928 ) ) ;
#20868 = CARTESIAN_POINT ( 'NONE',  ( -1.103634289736943552, 51.47986102780117079, -9.608635276217455612 ) ) ;
#20869 = CARTESIAN_POINT ( 'NONE',  ( 6.289692432696983637, 6.589071317541204564, 2.245373559999253033 ) ) ;
#20870 = SURFACE_SIDE_STYLE ('',( #69897 ) ) ;
#20871 = VERTEX_POINT ( 'NONE', #96177 ) ;
#20872 = CARTESIAN_POINT ( 'NONE',  ( 98.00245574399852444, -30.00000000000002132, 190.5288581759436966 ) ) ;
#20873 = CARTESIAN_POINT ( 'NONE',  ( 25.89378858170335462, 41.47439130909162941, -71.76338141261258841 ) ) ;
#20875 = CARTESIAN_POINT ( 'NONE',  ( 3.484756791224362438, 15.95824666716552365, 9.380169522195147991 ) ) ;
#20874 = AXIS2_PLACEMENT_3D ( 'NONE', #102271, #12719, #21915 ) ;
#20876 = CARTESIAN_POINT ( 'NONE',  ( 81.57104778221477659, -29.99999999999999645, -8.220818473322141884 ) ) ;
#20877 = VECTOR ( 'NONE', #105972, 1000.000000000000000 ) ;
#20878 = DIRECTION ( 'NONE',  ( 0.000000000000000000, -1.000000000000000000, 0.000000000000000000 ) ) ;
#20879 = EDGE_CURVE ( 'NONE', #17391, #97138, #78677, .T. ) ;
#20880 = ORIENTED_EDGE ( 'NONE', *, *, #28939, .T. ) ;
#20881 = VECTOR ( 'NONE', #88004, 1000.000000000000000 ) ;
#20882 = ORIENTED_EDGE ( 'NONE', *, *, #82735, .T. ) ;
#20883 = EDGE_LOOP ( 'NONE', ( #42773, #102989, #31084, #47960, #76600 ) ) ;
#20884 = DIRECTION ( 'NONE',  ( -1.000000000000000000, 0.000000000000000000, 0.000000000000000000 ) ) ;
#20885 = LINE ( 'NONE', #88221, #79478 ) ;
#20887 = STYLED_ITEM ( 'NONE', ( #65203 ), #19142 ) ;
#20886 = DIRECTION ( 'NONE',  ( -1.000000000000000000, 0.000000000000000000, 0.000000000000000000 ) ) ;
#20888 = CARTESIAN_POINT ( 'NONE',  ( -1.348501488157294759, -70.09340828808477397, 13.06360208188350214 ) ) ;
#20889 = DIRECTION ( 'NONE',  ( 0.000000000000000000, -1.000000000000000000, 0.000000000000000000 ) ) ;
#20890 = LINE ( 'NONE', #53724, #41434 ) ;
#20891 = ORIENTED_EDGE ( 'NONE', *, *, #102686, .T. ) ;
#20892 = CARTESIAN_POINT ( 'NONE',  ( -6.145467200826166376, 48.00000000000000000, -92.99666842290478996 ) ) ;
#20893 = AXIS2_PLACEMENT_3D ( 'NONE', #102558, #61587, #94483 ) ;
#20894 = VERTEX_POINT ( 'NONE', #7139 ) ;
#20895 = CARTESIAN_POINT ( 'NONE',  ( -0.3498606326581789605, 15.11603512203452837, -10.00000000000000000 ) ) ;
#20896 = CARTESIAN_POINT ( 'NONE',  ( 55.14648603844897679, -38.34252558323068882, 81.89861063354169346 ) ) ;
#20897 = CARTESIAN_POINT ( 'NONE',  ( -41.66301127302475749, 485.3863426732057746, -3.409513628938614982 ) ) ;
#20898 = CARTESIAN_POINT ( 'NONE',  ( 28.51814700840726857, 297.3184951835715424, 10.47819064956899204 ) ) ;
#20899 = CARTESIAN_POINT ( 'NONE',  ( 4.925903578703449526, 301.1861660590338943, -10.01402232597611608 ) ) ;
#20900 = CARTESIAN_POINT ( 'NONE',  ( 63.04335118806904603, -60.33862346574463231, 91.29151592764401357 ) ) ;
#20901 = ORIENTED_EDGE ( 'NONE', *, *, #54618, .T. ) ;
#20902 = CARTESIAN_POINT ( 'NONE',  ( 0.000000000000000000, -3.035766082959412415E-15, 0.000000000000000000 ) ) ;
#20903 = CARTESIAN_POINT ( 'NONE',  ( -49.70730529349785343, -35.51104931314910829, -36.21594116302647137 ) ) ;
#20904 = CARTESIAN_POINT ( 'NONE',  ( -5.887945094627411002, 11.68790215641263686, -3.787642776067695394 ) ) ;
#20905 = DIRECTION ( 'NONE',  ( 0.000000000000000000, 0.000000000000000000, 1.000000000000000000 ) ) ;
#20906 = ADVANCED_FACE ( 'NONE', ( #31978 ), #5553, .T. ) ;
#20907 = VERTEX_POINT ( 'NONE', #21774 ) ;
#20908 = AXIS2_PLACEMENT_3D ( 'NONE', #85357, #50838, #74592 ) ;
#20909 = FILL_AREA_STYLE ('',( #28443 ) ) ;
#20910 = CARTESIAN_POINT ( 'NONE',  ( -5.724587470723463412E-14, -15.58845726811991561, -1.205771365940065953 ) ) ;
#20911 = DIRECTION ( 'NONE',  ( 2.742080092235280244E-17, 0.000000000000000000, -1.000000000000000000 ) ) ;
#20912 = AXIS2_PLACEMENT_3D ( 'NONE', #81127, #98893, #15871 ) ;
#20913 = EDGE_CURVE ( 'NONE', #85839, #8913, #13100, .T. ) ;
#20914 = CYLINDRICAL_SURFACE ( 'NONE', #82262, 4.000000000000000000 ) ;
#20915 = CARTESIAN_POINT ( 'NONE',  ( 5.656854249492380582, -33.50000000409677625, -5.656854249492379694 ) ) ;
#20916 = CARTESIAN_POINT ( 'NONE',  ( 68.45015997180047407, -4.000000000000000000, 4.898587196589421703E-16 ) ) ;
#20917 = CARTESIAN_POINT ( 'NONE',  ( 86.36492701509820336, -20.96249612347034486, 181.2249750320262365 ) ) ;
#20918 = CARTESIAN_POINT ( 'NONE',  ( -5.363597346089342466, 41.33266196706077267, -58.39526881795508473 ) ) ;
#20919 = CARTESIAN_POINT ( 'NONE',  ( -9.998846395913654206, 7.501654003228592771, 5.000000000000001776 ) ) ;
#20920 = EDGE_CURVE ( 'NONE', #99126, #75857, #22916, .T. ) ;
#20921 = EDGE_CURVE ( 'NONE', #61384, #103962, #48665, .T. ) ;
#20922 = FILL_AREA_STYLE_COLOUR ( '', #16024 ) ;
#20923 = CARTESIAN_POINT ( 'NONE',  ( 13.72588371288480857, -50.98893574582776722, 29.76328409196439750 ) ) ;
#20924 = CARTESIAN_POINT ( 'NONE',  ( 33.26935678862407997, 435.1895192765533693, 10.58170431744235884 ) ) ;
#20925 = CARTESIAN_POINT ( 'NONE',  ( -100.7640968642291028, -30.00000000000000000, 180.6473348120972275 ) ) ;
#20926 = CONICAL_SURFACE ( 'NONE', #22597, 4.172000000000001485, 0.9599310885968750373 ) ;
#20927 = CARTESIAN_POINT ( 'NONE',  ( 7.592810154713590230E-15, 1.500000000000000000, -62.00000000000000000 ) ) ;
#20928 = CARTESIAN_POINT ( 'NONE',  ( 0.1301286458300882076, -57.67120203291111125, 41.61185487318789455 ) ) ;
#20930 = CARTESIAN_POINT ( 'NONE',  ( 3.587928128302542596, 304.8518027750386636, 9.936999415048941131 ) ) ;
#20929 = CARTESIAN_POINT ( 'NONE',  ( 14.29190075645216851, 6.456385560668102208, -7.561819230143448145 ) ) ;
#20931 = CARTESIAN_POINT ( 'NONE',  ( -17.52435683634852737, 50.00000000000000000, 63.16488839464014404 ) ) ;
#20932 = CARTESIAN_POINT ( 'NONE',  ( 7.500000000000000888, -3.000671055698259870, -20.99923901233272971 ) ) ;
#20933 = CARTESIAN_POINT ( 'NONE',  ( 11.89091310976916382, -16.57373600184161688, -34.65102486210439281 ) ) ;
#20934 = DIRECTION ( 'NONE',  ( 1.000000000000000000, 0.000000000000000000, 0.000000000000000000 ) ) ;
#20935 = CARTESIAN_POINT ( 'NONE',  ( 0.000000000000000000, 0.000000000000000000, 0.000000000000000000 ) ) ;
#20936 = CONICAL_SURFACE ( 'NONE', #10479, 5.000000000000010658, 0.9599310885968697082 ) ;
#20937 = ORIENTED_EDGE ( 'NONE', *, *, #36601, .F. ) ;
#20938 = SURFACE_STYLE_FILL_AREA ( #62942 ) ;
#20939 = CARTESIAN_POINT ( 'NONE',  ( -17.60110216499754188, -25.55142791915394085, 28.43521521110582384 ) ) ;
#20940 =( BOUNDED_SURFACE ( )  B_SPLINE_SURFACE ( 2, 3, ( 
 ( #40036, #39521, #88591, #72396 ),
 ( #29331, #104226, #5022, #56181 ),
 ( #70815, #6588, #62732, #31445 ) ),
 .UNSPECIFIED., .F., .F., .F. ) 
 B_SPLINE_SURFACE_WITH_KNOTS ( ( 3, 3 ),
 ( 4, 4 ),
 ( 0.000000000000000000, 1.000000000000000000 ),
 ( 0.000000000000000000, 0.003049892549641993172 ),
 .UNSPECIFIED. ) 
 GEOMETRIC_REPRESENTATION_ITEM ( )  RATIONAL_B_SPLINE_SURFACE ( (
 ( 1.000000000000000000, 1.000000000000000000, 1.000000000000000000, 1.000000000000000000),
 ( 1.857142857142858317, 1.857142857142858317, 1.857142857142858317, 1.857142857142858317),
 ( 1.000000000000000000, 1.000000000000000000, 1.000000000000000000, 1.000000000000000000) ) ) 
 REPRESENTATION_ITEM ( '' )  SURFACE ( )  );
#20942 = CARTESIAN_POINT ( 'NONE',  ( 41.46910480218704009, 484.7338956289814860, -3.418960549715446717 ) ) ;
#20941 = CARTESIAN_POINT ( 'NONE',  ( -85.46309781643650183, -60.00000000000000000, -15.18018135029764970 ) ) ;
#20943 = ADVANCED_FACE ( 'NONE', ( #87030 ), #19472, .F. ) ;
#20944 = ORIENTED_EDGE ( 'NONE', *, *, #102935, .F. ) ;
#20945 = B_SPLINE_CURVE_WITH_KNOTS ( 'NONE', 3,
 ( #49825, #64439, #55771, #31556, #88706, #80593, #89241, #40144, #97313, #23465, #81640, #73558 ),
 .UNSPECIFIED., .F., .F.,
 ( 4, 2, 2, 2, 2, 4 ),
 ( 0.04761886307670518126, 0.05150820645496530931, 0.05539754983322543735, 0.06317623658974569345, 0.07095492334626596342, 0.07873361010278621952 ),
 .UNSPECIFIED. ) ;
#20946 = TOROIDAL_SURFACE ( 'NONE', #51832, 6.999999999999999112, 0.5000000000000000000 ) ;
#20947 = SURFACE_STYLE_USAGE ( .BOTH. , #5244 ) ;
#20948 = ORIENTED_EDGE ( 'NONE', *, *, #40628, .T. ) ;
#20949 = CARTESIAN_POINT ( 'NONE',  ( -12.84929146819454182, 42.47186473153507080, -92.83514476613449062 ) ) ;
#20950 =( GEOMETRIC_REPRESENTATION_CONTEXT ( 3 ) GLOBAL_UNCERTAINTY_ASSIGNED_CONTEXT ( ( #40829 ) ) GLOBAL_UNIT_ASSIGNED_CONTEXT ( ( #61928, #36076, #68949 ) ) REPRESENTATION_CONTEXT ( 'NONE', 'WORKASPACE' ) );
#20951 = EDGE_CURVE ( 'NONE', #58013, #457, #41819, .T. ) ;
#20952 = CIRCLE ( 'NONE', #81172, 4.000000000000007105 ) ;
#20953 = CARTESIAN_POINT ( 'NONE',  ( 16.01293590580093351, 3.745177866445061010, -0.6593600975748525883 ) ) ;
#20954 = CYLINDRICAL_SURFACE ( 'NONE', #14825, 10.00000000000000000 ) ;
#20955 = ORIENTED_EDGE ( 'NONE', *, *, #57357, .F. ) ;
#20956 = CARTESIAN_POINT ( 'NONE',  ( 32.88333705524289741, 439.7317646416726689, 24.13381181826147071 ) ) ;
#20957 = CARTESIAN_POINT ( 'NONE',  ( 104.4029495770615910, -60.15230426517445039, 189.8444650207596851 ) ) ;
#20959 = SURFACE_STYLE_USAGE ( .BOTH. , #69985 ) ;
#20958 = CARTESIAN_POINT ( 'NONE',  ( -13.50000000000000178, 0.000000000000000000, 0.000000000000000000 ) ) ;
#20960 = ORIENTED_EDGE ( 'NONE', *, *, #15164, .F. ) ;
#20961 = ORIENTED_EDGE ( 'NONE', *, *, #95242, .F. ) ;
#20962 = VERTEX_POINT ( 'NONE', #33050 ) ;
#20963 = CARTESIAN_POINT ( 'NONE',  ( 24.30353620171109341, 306.6619372981346032, 10.34251987938447748 ) ) ;
#20964 = EDGE_LOOP ( 'NONE', ( #22639, #64641, #90698, #55674 ) ) ;
#20965 = EDGE_CURVE ( 'NONE', #29545, #14796, #31542, .T. ) ;
#20966 = FILL_AREA_STYLE_COLOUR ( '', #22097 ) ;
#20967 = CARTESIAN_POINT ( 'NONE',  ( -5.041270137995550904, 41.82074860089117152, -70.25592743835888143 ) ) ;
#20969 = CARTESIAN_POINT ( 'NONE',  ( -90.19250537024298353, -59.99999999999759126, -22.67060294277911225 ) ) ;
#20968 = VECTOR ( 'NONE', #6695, 1000.000000000000000 ) ;
#20970 = DIRECTION ( 'NONE',  ( -1.000000000000000000, -1.224606353822377258E-16, -0.000000000000000000 ) ) ;
#20971 = CARTESIAN_POINT ( 'NONE',  ( 34.27131652679207718, -60.00000000000002132, 45.75654928052989590 ) ) ;
#20972 = CARTESIAN_POINT ( 'NONE',  ( -10.49999999997808331, -5.000000000000000000, -12.52300748972991506 ) ) ;
#20973 = CARTESIAN_POINT ( 'NONE',  ( -6.228838570019490817, 41.78908843073880774, -58.91793930065269791 ) ) ;
#20974 = VECTOR ( 'NONE', #44953, 1000.000000000000000 ) ;
#20976 = CARTESIAN_POINT ( 'NONE',  ( 10.48337731409090701, -60.35894641967450980, 33.96424879542498587 ) ) ;
#20975 = CARTESIAN_POINT ( 'NONE',  ( -91.97835729869039767, -14.21045842199439591, 64.70454208516892436 ) ) ;
#20977 = CARTESIAN_POINT ( 'NONE',  ( -7.939150208838348100, 52.04628108490835814, 1.683917007163810764 ) ) ;
#20978 = CARTESIAN_POINT ( 'NONE',  ( -48.73406339952293109, -36.06067253240158266, 47.64192311054786444 ) ) ;
#20979 = AXIS2_PLACEMENT_3D ( 'NONE', #27008, #86296, #51765 ) ;
#20980 = DIRECTION ( 'NONE',  ( 0.000000000000000000, 1.000000000000000000, -0.000000000000000000 ) ) ;
#20981 = ORIENTED_EDGE ( 'NONE', *, *, #16211, .T. ) ;
#20982 = CARTESIAN_POINT ( 'NONE',  ( 39.68467815576448743, 459.8383127612376029, 1.879537633271029851 ) ) ;
#20983 = CARTESIAN_POINT ( 'NONE',  ( 5.290067270632322405, -1.200000000000000030E-05, 7.281152949374479100 ) ) ;
#20984 = PLANE ( 'NONE',  #65464 ) ;
#20985 = ORIENTED_EDGE ( 'NONE', *, *, #736, .T. ) ;
#20986 = CARTESIAN_POINT ( 'NONE',  ( -5.060123309432819738, -8.366457779114602644, 13.66741525926336465 ) ) ;
#20987 = ORIENTED_EDGE ( 'NONE', *, *, #44870, .T. ) ;
#20988 = CARTESIAN_POINT ( 'NONE',  ( 85.53273786284641744, -30.00000000000759570, -20.40353017611455044 ) ) ;
#20989 = CARTESIAN_POINT ( 'NONE',  ( 3.801077171203071536, -48.88909605940820313, 104.1059035333590685 ) ) ;
#20990 = CARTESIAN_POINT ( 'NONE',  ( -2.745291993961042731, -9.118645366782532236, -12.27859709492980578 ) ) ;
#20991 = CARTESIAN_POINT ( 'NONE',  ( -33.52312678239033517, 18.64316884709848665, 19.32152200342503079 ) ) ;
#20992 = CARTESIAN_POINT ( 'NONE',  ( 97.87774770175602157, -30.00000000000000000, 190.6451874487673877 ) ) ;
#20993 = LINE ( 'NONE', #5807, #29459 ) ;
#20994 = EDGE_LOOP ( 'NONE', ( #34298, #74438, #87803, #88676, #41785, #15289 ) ) ;
#20995 = VERTEX_POINT ( 'NONE', #49727 ) ;
#20996 = ORIENTED_EDGE ( 'NONE', *, *, #85794, .F. ) ;
#20997 = CARTESIAN_POINT ( 'NONE',  ( 55.11151443560458318, -42.96699192481832341, 61.94517765222524019 ) ) ;
#20998 = DIRECTION ( 'NONE',  ( 0.000000000000000000, -1.000000000000000000, 0.000000000000000000 ) ) ;
#20999 = CARTESIAN_POINT ( 'NONE',  ( 13.63130828375568981, 294.5445729804733901, -10.06530370901874072 ) ) ;
#21000 = VERTEX_POINT ( 'NONE', #80 ) ;
#21001 = FACE_OUTER_BOUND ( 'NONE', #31405, .T. ) ;
#21002 = EDGE_LOOP ( 'NONE', ( #36593, #28650, #77510, #10956 ) ) ;
#21003 = CARTESIAN_POINT ( 'NONE',  ( 0.05458999538772964233, -1.264741368073340144, -6.500000000000001776 ) ) ;
#21004 = CARTESIAN_POINT ( 'NONE',  ( 94.26160709180628317, -38.49159546897875828, 201.2047994037039018 ) ) ;
#21005 = CARTESIAN_POINT ( 'NONE',  ( 13.75548730145301057, 20.47407606505949218, 6.665969588725104700 ) ) ;
#21006 = CARTESIAN_POINT ( 'NONE',  ( 83.67118919527318610, -45.28250476704045724, 13.41276670706853658 ) ) ;
#21007 = CARTESIAN_POINT ( 'NONE',  ( 4.464296094009049476, 13.01099471650158534, -0.1149164202474796115 ) ) ;
#21008 = FACE_BOUND ( 'NONE', #82445, .T. ) ;
#21009 = AXIS2_PLACEMENT_3D ( 'NONE', #17140, #41926, #24189 ) ;
#21010 = CARTESIAN_POINT ( 'NONE',  ( -39.86761651079807223, 459.8416857619844222, 1.882458089121660905 ) ) ;
#21011 = STYLED_ITEM ( 'NONE', ( #80918 ), #51131 ) ;
#21012 = DIRECTION ( 'NONE',  ( 0.000000000000000000, -1.000000000000000000, 0.000000000000000000 ) ) ;
#21013 = ORIENTED_EDGE ( 'NONE', *, *, #85457, .T. ) ;
#21014 = CARTESIAN_POINT ( 'NONE',  ( -3.313708498984760276, -10.71875000409677270, -8.000000000000000000 ) ) ;
#21015 = EDGE_CURVE ( 'NONE', #74342, #78081, #46976, .T. ) ;
#21016 = CARTESIAN_POINT ( 'NONE',  ( 16.18712010533798562, 37.20509496956294981, -21.93868532144439598 ) ) ;
#21017 = CARTESIAN_POINT ( 'NONE',  ( -4.469491342313713922, 142.4783567884534818, 5.000000000000000000 ) ) ;
#21018 = ORIENTED_EDGE ( 'NONE', *, *, #59625, .T. ) ;
#21019 = EDGE_CURVE ( 'NONE', #90586, #31791, #65947, .T. ) ;
#21020 = CARTESIAN_POINT ( 'NONE',  ( -31.93573408248750312, 317.9195443334689344, -5.838035979257788277 ) ) ;
#21021 = CARTESIAN_POINT ( 'NONE',  ( -39.62459902451224991, 316.6078743528785253, 7.208843829914820311 ) ) ;
#21022 = CARTESIAN_POINT ( 'NONE',  ( 2.500000000000000444, -30.00000000000000000, 28.88619651857252535 ) ) ;
#21023 =( NAMED_UNIT ( * ) SI_UNIT ( $, .STERADIAN. ) SOLID_ANGLE_UNIT ( ) );
#21024 = CARTESIAN_POINT ( 'NONE',  ( -8.000000000000001776, -19.15624999999999289, 3.313708498984758943 ) ) ;
#21025 = CARTESIAN_POINT ( 'NONE',  ( -39.45711635436059339, -37.46255045984162280, 49.12914128638639255 ) ) ;
#21026 = VECTOR ( 'NONE', #9355, 1000.000000000000114 ) ;
#21027 = EDGE_CURVE ( 'NONE', #83885, #22672, #81346, .T. ) ;
#21028 = CIRCLE ( 'NONE', #226, 5.000000000000002665 ) ;
#21029 = PRODUCT_DEFINITION_SHAPE ( 'NONE', 'NONE',  #106812 ) ;
#21030 = CARTESIAN_POINT ( 'NONE',  ( 40.30492368078588328, 437.3365155501883237, 5.155601643837086634 ) ) ;
#21031 = EDGE_LOOP ( 'NONE', ( #24375, #60875, #39733, #61845 ) ) ;
#21032 = CARTESIAN_POINT ( 'NONE',  ( 85.72993351955908281, -28.54124513701082222, 179.8117750706674371 ) ) ;
#21033 = DIRECTION ( 'NONE',  ( 1.000000000000000000, 0.000000000000000000, 0.000000000000000000 ) ) ;
#21034 = CARTESIAN_POINT ( 'NONE',  ( 54.52222222222221859, 3.309500000000014541, 4.052968581778174646E-16 ) ) ;
#21035 = VERTEX_POINT ( 'NONE', #67524 ) ;
#21036 = CARTESIAN_POINT ( 'NONE',  ( -87.11468308431049934, -52.70903455444622665, 42.62993231004110584 ) ) ;
#21037 = EDGE_CURVE ( 'NONE', #74776, #76086, #91810, .T. ) ;
#21038 = DIRECTION ( 'NONE',  ( -0.000000000000000000, -0.000000000000000000, -1.000000000000000000 ) ) ;
#21039 = CARTESIAN_POINT ( 'NONE',  ( -2.384812152908770244, -5.000000000000002665, -98.00000000000000000 ) ) ;
#21040 = LINE ( 'NONE', #22071, #48968 ) ;
#21041 = AXIS2_PLACEMENT_3D ( 'NONE', #23311, #16249, #64292 ) ;
#21042 = CARTESIAN_POINT ( 'NONE',  ( 11.61272280578022098, -20.93722706496040331, 35.52699528997413836 ) ) ;
#21043 = CARTESIAN_POINT ( 'NONE',  ( 3.677391134430071151, -1.015220045778296276, 104.0097548473155626 ) ) ;
#21044 = CARTESIAN_POINT ( 'NONE',  ( 38.75764833851163615, -25.78963212653746240, 35.18533521607095338 ) ) ;
#21046 = CARTESIAN_POINT ( 'NONE',  ( -11.77389790720900464, 19.14645581668979446, 7.901544587056179125 ) ) ;
#21045 = CARTESIAN_POINT ( 'NONE',  ( 37.45944789261785957, 486.5137780151753759, 13.75061995631740963 ) ) ;
#21047 = PRESENTATION_LAYER_ASSIGNMENT (  '', '', ( #46858 ) ) ;
#21048 = CARTESIAN_POINT ( 'NONE',  ( 9.218636978371788970, 294.6649786875626660, -3.878494680376622483 ) ) ;
#21049 = DIRECTION ( 'NONE',  ( 0.000000000000000000, -1.000000000000000000, 0.000000000000000000 ) ) ;
#21050 = CARTESIAN_POINT ( 'NONE',  ( -27.99999999999999645, 0.000000000000000000, 0.000000000000000000 ) ) ;
#21051 = CARTESIAN_POINT ( 'NONE',  ( -16.46333734837338270, 294.5649015166168283, 1.876035010524102820 ) ) ;
#21052 = CARTESIAN_POINT ( 'NONE',  ( -83.27438428636391166, -38.00000000000004263, -5.225543532278351222 ) ) ;
#21053 = ORIENTED_EDGE ( 'NONE', *, *, #57481, .F. ) ;
#21054 = CARTESIAN_POINT ( 'NONE',  ( -9.285538112422313972, -2.937467806972811957, 14.74006110461671071 ) ) ;
#21055 = CARTESIAN_POINT ( 'NONE',  ( 46.00000000000000000, 488.2683853232034039, 2.802483919472203766 ) ) ;
#21056 = CARTESIAN_POINT ( 'NONE',  ( -14.29190075644809887, 19.61368180395988148, 4.501023549812855684 ) ) ;
#21058 = CARTESIAN_POINT ( 'NONE',  ( -6.362823198315364692, -47.40890495455883524, -34.69792613639604184 ) ) ;
#21057 = CARTESIAN_POINT ( 'NONE',  ( 2.494577234427376227E-15, -18.92596047533412573, 20.36976895023282097 ) ) ;
#21059 = ADVANCED_FACE ( 'NONE', ( #73458 ), #21169, .T. ) ;
#21060 = VERTEX_POINT ( 'NONE', #76655 ) ;
#21061 = FACE_OUTER_BOUND ( 'NONE', #38925, .T. ) ;
#21062 = ORIENTED_EDGE ( 'NONE', *, *, #93507, .T. ) ;
#21063 = EDGE_CURVE ( 'NONE', #12410, #18381, #37669, .T. ) ;
#21064 = ADVANCED_FACE ( 'NONE', ( #20076 ), #86674, .F. ) ;
#21065 = CARTESIAN_POINT ( 'NONE',  ( 14.83349330513380693, 4.898587196589411843E-16, -4.000000000000001776 ) ) ;
#21066 = CYLINDRICAL_SURFACE ( 'NONE', #58017, 4.000000000000000000 ) ;
#21067 = CARTESIAN_POINT ( 'NONE',  ( -94.39340477423540676, -59.99999999999999289, 44.46429842255393083 ) ) ;
#21068 = VERTEX_POINT ( 'NONE', #2224 ) ;
#21069 = CARTESIAN_POINT ( 'NONE',  ( 13.86650669486618881, 4.898587196589413815E-16, -4.000000000000000888 ) ) ;
#21070 = FILL_AREA_STYLE_COLOUR ( '', #48873 ) ;
#21071 = CARTESIAN_POINT ( 'NONE',  ( -9.699121749566360862, 26.82331239724179994, 2.444499528233560870 ) ) ;
#21073 = CYLINDRICAL_SURFACE ( 'NONE', #3075, 8.000000000000000000 ) ;
#21072 = CARTESIAN_POINT ( 'NONE',  ( -3.313708498984783812, -26.46875000000000000, 7.999999999999979572 ) ) ;
#21074 = ADVANCED_FACE ( 'NONE', ( #53460 ), #77199, .F. ) ;
#21075 = CARTESIAN_POINT ( 'NONE',  ( -83.47692913927937752, -35.99746531496888480, 168.8096269909763691 ) ) ;
#21076 = ORIENTED_EDGE ( 'NONE', *, *, #3982, .T. ) ;
#21077 = CARTESIAN_POINT ( 'NONE',  ( 6.499999999999999112, 3.752776749732559036, -6.064240316920397333 ) ) ;
#21078 = VERTEX_POINT ( 'NONE', #85290 ) ;
#21079 = VERTEX_POINT ( 'NONE', #3311 ) ;
#21080 = CARTESIAN_POINT ( 'NONE',  ( 12.10102349785733544, -5.000000000000000000, 11.47683805494732390 ) ) ;
#21081 = DIRECTION ( 'NONE',  ( 0.5735764363510468256, 0.8191520442889913545, 0.000000000000000000 ) ) ;
#21082 = VERTEX_POINT ( 'NONE', #68594 ) ;
#21083 = EDGE_CURVE ( 'NONE', #36198, #86058, #14244, .T. ) ;
#21084 = CARTESIAN_POINT ( 'NONE',  ( -31.86301241941225726, 472.3478509189352508, 13.84919938057076294 ) ) ;
#21085 = CARTESIAN_POINT ( 'NONE',  ( -33.00000000000000000, 488.6481008951270155, 3.890293910847612668 ) ) ;
#21086 = CARTESIAN_POINT ( 'NONE',  ( -83.13494729127086202, -57.67105474064026538, -28.32277909022158724 ) ) ;
#21087 = CARTESIAN_POINT ( 'NONE',  ( 7.934996450857314976, -13.86862456472531058, -1.050865690281777010 ) ) ;
#21088 = FACE_OUTER_BOUND ( 'NONE', #57393, .T. ) ;
#21089 = DIRECTION ( 'NONE',  ( 1.000000000000000000, 1.224606353822377258E-16, 0.000000000000000000 ) ) ;
#21090 =( LENGTH_UNIT ( ) NAMED_UNIT ( * ) SI_UNIT ( .MILLI., .METRE. ) );
#21091 = CARTESIAN_POINT ( 'NONE',  ( 4.165977904505312246, 15.00000000000000000, -9.090909090909088164 ) ) ;
#21092 = AXIS2_PLACEMENT_3D ( 'NONE', #7259, #40170, #71467 ) ;
#21093 = CARTESIAN_POINT ( 'NONE',  ( 90.14752496014264693, -29.99999999999995026, -6.310861463900848456 ) ) ;
#21094 = EDGE_CURVE ( 'NONE', #58946, #26193, #17008, .T. ) ;
#21095 = CIRCLE ( 'NONE', #7252, 2.000000000000001776 ) ;
#21096 = CARTESIAN_POINT ( 'NONE',  ( -63.58375344335239987, -14.21045842199425024, 93.96584349151677884 ) ) ;
#21097 = CARTESIAN_POINT ( 'NONE',  ( -56.04191766312286660, -22.14874848805373375, 55.49595916207043445 ) ) ;
#21098 = VERTEX_POINT ( 'NONE', #101998 ) ;
#21099 = ORIENTED_EDGE ( 'NONE', *, *, #78109, .F. ) ;
#21100 = CARTESIAN_POINT ( 'NONE',  ( -101.8270732106297345, -60.22023256173742567, 194.3861460195847712 ) ) ;
#21101 = EDGE_CURVE ( 'NONE', #43603, #5811, #12447, .T. ) ;
#21102 = CARTESIAN_POINT ( 'NONE',  ( -0.7843429689301302243, 52.06967622658047645, 8.013317272959927351 ) ) ;
#21103 = B_SPLINE_CURVE_WITH_KNOTS ( 'NONE', 3,
 ( #51837, #84751, #19531, #10832, #43752, #105176, #23219, #21636, #104637, #46929, #5424, #37830, #70161, #5933, #63674, #38348, #80886, #30790, #87941, #79303, #70693, #95492, #62093, #86890, #31322, #103583, #96563, #94986, #22697, #38860, #14022, #22158, #55534, #103065, #71208, #62606 ),
 .UNSPECIFIED., .F., .F.,
 ( 4, 2, 2, 2, 2, 2, 2, 2, 2, 2, 2, 2, 2, 2, 2, 2, 2, 4 ),
 ( 0.000000000000000000, 0.0007996222028895878841, 0.001599244405779175768, 0.003198488811558350669, 0.003998111014447940613, 0.004797733217337530123, 0.005597355420227121368, 0.006396977623116711746, 0.006796788724561506935, 0.007196599826006302991, 0.007996222028895893369, 0.008795844231785483747, 0.009595466434675074124, 0.01039508863756465756, 0.01119471084045424274, 0.01159452194189903619, 0.01199433304334382965, 0.01279395524623341482 ),
 .UNSPECIFIED. ) ;
#21104 = ORIENTED_EDGE ( 'NONE', *, *, #94948, .T. ) ;
#21105 = CARTESIAN_POINT ( 'NONE',  ( 18.94735611194717606, 49.28911315852006680, 62.03557990934028510 ) ) ;
#21106 =( LENGTH_UNIT ( ) NAMED_UNIT ( * ) SI_UNIT ( .MILLI., .METRE. ) );
#21107 = CARTESIAN_POINT ( 'NONE',  ( 11.84999999999999787, 1.533819458162526451E-15, 0.000000000000000000 ) ) ;
#21108 = CARTESIAN_POINT ( 'NONE',  ( -2.977408999572650039, -13.06250000204838280, -7.188101187500001821 ) ) ;
#21109 = CARTESIAN_POINT ( 'NONE',  ( -2.224272751641298562, -69.45625592918534608, 12.90769492712830413 ) ) ;
#21110 = FACE_OUTER_BOUND ( 'NONE', #3709, .T. ) ;
#21111 = CARTESIAN_POINT ( 'NONE',  ( 7.934914944860278041, -81.13154352799891456, -1.051261972695691771 ) ) ;
#21112 = CARTESIAN_POINT ( 'NONE',  ( -32.35336999986095208, 300.6590557721156642, 11.25190399080426751 ) ) ;
#21113 = CARTESIAN_POINT ( 'NONE',  ( -9.268239551722324165, 44.06621912919404593, -13.41314811874801016 ) ) ;
#21114 = CARTESIAN_POINT ( 'NONE',  ( 104.0908829527487711, -2.002967142162725287E-29, 5.000000000000011546 ) ) ;
#21115 = CARTESIAN_POINT ( 'NONE',  ( -1.469576158976823947E-15, -24.87499999999999289, 8.000000000000000000 ) ) ;
#21116 = UNCERTAINTY_MEASURE_WITH_UNIT (LENGTH_MEASURE( 1.000000000000000082E-05 ), #29470, 'distance_accuracy_value', 'NONE');
#21117 = CARTESIAN_POINT ( 'NONE',  ( -28.23837029583884828, -46.43733527002056150, 33.78025300252188146 ) ) ;
#21118 = CIRCLE ( 'NONE', #12431, 4.000000000000001776 ) ;
#21119 = ORIENTED_EDGE ( 'NONE', *, *, #99020, .T. ) ;
#21120 = VERTEX_POINT ( 'NONE', #27095 ) ;
#21121 = CARTESIAN_POINT ( 'NONE',  ( 47.01065226741122416, -25.69391163712711190, 42.17763454979905902 ) ) ;
#21122 = CIRCLE ( 'NONE', #34885, 13.00000000000003730 ) ;
#21123 = CARTESIAN_POINT ( 'NONE',  ( -1.159787357822634979, 11.84251578204911759, 50.01779155637117924 ) ) ;
#21124 = FACE_OUTER_BOUND ( 'NONE', #66385, .T. ) ;
#21125 = VECTOR ( 'NONE', #19610, 1000.000000000000227 ) ;
#21126 = CARTESIAN_POINT ( 'NONE',  ( -85.18710009866828159, -38.69275026109524163, 198.6025544802344598 ) ) ;
#21127 = ORIENTED_EDGE ( 'NONE', *, *, #75483, .T. ) ;
#21128 = CARTESIAN_POINT ( 'NONE',  ( 91.21471444279342222, -38.35841293779726158, -0.8993804321188152429 ) ) ;
#21129 = CARTESIAN_POINT ( 'NONE',  ( -18.92118552154158806, 48.85453644119221650, 62.14239264200793400 ) ) ;
#21130 = CARTESIAN_POINT ( 'NONE',  ( 6.743821559472605642, 40.92373752580943602, -71.01439591878522606 ) ) ;
#21131 = CARTESIAN_POINT ( 'NONE',  ( -33.06850474076788515, 435.0785904875464780, 15.57666385384312413 ) ) ;
#21132 = CARTESIAN_POINT ( 'NONE',  ( 0.05533025579362303714, -6.264553569211845918, 2.149474931388141830 ) ) ;
#21134 = TOROIDAL_SURFACE ( 'NONE', #81337, 13.00000000000000000, 2.000000000000000000 ) ;
#21133 = CARTESIAN_POINT ( 'NONE',  ( 12.50000000000000711, -3.000000000000000000, -78.42624373368740009 ) ) ;
#21135 = CARTESIAN_POINT ( 'NONE',  ( 108.8511657955034906, -59.99999999999997868, 194.0146055469417661 ) ) ;
#21136 = CARTESIAN_POINT ( 'NONE',  ( -15.98906220215687313, 34.48549488436115951, 24.06010465822882338 ) ) ;
#21137 = ORIENTED_EDGE ( 'NONE', *, *, #90201, .F. ) ;
#21138 = DIRECTION ( 'NONE',  ( 0.000000000000000000, 0.000000000000000000, -1.000000000000000000 ) ) ;
#21139 = ADVANCED_FACE ( 'NONE', ( #69645, #28687 ), #37307, .T. ) ;
#21140 = CARTESIAN_POINT ( 'NONE',  ( 74.07777777777778283, 6.915964383211875250E-15, 0.000000000000000000 ) ) ;
#21141 = ORIENTED_EDGE ( 'NONE', *, *, #27648, .T. ) ;
#21143 = CARTESIAN_POINT ( 'NONE',  ( 5.224631516565895417, 7.366007320495609356, -27.80123404716705693 ) ) ;
#21142 = CARTESIAN_POINT ( 'NONE',  ( -91.26961475985454797, -38.36108261039323963, -1.705770521583544586 ) ) ;
#21144 = CARTESIAN_POINT ( 'NONE',  ( 46.00000000000001421, 438.2677368034359233, 10.58177734929973290 ) ) ;
#21145 = DIRECTION ( 'NONE',  ( -1.000000000000000000, -1.224606353822377258E-16, -0.000000000000000000 ) ) ;
#21146 = CARTESIAN_POINT ( 'NONE',  ( -2.499999999999978684, -29.99999999999999645, 28.88619816519791073 ) ) ;
#21147 = CARTESIAN_POINT ( 'NONE',  ( 2.977408999572650927, -16.25000000204838813, -7.188101187500001821 ) ) ;
#21148 = CARTESIAN_POINT ( 'NONE',  ( 6.145467200816499442, -5.000000000008177459, -92.99666842292330671 ) ) ;
#21149 = EDGE_CURVE ( 'NONE', #84857, #77950, #59981, .T. ) ;
#21150 = EDGE_CURVE ( 'NONE', #64162, #93942, #105574, .T. ) ;
#21151 = CARTESIAN_POINT ( 'NONE',  ( 30.04234920459604652, 13.07620473719202714, -42.05403970751778076 ) ) ;
#21153 = ORIENTED_EDGE ( 'NONE', *, *, #40644, .T. ) ;
#21152 = DIRECTION ( 'NONE',  ( -1.000000000000000000, -1.224606353822377258E-16, -0.000000000000000000 ) ) ;
#21154 = CARTESIAN_POINT ( 'NONE',  ( 84.21880853279326118, -32.47281885837850268, 170.3671019177896824 ) ) ;
#21155 = ADVANCED_FACE ( 'NONE', ( #51309 ), #59083, .T. ) ;
#21156 = CARTESIAN_POINT ( 'NONE',  ( 9.609486011791450011, 8.908497650347621644, 0.000000000000000000 ) ) ;
#21157 = DIRECTION ( 'NONE',  ( 0.000000000000000000, 0.000000000000000000, -1.000000000000000000 ) ) ;
#21158 = EDGE_LOOP ( 'NONE', ( #69367, #90421, #72732, #23099 ) ) ;
#21159 = CIRCLE ( 'NONE', #69320, 4.000000000000000000 ) ;
#21160 = CARTESIAN_POINT ( 'NONE',  ( -33.97150963885389530, 317.2836215396021089, -6.519267954480356231 ) ) ;
#21161 = EDGE_CURVE ( 'NONE', #68169, #52941, #72834, .T. ) ;
#21162 = CARTESIAN_POINT ( 'NONE',  ( 2.602085213965210642E-15, 15.58845726811991561, -11.79422863405993382 ) ) ;
#21163 = FILL_AREA_STYLE ('',( #79343 ) ) ;
#21164 = DIRECTION ( 'NONE',  ( -1.000000000000000000, -1.224606353822377258E-16, -0.000000000000000000 ) ) ;
#21165 = PRESENTATION_LAYER_ASSIGNMENT (  '', '', ( #5631 ) ) ;
#21166 = FACE_OUTER_BOUND ( 'NONE', #21975, .T. ) ;
#21167 = CARTESIAN_POINT ( 'NONE',  ( 17.85301235858413804, 43.24702788698653677, 5.052089591447788131 ) ) ;
#21168 = ORIENTED_EDGE ( 'NONE', *, *, #75417, .F. ) ;
#21170 = CARTESIAN_POINT ( 'NONE',  ( -9.678462853824605361, 294.6717994822394644, 2.536598382984742273 ) ) ;
#21169 = CONICAL_SURFACE ( 'NONE', #40064, 6.500000000000000000, 1.047197551196600296 ) ;
#21171 = CARTESIAN_POINT ( 'NONE',  ( 0.000000000000000000, 0.000000000000000000, -6.999999999999993783 ) ) ;
#21172 = LINE ( 'NONE', #70209, #44207 ) ;
#21174 = CARTESIAN_POINT ( 'NONE',  ( -15.78841396623141513, 4.459144360354060588, -5.230423732636918288 ) ) ;
#21173 = DIRECTION ( 'NONE',  ( 0.000000000000000000, 1.000000000000000000, 0.000000000000000000 ) ) ;
#21175 = CARTESIAN_POINT ( 'NONE',  ( 2.977408999572650927, -17.37500000204838457, -7.188101187500001821 ) ) ;
#21176 = CARTESIAN_POINT ( 'NONE',  ( -30.00000000000000000, 488.7759337287078552, 4.253621113604353354 ) ) ;
#21177 = DIRECTION ( 'NONE',  ( 1.224646799147353454E-16, 0.000000000000000000, -1.000000000000000000 ) ) ;
#21178 = ORIENTED_EDGE ( 'NONE', *, *, #95616, .F. ) ;
#21179 = CARTESIAN_POINT ( 'NONE',  ( 38.79830821498527627, 485.8176106091541442, -4.884814968350399411 ) ) ;
#21180 = CARTESIAN_POINT ( 'NONE',  ( 43.75010090114224681, 464.8337800386878484, 11.75004750934975029 ) ) ;
#21181 = CARTESIAN_POINT ( 'NONE',  ( -9.311676254474896552, 11.24588917688063106, -8.673617379354307486E-16 ) ) ;
#21182 = DIRECTION ( 'NONE',  ( -0.5735764363510459374, -0.8191520442889919096, 0.000000000000000000 ) ) ;
#21183 =( GEOMETRIC_REPRESENTATION_CONTEXT ( 3 ) GLOBAL_UNCERTAINTY_ASSIGNED_CONTEXT ( ( #100320 ) ) GLOBAL_UNIT_ASSIGNED_CONTEXT ( ( #34411, #5718, #28441 ) ) REPRESENTATION_CONTEXT ( 'NONE', 'WORKASPACE' ) );
#21184 = ORIENTED_EDGE ( 'NONE', *, *, #71183, .T. ) ;
#21185 = CARTESIAN_POINT ( 'NONE',  ( -7.800811591264651845, 52.08872798781089131, -1.773736857837786784 ) ) ;
#21186 = CIRCLE ( 'NONE', #83271, 0.5000000000000004441 ) ;
#21187 = ORIENTED_EDGE ( 'NONE', *, *, #28723, .F. ) ;
#21188 = ADVANCED_FACE ( 'NONE', ( #53962 ), #70681, .T. ) ;
#21189 =( NAMED_UNIT ( * ) SI_UNIT ( $, .STERADIAN. ) SOLID_ANGLE_UNIT ( ) );
#21190 = DIRECTION ( 'NONE',  ( -1.000000000000000000, -0.000000000000000000, -0.000000000000000000 ) ) ;
#21191 = UNCERTAINTY_MEASURE_WITH_UNIT (LENGTH_MEASURE( 1.000000000000000082E-05 ), #57602, 'distance_accuracy_value', 'NONE');
#21192 = CARTESIAN_POINT ( 'NONE',  ( -110.5629728245914833, -60.00000000000001421, 189.2218377042151474 ) ) ;
#21193 = DIRECTION ( 'NONE',  ( -1.224646799147353454E-16, 0.000000000000000000, -1.000000000000000000 ) ) ;
#21195 = AXIS2_PLACEMENT_3D ( 'NONE', #49195, #32528, #104793 ) ;
#21194 = CARTESIAN_POINT ( 'NONE',  ( 20.21880305278369150, 304.8280059657581660, -9.005058168222337400 ) ) ;
#21196 = CARTESIAN_POINT ( 'NONE',  ( -5.075741750048029743, -4.332638003024074536, -17.09621982684887698 ) ) ;
#21197 = CARTESIAN_POINT ( 'NONE',  ( 5.299999999999999822, -7.505553499465137612, 3.546421054897781431E-16 ) ) ;
#21198 = CARTESIAN_POINT ( 'NONE',  ( -84.10365043901819604, -39.44059402239971490, 178.9954971936382435 ) ) ;
#21199 = CARTESIAN_POINT ( 'NONE',  ( 25.53945892759312031, 1.340359594676612611E-15, 0.000000000000000000 ) ) ;
#21200 = VERTEX_POINT ( 'NONE', #87953 ) ;
#21201 = CARTESIAN_POINT ( 'NONE',  ( -10.00000000000000178, 0.000000000000000000, -9.999999999999998224 ) ) ;
#21202 = CARTESIAN_POINT ( 'NONE',  ( 5.649205854336968535, -68.45354532811516890, -2.034449005107560993 ) ) ;
#21203 = CARTESIAN_POINT ( 'NONE',  ( -82.50477553219911897, -37.82685549418413729, 17.02917934263369304 ) ) ;
#21204 = CARTESIAN_POINT ( 'NONE',  ( -31.96729082391632559, 486.9543932134526472, 7.084325681754340742 ) ) ;
#21205 = CARTESIAN_POINT ( 'NONE',  ( -4.469712646659624866, 142.4802100387212533, -5.000000000000000000 ) ) ;
#21206 = CARTESIAN_POINT ( 'NONE',  ( -6.837824896291513355, -3.947820044545450102, -6.564402953523720718 ) ) ;
#21207 = CARTESIAN_POINT ( 'NONE',  ( 57.69562748396959506, 41.99999999991776178, -15.50526908263404735 ) ) ;
#21208 = CARTESIAN_POINT ( 'NONE',  ( 97.13532076618713518, -30.00000000000002842, 199.9107784265496264 ) ) ;
#21209 = CARTESIAN_POINT ( 'NONE',  ( -98.18081844100633759, 27.55047179872464724, 49.09040922050316880 ) ) ;
#21210 = ADVANCED_FACE ( 'NONE', ( #22172 ), #33514, .T. ) ;
#21211 = CARTESIAN_POINT ( 'NONE',  ( -109.5929118004772818, -60.00000000000001421, 123.9174817212569621 ) ) ;
#21212 = CARTESIAN_POINT ( 'NONE',  ( -63.92638894657200410, -46.43873725858485102, 86.65927405268175221 ) ) ;
#21213 = ORIENTED_EDGE ( 'NONE', *, *, #60902, .F. ) ;
#21214 = CARTESIAN_POINT ( 'NONE',  ( 94.36203364593035303, -29.99999999999990763, 200.0833959884570845 ) ) ;
#21215 = CARTESIAN_POINT ( 'NONE',  ( 62.40461286002861385, 39.42532709582792450, 18.42694020216206496 ) ) ;
#21216 = CARTESIAN_POINT ( 'NONE',  ( 76.83195493398949338, -60.00000000000498801, 195.9604342644627479 ) ) ;
#21217 = ORIENTED_EDGE ( 'NONE', *, *, #53760, .T. ) ;
#21218 = CARTESIAN_POINT ( 'NONE',  ( -33.00000000000000000, 463.5362553048592531, 6.739467187734391906 ) ) ;
#21219 = CARTESIAN_POINT ( 'NONE',  ( 5.082755093536325930, -17.84375000204838457, -5.082755093536325042 ) ) ;
#21220 = CONICAL_SURFACE ( 'NONE', #26383, 4.000000000000007105, 0.9599310885968835860 ) ;
#21221 = EDGE_CURVE ( 'NONE', #66555, #10104, #23529, .T. ) ;
#21222 = ORIENTED_EDGE ( 'NONE', *, *, #79354, .T. ) ;
#21223 = CARTESIAN_POINT ( 'NONE',  ( -8.000000000000001776, -26.84375000409677270, 3.313708498984759387 ) ) ;
#21224 = VERTEX_POINT ( 'NONE', #106225 ) ;
#21225 = CARTESIAN_POINT ( 'NONE',  ( 0.000000000000000000, 43.50000000000000711, -56.99999999999999289 ) ) ;
#21226 = AXIS2_PLACEMENT_3D ( 'NONE', #52685, #19850, #20393 ) ;
#21227 = CARTESIAN_POINT ( 'NONE',  ( -40.81956795959430906, 485.7841149218988335, -4.786840289928851355 ) ) ;
#21228 = CARTESIAN_POINT ( 'NONE',  ( -89.98621656989941187, -59.99999999999998579, -18.86310507760501665 ) ) ;
#21229 = CARTESIAN_POINT ( 'NONE',  ( 36.66638760098313554, 431.6597644233127085, 5.007224883190088960 ) ) ;
#21230 = CARTESIAN_POINT ( 'NONE',  ( -2.977408999572654480, -32.00000000204838813, 7.188101187499999156 ) ) ;
#21231 = DIRECTION ( 'NONE',  ( 0.000000000000000000, 0.000000000000000000, 1.000000000000000000 ) ) ;
#21232 = AXIS2_PLACEMENT_3D ( 'NONE', #86046, #43442, #61227 ) ;
#21233 = CARTESIAN_POINT ( 'NONE',  ( 8.127057321558243785, -4.285714285714296246, 23.93420880016848074 ) ) ;
#21234 = DIRECTION ( 'NONE',  ( -1.000000000000000000, -1.224606353822377258E-16, -0.000000000000000000 ) ) ;
#21235 = CARTESIAN_POINT ( 'NONE',  ( -7.896571385775229324, 108.7899799934575071, 1.305932416347436398 ) ) ;
#21236 = DIRECTION ( 'NONE',  ( 1.000000000000000000, 0.000000000000000000, -0.000000000000000000 ) ) ;
#21237 = CARTESIAN_POINT ( 'NONE',  ( 36.55294322374219718, 336.7270298077904727, -1.783817123648057335 ) ) ;
#21238 = ORIENTED_EDGE ( 'NONE', *, *, #24588, .T. ) ;
#21239 = CARTESIAN_POINT ( 'NONE',  ( -9.634713197495671011, 53.53784324394835181, -2.122499012415343334 ) ) ;
#21240 = CIRCLE ( 'NONE', #97018, 0.9999999999999998890 ) ;
#21241 = CARTESIAN_POINT ( 'NONE',  ( 35.05776305746996258, -25.64668665561590188, 32.62633962402455978 ) ) ;
#21242 = CARTESIAN_POINT ( 'NONE',  ( 22.23822744035697241, -8.673617379884035472E-16, -2.910977163136222678 ) ) ;
#21243 = EDGE_LOOP ( 'NONE', ( #99189, #38073, #10834, #26393, #60068, #22509 ) ) ;
#21244 = CARTESIAN_POINT ( 'NONE',  ( -9.999999999999996447, 48.00000000000000711, -83.69100306100429520 ) ) ;
#21246 = DIRECTION ( 'NONE',  ( -1.000000000000000000, -1.224606353822377258E-16, -0.000000000000000000 ) ) ;
#21245 = CARTESIAN_POINT ( 'NONE',  ( 6.831787912114839934, -4.999999999999999112, -15.36996511329311588 ) ) ;
#21247 = CARTESIAN_POINT ( 'NONE',  ( -5.000000000000000000, 0.000000000000000000, 0.000000000000000000 ) ) ;
#21248 = CARTESIAN_POINT ( 'NONE',  ( -4.852941176470598528, -3.000000000000002665, -70.80672828634229177 ) ) ;
#21249 = CARTESIAN_POINT ( 'NONE',  ( 2.499999999999997780, -18.83380486180452706, 27.02532357426314036 ) ) ;
#21250 = DIRECTION ( 'NONE',  ( -1.000000000000000000, -0.000000000000000000, -0.000000000000000000 ) ) ;
#21251 = DIRECTION ( 'NONE',  ( 0.000000000000000000, 0.000000000000000000, 1.000000000000000000 ) ) ;
#21252 = VERTEX_POINT ( 'NONE', #39928 ) ;
#21253 = CARTESIAN_POINT ( 'NONE',  ( 92.26678742429547242, -60.00000000000001421, 1.966542298145190326 ) ) ;
#21254 = CARTESIAN_POINT ( 'NONE',  ( 0.000000000000000000, 1.005902684993156715, -14.99698745252234566 ) ) ;
#21255 =( BOUNDED_CURVE ( )  B_SPLINE_CURVE ( 2, ( #99394, #154, #40650 ),
 .UNSPECIFIED., .F., .F. ) 
 B_SPLINE_CURVE_WITH_KNOTS ( ( 3, 3 ),
 ( 0.000000000000000000, 1.000000000000000000 ),
 .UNSPECIFIED. ) 
 CURVE ( )  GEOMETRIC_REPRESENTATION_ITEM ( )  RATIONAL_B_SPLINE_CURVE ( ( 1.000000000000000000, 1.857142857142858317, 1.000000000000000000 ) ) 
 REPRESENTATION_ITEM ( '' )  );
#21256 = PRESENTATION_LAYER_ASSIGNMENT (  '', '', ( #88364 ) ) ;
#21257 = CARTESIAN_POINT ( 'NONE',  ( -6.040019051097406333, 40.93519689175381870, -71.09856422274093291 ) ) ;
#21258 = CARTESIAN_POINT ( 'NONE',  ( 32.62207953394533178, 3.851859888774471706E-31, 5.000000000000001776 ) ) ;
#21259 = EDGE_LOOP ( 'NONE', ( #21351, #1306, #90105, #81875 ) ) ;
#21260 = B_SPLINE_CURVE_WITH_KNOTS ( 'NONE', 3,
 ( #2053, #34999, #957, #17203 ),
 .UNSPECIFIED., .F., .F.,
 ( 4, 4 ),
 ( 0.000000000000000000, 1.000000000000000000 ),
 .UNSPECIFIED. ) ;
#21261 = CARTESIAN_POINT ( 'NONE',  ( -105.7409267090946372, -30.00000000000445510, 194.2571602938600392 ) ) ;
#21262 = ORIENTED_EDGE ( 'NONE', *, *, #55043, .F. ) ;
#21263 = EDGE_CURVE ( 'NONE', #55118, #20770, #88413, .T. ) ;
#21264 = DIRECTION ( 'NONE',  ( -1.000000000000000000, -1.224606353822377258E-16, -0.000000000000000000 ) ) ;
#21265 = CYLINDRICAL_SURFACE ( 'NONE', #61454, 1.250000000000001110 ) ;
#21266 = CARTESIAN_POINT ( 'NONE',  ( 7.770228158362351145, 1.340359594676612611E-15, 0.000000000000000000 ) ) ;
#21267 = CARTESIAN_POINT ( 'NONE',  ( 14.37785056366748826, 21.52979621147868272, 5.240284069529759670 ) ) ;
#21268 = CARTESIAN_POINT ( 'NONE',  ( -6.499999999999999112, 0.6470732608156783972, -0.01945970098672775497 ) ) ;
#21269 = CARTESIAN_POINT ( 'NONE',  ( 2.977408999572650927, -32.75000000204839523, -7.188101187500001821 ) ) ;
#21270 = CARTESIAN_POINT ( 'NONE',  ( -44.19651249026929918, 485.6203925269955448, 3.557660179964223790 ) ) ;
#21271 = CARTESIAN_POINT ( 'NONE',  ( 9.076853247125631796, 45.89842957983098870, -14.51167170299882336 ) ) ;
#21272 = EDGE_CURVE ( 'NONE', #958, #106610, #56904, .T. ) ;
#21273 = ORIENTED_EDGE ( 'NONE', *, *, #94857, .T. ) ;
#21274 = ORIENTED_EDGE ( 'NONE', *, *, #81453, .F. ) ;
#21275 = CARTESIAN_POINT ( 'NONE',  ( 78.26004437794522062, -49.90185765714640098, 145.7829001237711850 ) ) ;
#21276 = CARTESIAN_POINT ( 'NONE',  ( 14.11595029532508505, 2.410436752314643716, 5.024000119269132369 ) ) ;
#21277 = ORIENTED_EDGE ( 'NONE', *, *, #31314, .T. ) ;
#21278 = CARTESIAN_POINT ( 'NONE',  ( -12.50000000000000355, 27.06290442698209020, -44.59571028169377627 ) ) ;
#21279 = ADVANCED_FACE ( 'NONE', ( #58221 ), #33988, .T. ) ;
#21280 = CARTESIAN_POINT ( 'NONE',  ( -5.082755093536325042, -20.09375000204838457, -5.082755093536325930 ) ) ;
#21281 = ADVANCED_FACE ( 'NONE', ( #106766 ), #64326, .T. ) ;
#21282 = CARTESIAN_POINT ( 'NONE',  ( -73.72791963761318357, -57.62431822613736898, 185.7849209195708227 ) ) ;
#21283 = ORIENTED_EDGE ( 'NONE', *, *, #102460, .F. ) ;
#21284 =( NAMED_UNIT ( * ) PLANE_ANGLE_UNIT ( ) SI_UNIT ( $, .RADIAN. ) );
#21285 = CARTESIAN_POINT ( 'NONE',  ( -4.497431761510338077, -10.54098124251033042, -3.972160586670083759 ) ) ;
#21286 = CARTESIAN_POINT ( 'NONE',  ( 6.913779129928547817, 41.73441125232163529, -59.30275354417914713 ) ) ;
#21287 = DIRECTION ( 'NONE',  ( 1.000000000000000000, 0.000000000000000000, 0.000000000000000000 ) ) ;
#21288 = CARTESIAN_POINT ( 'NONE',  ( 3.313708498984762052, -13.90625000409677092, -8.000000000000000000 ) ) ;
#21289 = CARTESIAN_POINT ( 'NONE',  ( -46.57764780881405642, -28.81936281876300754, 41.83085013884056735 ) ) ;
#21290 = CARTESIAN_POINT ( 'NONE',  ( 9.240220675753558766, 15.98931925350938243, 3.827754797006297505 ) ) ;
#21291 = CIRCLE ( 'NONE', #79838, 3.309500000000001663 ) ;
#21292 = DIRECTION ( 'NONE',  ( 0.000000000000000000, 0.000000000000000000, -1.000000000000000000 ) ) ;
#21293 = B_SPLINE_CURVE_WITH_KNOTS ( 'NONE', 3,
 ( #37428, #35834, #102656, #28815 ),
 .UNSPECIFIED., .F., .F.,
 ( 4, 4 ),
 ( 0.000000000000000000, 0.001831984915194361310 ),
 .UNSPECIFIED. ) ;
#21294 = CARTESIAN_POINT ( 'NONE',  ( 7.500000000000003553, 11.93422428098184263, -34.62196993281244062 ) ) ;
#21295 = CARTESIAN_POINT ( 'NONE',  ( 5.122460025286957652, 51.37854414394068669, 8.531152949374495975 ) ) ;
#21296 = AXIS2_PLACEMENT_3D ( 'NONE', #94791, #4170, #37102 ) ;
#21297 = DIRECTION ( 'NONE',  ( -1.000000000000000000, 0.000000000000000000, 0.000000000000000000 ) ) ;
#21298 = EDGE_LOOP ( 'NONE', ( #74131, #39104, #80104, #56121, #77221, #56805 ) ) ;
#21299 = CARTESIAN_POINT ( 'NONE',  ( -3.015909229672554037, -49.46458095252987874, 44.28828481597984990 ) ) ;
#21300 = CARTESIAN_POINT ( 'NONE',  ( 26.36650669486618881, 4.000000000000003553, 4.898587196589414801E-16 ) ) ;
#21301 = CONICAL_SURFACE ( 'NONE', #81512, 3.309500000000001663, 0.9599310885968770357 ) ;
#21302 = CARTESIAN_POINT ( 'NONE',  ( -2.455881507267896779, 14.68468481912377754, -6.558993639549812293 ) ) ;
#21303 = CARTESIAN_POINT ( 'NONE',  ( 67.85746092694749620, -30.20841432806020421, -30.53995510508960720 ) ) ;
#21304 = CARTESIAN_POINT ( 'NONE',  ( -81.04558864123690398, -30.00000000000000711, 140.2587397602939348 ) ) ;
#21305 = CARTESIAN_POINT ( 'NONE',  ( -19.99999999999999289, -4.000000000000000000, 25.00000000000000000 ) ) ;
#21306 = ORIENTED_EDGE ( 'NONE', *, *, #74149, .T. ) ;
#21307 = CARTESIAN_POINT ( 'NONE',  ( 0.9999999999999954481, -50.00000000000000000, 44.97220075561143204 ) ) ;
#21308 = CARTESIAN_POINT ( 'NONE',  ( 83.92145523934827622, -57.54641214311970998, 201.7057418963653959 ) ) ;
#21309 = CARTESIAN_POINT ( 'NONE',  ( 66.60435403501256246, -60.22831153350267641, -27.67107985133044679 ) ) ;
#21310 = ADVANCED_FACE ( 'NONE', ( #74395 ), #81673, .F. ) ;
#21311 = CARTESIAN_POINT ( 'NONE',  ( -5.727634848076409213, -4.575561887447700649, -6.326622577870337771 ) ) ;
#21312 = CARTESIAN_POINT ( 'NONE',  ( -16.10528882106922310, 21.79591095385115906, 1.082486061764422081 ) ) ;
#21313 = CARTESIAN_POINT ( 'NONE',  ( 9.999999999999998224, -3.000000000000002665, -83.69100306100429520 ) ) ;
#21314 = CARTESIAN_POINT ( 'NONE',  ( -50.42178165167939596, -60.00000000000000711, 72.86386456530777878 ) ) ;
#21315 = CARTESIAN_POINT ( 'NONE',  ( -2.241046694639150960, 6.576374040526485665, -6.171384342982733529 ) ) ;
#21316 = DIRECTION ( 'NONE',  ( 1.000000000000000000, -0.000000000000000000, -0.000000000000000000 ) ) ;
#21317 = CARTESIAN_POINT ( 'NONE',  ( -11.54772599577038505, 50.00000000000000000, 62.20121126512094634 ) ) ;
#21318 = CARTESIAN_POINT ( 'NONE',  ( -86.39403411959629864, -17.39645492706551622, 179.4242455222010335 ) ) ;
#21320 = ORIENTED_EDGE ( 'NONE', *, *, #59750, .T. ) ;
#21319 = STYLED_ITEM ( 'NONE', ( #83447 ), #17300 ) ;
#21321 = CARTESIAN_POINT ( 'NONE',  ( 36.62596431772431060, 370.5219051594085045, 4.028350488951735642 ) ) ;
#21322 = CARTESIAN_POINT ( 'NONE',  ( -19.36103579130787367, 294.6347466944262692, -10.04613669444748680 ) ) ;
#21323 = CARTESIAN_POINT ( 'NONE',  ( -5.448357726063037809, 41.97585548067615235, -59.38396255182521344 ) ) ;
#21324 = DIRECTION ( 'NONE',  ( 2.855347482703417278E-17, -0.7561819230137100112, -0.6543614439339221489 ) ) ;
#21325 = CIRCLE ( 'NONE', #95362, 3.000000000000017764 ) ;
#21326 = CARTESIAN_POINT ( 'NONE',  ( 11.33049201284865859, -4.963977770831442982, -77.06423821557504539 ) ) ;
#21327 = CARTESIAN_POINT ( 'NONE',  ( -20.70564462400559336, 303.8824169543686367, -9.993494645898625350 ) ) ;
#21328 = CARTESIAN_POINT ( 'NONE',  ( -82.43052579600562524, -37.77911483926543923, -12.82222265178975462 ) ) ;
#21329 = CARTESIAN_POINT ( 'NONE',  ( 48.02835407290504577, 9.771516447483525880, -16.85535821593549954 ) ) ;
#21330 = LINE ( 'NONE', #39088, #10348 ) ;
#21331 = CIRCLE ( 'NONE', #35105, 5.000000000000001776 ) ;
#21332 = ORIENTED_EDGE ( 'NONE', *, *, #62915, .F. ) ;
#21333 = CARTESIAN_POINT ( 'NONE',  ( 18.12552907611484443, 50.00000000000002132, 61.72817625373181016 ) ) ;
#21334 = CARTESIAN_POINT ( 'NONE',  ( 13.39322541715468162, 24.41533748129609549, 2.568124331425434725 ) ) ;
#21335 = CARTESIAN_POINT ( 'NONE',  ( -3.301606509414339641, -4.285714285714286476, -25.22241582816893413 ) ) ;
#21336 = CARTESIAN_POINT ( 'NONE',  ( 86.55961277372783513, -14.21045842199431597, 7.754469001180375187 ) ) ;
#21337 = CARTESIAN_POINT ( 'NONE',  ( -82.19152542213547008, -22.15616930489894187, 140.5469334434418727 ) ) ;
#21338 = VERTEX_POINT ( 'NONE', #53332 ) ;
#21339 = DIRECTION ( 'NONE',  ( -1.000000000000000000, -1.224606353822377258E-16, -0.000000000000000000 ) ) ;
#21340 = LINE ( 'NONE', #38062, #31674 ) ;
#21341 = CARTESIAN_POINT ( 'NONE',  ( 73.76777583395416116, -57.62289582277519884, 185.9891449441927307 ) ) ;
#21342 = CARTESIAN_POINT ( 'NONE',  ( 37.18367258770028627, 50.00000000000001421, 51.09969904534472107 ) ) ;
#21343 = CARTESIAN_POINT ( 'NONE',  ( 36.06705365364255300, 330.6635994761463166, -3.195544000931108908 ) ) ;
#21344 = EDGE_CURVE ( 'NONE', #58101, #82907, #34525, .T. ) ;
#21345 = DIRECTION ( 'NONE',  ( -0.000000000000000000, -1.000000000000000000, -0.000000000000000000 ) ) ;
#21346 = ORIENTED_EDGE ( 'NONE', *, *, #22619, .T. ) ;
#21347 = CARTESIAN_POINT ( 'NONE',  ( -32.28930913497458022, 488.2717154064632723, 9.213726894912692700 ) ) ;
#21348 = CARTESIAN_POINT ( 'NONE',  ( 7.500000000000006217, 39.99999999999942446, -59.88032989331673406 ) ) ;
#21349 = DIRECTION ( 'NONE',  ( 0.5735764363510462704, 0.8191520442889915765, 0.000000000000000000 ) ) ;
#21350 = CARTESIAN_POINT ( 'NONE',  ( -1.320432766682874540E-15, -22.53125000204838457, 7.188101187500000044 ) ) ;
#21351 = ORIENTED_EDGE ( 'NONE', *, *, #32136, .F. ) ;
#21352 = CARTESIAN_POINT ( 'NONE',  ( -21.19348424345033521, 294.8901562694577478, 1.945151701991089332 ) ) ;
#21354 = EDGE_CURVE ( 'NONE', #70423, #64859, #40206, .T. ) ;
#21353 = LINE ( 'NONE', #30494, #42901 ) ;
#21355 = CARTESIAN_POINT ( 'NONE',  ( 7.149999999999997691, 41.65000000000000568, -59.82695526683420439 ) ) ;
#21356 = LINE ( 'NONE', #14273, #18732 ) ;
#21357 = CARTESIAN_POINT ( 'NONE',  ( 6.999999999999998224, -13.84208359229911345, -5.811937548932195163 ) ) ;
#21358 = CARTESIAN_POINT ( 'NONE',  ( -36.53813723229947641, 463.3027015936762041, 20.13340496300980931 ) ) ;
#21359 = ORIENTED_EDGE ( 'NONE', *, *, #67931, .T. ) ;
#21360 = CARTESIAN_POINT ( 'NONE',  ( 11.11919979409320014, -59.99999999999998579, -42.37939734519866875 ) ) ;
#21362 = CARTESIAN_POINT ( 'NONE',  ( 27.03795841298799374, -32.52614811046257870, 31.02465613286181068 ) ) ;
#21361 = CARTESIAN_POINT ( 'NONE',  ( -67.17213121490354411, -60.00000000000000000, 138.9710117141604826 ) ) ;
#21363 = CARTESIAN_POINT ( 'NONE',  ( -1.446302031375384789E-15, 60.76237703744687479, 11.80995232570204045 ) ) ;
#21364 = ORIENTED_EDGE ( 'NONE', *, *, #22767, .F. ) ;
#21365 = UNCERTAINTY_MEASURE_WITH_UNIT (LENGTH_MEASURE( 1.000000000000000082E-05 ), #63511, 'distance_accuracy_value', 'NONE');
#21366 = VERTEX_POINT ( 'NONE', #92175 ) ;
#21367 = CARTESIAN_POINT ( 'NONE',  ( -11.17734400176825993, -4.285714285714295357, -22.67073868809949744 ) ) ;
#21368 = CARTESIAN_POINT ( 'NONE',  ( 71.61875643530994751, -38.00000000000000000, -21.68328091587414264 ) ) ;
#21369 =( NAMED_UNIT ( * ) PLANE_ANGLE_UNIT ( ) SI_UNIT ( $, .RADIAN. ) );
#21370 = AXIS2_PLACEMENT_3D ( 'NONE', #29282, #36838, #102598 ) ;
#21371 = DIRECTION ( 'NONE',  ( -1.000000000000000000, -1.224606353822377258E-16, -0.000000000000000000 ) ) ;
#21372 = CARTESIAN_POINT ( 'NONE',  ( -16.10173312979620164, 5.477053992178055886, 4.739458514423359858 ) ) ;
#21373 = ORIENTED_EDGE ( 'NONE', *, *, #70412, .T. ) ;
#21374 = DIRECTION ( 'NONE',  ( 1.000000000000000000, 0.000000000000000000, 0.000000000000000000 ) ) ;
#21375 = CARTESIAN_POINT ( 'NONE',  ( 86.61592898532583717, -30.00000000000007461, 182.1137437502129046 ) ) ;
#21376 = CARTESIAN_POINT ( 'NONE',  ( -13.02156499116019894, 23.73570805843572273, -4.328872242394949943 ) ) ;
#21377 = ADVANCED_FACE ( 'NONE', ( #75998 ), #29854, .F. ) ;
#21378 = CARTESIAN_POINT ( 'NONE',  ( 0.000000000000000000, 51.11204936430951307, -27.84083606136722366 ) ) ;
#21379 = CARTESIAN_POINT ( 'NONE',  ( 81.59414243538543587, -30.00000000000000355, -6.877237798308948769 ) ) ;
#21380 = AXIS2_PLACEMENT_3D ( 'NONE', #35680, #43202, #101960 ) ;
#21381 = LINE ( 'NONE', #94730, #43274 ) ;
#21382 = ORIENTED_EDGE ( 'NONE', *, *, #41169, .F. ) ;
#21383 = ORIENTED_EDGE ( 'NONE', *, *, #12795, .T. ) ;
#21384 = B_SPLINE_CURVE_WITH_KNOTS ( 'NONE', 3,
 ( #30911, #64839, #56178, #89118, #48103, #63793, #47577, #15215, #95618, #21759, #55650, #87533, #81004, #40033, #79423, #105818, #104223, #30371, #31958, #55134, #88063, #6056, #14143, #79945, #40558, #65369, #98262, #106335, #73976, #73441, #15749, #91259, #90175, #48633, #42685, #82069, #98780, #42147, #66424, #50241, #24416, #81517, #1130, #75582, #97717, #32499, #57254, #23883, #56726, #75032, #58887, #17369, #82615, #8717, #34637, #66975, #99854, #17900, #41625, #83144, #26028, #1679, #9241, #587, #7641, #57786, #89648, #99308, #24933, #41095, #58336, #16278 ),
 .UNSPECIFIED., .F., .F.,
 ( 4, 2, 2, 2, 2, 2, 2, 2, 2, 2, 2, 2, 2, 2, 2, 2, 2, 2, 2, 2, 2, 2, 2, 2, 2, 2, 2, 2, 2, 2, 2, 2, 2, 2, 2, 4 ),
 ( 0.7782500970722819877, 0.7790724996784590406, 0.7798949022846362045, 0.7815397074969903102, 0.7823621101031673630, 0.7831845127093445269, 0.7840069153155215798, 0.7848293179216986326, 0.7864741231340527383, 0.7881189283464068440, 0.7897637335587609497, 0.7914085387711150554, 0.7946981491958233779, 0.7979877596205315893, 0.8012773700452399117, 0.8045669804699481231, 0.8111462013193646570, 0.8177254221687813018, 0.8243046430181978357, 0.8308838638676143695, 0.8440423055664473262, 0.8572007472652803939, 0.8835176306629464182, 0.9098345140606124426, 0.9229929557594453993, 0.9361513974582784670, 0.9493098391571115346, 0.9558890600065279575, 0.9624682808559444913, 0.9690475017053610252, 0.9756267225547775590, 0.9789163329794857704, 0.9822059434041939818, 0.9854955538289023043, 0.9871403590412564100, 0.9887851642536105157 ),
 .UNSPECIFIED. ) ;
#21385 = ORIENTED_EDGE ( 'NONE', *, *, #100977, .F. ) ;
#21386 = CARTESIAN_POINT ( 'NONE',  ( -7.899999792244746466, 11.02739026146940127, 8.477105736121037793E-15 ) ) ;
#21387 = DIRECTION ( 'NONE',  ( -1.000000000000000000, -1.224606353822377258E-16, -0.000000000000000000 ) ) ;
#21388 = CARTESIAN_POINT ( 'NONE',  ( 35.45036406932566564, 436.3203772529585649, 5.179456583034234285 ) ) ;
#21389 = CARTESIAN_POINT ( 'NONE',  ( -43.67905695453814019, 391.1919955517727772, 15.78495246862232371 ) ) ;
#21390 =( NAMED_UNIT ( * ) PLANE_ANGLE_UNIT ( ) SI_UNIT ( $, .RADIAN. ) );
#21391 = CARTESIAN_POINT ( 'NONE',  ( -7.999912353029506207, -88.99982470603094953, -0.2691822806795012846 ) ) ;
#21392 = CARTESIAN_POINT ( 'NONE',  ( -10.00000000000000355, 15.00000000000000000, -10.00000000000000000 ) ) ;
#21393 = EDGE_LOOP ( 'NONE', ( #65544, #78137, #80168, #25293, #23870, #60961 ) ) ;
#21394 = CARTESIAN_POINT ( 'NONE',  ( -1.308996937483426715, 48.00000000000000000, -95.00000000000000000 ) ) ;
#21395 = ORIENTED_EDGE ( 'NONE', *, *, #34710, .F. ) ;
#21396 = CARTESIAN_POINT ( 'NONE',  ( 0.000000000000000000, 0.000000000000000000, 5.000000000000002665 ) ) ;
#21397 = CARTESIAN_POINT ( 'NONE',  ( -40.86966971611449395, 485.5857298029526419, -4.179518346797930661 ) ) ;
#21398 = CARTESIAN_POINT ( 'NONE',  ( -80.86886930798023343, -59.99999999999999289, 181.8382583209386212 ) ) ;
#21399 = CARTESIAN_POINT ( 'NONE',  ( 63.35320627527596571, -39.48236604681514450, 81.40631686326936745 ) ) ;
#21400 = ORIENTED_EDGE ( 'NONE', *, *, #97418, .T. ) ;
#21401 = CARTESIAN_POINT ( 'NONE',  ( 0.000000000000000000, 4.898587196589413815E-16, -4.000000000000000888 ) ) ;
#21402 = EDGE_CURVE ( 'NONE', #55161, #79135, #17818, .T. ) ;
#21403 = DIRECTION ( 'NONE',  ( 0.000000000000000000, 0.000000000000000000, -1.000000000000000000 ) ) ;
#21404 = CARTESIAN_POINT ( 'NONE',  ( -41.17613404335627081, 436.9855557163879212, 5.736539807628611598 ) ) ;
#21405 = CIRCLE ( 'NONE', #79940, 5.000000000000002665 ) ;
#21406 = ADVANCED_FACE ( 'NONE', ( #63019 ), #22996, .T. ) ;
#21407 = CARTESIAN_POINT ( 'NONE',  ( -9.736013035283027861, 51.35462565537034152, 2.350814639870274725 ) ) ;
#21408 = ORIENTED_EDGE ( 'NONE', *, *, #105099, .T. ) ;
#21409 = CARTESIAN_POINT ( 'NONE',  ( -7.000000000000000000, 8.572527594031471218E-16, -12.27439246179028309 ) ) ;
#21410 = CARTESIAN_POINT ( 'NONE',  ( -70.67923476944599770, -59.99999999999996447, -26.10759862510926510 ) ) ;
#21411 = EDGE_CURVE ( 'NONE', #21786, #12582, #7400, .T. ) ;
#21412 = CARTESIAN_POINT ( 'NONE',  ( 0.000000000000000000, 0.000000000000000000, -8.000000000000000000 ) ) ;
#21413 = FACE_OUTER_BOUND ( 'NONE', #80351, .T. ) ;
#21414 = CARTESIAN_POINT ( 'NONE',  ( 0.000000000000000000, 0.000000000000000000, -8.000000000000000000 ) ) ;
#21415 = CARTESIAN_POINT ( 'NONE',  ( 86.32949698655070847, -24.59755161587166938, 182.4574572108609516 ) ) ;
#21416 = DIRECTION ( 'NONE',  ( -1.000000000000000000, -1.224606353822377258E-16, -0.000000000000000000 ) ) ;
#21417 = CARTESIAN_POINT ( 'NONE',  ( -9.743481591712932044, 8.211523606034065281, 0.000000000000000000 ) ) ;
#21418 = CARTESIAN_POINT ( 'NONE',  ( 6.928203230275508773, -9.730690703044611922, -4.000000000000000000 ) ) ;
#21419 = CARTESIAN_POINT ( 'NONE',  ( 70.54732098882475100, -29.99999999999997868, -20.45443121223284777 ) ) ;
#21420 = DIRECTION ( 'NONE',  ( 0.5735764363510557073, -0.8191520442889850262, 1.003171929053516612E-16 ) ) ;
#21421 = CARTESIAN_POINT ( 'NONE',  ( 13.90371668366488400, -50.40548167538292290, 25.34313603510888413 ) ) ;
#21422 = CARTESIAN_POINT ( 'NONE',  ( 34.50115457526765539, 434.4752522064443383, 9.494722064492803426 ) ) ;
#21423 = CARTESIAN_POINT ( 'NONE',  ( -100.0855808037712364, -29.99999999999999645, 154.6059760397357365 ) ) ;
#21424 = B_SPLINE_CURVE_WITH_KNOTS ( 'NONE', 3,
 ( #77613, #69526, #5320, #86785, #53855 ),
 .UNSPECIFIED., .F., .F.,
 ( 4, 1, 4 ),
 ( 0.000000000000000000, 0.003752776749732567464, 0.007505553499465134927 ),
 .UNSPECIFIED. ) ;
#21425 = AXIS2_PLACEMENT_3D ( 'NONE', #58340, #34108, #8191 ) ;
#21426 = CARTESIAN_POINT ( 'NONE',  ( -36.87655955837857391, 438.2068510013161244, 3.933030107424709598 ) ) ;
#21427 = CARTESIAN_POINT ( 'NONE',  ( 19.23263920009527084, -57.67182620447307784, 42.11598537107099105 ) ) ;
#21428 = CARTESIAN_POINT ( 'NONE',  ( 22.61650669486618526, 1.474610560812782335E-15, 0.000000000000000000 ) ) ;
#21429 = EDGE_CURVE ( 'NONE', #19762, #36055, #21240, .T. ) ;
#21430 = FACE_OUTER_BOUND ( 'NONE', #51220, .T. ) ;
#21431 = CARTESIAN_POINT ( 'NONE',  ( -18.83603686460278936, 49.99999999999999289, 60.80789323821156955 ) ) ;
#21432 = DIRECTION ( 'NONE',  ( 0.9730146112117565860, 0.000000000000000000, 0.2307435077492631936 ) ) ;
#21433 = CIRCLE ( 'NONE', #49186, 3.000000000000002220 ) ;
#21434 = CARTESIAN_POINT ( 'NONE',  ( -46.00000000000000000, 461.8820044443818347, 11.41122057645802990 ) ) ;
#21435 = CONICAL_SURFACE ( 'NONE', #57565, 7.000000000000000000, 0.9599310885968753704 ) ;
#21436 = CARTESIAN_POINT ( 'NONE',  ( 11.81369408999756132, -16.55887885820839500, -34.65806031955098376 ) ) ;
#21437 = EDGE_CURVE ( 'NONE', #31791, #57731, #106566, .T. ) ;
#21438 = CARTESIAN_POINT ( 'NONE',  ( 26.08349330513380693, 1.593028355512270962E-15, 0.000000000000000000 ) ) ;
#21439 = AXIS2_PLACEMENT_3D ( 'NONE', #83375, #56960, #42384 ) ;
#21440 = CARTESIAN_POINT ( 'NONE',  ( -86.62109302441706404, -61.00656027186597186, 194.7265321822163457 ) ) ;
#21441 = ORIENTED_EDGE ( 'NONE', *, *, #17580, .F. ) ;
#21442 = CARTESIAN_POINT ( 'NONE',  ( 38.47428897412591198, 485.7788508071993760, -4.770630528148357641 ) ) ;
#21443 = CARTESIAN_POINT ( 'NONE',  ( 33.21174982057957692, 465.5907685032113363, 15.87814633359622540 ) ) ;
#21444 = CARTESIAN_POINT ( 'NONE',  ( -14.28891041865645661, -22.06856204435137059, 27.67569685217618058 ) ) ;
#21447 = ADVANCED_FACE ( 'NONE', ( #30675 ), #54904, .F. ) ;
#21446 = CARTESIAN_POINT ( 'NONE',  ( -39.75288494767817582, 438.7659461435675325, 23.14726008740691299 ) ) ;
#21445 = CARTESIAN_POINT ( 'NONE',  ( -85.82110451813760221, -59.99999999999992895, -14.40634215571435561 ) ) ;
#21448 = ORIENTED_EDGE ( 'NONE', *, *, #43266, .F. ) ;
#21449 = CARTESIAN_POINT ( 'NONE',  ( 15.72218280906591303, 5.595371698622046530, -6.516822309424127546 ) ) ;
#21450 = CARTESIAN_POINT ( 'NONE',  ( 43.41290683822508356, 487.0833545439620593, 7.569976829064907875 ) ) ;
#21451 = CARTESIAN_POINT ( 'NONE',  ( 43.58349330513380693, 4.898587196589405926E-16, -4.000000000000001776 ) ) ;
#21452 = DIRECTION ( 'NONE',  ( 0.000000000000000000, 1.000000000000000000, 0.000000000000000000 ) ) ;
#21453 = EDGE_LOOP ( 'NONE', ( #42985, #67379, #86534, #102278, #40101 ) ) ;
#21454 = PLANE ( 'NONE',  #49803 ) ;
#21455 = FILL_AREA_STYLE_COLOUR ( '', #72974 ) ;
#21457 = DIRECTION ( 'NONE',  ( 0.000000000000000000, 0.000000000000000000, -1.000000000000000000 ) ) ;
#21456 = CARTESIAN_POINT ( 'NONE',  ( 0.000000000000000000, 0.000000000000000000, 0.000000000000000000 ) ) ;
#21458 = DIRECTION ( 'NONE',  ( 0.000000000000000000, -1.000000000000000000, 0.000000000000000000 ) ) ;
#21459 = VERTEX_POINT ( 'NONE', #95917 ) ;
#21460 = AXIS2_PLACEMENT_3D ( 'NONE', #36153, #51746, #68489 ) ;
#21461 = ORIENTED_EDGE ( 'NONE', *, *, #81615, .F. ) ;
#21462 = CARTESIAN_POINT ( 'NONE',  ( -25.40811296394797125, 308.2121404732505425, 10.71478048255157312 ) ) ;
#21463 = ORIENTED_EDGE ( 'NONE', *, *, #83714, .T. ) ;
#21464 = SURFACE_STYLE_USAGE ( .BOTH. , #95331 ) ;
#21465 = CIRCLE ( 'NONE', #2492, 8.000000000000000000 ) ;
#21466 = EDGE_CURVE ( 'NONE', #23893, #9941, #79191, .T. ) ;
#21467 = CARTESIAN_POINT ( 'NONE',  ( 13.38090213880806978, -54.00000000000000711, 31.11721482942554928 ) ) ;
#21468 = SURFACE_SIDE_STYLE ('',( #19896 ) ) ;
#21469 = VERTEX_POINT ( 'NONE', #47347 ) ;
#21470 = AXIS2_PLACEMENT_3D ( 'NONE', #9975, #17559, #42878 ) ;
#21471 = FACE_OUTER_BOUND ( 'NONE', #90200, .T. ) ;
#21472 = CARTESIAN_POINT ( 'NONE',  ( -6.074379036182786962, 41.75280167827273203, -70.48890184034459594 ) ) ;
#21473 = STYLED_ITEM ( 'NONE', ( #28045 ), #16884 ) ;
#21474 = CARTESIAN_POINT ( 'NONE',  ( -80.67090657556497035, -59.99999999999261036, 200.2785666839474743 ) ) ;
#21475 = LINE ( 'NONE', #54310, #103076 ) ;
#21476 = CARTESIAN_POINT ( 'NONE',  ( 18.45572942341445000, -60.00000000000000000, 40.03357716053164239 ) ) ;
#21477 = CARTESIAN_POINT ( 'NONE',  ( -14.68326754034733739, -5.000000000000000888, -7.357674878908997407 ) ) ;
#21478 = CARTESIAN_POINT ( 'NONE',  ( -5.373715199254561981, 41.43915796864546053, -58.48990672293015081 ) ) ;
#21480 = CARTESIAN_POINT ( 'NONE',  ( 10.26626668568163403, -39.47268289290210674, 30.48008405508823415 ) ) ;
#21479 = CARTESIAN_POINT ( 'NONE',  ( -90.16416446821634167, -14.21045842199442077, 52.56827875477732448 ) ) ;
#21481 = ADVANCED_FACE ( 'NONE', ( #4246 ), #47353, .F. ) ;
#21482 = SURFACE_SIDE_STYLE ('',( #45729 ) ) ;
#21483 = CARTESIAN_POINT ( 'NONE',  ( -48.60191364056953489, -46.44422754269193376, 50.71984063344733329 ) ) ;
#21484 = CYLINDRICAL_SURFACE ( 'NONE', #59069, 4.000000000000002665 ) ;
#21485 = ORIENTED_EDGE ( 'NONE', *, *, #84552, .T. ) ;
#21486 = EDGE_CURVE ( 'NONE', #50381, #32861, #55654, .T. ) ;
#21487 = CARTESIAN_POINT ( 'NONE',  ( 40.36516081888879626, 459.8940149412731557, 1.928085546549638929 ) ) ;
#21488 = CARTESIAN_POINT ( 'NONE',  ( 17.73901163440294226, 36.76451030150755628, 22.27377543627835621 ) ) ;
#21489 = DIRECTION ( 'NONE',  ( 0.000000000000000000, -1.000000000000000000, 0.000000000000000000 ) ) ;
#21490 = ORIENTED_EDGE ( 'NONE', *, *, #87375, .F. ) ;
#21492 = B_SPLINE_CURVE_WITH_KNOTS ( 'NONE', 3,
 ( #17069, #92006, #66672, #75281, #17605, #18141, #50997, #8425, #1377, #8952 ),
 .UNSPECIFIED., .F., .F.,
 ( 4, 2, 2, 2, 4 ),
 ( 0.000000000000000000, 0.001993803085173304762, 0.003987606170346609524, 0.005981409255519914286, 0.007975212340693219049 ),
 .UNSPECIFIED. ) ;
#21491 = CARTESIAN_POINT ( 'NONE',  ( -15.43550796417891746, -5.411715871157647406, 14.00207068577347869 ) ) ;
#21493 = ORIENTED_EDGE ( 'NONE', *, *, #20157, .F. ) ;
#21494 = CARTESIAN_POINT ( 'NONE',  ( 88.16768356981283716, -29.99999999999916156, -16.73627450970226249 ) ) ;
#21495 = CARTESIAN_POINT ( 'NONE',  ( 0.000000000000000000, 44.00000000000000711, 0.000000000000000000 ) ) ;
#21496 = CARTESIAN_POINT ( 'NONE',  ( 6.731699451537835444, 41.74873278439808644, -59.11937199553665323 ) ) ;
#21497 = CARTESIAN_POINT ( 'NONE',  ( 29.83308852632731245, 41.99999999995888089, 51.76085035125569789 ) ) ;
#21498 = CARTESIAN_POINT ( 'NONE',  ( 99.78582084211559788, -30.00000000000000000, 186.6030678800591147 ) ) ;
#21499 = VECTOR ( 'NONE', #41353, 1000.000000000000000 ) ;
#21500 = CARTESIAN_POINT ( 'NONE',  ( 0.000000000000000000, 36.79151656018385097, -22.55262289886175964 ) ) ;
#21501 = ORIENTED_EDGE ( 'NONE', *, *, #7536, .T. ) ;
#21502 = AXIS2_PLACEMENT_3D ( 'NONE', #79705, #88348, #20998 ) ;
#21503 = ORIENTED_EDGE ( 'NONE', *, *, #95578, .T. ) ;
#21504 = VERTEX_POINT ( 'NONE', #24179 ) ;
#21505 = CARTESIAN_POINT ( 'NONE',  ( -27.71614854450405119, 36.65793962528498184, 7.705128702296750731 ) ) ;
#21506 = CARTESIAN_POINT ( 'NONE',  ( 29.34999999999999787, 3.309500000000003439, 4.052968581778167743E-16 ) ) ;
#21507 = CARTESIAN_POINT ( 'NONE',  ( 42.40769230769231513, 1.411358822780289120E-15, 0.000000000000000000 ) ) ;
#21508 = ORIENTED_EDGE ( 'NONE', *, *, #95673, .T. ) ;
#21509 = CARTESIAN_POINT ( 'NONE',  ( 29.66054107240687543, 1.482358050883964840E-15, 0.000000000000000000 ) ) ;
#21510 = ORIENTED_EDGE ( 'NONE', *, *, #56340, .F. ) ;
#21511 =( LENGTH_UNIT ( ) NAMED_UNIT ( * ) SI_UNIT ( .MILLI., .METRE. ) );
#21512 = CARTESIAN_POINT ( 'NONE',  ( 105.6313430892477356, -38.38280832454254465, 196.7987401768915845 ) ) ;
#21513 = CARTESIAN_POINT ( 'NONE',  ( 11.46758739460970133, 14.79966376039287823, 9.840969504964308001 ) ) ;
#21514 = VECTOR ( 'NONE', #95791, 999.9999999999998863 ) ;
#21515 = CARTESIAN_POINT ( 'NONE',  ( 82.50935014594617201, -37.85473763363789601, 17.02533865044420835 ) ) ;
#21516 = DIRECTION ( 'NONE',  ( 0.8660254037844382635, 0.5000000000000006661, 0.000000000000000000 ) ) ;
#21517 = COLOUR_RGB ( '', 0.31764706, 0.68627451, 0.89019608) ;
#21518 = CARTESIAN_POINT ( 'NONE',  ( 42.08346088162276999, 343.2171893020684479, 13.37295717174569099 ) ) ;
#21519 = CONICAL_SURFACE ( 'NONE', #95550, 4.250000000000000000, 0.9599310885968754814 ) ;
#21520 = CARTESIAN_POINT ( 'NONE',  ( 4.898587196589412829E-16, -24.31250000409677270, -8.000000000000000000 ) ) ;
#21521 =( GEOMETRIC_REPRESENTATION_CONTEXT ( 3 ) GLOBAL_UNCERTAINTY_ASSIGNED_CONTEXT ( ( #48415 ) ) GLOBAL_UNIT_ASSIGNED_CONTEXT ( ( #75956, #99698, #67869 ) ) REPRESENTATION_CONTEXT ( 'NONE', 'WORKASPACE' ) );
#21522 = CARTESIAN_POINT ( 'NONE',  ( 26.84999999999999787, 1.533819458162526451E-15, 0.000000000000000000 ) ) ;
#21523 = CIRCLE ( 'NONE', #98920, 4.000000000000007105 ) ;
#21524 = CIRCLE ( 'NONE', #14609, 5.000000000000010658 ) ;
#21525 = VERTEX_POINT ( 'NONE', #41387 ) ;
#21526 = EDGE_CURVE ( 'NONE', #91723, #59944, #83237, .T. ) ;
#21527 = CARTESIAN_POINT ( 'NONE',  ( 0.000000000000000000, -30.00000000000000000, 8.000000000000000000 ) ) ;
#21528 = CARTESIAN_POINT ( 'NONE',  ( 15.41108395495531269, 43.84921856205087209, -89.31326237052935824 ) ) ;
#21529 = CARTESIAN_POINT ( 'NONE',  ( -2.861889033126343573, 85.75214027433212038, 4.999999999999998224 ) ) ;
#21530 = EDGE_LOOP ( 'NONE', ( #69089, #57750, #66040, #48114 ) ) ;
#21531 = DIRECTION ( 'NONE',  ( 1.000000000000000000, 0.000000000000000000, -0.000000000000000000 ) ) ;
#21532 = CARTESIAN_POINT ( 'NONE',  ( -29.45300615175912284, 297.5885148576093115, 2.537559088144822006 ) ) ;
#21533 = CARTESIAN_POINT ( 'NONE',  ( 0.5805565836007654523, 7.505553499465139389, 1.865978384307260116E-16 ) ) ;
#21534 = CARTESIAN_POINT ( 'NONE',  ( -3.313708498984760720, -24.03124999999999645, -8.000000000000000000 ) ) ;
#21535 = CARTESIAN_POINT ( 'NONE',  ( -43.25590865262737594, -38.30618195179057039, 54.80721966442113313 ) ) ;
#21536 = EDGE_CURVE ( 'NONE', #12685, #1846, #49468, .T. ) ;
#21537 = CARTESIAN_POINT ( 'NONE',  ( 41.17613404335629212, 436.9855557163879780, 5.736539807628617815 ) ) ;
#21538 = EDGE_LOOP ( 'NONE', ( #34058, #24245, #16317, #90718, #30531, #20766 ) ) ;
#21539 = CARTESIAN_POINT ( 'NONE',  ( 83.43191453633141919, -53.72065295603601953, 187.4671049082887464 ) ) ;
#21540 = CARTESIAN_POINT ( 'NONE',  ( -49.22180010227538105, 7.740565218139797032, 15.98496799241658550 ) ) ;
#21541 = CARTESIAN_POINT ( 'NONE',  ( 56.22793774957824553, 6.975173280561618775E-15, 0.000000000000000000 ) ) ;
#21542 = ORIENTED_EDGE ( 'NONE', *, *, #41496, .F. ) ;
#21543 = CARTESIAN_POINT ( 'NONE',  ( 94.06712173148491729, -57.67497447195143678, 4.449674835890252922 ) ) ;
#21544 = CARTESIAN_POINT ( 'NONE',  ( 5.947762761376478302, -2.501851166488387346, -6.500000000000002665 ) ) ;
#21545 = CARTESIAN_POINT ( 'NONE',  ( -11.46641754970919358, -5.000000000000002665, -75.26692388747306950 ) ) ;
#21546 = CARTESIAN_POINT ( 'NONE',  ( -29.86026515094337341, 12.86933730193438485, 39.60535821593512651 ) ) ;
#21547 =( BOUNDED_CURVE ( )  B_SPLINE_CURVE ( 2, ( #71945, #89198, #98340, #13695, #47655, #80550, #15296, #48183, #32036 ),
 .UNSPECIFIED., .F., .F. ) 
 B_SPLINE_CURVE_WITH_KNOTS ( ( 3, 2, 2, 2, 3 ),
 ( 0.9264705882352941568, 0.9338235294117647189, 0.9411764705882352811, 0.9485294117647057321, 0.9558823529411764053 ),
 .UNSPECIFIED. ) 
 CURVE ( )  GEOMETRIC_REPRESENTATION_ITEM ( )  RATIONAL_B_SPLINE_CURVE ( ( 1.000000000000000000, 0.9238795325112867385, 1.000000000000000000, 0.9238795325112867385, 1.000000000000000000, 0.9238795325112867385, 1.000000000000000000, 0.9238795325112878487, 0.9999999999999988898 ) ) 
 REPRESENTATION_ITEM ( '' )  );
#21548 = AXIS2_PLACEMENT_3D ( 'NONE', #77631, #4804, #77093 ) ;
#21549 = EDGE_CURVE ( 'NONE', #2695, #46619, #100480, .T. ) ;
#21550 = EDGE_CURVE ( 'NONE', #63024, #104720, #89970, .T. ) ;
#21551 = CARTESIAN_POINT ( 'NONE',  ( 51.88291765283141643, 335.6183258647025696, 267.1969486012846460 ) ) ;
#21552 = CARTESIAN_POINT ( 'NONE',  ( 7.992336736730297098, -19.45074496869593261, 35.23616762893431087 ) ) ;
#21553 = CARTESIAN_POINT ( 'NONE',  ( 45.26904958275400048, -28.38839725260003277, 40.36013178830350512 ) ) ;
#21555 = CARTESIAN_POINT ( 'NONE',  ( -12.52826048495583144, 20.76158922763902126, 6.344216544754339715 ) ) ;
#21554 = CARTESIAN_POINT ( 'NONE',  ( 37.48079164320805035, 473.0294839324634495, 17.43702840686824729 ) ) ;
#21556 = EDGE_CURVE ( 'NONE', #71103, #96068, #31725, .T. ) ;
#21557 = CARTESIAN_POINT ( 'NONE',  ( 7.196962703002473205, 302.2659962052679248, -10.02664813804953248 ) ) ;
#21558 = CARTESIAN_POINT ( 'NONE',  ( 43.66633623381847684, 409.2573964131182152, 16.13396782784120376 ) ) ;
#21559 = CARTESIAN_POINT ( 'NONE',  ( -42.87890296919689348, 485.5827577773663393, 6.686241925529927244 ) ) ;
#21560 = DIRECTION ( 'NONE',  ( 0.000000000000000000, -1.000000000000000000, 0.000000000000000000 ) ) ;
#21561 = ORIENTED_EDGE ( 'NONE', *, *, #47594, .T. ) ;
#21562 = CARTESIAN_POINT ( 'NONE',  ( -10.79486422923573485, -1.039336085533928422, 20.32133261175441774 ) ) ;
#21563 = CARTESIAN_POINT ( 'NONE',  ( 0.000000000000000000, 0.000000000000000000, 0.000000000000000000 ) ) ;
#21564 = CARTESIAN_POINT ( 'NONE',  ( 5.725004243152315375, -61.42480851744632986, -1.812899781754685913 ) ) ;
#21567 = EDGE_CURVE ( 'NONE', #23946, #25901, #59170, .T. ) ;
#21566 = CARTESIAN_POINT ( 'NONE',  ( 1.561251481115253359, -34.58958075603053572, -32.65459240829875398 ) ) ;
#21565 = FILL_AREA_STYLE_COLOUR ( '', #12255 ) ;
#21568 = EDGE_CURVE ( 'NONE', #49969, #12309, #45390, .T. ) ;
#21569 = CIRCLE ( 'NONE', #42235, 4.000000000000001776 ) ;
#21570 = EDGE_LOOP ( 'NONE', ( #67666, #76803 ) ) ;
#21571 = CARTESIAN_POINT ( 'NONE',  ( 0.3875187462253061321, 8.436519985394745902, -7.781689322727966207 ) ) ;
#21573 = B_SPLINE_CURVE_WITH_KNOTS ( 'NONE', 3,
 ( #14371, #24115, #72624, #81233, #65601, #15447, #47280, #82310, #32734, #7350, #8420, #56958, #96394, #31666, #64550, #40259, #7879, #32185, #22524, #23576, #89879, #81757, #40786, #73680, #98487, #106582, #88296, #24640 ),
 .UNSPECIFIED., .F., .F.,
 ( 4, 2, 2, 2, 2, 2, 2, 2, 2, 2, 2, 2, 2, 4 ),
 ( 6.362890571982298922E-17, 0.001872779778676164110, 0.002809169668014214073, 0.003745559557352264035, 0.004681949446690313564, 0.005618339336028363960, 0.006554729225366414357, 0.007491119114704463886, 0.009363898893380562943, 0.01030028878271861160, 0.01123667867205666027, 0.01217306856139470893, 0.01310945845073275759, 0.01498223822940885491 ),
 .UNSPECIFIED. ) ;
#21572 = DIRECTION ( 'NONE',  ( 0.000000000000000000, 1.000000000000000000, 0.000000000000000000 ) ) ;
#21574 = EDGE_LOOP ( 'NONE', ( #40666, #88295, #83170, #95130, #95720, #4596 ) ) ;
#21575 = CONICAL_SURFACE ( 'NONE', #52566, 4.000000000000001776, 0.9599310885968774798 ) ;
#21576 = CYLINDRICAL_SURFACE ( 'NONE', #17348, 4.000000000000000000 ) ;
#21577 = CARTESIAN_POINT ( 'NONE',  ( 74.56127108291157413, 6.975173280561618775E-15, 0.000000000000000000 ) ) ;
#21578 = B_SPLINE_CURVE_WITH_KNOTS ( 'NONE', 3,
 ( #52288, #44216, #77107, #44756, #3223, #69033, #28065, #77645 ),
 .UNSPECIFIED., .F., .F.,
 ( 4, 2, 2, 4 ),
 ( 6.071532165918824830E-18, 0.001701937957019037306, 0.003403875914038068540, 0.006807751828076084172 ),
 .UNSPECIFIED. ) ;
#21579 = VECTOR ( 'NONE', #42115, 1000.000000000000000 ) ;
#21580 = CARTESIAN_POINT ( 'NONE',  ( -92.61469415333380084, -60.00000000000000000, -10.15781130840770707 ) ) ;
#21581 = ORIENTED_EDGE ( 'NONE', *, *, #85346, .T. ) ;
#21582 = DIRECTION ( 'NONE',  ( 0.000000000000000000, -1.000000000000000000, 0.000000000000000000 ) ) ;
#21583 = AXIS2_PLACEMENT_3D ( 'NONE', #72656, #73709, #106613 ) ;
#21584 = SURFACE_STYLE_FILL_AREA ( #78708 ) ;
#21585 = STYLED_ITEM ( 'NONE', ( #61650 ), #56122 ) ;
#21586 = CARTESIAN_POINT ( 'NONE',  ( 13.09999999999999787, 1.533819458162526451E-15, 0.000000000000000000 ) ) ;
#21587 = VECTOR ( 'NONE', #64415, 1000.000000000000000 ) ;
#21588 = CARTESIAN_POINT ( 'NONE',  ( 67.96666666666666856, 3.309500000000014541, 0.000000000000000000 ) ) ;
#21589 = B_SPLINE_CURVE_WITH_KNOTS ( 'NONE', 3,
 ( #81359, #58161, #73267, #74861 ),
 .UNSPECIFIED., .F., .F.,
 ( 4, 4 ),
 ( 0.000000000000000000, 1.408790152747863330E-05 ),
 .UNSPECIFIED. ) ;
#21590 = CARTESIAN_POINT ( 'NONE',  ( -82.39333457580713116, -42.97489278574533955, 169.7347533911100470 ) ) ;
#21591 = ORIENTED_EDGE ( 'NONE', *, *, #82955, .T. ) ;
#21592 = AXIS2_PLACEMENT_3D ( 'NONE', #60357, #101328, #4222 ) ;
#21593 = CARTESIAN_POINT ( 'NONE',  ( -41.71840012517714769, 489.3048647944248728, 10.52957302900678904 ) ) ;
#21594 = VERTEX_POINT ( 'NONE', #24699 ) ;
#21595 = AXIS2_PLACEMENT_3D ( 'NONE', #95026, #44881, #21683 ) ;
#21596 = ORIENTED_EDGE ( 'NONE', *, *, #43997, .F. ) ;
#21597 = DIRECTION ( 'NONE',  ( 0.8191520442889881348, 0.000000000000000000, 0.5735764363510513775 ) ) ;
#21598 = ADVANCED_FACE ( 'NONE', ( #81821 ), #65667, .T. ) ;
#21599 = CARTESIAN_POINT ( 'NONE',  ( -1.401502055033657879, -70.62283062862942984, 13.06788351849044538 ) ) ;
#21600 = DIRECTION ( 'NONE',  ( 0.000000000000000000, 0.000000000000000000, -1.000000000000000000 ) ) ;
#21601 = VERTEX_POINT ( 'NONE', #41915 ) ;
#21602 = DIRECTION ( 'NONE',  ( -0.000000000000000000, -0.000000000000000000, -1.000000000000000000 ) ) ;
#21603 = CARTESIAN_POINT ( 'NONE',  ( -91.67701774657527380, -57.66167918384760327, -19.87712626951747552 ) ) ;
#21604 = CARTESIAN_POINT ( 'NONE',  ( -5.650483388624516046, -68.45566596850382268, 2.031129859422141415 ) ) ;
#21605 = DIRECTION ( 'NONE',  ( 0.000000000000000000, 0.000000000000000000, 1.000000000000000000 ) ) ;
#21606 = CARTESIAN_POINT ( 'NONE',  ( -9.165151389911683211, 104.7370448908366001, 4.000000000000002665 ) ) ;
#21607 = CARTESIAN_POINT ( 'NONE',  ( 0.000000000000000000, 1.502314598737159228E-15, -8.000000000000000000 ) ) ;
#21608 = DIRECTION ( 'NONE',  ( 0.000000000000000000, 0.000000000000000000, -1.000000000000000000 ) ) ;
#21609 = CARTESIAN_POINT ( 'NONE',  ( 77.20805073229469428, -29.99999999999999289, -26.53535389768476449 ) ) ;
#21610 = EDGE_CURVE ( 'NONE', #64980, #74552, #68187, .T. ) ;
#21611 = CARTESIAN_POINT ( 'NONE',  ( -60.31416392689769879, -59.99999999999997158, 109.8312514449790456 ) ) ;
#21612 = CARTESIAN_POINT ( 'NONE',  ( -56.66586820654334389, -18.67493726981144775, 55.37565512294952441 ) ) ;
#21613 = ORIENTED_EDGE ( 'NONE', *, *, #44870, .F. ) ;
#21614 = DIRECTION ( 'NONE',  ( -1.000000000000000000, -1.224606353822377258E-16, -0.000000000000000000 ) ) ;
#21615 = EDGE_LOOP ( 'NONE', ( #40767, #90007 ) ) ;
#21616 = CARTESIAN_POINT ( 'NONE',  ( -101.6828279354359665, -52.72024364583853639, 192.5462694633920648 ) ) ;
#21617 = DIRECTION ( 'NONE',  ( 0.000000000000000000, 0.000000000000000000, 1.000000000000000000 ) ) ;
#21618 = VERTEX_POINT ( 'NONE', #15514 ) ;
#21619 = CARTESIAN_POINT ( 'NONE',  ( 19.01543600231714493, 49.53930566124419244, 61.88648251802599987 ) ) ;
#21620 = CARTESIAN_POINT ( 'NONE',  ( -10.00000000000000178, 15.00000000000000000, 4.582575694955834500 ) ) ;
#21621 = CARTESIAN_POINT ( 'NONE',  ( -5.082755093536325042, -12.96875000204838280, -5.082755093536325930 ) ) ;
#21622 = EDGE_CURVE ( 'NONE', #102923, #16386, #55944, .T. ) ;
#21623 = CARTESIAN_POINT ( 'NONE',  ( -4.855126259300333480, -63.86661610792060628, 12.98872547890887574 ) ) ;
#21624 = DIRECTION ( 'NONE',  ( 0.5401002696853186569, -0.5464483025172026665, -0.6400671459791652529 ) ) ;
#21625 =( NAMED_UNIT ( * ) PLANE_ANGLE_UNIT ( ) SI_UNIT ( $, .RADIAN. ) );
#21626 = CARTESIAN_POINT ( 'NONE',  ( -30.55228927099183522, 298.7536840786443690, 10.80461237140096209 ) ) ;
#21627 = CARTESIAN_POINT ( 'NONE',  ( -8.031083489010908849, 46.98771334398849575, 0.000000000000000000 ) ) ;
#21628 = CARTESIAN_POINT ( 'NONE',  ( 4.460266806907394965, -48.83471559826429598, 104.3906379647731910 ) ) ;
#21629 = DIRECTION ( 'NONE',  ( -1.000000000000000000, -0.000000000000000000, -0.000000000000000000 ) ) ;
#21630 = B_SPLINE_CURVE_WITH_KNOTS ( 'NONE', 3,
 ( #20684, #38424, #61641, #14099, #103141, #47006, #95062, #96637, #44918, #62687, #103661, #77803, #36847, #62172, #53523, #71287, #29289, #3914, #63218, #29812 ),
 .UNSPECIFIED., .F., .F.,
 ( 4, 2, 2, 2, 2, 2, 2, 2, 2, 4 ),
 ( 0.003121586077445279335, 0.003625240300813460572, 0.004128894524181641809, 0.004632548747549822613, 0.005136202970918004283, 0.005639857194286185954, 0.005891684305970274621, 0.006143511417654363288, 0.006647165641022527612, 0.007150819864390691935 ),
 .UNSPECIFIED. ) ;
#21631 = CARTESIAN_POINT ( 'NONE',  ( -27.18871072888273943, -22.10006771587053720, 29.24485317054519484 ) ) ;
#21632 = ORIENTED_EDGE ( 'NONE', *, *, #97991, .T. ) ;
#21633 = ORIENTED_EDGE ( 'NONE', *, *, #50456, .F. ) ;
#21634 = CARTESIAN_POINT ( 'NONE',  ( 46.99422950215318195, -18.77626701132429332, 40.15805432195738689 ) ) ;
#21635 = CARTESIAN_POINT ( 'NONE',  ( 6.337538409676599689E-15, 7.746009256456446224, 51.75000000000000711 ) ) ;
#21636 = CARTESIAN_POINT ( 'NONE',  ( -6.481088301903609405, 16.00512455538761358, 2.652222390170979160 ) ) ;
#21637 = CARTESIAN_POINT ( 'NONE',  ( -105.5600001555610277, -38.38496021441782347, 196.8991584141934936 ) ) ;
#21638 = EDGE_LOOP ( 'NONE', ( #67416, #54472, #62585, #18465 ) ) ;
#21639 = CARTESIAN_POINT ( 'NONE',  ( 90.90468814451379842, -38.40428968624316752, -13.09899789428958883 ) ) ;
#21640 = SURFACE_STYLE_FILL_AREA ( #46421 ) ;
#21641 = DIRECTION ( 'NONE',  ( 0.000000000000000000, -1.000000000000000000, 0.000000000000000000 ) ) ;
#21642 = CARTESIAN_POINT ( 'NONE',  ( -42.70777704799414209, 431.8248371325450989, 18.68372644223032353 ) ) ;
#21643 =( NAMED_UNIT ( * ) SI_UNIT ( $, .STERADIAN. ) SOLID_ANGLE_UNIT ( ) );
#21644 = CARTESIAN_POINT ( 'NONE',  ( 5.255459937908828927, 41.40616594607992340, -70.76123423727798922 ) ) ;
#21645 = CARTESIAN_POINT ( 'NONE',  ( -32.15713331982922796, 435.6530683308595826, 19.42064546954540916 ) ) ;
#21646 = CARTESIAN_POINT ( 'NONE',  ( -2.478418403666082792E-15, -5.948846446048902337, 2.696295709017763276 ) ) ;
#21647 = CARTESIAN_POINT ( 'NONE',  ( -30.00000000000994405, 486.6562833505550998, 5.030808486074148433 ) ) ;
#21648 = CARTESIAN_POINT ( 'NONE',  ( 86.16588619706764973, -59.99999999999999289, 200.6625549664367441 ) ) ;
#21649 = CIRCLE ( 'NONE', #68106, 4.172000000000009479 ) ;
#21650 = FILL_AREA_STYLE_COLOUR ( '', #71504 ) ;
#21651 = VERTEX_POINT ( 'NONE', #72684 ) ;
#21652 = CARTESIAN_POINT ( 'NONE',  ( -30.73227349664980323, 297.9212584795371868, -9.326660378782543503 ) ) ;
#21653 = EDGE_CURVE ( 'NONE', #88418, #88217, #65895, .T. ) ;
#21654 = CARTESIAN_POINT ( 'NONE',  ( 72.11682663846713126, 4.000000000000014211, 0.000000000000000000 ) ) ;
#21655 = VECTOR ( 'NONE', #39286, 1000.000000000000000 ) ;
#21656 = CARTESIAN_POINT ( 'NONE',  ( -7.934203308536662114, 26.13299659982202883, 1.057099537198549877 ) ) ;
#21657 = VERTEX_POINT ( 'NONE', #3994 ) ;
#21659 = CARTESIAN_POINT ( 'NONE',  ( 0.000000000000000000, 0.000000000000000000, -7.131971428571428184 ) ) ;
#21658 = CARTESIAN_POINT ( 'NONE',  ( -90.58636909219461586, -38.34954571021286540, 13.76841356955266171 ) ) ;
#21660 = LINE ( 'NONE', #95519, #37459 ) ;
#21661 = CARTESIAN_POINT ( 'NONE',  ( 3.750000000000007105, 6.495190528383288253, 1.734723475976807094E-15 ) ) ;
#21662 = CARTESIAN_POINT ( 'NONE',  ( -7.188101187500000044, -15.78125000204838635, -8.802885111219163269E-16 ) ) ;
#21663 = MECHANICAL_DESIGN_GEOMETRIC_PRESENTATION_REPRESENTATION (  '', ( #57792 ), #90526 ) ;
#21664 = CARTESIAN_POINT ( 'NONE',  ( -2.617478844992371823, -5.000000000000002665, -75.26027323389158141 ) ) ;
#21665 = EDGE_CURVE ( 'NONE', #45998, #25171, #15640, .T. ) ;
#21666 = VECTOR ( 'NONE', #87892, 1000.000000000000000 ) ;
#21667 = AXIS2_PLACEMENT_3D ( 'NONE', #101057, #26161, #50896 ) ;
#21668 = DIRECTION ( 'NONE',  ( -1.000000000000000000, -0.000000000000000000, -0.000000000000000000 ) ) ;
#21669 = CIRCLE ( 'NONE', #102632, 5.000000000000002665 ) ;
#21671 = ORIENTED_EDGE ( 'NONE', *, *, #101985, .F. ) ;
#21670 = DIRECTION ( 'NONE',  ( -0.000000000000000000, 1.000000000000000000, -0.000000000000000000 ) ) ;
#21672 = CARTESIAN_POINT ( 'NONE',  ( 82.57334049262250630, -46.47784298928625901, 176.6328590447577369 ) ) ;
#21673 = CARTESIAN_POINT ( 'NONE',  ( 9.046057234714689699, 137.5248812442146971, -1.301042606982603940E-15 ) ) ;
#21674 = CONICAL_SURFACE ( 'NONE', #100851, 4.000000000000001776, 0.9599310885968808105 ) ;
#21675 = CARTESIAN_POINT ( 'NONE',  ( -38.28124992147791517, 438.9555075391706964, 23.36623646420498090 ) ) ;
#21676 = VERTEX_POINT ( 'NONE', #69789 ) ;
#21677 = CARTESIAN_POINT ( 'NONE',  ( -22.35039165680892381, 303.1532478080135320, -9.935478914023770258 ) ) ;
#21678 = CARTESIAN_POINT ( 'NONE',  ( 16.91717221323107978, 34.22367470353576380, 24.29879862547840474 ) ) ;
#21679 = CARTESIAN_POINT ( 'NONE',  ( 37.56673239365841255, 27.60449318992554169, -13.45617127781092215 ) ) ;
#21680 = CARTESIAN_POINT ( 'NONE',  ( 34.35000000000000142, 1.533819458162526451E-15, 0.000000000000000000 ) ) ;
#21681 = CARTESIAN_POINT ( 'NONE',  ( -34.53113281790295019, 42.66782721010052626, -63.02754100881575994 ) ) ;
#21682 = CIRCLE ( 'NONE', #18206, 2.999999999999982236 ) ;
#21683 = DIRECTION ( 'NONE',  ( 0.000000000000000000, 1.000000000000000000, 0.000000000000000000 ) ) ;
#21684 = ADVANCED_FACE ( 'NONE', ( #28845 ), #13118, .T. ) ;
#21685 = VERTEX_POINT ( 'NONE', #27781 ) ;
#21686 = CARTESIAN_POINT ( 'NONE',  ( -76.72318010411292732, -30.00000000000000711, -16.84941602192575516 ) ) ;
#21687 = CARTESIAN_POINT ( 'NONE',  ( 25.59999999999999787, 1.533819458162526451E-15, 0.000000000000000000 ) ) ;
#21689 = EDGE_CURVE ( 'NONE', #102866, #98734, #81520, .T. ) ;
#21688 = DIRECTION ( 'NONE',  ( -1.000000000000000000, -0.000000000000000000, -0.000000000000000000 ) ) ;
#21691 = CARTESIAN_POINT ( 'NONE',  ( -13.03515395759786877, 4.280348557850227387, -7.334716606105208925 ) ) ;
#21690 = PLANE ( 'NONE',  #94823 ) ;
#21692 = CARTESIAN_POINT ( 'NONE',  ( -2.977408999572654480, -16.62500000204838457, 7.188101187499999156 ) ) ;
#21693 = CARTESIAN_POINT ( 'NONE',  ( 0.000000000000000000, 0.000000000000000000, 0.000000000000000000 ) ) ;
#21694 = CARTESIAN_POINT ( 'NONE',  ( 9.742892617412987732, -5.000000000000000000, -2.583889972060940288 ) ) ;
#21695 = CONTEXT_DEPENDENT_SHAPE_REPRESENTATION ( #9443, #80427 ) ;
#21696 = EDGE_LOOP ( 'NONE', ( #58513, #11991 ) ) ;
#21697 = FILL_AREA_STYLE_COLOUR ( '', #26886 ) ;
#21698 = DIRECTION ( 'NONE',  ( 0.5735764363510470476, -0.8191520442889911324, 1.003171929053524007E-16 ) ) ;
#21699 = CARTESIAN_POINT ( 'NONE',  ( -5.435697248882358501, 5.410530404478980593, -4.999999999999999112 ) ) ;
#21700 = CARTESIAN_POINT ( 'NONE',  ( -5.693345022499886277, -3.000000000001474820, -71.09407784968050237 ) ) ;
#21701 = PLANE ( 'NONE',  #27708 ) ;
#21702 = VERTEX_POINT ( 'NONE', #4515 ) ;
#21703 =( LENGTH_UNIT ( ) NAMED_UNIT ( * ) SI_UNIT ( .MILLI., .METRE. ) );
#21704 = DIRECTION ( 'NONE',  ( -1.000000000000000000, -0.000000000000000000, -0.000000000000000000 ) ) ;
#21705 = ORIENTED_EDGE ( 'NONE', *, *, #69028, .T. ) ;
#21706 = CARTESIAN_POINT ( 'NONE',  ( 34.42407431220851066, 6.123233995736770227E-16, -5.000000000000002665 ) ) ;
#21707 = FILL_AREA_STYLE_COLOUR ( '', #27790 ) ;
#21708 = CARTESIAN_POINT ( 'NONE',  ( -42.31627492074115793, 39.52091083735819410, -49.87351597195841890 ) ) ;
#21709 = CARTESIAN_POINT ( 'NONE',  ( 6.222583235320747974, 4.088462131826499757, -6.499999999999999112 ) ) ;
#21710 = CARTESIAN_POINT ( 'NONE',  ( -112.1573604782814328, -60.00000000000000711, 176.8690052302545155 ) ) ;
#21711 = CARTESIAN_POINT ( 'NONE',  ( -10.00000000000000000, -15.00000000000000000, 10.00000000000000178 ) ) ;
#21712 = DIRECTION ( 'NONE',  ( -1.000000000000000000, -1.224606353822377258E-16, -0.000000000000000000 ) ) ;
#21713 = FACE_OUTER_BOUND ( 'NONE', #105377, .T. ) ;
#21714 = DIRECTION ( 'NONE',  ( 0.000000000000000000, 0.5000000000000016653, 0.8660254037844375974 ) ) ;
#21715 = CARTESIAN_POINT ( 'NONE',  ( -82.18871635490596361, -57.14381643118496612, 185.7790063223330321 ) ) ;
#21716 = CIRCLE ( 'NONE', #47539, 5.000000000000002665 ) ;
#21717 = CARTESIAN_POINT ( 'NONE',  ( 43.57271197750083758, 41.43538979188361537, -50.59742473857805578 ) ) ;
#21718 = ORIENTED_EDGE ( 'NONE', *, *, #42074, .F. ) ;
#21719 =( NAMED_UNIT ( * ) PLANE_ANGLE_UNIT ( ) SI_UNIT ( $, .RADIAN. ) );
#21720 = EDGE_CURVE ( 'NONE', #66543, #69600, #53597, .T. ) ;
#21722 = CARTESIAN_POINT ( 'NONE',  ( 4.472135954999578722, -65.00000000000000000, 4.000000000000002665 ) ) ;
#21721 = CIRCLE ( 'NONE', #83731, 7.999999999999989342 ) ;
#21723 = CARTESIAN_POINT ( 'NONE',  ( -85.24306519959390016, -52.70679759000483244, 22.59225849838333744 ) ) ;
#21724 = CARTESIAN_POINT ( 'NONE',  ( -32.01678793614195939, 487.4833407576300033, 8.028904756518427277 ) ) ;
#21725 = SURFACE_STYLE_USAGE ( .BOTH. , #37918 ) ;
#21726 = CARTESIAN_POINT ( 'NONE',  ( 8.441095186759753233, 123.9902009031629717, -5.000000000000000000 ) ) ;
#21727 =( LENGTH_UNIT ( ) NAMED_UNIT ( * ) SI_UNIT ( .MILLI., .METRE. ) );
#21728 = CARTESIAN_POINT ( 'NONE',  ( -19.32152200341433357, 18.64316884707570310, 33.52312678237270660 ) ) ;
#21729 = CARTESIAN_POINT ( 'NONE',  ( 100.7999351731576354, -29.99999999999990763, 198.8735152728553999 ) ) ;
#21730 = EDGE_CURVE ( 'NONE', #78936, #104803, #53978, .T. ) ;
#21731 = CARTESIAN_POINT ( 'NONE',  ( -91.01385585952614576, -29.99999999999999289, 38.60219201899132457 ) ) ;
#21732 = CARTESIAN_POINT ( 'NONE',  ( -63.70546524352059237, -49.91541863491629982, 87.81759370848021717 ) ) ;
#21733 = COLOUR_RGB ( '', 0.72549020, 0.75294118, 0.79215686) ;
#21734 = ORIENTED_EDGE ( 'NONE', *, *, #48186, .F. ) ;
#21735 = CARTESIAN_POINT ( 'NONE',  ( 64.12441025417933815, 39.42592377905895518, -11.04313413768638164 ) ) ;
#21736 = CARTESIAN_POINT ( 'NONE',  ( 100.3830179364247783, -59.99999999999631228, 204.2895793215106437 ) ) ;
#21737 = AXIS2_PLACEMENT_3D ( 'NONE', #50256, #100399, #75044 ) ;
#21739 = ORIENTED_EDGE ( 'NONE', *, *, #75897, .F. ) ;
#21738 = AXIS2_PLACEMENT_3D ( 'NONE', #72892, #9226, #73425 ) ;
#21740 = CARTESIAN_POINT ( 'NONE',  ( 14.11595029532508860, 2.410436752314647713, 5.024000119269133258 ) ) ;
#21742 = AXIS2_PLACEMENT_3D ( 'NONE', #29433, #47152, #96267 ) ;
#21741 = CARTESIAN_POINT ( 'NONE',  ( 7.188101187500000044, -18.03125000204838457, 0.000000000000000000 ) ) ;
#21743 = DIRECTION ( 'NONE',  ( 0.000000000000000000, 0.000000000000000000, -1.000000000000000000 ) ) ;
#21744 = ORIENTED_EDGE ( 'NONE', *, *, #81569, .T. ) ;
#21745 = CARTESIAN_POINT ( 'NONE',  ( 3.454253436624921569, -49.15858197120396511, 103.7259032015043090 ) ) ;
#21746 = ORIENTED_EDGE ( 'NONE', *, *, #63394, .T. ) ;
#21747 = CARTESIAN_POINT ( 'NONE',  ( 10.61273427954644077, 46.03711080233982500, -12.94042145964163204 ) ) ;
#21748 = CARTESIAN_POINT ( 'NONE',  ( -40.16087957073754211, 485.8454018306724720, -4.964645702805049687 ) ) ;
#21749 = CARTESIAN_POINT ( 'NONE',  ( -92.70901343235634329, -59.99999999999998579, -4.635296546728438827 ) ) ;
#21750 = CARTESIAN_POINT ( 'NONE',  ( 36.73048575021757500, 408.0658092706848947, 6.298725112593818842 ) ) ;
#21751 = CARTESIAN_POINT ( 'NONE',  ( -5.082755093536325042, -9.593750002048384573, -5.082755093536325930 ) ) ;
#21752 = EDGE_CURVE ( 'NONE', #78525, #23615, #28694, .T. ) ;
#21753 = CARTESIAN_POINT ( 'NONE',  ( 32.80551872593211726, 486.0171861992458844, 5.671217483528002923 ) ) ;
#21754 = CIRCLE ( 'NONE', #14857, 7.000000000000006217 ) ;
#21755 = CARTESIAN_POINT ( 'NONE',  ( 19.00223544648544305, -4.285714285714295357, 16.66764709352488083 ) ) ;
#21756 = CARTESIAN_POINT ( 'NONE',  ( 7.996668422908976837, 49.99999999999999289, -78.85453279918145597 ) ) ;
#21757 = CARTESIAN_POINT ( 'NONE',  ( -46.00000000000000711, 437.9209086209079373, 12.30656597848518885 ) ) ;
#21758 = DIRECTION ( 'NONE',  ( -0.000000000000000000, -1.000000000000000000, -0.000000000000000000 ) ) ;
#21759 = CARTESIAN_POINT ( 'NONE',  ( 101.5344860084426415, -60.00000000000007105, 194.6295455690923859 ) ) ;
#21760 = ORIENTED_EDGE ( 'NONE', *, *, #17702, .T. ) ;
#21761 = DIRECTION ( 'NONE',  ( 0.000000000000000000, 0.000000000000000000, 1.000000000000000000 ) ) ;
#21762 = CARTESIAN_POINT ( 'NONE',  ( 9.999999999999998224, 0.000000000000000000, -9.999999999999998224 ) ) ;
#21763 = CARTESIAN_POINT ( 'NONE',  ( 32.88952925475911115, -29.08932276880856804, 32.34176666536721712 ) ) ;
#21764 = CARTESIAN_POINT ( 'NONE',  ( -16.57301948837645256, -1.734723475976807094E-15, 4.453875240771298039 ) ) ;
#21765 = ORIENTED_EDGE ( 'NONE', *, *, #47265, .T. ) ;
#21766 = CARTESIAN_POINT ( 'NONE',  ( 8.099999999999999645, 3.752776749732561257, -6.499999999999999112 ) ) ;
#21767 = EDGE_LOOP ( 'NONE', ( #90185, #8955, #91485, #87159 ) ) ;
#21769 = CARTESIAN_POINT ( 'NONE',  ( -35.76320840016588676, 388.4727839510825333, 5.610592865731860002 ) ) ;
#21768 = CARTESIAN_POINT ( 'NONE',  ( 9.310717075081306859, -4.999999999999999112, -18.36753075048013528 ) ) ;
#21770 = DIRECTION ( 'NONE',  ( 1.000000000000000000, 0.000000000000000000, 0.000000000000000000 ) ) ;
#21771 = DIRECTION ( 'NONE',  ( -1.000000000000000000, -1.224606353822377258E-16, -0.000000000000000000 ) ) ;
#21772 = CARTESIAN_POINT ( 'NONE',  ( -41.81614247337329004, 436.2534677952782545, 7.171297734019188574 ) ) ;
#21773 = CARTESIAN_POINT ( 'NONE',  ( -49.19747204248731265, 12.91412732281234810, -16.05397513443227808 ) ) ;
#21774 = CARTESIAN_POINT ( 'NONE',  ( 7.894787914004607998, 1.238680740843649375E-13, -7.591390474663426424 ) ) ;
#21775 = VERTEX_POINT ( 'NONE', #78929 ) ;
#21776 = AXIS2_PLACEMENT_3D ( 'NONE', #94694, #69869, #12145 ) ;
#21777 = CARTESIAN_POINT ( 'NONE',  ( 101.2378610160001529, -59.99999999999999289, 88.29373084620047507 ) ) ;
#21778 = CARTESIAN_POINT ( 'NONE',  ( 28.35315596375243530, 34.20571024640019431, -8.697504746618690774 ) ) ;
#21779 = B_SPLINE_CURVE_WITH_KNOTS ( 'NONE', 3,
 ( #51365, #58409, #57856, #33099, #58947, #65964, #98845, #91321, #42751, #57325, #92351, #16897, #34163, #84276, #10372, #74577, #654, #33619, #9304, #67040, #26092, #1744 ),
 .UNSPECIFIED., .F., .F.,
 ( 4, 2, 2, 2, 2, 2, 2, 2, 2, 2, 4 ),
 ( 0.003152549850706256023, 0.003404493534967637219, 0.003656437219229017981, 0.004160324587751784708, 0.004664211956274550569, 0.005168099324797318164, 0.005671986693320084025, 0.006175874061842850753, 0.006679761430365617481, 0.006931705114627000411, 0.007183648798888385076 ),
 .UNSPECIFIED. ) ;
#21780 = DIRECTION ( 'NONE',  ( -0.000000000000000000, 0.000000000000000000, -1.000000000000000000 ) ) ;
#21781 = CARTESIAN_POINT ( 'NONE',  ( 0.000000000000000000, 0.000000000000000000, 4.000000000000000000 ) ) ;
#21782 = CARTESIAN_POINT ( 'NONE',  ( -12.67403057162867341, 18.60284021993737724, -8.290260067447448478 ) ) ;
#21783 = VERTEX_POINT ( 'NONE', #84909 ) ;
#21784 = ADVANCED_FACE ( 'NONE', ( #35865 ), #24753, .T. ) ;
#21785 = CARTESIAN_POINT ( 'NONE',  ( -83.82331579519006937, -29.99999999999999645, 159.3544112921956923 ) ) ;
#21786 = VERTEX_POINT ( 'NONE', #70848 ) ;
#21787 = DIRECTION ( 'NONE',  ( 0.000000000000000000, 1.000000000000000000, 0.000000000000000000 ) ) ;
#21788 =( NAMED_UNIT ( * ) SI_UNIT ( $, .STERADIAN. ) SOLID_ANGLE_UNIT ( ) );
#21789 = CARTESIAN_POINT ( 'NONE',  ( 28.58349330513380337, 4.000000000000003553, 0.000000000000000000 ) ) ;
#21790 = CARTESIAN_POINT ( 'NONE',  ( 14.77017712487585932, 22.74518112339139364, -2.603937284864370039 ) ) ;
#21791 = CARTESIAN_POINT ( 'NONE',  ( -6.499999999999999112, 3.752776749732556816, -0.7999999999999821698 ) ) ;
#21792 = CARTESIAN_POINT ( 'NONE',  ( -5.082755093536325042, -33.96875000204838813, -5.082755093536325930 ) ) ;
#21793 = CARTESIAN_POINT ( 'NONE',  ( 20.77592568779148863, 1.482358050883964840E-15, 0.000000000000000000 ) ) ;
#21795 = ADVANCED_FACE ( 'NONE', ( #14710 ), #79460, .T. ) ;
#21794 = SURFACE_STYLE_FILL_AREA ( #44998 ) ;
#21796 = ORIENTED_EDGE ( 'NONE', *, *, #1013, .F. ) ;
#21797 = APPLICATION_CONTEXT ( 'automotive_design' ) ;
#21799 = ORIENTED_EDGE ( 'NONE', *, *, #59004, .T. ) ;
#21798 = CARTESIAN_POINT ( 'NONE',  ( 0.000000000000000000, 0.000000000000000000, -12.97459999999999525 ) ) ;
#21800 = CARTESIAN_POINT ( 'NONE',  ( 78.12193372058688112, -56.83984770602898351, 152.8020783963501970 ) ) ;
#21801 = AXIS2_PLACEMENT_3D ( 'NONE', #60266, #77487, #83437 ) ;
#21802 = FILL_AREA_STYLE ('',( #95663 ) ) ;
#21803 = ORIENTED_EDGE ( 'NONE', *, *, #33055, .T. ) ;
#21804 = CARTESIAN_POINT ( 'NONE',  ( -12.50000000000000355, 27.16932851130122728, -44.70834376557844791 ) ) ;
#21805 = CARTESIAN_POINT ( 'NONE',  ( 7.151597709147949011, -86.78929265052215669, 3.587174531012140566 ) ) ;
#21806 = CARTESIAN_POINT ( 'NONE',  ( -5.082755093536325042, -21.59375000204838457, -5.082755093536325930 ) ) ;
#21807 = CARTESIAN_POINT ( 'NONE',  ( -5.651997800604014799, -57.67124204504380458, 41.59089347824649252 ) ) ;
#21808 = CARTESIAN_POINT ( 'NONE',  ( 9.965951495596808485, 294.6437651480115960, 1.892775183163956543 ) ) ;
#21809 = AXIS2_PLACEMENT_3D ( 'NONE', #104423, #88259, #65028 ) ;
#21810 = ADVANCED_FACE ( 'NONE', ( #88619 ), #6627, .F. ) ;
#21811 = ORIENTED_EDGE ( 'NONE', *, *, #49203, .T. ) ;
#21812 = CARTESIAN_POINT ( 'NONE',  ( -4.656749229489888897, -11.31760408126432083, -3.785628640239143028 ) ) ;
#21813 = CARTESIAN_POINT ( 'NONE',  ( -9.646083234704171616, 81.98709390976522116, -2.643797197754290007 ) ) ;
#21814 = CARTESIAN_POINT ( 'NONE',  ( 33.00000000000000000, 461.8163627757383551, 11.11111419091032460 ) ) ;
#21815 = AXIS2_PLACEMENT_3D ( 'NONE', #10703, #43617, #58754 ) ;
#21816 = CIRCLE ( 'NONE', #73414, 12.00000000000000711 ) ;
#21817 = CARTESIAN_POINT ( 'NONE',  ( 3.313708498984762052, -10.90625000409677270, -8.000000000000000000 ) ) ;
#21818 = STYLED_ITEM ( 'NONE', ( #91924 ), #23822 ) ;
#21819 = CARTESIAN_POINT ( 'NONE',  ( -35.72250249440244829, -24.40408281891684084, 33.76365376224248394 ) ) ;
#21820 = CIRCLE ( 'NONE', #32126, 3.981862520314373377 ) ;
#21821 = CARTESIAN_POINT ( 'NONE',  ( -36.57300281741547821, 26.05217144207286140, 11.44322539509465386 ) ) ;
#21822 = AXIS2_PLACEMENT_3D ( 'NONE', #105790, #64807, #23853 ) ;
#21823 = DIRECTION ( 'NONE',  ( 0.000000000000000000, 0.000000000000000000, 1.000000000000000000 ) ) ;
#21824 = EDGE_CURVE ( 'NONE', #19922, #16154, #43962, .T. ) ;
#21825 = CARTESIAN_POINT ( 'NONE',  ( 7.500000000006690648, 42.38482959929934424, -59.14603436866633501 ) ) ;
#21826 = CARTESIAN_POINT ( 'NONE',  ( -10.25013302800875437, -12.02071073709907445, 17.45400528659170192 ) ) ;
#21827 = EDGE_LOOP ( 'NONE', ( #5139, #38896, #98374, #59312 ) ) ;
#21828 = CIRCLE ( 'NONE', #4551, 8.142857142857131691 ) ;
#21829 = CARTESIAN_POINT ( 'NONE',  ( -3.082707893549554878, 15.00000000000006928, 9.999999999999859668 ) ) ;
#21830 = CIRCLE ( 'NONE', #75213, 11.27631144943088515 ) ;
#21831 = CARTESIAN_POINT ( 'NONE',  ( -0.2707382100857756990, 13.85270131633358837, -7.000000000000010658 ) ) ;
#21832 = CARTESIAN_POINT ( 'NONE',  ( 33.33710378954599207, -24.76289289388104464, -37.00238709877101684 ) ) ;
#21833 = CARTESIAN_POINT ( 'NONE',  ( -71.02231249463051199, -30.00000000000000000, 98.64568665504826583 ) ) ;
#21834 = DIRECTION ( 'NONE',  ( 0.000000000000000000, 0.000000000000000000, -1.000000000000000000 ) ) ;
#21835 = ORIENTED_EDGE ( 'NONE', *, *, #6541, .T. ) ;
#21836 = VECTOR ( 'NONE', #2235, 1000.000000000000000 ) ;
#21837 = CARTESIAN_POINT ( 'NONE',  ( 1.558897133830167814, -49.97004945637518603, 44.88304531907225225 ) ) ;
#21838 = CARTESIAN_POINT ( 'NONE',  ( 96.53708244649047288, -57.62217743364686839, 204.4821657146100051 ) ) ;
#21839 = CARTESIAN_POINT ( 'NONE',  ( 68.60688657586096895, -47.40901989918412340, -24.67624544561557087 ) ) ;
#21840 = CARTESIAN_POINT ( 'NONE',  ( -0.9108756637654614741, -6.979659189792516649, -6.219623095963290993 ) ) ;
#21841 = FACE_OUTER_BOUND ( 'NONE', #70, .T. ) ;
#21842 = DIRECTION ( 'NONE',  ( -1.000000000000000000, -1.224606353822377258E-16, -0.000000000000000000 ) ) ;
#21843 = PRODUCT_DEFINITION_SHAPE ( 'NONE', 'NONE',  #8033 ) ;
#21844 = CARTESIAN_POINT ( 'NONE',  ( -50.48252356805748775, -60.00000000000000711, 73.01728160295303383 ) ) ;
#21845 = CARTESIAN_POINT ( 'NONE',  ( 0.000000000000000000, 0.000000000000000000, 0.000000000000000000 ) ) ;
#21846 = CARTESIAN_POINT ( 'NONE',  ( 32.61650669486618881, 4.000000000000003553, 4.898587196589414801E-16 ) ) ;
#21847 = CARTESIAN_POINT ( 'NONE',  ( 65.26738680894031575, 49.99999999999999289, 0.8120011905333047730 ) ) ;
#21848 = AXIS2_PLACEMENT_3D ( 'NONE', #71438, #55251, #88175 ) ;
#21849 = CARTESIAN_POINT ( 'NONE',  ( -86.16350626793575884, -28.29804646221614206, 183.0077501213199298 ) ) ;
#21850 = VERTEX_POINT ( 'NONE', #46566 ) ;
#21851 = CARTESIAN_POINT ( 'NONE',  ( 33.19417746838672656, 318.2631342106616898, -6.512803730419179260 ) ) ;
#21852 = VECTOR ( 'NONE', #15737, 1000.000000000000000 ) ;
#21853 = CARTESIAN_POINT ( 'NONE',  ( 10.73176661990081371, 1.340359594676612611E-15, 0.000000000000000000 ) ) ;
#21854 = EDGE_CURVE ( 'NONE', #37936, #38119, #5571, .T. ) ;
#21855 = B_SPLINE_CURVE_WITH_KNOTS ( 'NONE', 3,
 ( #7997, #105631, #80285, #89467, #88932, #6398, #6934, #22636, #104571, #72728, #30724, #31771, #15560, #63612, #7454, #73247, #39333, #72213, #106151, #32839, #105115, #64652, #32307, #79765, #55471, #65180, #81871, #88408, #98073, #48974, #89987, #57073, #16095, #14479, #82960, #92643, #50566, #91596, #17707, #74324, #51108, #83482, #59767, #41433, #50050, #99122, #66783, #2560, #18801, #2029, #59233, #928, #76452, #100203, #9582, #74846, #33368, #67840, #8527, #51646, #43565, #99670, #1489, #91072, #58144, #401, #84568, #26368, #33913, #75392, #75929, #25288, #100730, #42496, #84025, #34453, #10648, #9055, #66237, #10131, #67323, #18249, #17179, #92106, #41963, #43041, #34977, #65717, #57595, #26892 ),
 .UNSPECIFIED., .F., .F.,
 ( 4, 2, 2, 2, 1, 1, 2, 2, 2, 2, 2, 2, 1, 2, 2, 1, 2, 2, 2, 1, 1, 2, 2, 1, 2, 2, 1, 1, 1, 2, 2, 1, 2, 2, 1, 1, 1, 2, 2, 1, 2, 2, 2, 1, 1, 1, 2, 2, 1, 2, 1, 1, 1, 2, 2, 4 ),
 ( 0.5023353322599047877, 0.5334393739936618140, 0.5489913948605402716, 0.5567674052939795004, 0.5606554105106991148, 0.5616274118148790739, 0.5621134124669689980, 0.5625994131190590331, 0.5645434157274189513, 0.5956474574611777539, 0.6111994783280572108, 0.6189754887614968837, 0.6228634939782167201, 0.6248074965865767494, 0.6257794978907567085, 0.6267514991949366676, 0.6889595826624540509, 0.7200636243962127425, 0.7356156452630919773, 0.7433916556965316502, 0.7472796609132515977, 0.7492236635216116269, 0.7501956648257915861, 0.7511676661299715452, 0.7822717078637267951, 0.7978237287306044756, 0.8055997391640433714, 0.8094877443807628747, 0.8114317469891225709, 0.8124037482933024190, 0.8128897489453923431, 0.8133757495974822671, 0.8444797913312427351, 0.8600318121981230801, 0.8678078226315633081, 0.8716958278482832556, 0.8736398304566432849, 0.8746118317608234660, 0.8750978324129135011, 0.8755838330650034251, 0.9066878747987620057, 0.9222398956656412405, 0.9300159060990808024, 0.9339039113158006389, 0.9358479139241604461, 0.9368199152283405162, 0.9373059158804304403, 0.9375489162064755133, 0.9377919165325204753, 0.9533439373993892740, 0.9611199478328236179, 0.9650079530495406788, 0.9669519556578993758, 0.9679239569620786687, 0.9688959582662579617, 1.000000000000000000 ),
 .UNSPECIFIED. ) ;
#21856 = CARTESIAN_POINT ( 'NONE',  ( -84.79560538139988068, -60.18951872861072161, -16.38072637616851779 ) ) ;
#21857 = PLANE ( 'NONE',  #106209 ) ;
#21858 = DIRECTION ( 'NONE',  ( 0.2284631855477637086, 0.3307511317731879896, 0.9156463627843030029 ) ) ;
#21859 = EDGE_LOOP ( 'NONE', ( #59590, #42573, #72784, #86621, #92699 ) ) ;
#21860 = CARTESIAN_POINT ( 'NONE',  ( 18.81234315776984900, 49.99999999999999289, 60.84005166012197208 ) ) ;
#21861 = CARTESIAN_POINT ( 'NONE',  ( 12.85196282309222227, 23.41805309023355974, 4.899702151067347522 ) ) ;
#21862 = EDGE_CURVE ( 'NONE', #59944, #38219, #59456, .T. ) ;
#21863 = CARTESIAN_POINT ( 'NONE',  ( 3.301606509414619861, -4.285714285714286476, 25.22241582816893413 ) ) ;
#21864 = DIRECTION ( 'NONE',  ( 0.000000000000000000, -1.000000000000000000, 0.000000000000000000 ) ) ;
#21865 = EDGE_CURVE ( 'NONE', #72256, #48691, #88098, .T. ) ;
#21866 = CARTESIAN_POINT ( 'NONE',  ( 75.59946810849663734, -59.99999999999992895, -32.85428466877961284 ) ) ;
#21867 = CARTESIAN_POINT ( 'NONE',  ( -78.94945067621699764, -42.96865013358673480, 142.9639642539773376 ) ) ;
#21868 = EDGE_LOOP ( 'NONE', ( #93724, #55952, #52632, #98002 ) ) ;
#21869 = CARTESIAN_POINT ( 'NONE',  ( 25.21823338009918203, -5.000000000000000000, 6.123233995736768255E-16 ) ) ;
#21870 = CARTESIAN_POINT ( 'NONE',  ( 3.733178250754431993, 42.00000000000000000, -68.31018313526459451 ) ) ;
#21871 = CARTESIAN_POINT ( 'NONE',  ( 86.82793481660095836, -57.58489263483398446, 203.0475982403202408 ) ) ;
#21872 = CARTESIAN_POINT ( 'NONE',  ( 47.93998421967890522, 50.00000000000002132, 40.89468907122802221 ) ) ;
#21873 = UNCERTAINTY_MEASURE_WITH_UNIT (LENGTH_MEASURE( 1.000000000000000082E-05 ), #52105, 'distance_accuracy_value', 'NONE');
#21874 = CARTESIAN_POINT ( 'NONE',  ( 30.82100972494468394, 309.0976561879820110, -8.562264960266007918 ) ) ;
#21875 = DIRECTION ( 'NONE',  ( 0.000000000000000000, 0.000000000000000000, 1.000000000000000000 ) ) ;
#21876 = VERTEX_POINT ( 'NONE', #47082 ) ;
#21877 = CARTESIAN_POINT ( 'NONE',  ( 7.499999999999999112, 1.854554393013827518, -0.1880126015361714420 ) ) ;
#21878 = CARTESIAN_POINT ( 'NONE',  ( 0.000000000000000000, -54.00000000000000711, 27.00000000000000000 ) ) ;
#21879 = FACE_OUTER_BOUND ( 'NONE', #5691, .T. ) ;
#21880 = CARTESIAN_POINT ( 'NONE',  ( -5.082755093536325042, -27.59375000204838457, -5.082755093536325930 ) ) ;
#21881 = EDGE_CURVE ( 'NONE', #48515, #101241, #47344, .T. ) ;
#21882 = ORIENTED_EDGE ( 'NONE', *, *, #35443, .T. ) ;
#21883 = CARTESIAN_POINT ( 'NONE',  ( 9.349999999999997868, 3.309500000000003439, 0.000000000000000000 ) ) ;
#21884 =( BOUNDED_SURFACE ( )  B_SPLINE_SURFACE ( 3, 2, ( 
 ( #16672, #7497, #97569 ),
 ( #16135, #99169, #106734 ),
 ( #8037, #8573, #58190 ),
 ( #49021, #56585, #106191 ),
 ( #39894, #65758, #66284 ),
 ( #50098, #98639, #65226 ),
 ( #973, #98118, #74363 ),
 ( #31813, #57642, #73840 ),
 ( #83003, #9098, #89508 ),
 ( #32883, #24267, #90563 ),
 ( #42006, #33955, #47958 ),
 ( #15602, #97054, #442 ),
 ( #81918, #23199, #74888 ),
 ( #40950, #81387, #80865 ),
 ( #6977, #72769, #105674 ),
 ( #1529, #68967, #19388 ),
 ( #60871, #101323, #35019 ),
 ( #77036, #100242, #101840 ),
 ( #85131, #2605, #93759 ),
 ( #25885, #66826, #43082 ),
 ( #100771, #26935, #91638 ),
 ( #34495, #9626, #19917 ),
 ( #27472, #75971, #17751 ),
 ( #67364, #51688, #10168 ),
 ( #28002, #10690, #60350 ),
 ( #93226, #51150, #50607 ),
 ( #43605, #3153, #84608 ),
 ( #99715, #35554, #58743 ) ),
 .UNSPECIFIED., .F., .F., .F. ) 
 B_SPLINE_SURFACE_WITH_KNOTS ( ( 4, 2, 2, 2, 2, 2, 2, 2, 2, 2, 2, 2, 2, 4 ),
 ( 3, 3 ),
 ( -1.788854400197697518E-05, 0.0008258451467760102556, 0.001669578837553997415, 0.002513312528331984683, 0.003357046219109971735, 0.004200779909887959220, 0.005044513600665946271, 0.006731980982221920373, 0.007575714672999907424, 0.008419448363777894476, 0.01010691574533386858, 0.01095064943611185650, 0.01179438312688984442, 0.01348185050844581852 ),
 ( 0.000000000000000000, 1.000000000000000000 ),
 .UNSPECIFIED. ) 
 GEOMETRIC_REPRESENTATION_ITEM ( )  RATIONAL_B_SPLINE_SURFACE ( (
 ( 1.000000000000000000, 1.000000000000000000, 1.000000000000000000),
 ( 1.000000000000000000, 1.000005597032284976, 1.000000000000000000),
 ( 1.000000000000000000, 0.9981174035053985705, 1.000000000000000000),
 ( 1.000000000000000000, 0.9910941550115122123, 1.000000000000000000),
 ( 1.000000000000000000, 0.9859587391819751856, 1.000000000000000000),
 ( 1.000000000000000000, 0.9732073139009395080, 1.000000000000000000),
 ( 1.000000000000000000, 0.9655956055815202443, 1.000000000000000000),
 ( 1.000000000000000000, 0.9487954604282968774, 1.000000000000000000),
 ( 1.000000000000000000, 0.9396125312366238047, 1.000000000000000000),
 ( 1.000000000000000000, 0.9205547400728270047, 1.000000000000000000),
 ( 1.000000000000000000, 0.9106598259483166258, 1.000000000000000000),
 ( 1.000000000000000000, 0.8910166268681486423, 1.000000000000000000),
 ( 1.000000000000000000, 0.8812839758754353880, 1.000000000000000000),
 ( 1.000000000000000000, 0.8530381836181091249, 1.000000000000000000),
 ( 1.000000000000000000, 0.8355499924272906664, 1.000000000000000000),
 ( 1.000000000000000000, 0.8121180734272108737, 1.000000000000000000),
 ( 1.000000000000000000, 0.8047528071544994832, 1.000000000000000000),
 ( 1.000000000000000000, 0.7908772856458535783, 1.000000000000000000),
 ( 1.000000000000000000, 0.7843397418763655704, 1.000000000000000000),
 ( 1.000000000000000000, 0.7662143347336847210, 1.000000000000000000),
 ( 1.000000000000000000, 0.7560053113360732935, 1.000000000000000000),
 ( 1.000000000000000000, 0.7426428230152902765, 1.000000000000000000),
 ( 1.000000000000000000, 0.7385160411530290459, 1.000000000000000000),
 ( 1.000000000000000000, 0.7308023910617710284, 1.000000000000000000),
 ( 1.000000000000000000, 0.7272503285417218910, 1.000000000000000000),
 ( 1.000000000000000000, 0.7174350756258216499, 1.000000000000000000),
 ( 1.000000000000000000, 0.7119478818699274125, 1.000000000000000000),
 ( 1.000000000000000000, 0.7071066567438195616, 1.000000000000000000) ) ) 
 REPRESENTATION_ITEM ( '' )  SURFACE ( )  );
#21885 = CARTESIAN_POINT ( 'NONE',  ( -5.656854249492381470, -23.56249999999999289, 5.656854249492379694 ) ) ;
#21886 = CARTESIAN_POINT ( 'NONE',  ( 0.6424259193445743810, 34.23289850721570104, 29.57547277752458470 ) ) ;
#21887 = CARTESIAN_POINT ( 'NONE',  ( 25.86712516739308398, 37.16009387618654358, 8.998664997537444421 ) ) ;
#21888 = CARTESIAN_POINT ( 'NONE',  ( 0.000000000000000000, 9.237604307034018802, 1.301042606982603546E-15 ) ) ;
#21889 = ORIENTED_EDGE ( 'NONE', *, *, #12577, .T. ) ;
#21890 = FACE_OUTER_BOUND ( 'NONE', #57544, .T. ) ;
#21891 = VECTOR ( 'NONE', #92777, 1000.000000000000000 ) ;
#21893 = CARTESIAN_POINT ( 'NONE',  ( 28.08999935184878893, -42.95675325573949266, 33.12999348514809839 ) ) ;
#21892 = CARTESIAN_POINT ( 'NONE',  ( -55.44100834966593538, -14.21045842199449361, 70.81055559928208254 ) ) ;
#21894 = CARTESIAN_POINT ( 'NONE',  ( 23.38404382908447943, 27.34872606290120700, -33.19783523858093588 ) ) ;
#21895 = VERTEX_POINT ( 'NONE', #7377 ) ;
#21896 = EDGE_LOOP ( 'NONE', ( #99585, #39872, #28176, #58849 ) ) ;
#21897 = CARTESIAN_POINT ( 'NONE',  ( -15.38541618194247285, -4.285714285714295357, -20.05453516056602581 ) ) ;
#21898 = CARTESIAN_POINT ( 'NONE',  ( -2.898330757982067934E-15, 60.00000000000000000, 23.66666666666665719 ) ) ;
#21899 = CARTESIAN_POINT ( 'NONE',  ( -43.72316710615100277, 464.1667603278365277, 8.066774506823993107 ) ) ;
#21900 = AXIS2_PLACEMENT_3D ( 'NONE', #99877, #17389, #1150 ) ;
#21901 = CIRCLE ( 'NONE', #64976, 4.000000000000000888 ) ;
#21902 = CARTESIAN_POINT ( 'NONE',  ( 6.162888688655346670, -3.752776749732575468, -6.499999999999999112 ) ) ;
#21903 = EDGE_LOOP ( 'NONE', ( #2621, #99341, #42255, #97070 ) ) ;
#21904 = CARTESIAN_POINT ( 'NONE',  ( 97.15356149169568312, 1.016364837396684119E-14, 0.000000000000000000 ) ) ;
#21905 = CARTESIAN_POINT ( 'NONE',  ( -13.40082383129016819, 24.42921809578557202, 2.579497271388879298 ) ) ;
#21906 = CARTESIAN_POINT ( 'NONE',  ( -82.57697026063134160, -41.66718125965567054, -14.02672778557674249 ) ) ;
#21907 =( GEOMETRIC_REPRESENTATION_CONTEXT ( 3 ) GLOBAL_UNCERTAINTY_ASSIGNED_CONTEXT ( ( #83660 ) ) GLOBAL_UNIT_ASSIGNED_CONTEXT ( ( #67984, #11314, #58289 ) ) REPRESENTATION_CONTEXT ( 'NONE', 'WORKASPACE' ) );
#21908 = CARTESIAN_POINT ( 'NONE',  ( 81.17160454977077677, -29.99999999999999289, 1.346216154707244428 ) ) ;
#21909 = CARTESIAN_POINT ( 'NONE',  ( 6.499999999999999112, -2.534234941938121821, -0.3584823952106133693 ) ) ;
#21910 = ORIENTED_EDGE ( 'NONE', *, *, #16379, .F. ) ;
#21911 = EDGE_LOOP ( 'NONE', ( #75512, #52087, #48912, #1634, #85450, #94840, #65198, #21076, #53714, #13880, #86234 ) ) ;
#21912 = VERTEX_POINT ( 'NONE', #81788 ) ;
#21913 = DIRECTION ( 'NONE',  ( -0.000000000000000000, -0.000000000000000000, 1.000000000000000000 ) ) ;
#21914 =( NAMED_UNIT ( * ) PLANE_ANGLE_UNIT ( ) SI_UNIT ( $, .RADIAN. ) );
#21915 = DIRECTION ( 'NONE',  ( 0.000000000000000000, -1.000000000000000000, 0.000000000000000000 ) ) ;
#21916 = LINE ( 'NONE', #79060, #75537 ) ;
#21917 = FILL_AREA_STYLE ('',( #29492 ) ) ;
#21918 = CARTESIAN_POINT ( 'NONE',  ( 0.2595206531158521512, 2.531175536751804067, -6.500000000000002665 ) ) ;
#21919 = ORIENTED_EDGE ( 'NONE', *, *, #49730, .F. ) ;
#21921 = ADVANCED_FACE ( 'NONE', ( #40816 ), #47834, .T. ) ;
#21920 = CARTESIAN_POINT ( 'NONE',  ( -7.996668422906947349, 48.00000000000000000, -78.85453279917602742 ) ) ;
#21922 = EDGE_LOOP ( 'NONE', ( #79654, #28457, #53511, #71468 ) ) ;
#21923 = DIRECTION ( 'NONE',  ( -0.000000000000000000, 1.000000000000000000, -0.000000000000000000 ) ) ;
#21924 = DIRECTION ( 'NONE',  ( 0.000000000000000000, -1.000000000000000000, 0.000000000000000000 ) ) ;
#21925 = LINE ( 'NONE', #30543, #16224 ) ;
#21926 = TOROIDAL_SURFACE ( 'NONE', #104566, 9.500000000000000000, 2.000000000000000000 ) ;
#21927 = FACE_OUTER_BOUND ( 'NONE', #94716, .T. ) ;
#21928 = CARTESIAN_POINT ( 'NONE',  ( 63.69280158076683307, -39.48211605329254326, 82.38451565384035291 ) ) ;
#21929 = VERTEX_POINT ( 'NONE', #40291 ) ;
#21930 = CARTESIAN_POINT ( 'NONE',  ( 41.86592229012135391, 465.6952443684891705, 15.31587819977333886 ) ) ;
#21931 = MECHANICAL_DESIGN_GEOMETRIC_PRESENTATION_REPRESENTATION (  '', ( #77011 ), #28963 ) ;
#21932 = CARTESIAN_POINT ( 'NONE',  ( -45.15185372570044819, -34.39553445584278535, -36.86152318962493979 ) ) ;
#21933 = CARTESIAN_POINT ( 'NONE',  ( -7.000182694785904047, 8.999680283969629713, 0.2646331733798830133 ) ) ;
#21934 = CARTESIAN_POINT ( 'NONE',  ( 30.00000000000000000, 1.102182119232617714E-15, -9.000000000000000000 ) ) ;
#21935 = VERTEX_POINT ( 'NONE', #80740 ) ;
#21936 = SURFACE_STYLE_FILL_AREA ( #95807 ) ;
#21937 =( LENGTH_UNIT ( ) NAMED_UNIT ( * ) SI_UNIT ( .MILLI., .METRE. ) );
#21938 = CARTESIAN_POINT ( 'NONE',  ( -4.789139187686886956, -60.00000000000000711, -36.83444369039217747 ) ) ;
#21939 = FACE_OUTER_BOUND ( 'NONE', #56542, .T. ) ;
#21940 = CARTESIAN_POINT ( 'NONE',  ( -3.313708498984760720, -27.21875000409677625, -8.000000000000000000 ) ) ;
#21941 = CARTESIAN_POINT ( 'NONE',  ( 0.000000000000000000, -5.000000000000000000, 10.00000000000000000 ) ) ;
#21942 = CARTESIAN_POINT ( 'NONE',  ( 85.66261666857552370, -61.05915153208074742, 194.0543246977708520 ) ) ;
#21943 = AXIS2_PLACEMENT_3D ( 'NONE', #41422, #106683, #17697 ) ;
#21944 = DIRECTION ( 'NONE',  ( 0.000000000000000000, 0.000000000000000000, 1.000000000000000000 ) ) ;
#21945 = EDGE_CURVE ( 'NONE', #42316, #85095, #55941, .T. ) ;
#21946 = AXIS2_PLACEMENT_3D ( 'NONE', #16061, #24717, #65145 ) ;
#21947 = CARTESIAN_POINT ( 'NONE',  ( -9.465790868195963270, 9.886732697601933850, 5.000000000000158984 ) ) ;
#21948 = SURFACE_SIDE_STYLE ('',( #46722 ) ) ;
#21949 = CARTESIAN_POINT ( 'NONE',  ( 18.57084990933715218, -18.11241891143331983, -33.93312537572241183 ) ) ;
#21950 = ORIENTED_EDGE ( 'NONE', *, *, #64272, .T. ) ;
#21951 = CARTESIAN_POINT ( 'NONE',  ( 13.45079846400082957, -53.73420772973362602, 23.11721482942554573 ) ) ;
#21952 = CARTESIAN_POINT ( 'NONE',  ( 34.77793752178678943, 435.8715891072652084, 8.130587104768295603 ) ) ;
#21953 = CARTESIAN_POINT ( 'NONE',  ( -99.75299316808613526, -30.00000000000000355, 151.3284628849059459 ) ) ;
#21954 = CONICAL_SURFACE ( 'NONE', #13282, 6.500000000000000000, 1.047197551196600296 ) ;
#21955 = CARTESIAN_POINT ( 'NONE',  ( 26.84999999999999787, 1.533819458162526451E-15, 0.000000000000000000 ) ) ;
#21956 = AXIS2_PLACEMENT_3D ( 'NONE', #35249, #50851, #84837 ) ;
#21957 = CARTESIAN_POINT ( 'NONE',  ( 43.07244424302177777, -57.68573873175960642, 61.15634709738809249 ) ) ;
#21959 = CARTESIAN_POINT ( 'NONE',  ( 43.75010090113823225, 464.8337800386758545, 11.75004750935514686 ) ) ;
#21958 = CARTESIAN_POINT ( 'NONE',  ( -1.484885661199817548E-13, 25.16821295365152622, -40.75000000000150635 ) ) ;
#21960 = CARTESIAN_POINT ( 'NONE',  ( -17.82614187044788778, 49.99999999999999289, 62.13962658379361415 ) ) ;
#21961 = FILL_AREA_STYLE ('',( #97392 ) ) ;
#21962 = CARTESIAN_POINT ( 'NONE',  ( 3.857142857142850545, -1.200583151104938517, 103.1763305333244318 ) ) ;
#21963 = PRESENTATION_LAYER_ASSIGNMENT (  '', '', ( #77062 ) ) ;
#21964 = AXIS2_PLACEMENT_3D ( 'NONE', #53641, #21842, #4567 ) ;
#21965 = FACE_BOUND ( 'NONE', #39520, .T. ) ;
#21966 = DIRECTION ( 'NONE',  ( 0.000000000000000000, 1.000000000000000000, 0.000000000000000000 ) ) ;
#21967 = CARTESIAN_POINT ( 'NONE',  ( -87.48428544808629681, -35.37239160489516365, 189.1147638953327998 ) ) ;
#21968 = EDGE_LOOP ( 'NONE', ( #10773, #36502, #81702, #30509, #18501 ) ) ;
#21969 = CARTESIAN_POINT ( 'NONE',  ( 39.04140135028778502, 485.1684443570251801, -4.294922607834593009 ) ) ;
#21970 = CARTESIAN_POINT ( 'NONE',  ( 70.89460441624491693, 6.975173280561618775E-15, 0.000000000000000000 ) ) ;
#21971 = CARTESIAN_POINT ( 'NONE',  ( -11.36750716639379988, -42.95774986353630709, 31.07752345680997408 ) ) ;
#21972 = AXIS2_PLACEMENT_3D ( 'NONE', #94120, #93599, #36983 ) ;
#21974 = CARTESIAN_POINT ( 'NONE',  ( 46.00000000000000000, 500.0000000000002274, -5.000000000000001776 ) ) ;
#21973 = CARTESIAN_POINT ( 'NONE',  ( -88.36736620956926913, -59.99999999999997158, 42.82440024210349350 ) ) ;
#21975 = EDGE_LOOP ( 'NONE', ( #51437, #32667, #94259, #61749, #96976 ) ) ;
#21976 = CARTESIAN_POINT ( 'NONE',  ( -43.69392749306696544, 464.9769837083814537, 8.436995239877180808 ) ) ;
#21977 =( NAMED_UNIT ( * ) PLANE_ANGLE_UNIT ( ) SI_UNIT ( $, .RADIAN. ) );
#21978 = CARTESIAN_POINT ( 'NONE',  ( 56.96666666666666856, 6.915964383211875250E-15, 0.000000000000000000 ) ) ;
#21979 = CARTESIAN_POINT ( 'NONE',  ( 15.43758579535049691, 2.782614627089976533, -1.951547078872143626 ) ) ;
#21980 = CARTESIAN_POINT ( 'NONE',  ( 71.68560605309247080, -60.00000000000000000, 151.9124196244835332 ) ) ;
#21981 = CARTESIAN_POINT ( 'NONE',  ( -41.58649125062324003, 315.0454808444952732, -5.157136739128146630 ) ) ;
#21982 = EDGE_LOOP ( 'NONE', ( #22752, #55926, #81246 ) ) ;
#21983 =( NAMED_UNIT ( * ) SI_UNIT ( $, .STERADIAN. ) SOLID_ANGLE_UNIT ( ) );
#21984 =( NAMED_UNIT ( * ) SI_UNIT ( $, .STERADIAN. ) SOLID_ANGLE_UNIT ( ) );
#21986 = CARTESIAN_POINT ( 'NONE',  ( 7.125691916903466705, 41.67430808309654822, -69.26730091920677523 ) ) ;
#21985 = DIRECTION ( 'NONE',  ( 1.000000000000000000, 0.000000000000000000, 0.000000000000000000 ) ) ;
#21988 = MECHANICAL_DESIGN_GEOMETRIC_PRESENTATION_REPRESENTATION (  '', ( #32302 ), #42590 ) ;
#21987 = DIRECTION ( 'NONE',  ( -1.000000000000000000, -1.224606353822377258E-16, -0.000000000000000000 ) ) ;
#21989 = FACE_OUTER_BOUND ( 'NONE', #45129, .T. ) ;
#21990 = ORIENTED_EDGE ( 'NONE', *, *, #54014, .F. ) ;
#21991 = ORIENTED_EDGE ( 'NONE', *, *, #81424, .F. ) ;
#21993 = CARTESIAN_POINT ( 'NONE',  ( -23.88426421104139763, 306.2535832371898437, 10.24728475601139976 ) ) ;
#21992 = STYLED_ITEM ( 'NONE', ( #95476 ), #102386 ) ;
#21994 = EDGE_CURVE ( 'NONE', #43519, #19141, #793, .T. ) ;
#21995 = ORIENTED_EDGE ( 'NONE', *, *, #66345, .F. ) ;
#21996 = EDGE_CURVE ( 'NONE', #57839, #45703, #47967, .T. ) ;
#21997 = CARTESIAN_POINT ( 'NONE',  ( -41.35836404316634685, 461.4284568614622231, 2.579347946915543588 ) ) ;
#21998 = ORIENTED_EDGE ( 'NONE', *, *, #95773, .F. ) ;
#21999 = CARTESIAN_POINT ( 'NONE',  ( -6.241999136123610015, 41.80321047224195041, -70.33316275629502456 ) ) ;
#22000 = CARTESIAN_POINT ( 'NONE',  ( -84.79750510667604146, -60.00000000000488853, 202.7836688792506550 ) ) ;
#22001 = CARTESIAN_POINT ( 'NONE',  ( 44.14489099987147824, 485.6019929922275082, 3.572971381548252889 ) ) ;
#22002 = CARTESIAN_POINT ( 'NONE',  ( 38.24823956341693076, -60.00000000000000000, 49.79050390885200272 ) ) ;
#22003 = CARTESIAN_POINT ( 'NONE',  ( 9.833493305133801599, -4.000000000000000000, 4.898587196589415787E-16 ) ) ;
#22004 = DIRECTION ( 'NONE',  ( -0.000000000000000000, -1.000000000000000000, -0.000000000000000000 ) ) ;
#22006 = CARTESIAN_POINT ( 'NONE',  ( 11.32701196670594612, -39.47267329916473244, 30.49584611229249376 ) ) ;
#22005 = CARTESIAN_POINT ( 'NONE',  ( -101.8002770060248139, -59.99999999999998579, 77.51242708015574578 ) ) ;
#22007 = DIRECTION ( 'NONE',  ( 0.000000000000000000, 0.000000000000000000, 1.000000000000000000 ) ) ;
#22008 = VECTOR ( 'NONE', #84998, 1000.000000000000000 ) ;
#22009 = CARTESIAN_POINT ( 'NONE',  ( -45.48440666609703698, -36.07416133972417782, 43.31486618243847175 ) ) ;
#22010 = CARTESIAN_POINT ( 'NONE',  ( -3.014384158603856445, 20.49438651917788334, 6.320775516481683454 ) ) ;
#22011 = ORIENTED_EDGE ( 'NONE', *, *, #30734, .T. ) ;
#22012 = CARTESIAN_POINT ( 'NONE',  ( 36.47247920115664499, 437.5953975496288422, 4.244884750893885617 ) ) ;
#22013 = CARTESIAN_POINT ( 'NONE',  ( 17.83066785977196034, 36.70615155823221443, 22.40577935710491531 ) ) ;
#22014 =( NAMED_UNIT ( * ) PLANE_ANGLE_UNIT ( ) SI_UNIT ( $, .RADIAN. ) );
#22015 = ORIENTED_EDGE ( 'NONE', *, *, #69638, .F. ) ;
#22016 = CARTESIAN_POINT ( 'NONE',  ( -9.149732096576093099, -3.297952640180834560, 14.67458069835285706 ) ) ;
#22017 = VECTOR ( 'NONE', #93151, 1000.000000000000000 ) ;
#22018 = ORIENTED_EDGE ( 'NONE', *, *, #52450, .T. ) ;
#22019 = CARTESIAN_POINT ( 'NONE',  ( 81.72147651377501631, -29.99999999996476774, 193.8235977729058845 ) ) ;
#22020 = FILL_AREA_STYLE_COLOUR ( '', #18114 ) ;
#22021 = CARTESIAN_POINT ( 'NONE',  ( 6.364221311682587867, 41.95991762558126936, -59.61869606621115736 ) ) ;
#22022 = CARTESIAN_POINT ( 'NONE',  ( 98.32443016958239923, -30.00000000000000000, 190.1219309493679646 ) ) ;
#22023 = CARTESIAN_POINT ( 'NONE',  ( 0.7145311798163216377, 4.618802153517004960, 7.999999999999998224 ) ) ;
#22024 = EDGE_LOOP ( 'NONE', ( #62151, #22035, #55111, #74225, #101277 ) ) ;
#22025 = VERTEX_POINT ( 'NONE', #97450 ) ;
#22026 = ORIENTED_EDGE ( 'NONE', *, *, #29366, .F. ) ;
#22027 = AXIS2_PLACEMENT_3D ( 'NONE', #91481, #85518, #44526 ) ;
#22028 = CARTESIAN_POINT ( 'NONE',  ( -28.10508442060149292, 36.32168591140393943, 9.575330628090654272 ) ) ;
#22029 = CARTESIAN_POINT ( 'NONE',  ( 44.12472801211155371, 485.7238370326410859, 3.975897585125152123 ) ) ;
#22030 = CARTESIAN_POINT ( 'NONE',  ( 19.07845090537422550, 294.6331628770684574, 9.890526070132905190 ) ) ;
#22031 = SHAPE_REPRESENTATION ( '16. Toe', ( #10728 ), #26637 ) ;
#22032 = ORIENTED_EDGE ( 'NONE', *, *, #12325, .T. ) ;
#22034 = EDGE_CURVE ( 'NONE', #28006, #25105, #73165, .T. ) ;
#22033 = CARTESIAN_POINT ( 'NONE',  ( -16.04706041842033315, 4.602438919581462784, -3.432847546122274274 ) ) ;
#22035 = ORIENTED_EDGE ( 'NONE', *, *, #79066, .T. ) ;
#22036 = CARTESIAN_POINT ( 'NONE',  ( 101.5909309265440470, -38.45050066038580638, 199.8806868041374400 ) ) ;
#22037 = CARTESIAN_POINT ( 'NONE',  ( 14.11595029532509216, 2.410436752314641051, 5.024000119269121711 ) ) ;
#22038 = CARTESIAN_POINT ( 'NONE',  ( 82.53206627490877167, -37.86144382515931994, 6.795202634608455305 ) ) ;
#22039 = DIRECTION ( 'NONE',  ( -1.000000000000000000, 0.000000000000000000, 0.000000000000000000 ) ) ;
#22040 = VECTOR ( 'NONE', #61378, 1000.000000000000000 ) ;
#22041 = CARTESIAN_POINT ( 'NONE',  ( 42.75497199330776255, 415.3167855576094212, 19.81357880037930030 ) ) ;
#22042 = AXIS2_PLACEMENT_3D ( 'NONE', #101756, #37061, #18752 ) ;
#22043 = CARTESIAN_POINT ( 'NONE',  ( -43.00000000000000000, 461.4080316921935605, 3.462976341553817949 ) ) ;
#22044 = CARTESIAN_POINT ( 'NONE',  ( -27.10511071441192144, -1.200000000000000030E-05, -8.806984339685890006 ) ) ;
#22045 = CARTESIAN_POINT ( 'NONE',  ( 1.226845885076769616, -0.004855998333466520281, 101.2646151595213411 ) ) ;
#22046 =( GEOMETRIC_REPRESENTATION_CONTEXT ( 3 ) GLOBAL_UNCERTAINTY_ASSIGNED_CONTEXT ( ( #62087 ) ) GLOBAL_UNIT_ASSIGNED_CONTEXT ( ( #66155, #6311, #72126 ) ) REPRESENTATION_CONTEXT ( 'NONE', 'WORKASPACE' ) );
#22047 = EDGE_LOOP ( 'NONE', ( #91033, #72469, #95253, #99096 ) ) ;
#22048 = ADVANCED_FACE ( 'NONE', ( #33284 ), #16014, .T. ) ;
#22049 = SURFACE_STYLE_USAGE ( .BOTH. , #63026 ) ;
#22050 = CARTESIAN_POINT ( 'NONE',  ( -34.23250573208579794, 462.3234378130318305, 4.646251724931845573 ) ) ;
#22051 = DIRECTION ( 'NONE',  ( -1.000000000000000000, 0.000000000000000000, 0.000000000000000000 ) ) ;
#22052 = ORIENTED_EDGE ( 'NONE', *, *, #59439, .F. ) ;
#22053 = B_SPLINE_CURVE_WITH_KNOTS ( 'NONE', 3,
 ( #59978, #92840, #19003, #9785, #100401, #34652, #92300, #42701, #75598, #42165 ),
 .UNSPECIFIED., .F., .F.,
 ( 4, 2, 2, 2, 4 ),
 ( -2.000195913693157031E-05, 0.001085800244612924797, 0.002191602448362780890, 0.003297404652112636333, 0.004403206855862491775 ),
 .UNSPECIFIED. ) ;
#22054 = CARTESIAN_POINT ( 'NONE',  ( 0.000000000000000000, 0.000000000000000000, 5.000000000000002665 ) ) ;
#22055 = CARTESIAN_POINT ( 'NONE',  ( -35.49987330852459166, 304.0097181485430156, 4.051457700508126258 ) ) ;
#22056 = DIRECTION ( 'NONE',  ( 0.000000000000000000, -1.000000000000000000, 0.000000000000000000 ) ) ;
#22057 = DIRECTION ( 'NONE',  ( -1.000000000000000000, -1.224606353822377258E-16, -0.000000000000000000 ) ) ;
#22058 = CARTESIAN_POINT ( 'NONE',  ( 5.656854249492380582, -16.81249999999999289, -5.656854249492379694 ) ) ;
#22059 = CARTESIAN_POINT ( 'NONE',  ( 26.53083019430453859, -22.65905336700136630, 37.38260693527033851 ) ) ;
#22060 = CIRCLE ( 'NONE', #30693, 8.000000000000000000 ) ;
#22061 = CARTESIAN_POINT ( 'NONE',  ( 0.000000000000000000, 0.000000000000000000, 14.78272384904389192 ) ) ;
#22062 = ORIENTED_EDGE ( 'NONE', *, *, #37892, .T. ) ;
#22063 = CARTESIAN_POINT ( 'NONE',  ( 85.67953511968930513, -35.65700491136370687, 184.2338551578000363 ) ) ;
#22065 = AXIS2_PLACEMENT_3D ( 'NONE', #100519, #196, #1264 ) ;
#22064 = CARTESIAN_POINT ( 'NONE',  ( -49.27910061723718371, 7.914421806211214161, 15.56686240200379423 ) ) ;
#22066 = EDGE_CURVE ( 'NONE', #98501, #5193, #89390, .T. ) ;
#22067 = FILL_AREA_STYLE ('',( #94890 ) ) ;
#22068 = ORIENTED_EDGE ( 'NONE', *, *, #98458, .T. ) ;
#22069 = CARTESIAN_POINT ( 'NONE',  ( 93.83525582135544596, -57.67459712079030254, 11.50689781192917671 ) ) ;
#22070 = DIRECTION ( 'NONE',  ( 0.000000000000000000, -1.000000000000000000, 0.000000000000000000 ) ) ;
#22071 = CARTESIAN_POINT ( 'NONE',  ( 16.84999999999999787, 3.309500000000003439, 4.052968581778167743E-16 ) ) ;
#22072 = CARTESIAN_POINT ( 'NONE',  ( -7.664487212094859281, -22.09574587988852556, -38.54460460203753058 ) ) ;
#22073 = EDGE_CURVE ( 'NONE', #16303, #87833, #40215, .T. ) ;
#22074 = SHAPE_REPRESENTATION_RELATIONSHIP ( 'NONE' , 'NONE' ,  #533, #64127 ) ;
#22075 = AXIS2_PLACEMENT_3D ( 'NONE', #97660, #15162, #48047 ) ;
#22076 = FACE_OUTER_BOUND ( 'NONE', #18618, .T. ) ;
#22077 = CARTESIAN_POINT ( 'NONE',  ( 24.34999999999999787, 1.533819458162526451E-15, 0.000000000000000000 ) ) ;
#22078 = CARTESIAN_POINT ( 'NONE',  ( 37.73245083015999057, -25.32999417115200558, 34.64601903076129474 ) ) ;
#22079 = CIRCLE ( 'NONE', #13412, 4.000000000000000888 ) ;
#22081 = CARTESIAN_POINT ( 'NONE',  ( -13.40447963469854820, 7.804086714771164779, 8.560322119383409145 ) ) ;
#22080 = CARTESIAN_POINT ( 'NONE',  ( -42.69811214730272297, 434.9611672192513652, 18.34625614733208820 ) ) ;
#22082 = CARTESIAN_POINT ( 'NONE',  ( 9.659964574192086317, 294.6522956596213021, -2.587254427043884419 ) ) ;
#22083 =( NAMED_UNIT ( * ) PLANE_ANGLE_UNIT ( ) SI_UNIT ( $, .RADIAN. ) );
#22084 = CARTESIAN_POINT ( 'NONE',  ( -42.36837551588181583, -33.99149918245159085, -29.05969016418114492 ) ) ;
#22085 = CARTESIAN_POINT ( 'NONE',  ( -21.19348424345033521, 294.8901562694577478, 1.945151701991089332 ) ) ;
#22086 = VECTOR ( 'NONE', #87908, 1000.000000000000000 ) ;
#22087 = CARTESIAN_POINT ( 'NONE',  ( -102.5618070566913218, -38.00000000000000000, 164.2657687415081682 ) ) ;
#22088 = VECTOR ( 'NONE', #27538, 1000.000000000000000 ) ;
#22089 = VERTEX_POINT ( 'NONE', #321 ) ;
#22090 = CARTESIAN_POINT ( 'NONE',  ( -8.621479322451524041, -1.224621629255531419, 15.49382773535086066 ) ) ;
#22091 = DIRECTION ( 'NONE',  ( -1.000000000000000000, -1.224606353822377258E-16, -0.000000000000000000 ) ) ;
#22092 = CARTESIAN_POINT ( 'NONE',  ( 4.472135954999577834, -64.86420795053444976, 4.000000000000002665 ) ) ;
#22094 = CARTESIAN_POINT ( 'NONE',  ( -40.42326134380499525, -21.77016373189269416, -27.31203147464151115 ) ) ;
#22093 = LINE ( 'NONE', #31259, #5347 ) ;
#22095 = VERTEX_POINT ( 'NONE', #23072 ) ;
#22096 = CARTESIAN_POINT ( 'NONE',  ( 6.523606932381285084, 4.893847819346740735, -7.213065638940823199 ) ) ;
#22097 = COLOUR_RGB ( '', 0.08235294, 0.09019608, 0.10196078) ;
#22098 = AXIS2_PLACEMENT_3D ( 'NONE', #79543, #71442, #30489 ) ;
#22099 = ORIENTED_EDGE ( 'NONE', *, *, #88968, .T. ) ;
#22100 = AXIS2_PLACEMENT_3D ( 'NONE', #30182, #54410, #53900 ) ;
#22101 = LINE ( 'NONE', #77670, #63853 ) ;
#22102 = CARTESIAN_POINT ( 'NONE',  ( 0.000000000000000000, 0.000000000000000000, 0.000000000000000000 ) ) ;
#22103 = CARTESIAN_POINT ( 'NONE',  ( -92.65366311753854234, -60.00000000000000711, -9.671686281151320230 ) ) ;
#22104 = ORIENTED_EDGE ( 'NONE', *, *, #100591, .F. ) ;
#22105 = CARTESIAN_POINT ( 'NONE',  ( 7.999999999999998224, -27.78125000409677270, 3.313708498984766049 ) ) ;
#22106 =( LENGTH_UNIT ( ) NAMED_UNIT ( * ) SI_UNIT ( .MILLI., .METRE. ) );
#22107 = CIRCLE ( 'NONE', #11755, 8.750000000000023093 ) ;
#22108 = CARTESIAN_POINT ( 'NONE',  ( -9.699189539447127473, 26.82307771753288250, -2.444343703917214672 ) ) ;
#22110 = CARTESIAN_POINT ( 'NONE',  ( 0.000000000000000000, 43.19193163660326462, -24.55262289886175964 ) ) ;
#22109 = SURFACE_STYLE_FILL_AREA ( #4846 ) ;
#22111 = CARTESIAN_POINT ( 'NONE',  ( -84.47875027511349799, -18.66658693311171291, 151.2515477827395500 ) ) ;
#22112 = EDGE_LOOP ( 'NONE', ( #87473, #34980, #95910, #14017, #23754 ) ) ;
#22113 = CARTESIAN_POINT ( 'NONE',  ( -12.81917055448085030, 0.000000000000000000, 11.24487389205527776 ) ) ;
#22114 = ORIENTED_EDGE ( 'NONE', *, *, #43290, .F. ) ;
#22115 = ORIENTED_EDGE ( 'NONE', *, *, #37496, .F. ) ;
#22116 = CARTESIAN_POINT ( 'NONE',  ( 16.49565406582141947, -5.000000000000000000, 2.458857127971515233 ) ) ;
#22117 = ADVANCED_FACE ( 'NONE', ( #80208 ), #66156, .F. ) ;
#22118 = CARTESIAN_POINT ( 'NONE',  ( -6.125000000000000000, -60.71953810597580059, 14.41094225130411033 ) ) ;
#22119 = ORIENTED_EDGE ( 'NONE', *, *, #26063, .T. ) ;
#22120 = CARTESIAN_POINT ( 'NONE',  ( -10.28624191511830155, 45.38549880562041494, -15.40779740156157196 ) ) ;
#22121 = PRESENTATION_LAYER_ASSIGNMENT (  '', '', ( #104790 ) ) ;
#22122 = CARTESIAN_POINT ( 'NONE',  ( -9.341953373613076650, 15.21714514899110249, -3.572352985695669059 ) ) ;
#22123 = CARTESIAN_POINT ( 'NONE',  ( -81.06400256271496119, -57.51341943371168952, 199.7941202169005805 ) ) ;
#22124 = CARTESIAN_POINT ( 'NONE',  ( 0.7145311798163195283, -4.618802153516994302, 8.000000000000000000 ) ) ;
#22125 = DIRECTION ( 'NONE',  ( 0.000000000000000000, -1.000000000000000000, 0.000000000000000000 ) ) ;
#22126 = CARTESIAN_POINT ( 'NONE',  ( 84.73333333333332007, 4.172000000000019249, 5.109226446042768454E-16 ) ) ;
#22127 = EDGE_CURVE ( 'NONE', #91623, #70179, #39253, .T. ) ;
#22128 = CARTESIAN_POINT ( 'NONE',  ( 94.69963775048552179, -60.00000000000009948, 1.032162584924374293 ) ) ;
#22129 = CARTESIAN_POINT ( 'NONE',  ( -49.67087318978585841, -59.99999999999999289, 77.31351762338060496 ) ) ;
#22130 = B_SPLINE_CURVE_WITH_KNOTS ( 'NONE', 3,
 ( #94052, #44446, #20214, #77341, #3452, #85988, #36398, #12059, #44989, #69784, #77874, #102137, #102676, #56753, #73468, #63820, #40586, #55680, #57281, #39547, #8214, #14703, #22317, #105327, #48661, #106363, #23912, #16304, #31988, #74007, #15247, #41123, #90204, #31470 ),
 .UNSPECIFIED., .F., .F.,
 ( 4, 2, 2, 2, 2, 2, 2, 2, 2, 2, 2, 2, 2, 2, 2, 2, 4 ),
 ( 6.938893903907228378E-18, 0.0007899780065504824781, 0.001579956013100958017, 0.002369934019651433448, 0.003159912026201909096, 0.003949890032752384310, 0.004739868039302859958, 0.005529846045853335605, 0.006319824052403811253, 0.007109802058954286900, 0.007899780065504761681, 0.008689758072055237328, 0.009479736078605712976, 0.01026971408515618862, 0.01105969209170666427, 0.01184967009825713992, 0.01263964810480761557 ),
 .UNSPECIFIED. ) ;
#22131 = CARTESIAN_POINT ( 'NONE',  ( -56.41525400592121287, -42.96960946770816037, 64.88850874853261530 ) ) ;
#22132 = VECTOR ( 'NONE', #97926, 999.9999999999998863 ) ;
#22133 = ORIENTED_EDGE ( 'NONE', *, *, #88118, .F. ) ;
#22134 = CARTESIAN_POINT ( 'NONE',  ( -73.50473004590615744, -60.00000000000000000, -24.84693947030580574 ) ) ;
#22135 = ORIENTED_EDGE ( 'NONE', *, *, #87583, .T. ) ;
#22136 = CARTESIAN_POINT ( 'NONE',  ( -102.6327129110277099, -60.18409667677708086, 193.3961458806942062 ) ) ;
#22137 = EDGE_CURVE ( 'NONE', #87652, #38500, #63357, .T. ) ;
#22138 = CYLINDRICAL_SURFACE ( 'NONE', #47745, 8.000000000000000000 ) ;
#22139 = CIRCLE ( 'NONE', #90960, 5.000000000000000000 ) ;
#22140 = VERTEX_POINT ( 'NONE', #1945 ) ;
#22141 = CARTESIAN_POINT ( 'NONE',  ( 18.92236309988041043, 48.94305489900515482, 62.13249689941736165 ) ) ;
#22142 = CARTESIAN_POINT ( 'NONE',  ( 108.0899631164236609, -38.35819308738822997, 192.6723653064404402 ) ) ;
#22143 = CARTESIAN_POINT ( 'NONE',  ( -43.00000000000000000, 485.2629658518202405, -2.796394914059407100 ) ) ;
#22144 = CARTESIAN_POINT ( 'NONE',  ( 7.188101187499999156, -10.62500000204838813, 2.977408999572654924 ) ) ;
#22145 = PRESENTATION_STYLE_ASSIGNMENT (( #39384 ) ) ;
#22146 = FACE_OUTER_BOUND ( 'NONE', #49735, .T. ) ;
#22147 = CARTESIAN_POINT ( 'NONE',  ( 32.43164319908647286, 464.5283015133045978, 9.485638277864474333 ) ) ;
#22148 = CARTESIAN_POINT ( 'NONE',  ( -9.657909026534005292, 43.42990472694053494, -15.25053491157621899 ) ) ;
#22149 = CARTESIAN_POINT ( 'NONE',  ( -0.7843950794064245002, 34.98204345154115913, 27.51314879577667583 ) ) ;
#22150 = DIRECTION ( 'NONE',  ( -1.000000000000000000, -1.224606353822377258E-16, -0.000000000000000000 ) ) ;
#22151 = UNCERTAINTY_MEASURE_WITH_UNIT (LENGTH_MEASURE( 1.000000000000000082E-05 ), #20564, 'distance_accuracy_value', 'NONE');
#22152 = CARTESIAN_POINT ( 'NONE',  ( -29.01716069711826762, -49.91287937905969585, 34.62871294549472623 ) ) ;
#22153 = AXIS2_PLACEMENT_3D ( 'NONE', #59900, #92771, #53390 ) ;
#22154 = ORIENTED_EDGE ( 'NONE', *, *, #22739, .F. ) ;
#22155 = ORIENTED_EDGE ( 'NONE', *, *, #56964, .T. ) ;
#22156 = CARTESIAN_POINT ( 'NONE',  ( 47.01495483615595816, -29.15207790528993570, 43.18957708107585347 ) ) ;
#22157 = CYLINDRICAL_SURFACE ( 'NONE', #33575, 5.000000000000000888 ) ;
#22159 = VECTOR ( 'NONE', #95770, 1000.000000000000000 ) ;
#22158 = CARTESIAN_POINT ( 'NONE',  ( -5.839745530781596194, 14.05731516213037402, -3.859993546116442076 ) ) ;
#22161 = EDGE_CURVE ( 'NONE', #28378, #12793, #52099, .T. ) ;
#22160 = CARTESIAN_POINT ( 'NONE',  ( -108.0744233114761244, -38.35871118714575090, 192.8189671270986310 ) ) ;
#22162 = ORIENTED_EDGE ( 'NONE', *, *, #23083, .F. ) ;
#22163 = CARTESIAN_POINT ( 'NONE',  ( 85.86996992767592474, -38.36131443074192049, -22.03495116904964135 ) ) ;
#22164 = CARTESIAN_POINT ( 'NONE',  ( 11.40901652478997796, 14.23906480821464449, -9.939951793343480446 ) ) ;
#22165 = CARTESIAN_POINT ( 'NONE',  ( -6.503415501679381983, 41.93912328290132052, -68.91429205811094505 ) ) ;
#22166 = CARTESIAN_POINT ( 'NONE',  ( 30.00000000000000355, 461.8665156241228260, 11.40533150091922820 ) ) ;
#22167 = CARTESIAN_POINT ( 'NONE',  ( 10.90727606233362756, 43.80400056797084574, 13.07007756734143555 ) ) ;
#22168 = FACE_OUTER_BOUND ( 'NONE', #28813, .T. ) ;
#22169 = CARTESIAN_POINT ( 'NONE',  ( -32.42294576121290817, 435.8436782518352288, 18.25571606399968516 ) ) ;
#22170 = CARTESIAN_POINT ( 'NONE',  ( 32.42656933071582159, 485.5064012031800189, 3.828740380144981081 ) ) ;
#22171 = CARTESIAN_POINT ( 'NONE',  ( 5.000000000000000000, -19.72300213744072650, -4.527428753827365426 ) ) ;
#22172 = FACE_OUTER_BOUND ( 'NONE', #3653, .T. ) ;
#22173 = CIRCLE ( 'NONE', #91066, 4.172000000000009479 ) ;
#22174 = CARTESIAN_POINT ( 'NONE',  ( 94.81893203379229362, -60.00000000000002132, 202.5725863315619222 ) ) ;
#22175 = CONICAL_SURFACE ( 'NONE', #32562, 8.000000000000000000, 0.9599310885968911355 ) ;
#22176 = CARTESIAN_POINT ( 'NONE',  ( 0.000000000000000000, 0.000000000000000000, 0.000000000000000000 ) ) ;
#22177 = VERTEX_POINT ( 'NONE', #3021 ) ;
#22178 = CARTESIAN_POINT ( 'NONE',  ( 57.43676197718647103, -22.13903279540451052, 58.37046990149170256 ) ) ;
#22179 = CARTESIAN_POINT ( 'NONE',  ( -35.45950249840887381, 303.1341283215246563, -0.1035848689192439415 ) ) ;
#22180 = ADVANCED_FACE ( 'NONE', ( #90983, #34367, #35971, #67242 ), #101194, .T. ) ;
#22181 = CARTESIAN_POINT ( 'NONE',  ( 7.897196874019792645, 33.79127204167807008, -1.302055520192088256 ) ) ;
#22182 = VERTEX_POINT ( 'NONE', #19273 ) ;
#22184 = CARTESIAN_POINT ( 'NONE',  ( -14.62404193421258647, 22.28898781335485779, 3.917683339309744994 ) ) ;
#22183 = CARTESIAN_POINT ( 'NONE',  ( -107.3760131578118404, -38.36153571196422973, 194.1939700411200533 ) ) ;
#22185 = CARTESIAN_POINT ( 'NONE',  ( -42.68467435370097718, 439.3123962055185530, 17.84297149534227955 ) ) ;
#22186 = CARTESIAN_POINT ( 'NONE',  ( 27.42085833529588257, 312.9751210562151300, 10.90118510545367414 ) ) ;
#22188 = DIRECTION ( 'NONE',  ( -0.000000000000000000, 1.000000000000000000, -0.000000000000000000 ) ) ;
#22187 =( GEOMETRIC_REPRESENTATION_CONTEXT ( 3 ) GLOBAL_UNCERTAINTY_ASSIGNED_CONTEXT ( ( #10572 ) ) GLOBAL_UNIT_ASSIGNED_CONTEXT ( ( #64046, #13863, #103423 ) ) REPRESENTATION_CONTEXT ( 'NONE', 'WORKASPACE' ) );
#22189 = CARTESIAN_POINT ( 'NONE',  ( 7.999999999999998224, -30.59374999999999289, 3.313708498984766493 ) ) ;
#22190 = CARTESIAN_POINT ( 'NONE',  ( 2.617478844992707110, -5.000000000000015099, -94.73972676610841859 ) ) ;
#22191 = AXIS2_PLACEMENT_3D ( 'NONE', #56496, #23111, #14440 ) ;
#22192 = CIRCLE ( 'NONE', #20536, 13.27631144943088515 ) ;
#22193 = CARTESIAN_POINT ( 'NONE',  ( 29.77344787310960328, 13.34785391060249538, -42.10535821593529704 ) ) ;
#22195 = ORIENTED_EDGE ( 'NONE', *, *, #7815, .F. ) ;
#22194 = CARTESIAN_POINT ( 'NONE',  ( -7.801642220026312025, 101.4120317385096683, 1.787233835843584417 ) ) ;
#22196 = CARTESIAN_POINT ( 'NONE',  ( 82.14827175627938516, -49.98004452256672181, 178.0753244963457291 ) ) ;
#22197 = CARTESIAN_POINT ( 'NONE',  ( 8.216398312217762623, 115.1611316811069798, 0.000000000000000000 ) ) ;
#22198 = CARTESIAN_POINT ( 'NONE',  ( -35.50355603268687332, 439.1325461877797238, 24.06453856846038519 ) ) ;
#22199 = ORIENTED_EDGE ( 'NONE', *, *, #77384, .T. ) ;
#22200 = CARTESIAN_POINT ( 'NONE',  ( -28.32351931790351429, 306.0343727091704977, -9.290635017633318782 ) ) ;
#22201 = CARTESIAN_POINT ( 'NONE',  ( 7.261743840240279191, -3.634783834950141124, -18.04052776595507268 ) ) ;
#22202 = CARTESIAN_POINT ( 'NONE',  ( 1.224646799147353651E-15, 300.0000000000000000, 10.00000000000000178 ) ) ;
#22203 = CARTESIAN_POINT ( 'NONE',  ( -11.69514296590995706, 50.00000000000000000, -88.12259424196773239 ) ) ;
#22204 = CARTESIAN_POINT ( 'NONE',  ( -25.50394049119971740, 43.61918368478458774, -75.43787865382840607 ) ) ;
#22205 = FILL_AREA_STYLE_COLOUR ( '', #40498 ) ;
#22206 = ADVANCED_FACE ( 'NONE', ( #68300 ), #57713, .T. ) ;
#22207 = ORIENTED_EDGE ( 'NONE', *, *, #49462, .T. ) ;
#22208 = VECTOR ( 'NONE', #65161, 1000.000000000000227 ) ;
#22209 = CARTESIAN_POINT ( 'NONE',  ( -81.59189379692385558, -30.00000000000000711, -7.173991459043422836 ) ) ;
#22210 = CARTESIAN_POINT ( 'NONE',  ( -1.000000000000000000, -43.09265016209167953, 0.3552338647577958919 ) ) ;
#22211 = CARTESIAN_POINT ( 'NONE',  ( 0.000000000000000000, 6.928203230275506108, 4.000000000000007105 ) ) ;
#22212 = EDGE_CURVE ( 'NONE', #53832, #84815, #74885, .T. ) ;
#22215 = AXIS2_PLACEMENT_3D ( 'NONE', #92841, #92301, #19004 ) ;
#22214 = CARTESIAN_POINT ( 'NONE',  ( -11.79855021826020511, 16.42585737932439471, -9.399101548535638173 ) ) ;
#22213 = CARTESIAN_POINT ( 'NONE',  ( -0.7156389501956513799, -18.04057304077605295, 35.00644575174603546 ) ) ;
#22216 = CIRCLE ( 'NONE', #49745, 4.000000000000007105 ) ;
#22217 = CARTESIAN_POINT ( 'NONE',  ( -7.188101187500002709, -19.81250000204838813, 2.977408999572648707 ) ) ;
#22218 = UNCERTAINTY_MEASURE_WITH_UNIT (LENGTH_MEASURE( 1.000000000000000082E-05 ), #37013, 'distance_accuracy_value', 'NONE');
#22219 = DIRECTION ( 'NONE',  ( 0.000000000000000000, 1.224646799147353454E-16, 1.000000000000000000 ) ) ;
#22220 = EDGE_CURVE ( 'NONE', #25066, #24456, #67762, .T. ) ;
#22221 = CARTESIAN_POINT ( 'NONE',  ( 4.142849616820252293E-15, 27.68727484027578356, 33.82893434829263413 ) ) ;
#22222 = ORIENTED_EDGE ( 'NONE', *, *, #79354, .F. ) ;
#22223 = EDGE_CURVE ( 'NONE', #54822, #45637, #25206, .T. ) ;
#22224 =( NAMED_UNIT ( * ) PLANE_ANGLE_UNIT ( ) SI_UNIT ( $, .RADIAN. ) );
#22225 = CARTESIAN_POINT ( 'NONE',  ( 7.894958282449376696, -1.603399432393033397, -7.593838100136811597 ) ) ;
#22226 = CARTESIAN_POINT ( 'NONE',  ( -9.311676253867856801, 11.24588917681355049, -5.000000000000000000 ) ) ;
#22227 = CARTESIAN_POINT ( 'NONE',  ( 87.62222222222222001, 4.172000000000019249, 5.109226446042768454E-16 ) ) ;
#22228 = CARTESIAN_POINT ( 'NONE',  ( -10.39117206796836257, 0.000000000000000000, -8.500000000000000000 ) ) ;
#22229 = ORIENTED_EDGE ( 'NONE', *, *, #90307, .T. ) ;
#22230 = AXIS2_PLACEMENT_3D ( 'NONE', #47492, #39433, #31360 ) ;
#22231 = CARTESIAN_POINT ( 'NONE',  ( -3.594029361870008099, -9.531975552773349847, 6.225090491531444670 ) ) ;
#22232 = DIRECTION ( 'NONE',  ( -1.000000000000000000, -0.000000000000000000, -0.000000000000000000 ) ) ;
#22233 = ORIENTED_EDGE ( 'NONE', *, *, #63437, .F. ) ;
#22234 = DIRECTION ( 'NONE',  ( -0.000000000000000000, 1.000000000000000000, -0.000000000000000000 ) ) ;
#22235 = CARTESIAN_POINT ( 'NONE',  ( -46.21205304293484062, 39.15065308173836200, -44.64295635327282241 ) ) ;
#22236 = FACE_OUTER_BOUND ( 'NONE', #68298, .T. ) ;
#22237 = UNCERTAINTY_MEASURE_WITH_UNIT (LENGTH_MEASURE( 1.000000000000000082E-05 ), #98513, 'distance_accuracy_value', 'NONE');
#22238 = CARTESIAN_POINT ( 'NONE',  ( -111.1099793248805838, -60.00000000000001421, 153.2218623716563286 ) ) ;
#22239 = DIRECTION ( 'NONE',  ( -1.000000000000000000, 0.000000000000000000, 0.000000000000000000 ) ) ;
#22240 = CARTESIAN_POINT ( 'NONE',  ( 3.250000000000015099, 5.629165124598843661, 1.734723475976807094E-15 ) ) ;
#22241 = DIRECTION ( 'NONE',  ( 1.000000000000000000, -0.000000000000000000, -0.000000000000000000 ) ) ;
#22242 =( NAMED_UNIT ( * ) SI_UNIT ( $, .STERADIAN. ) SOLID_ANGLE_UNIT ( ) );
#22243 = AXIS2_PLACEMENT_3D ( 'NONE', #53849, #29111, #72165 ) ;
#22244 = CARTESIAN_POINT ( 'NONE',  ( -83.69448559273577359, -46.54495372303564693, 183.4117449980363403 ) ) ;
#22245 = VERTEX_POINT ( 'NONE', #100649 ) ;
#22246 = CARTESIAN_POINT ( 'NONE',  ( 39.06570142950455704, 42.03544815418795366, -56.79353983682526774 ) ) ;
#22247 = ORIENTED_EDGE ( 'NONE', *, *, #43306, .T. ) ;
#22248 = CARTESIAN_POINT ( 'NONE',  ( 5.500000036871884213, 42.00000000000000000, -68.91429207046176941 ) ) ;
#22249 = EDGE_CURVE ( 'NONE', #48784, #35708, #98982, .T. ) ;
#22250 = CARTESIAN_POINT ( 'NONE',  ( 1.000000000000000000, -68.32597503901369862, 12.04364623808666224 ) ) ;
#22251 = CARTESIAN_POINT ( 'NONE',  ( -84.90758499310180696, -52.70380024735796809, 13.63252645412560682 ) ) ;
#22252 = DIRECTION ( 'NONE',  ( 0.000000000000000000, -1.000000000000000000, 0.000000000000000000 ) ) ;
#22253 = CARTESIAN_POINT ( 'NONE',  ( -7.045755811259135193, -63.69658396986448423, 3.790843699961855773 ) ) ;
#22254 = CARTESIAN_POINT ( 'NONE',  ( 8.986804597165106046, 15.43199845811895266, 9.201869806248672558E-30 ) ) ;
#22255 = DIRECTION ( 'NONE',  ( -1.000000000000000000, -1.224606353822377258E-16, -0.000000000000000000 ) ) ;
#22256 = CARTESIAN_POINT ( 'NONE',  ( 15.50526908265481296, 41.99999999991779731, -57.69562748401063601 ) ) ;
#22257 = PRESENTATION_LAYER_ASSIGNMENT (  '', '', ( #34359 ) ) ;
#22258 = EDGE_CURVE ( 'NONE', #103579, #20459, #58163, .T. ) ;
#22259 = CARTESIAN_POINT ( 'NONE',  ( 99.10782808284749024, -14.21045842199446163, 197.1815751231716263 ) ) ;
#22260 = CARTESIAN_POINT ( 'NONE',  ( -104.0151861009774166, -30.00000000000006750, 120.6691871043967126 ) ) ;
#22261 = CARTESIAN_POINT ( 'NONE',  ( -62.71288653495292209, -60.34586746940613011, 90.28915145330465464 ) ) ;
#22262 = ORIENTED_EDGE ( 'NONE', *, *, #54425, .T. ) ;
#22263 = CARTESIAN_POINT ( 'NONE',  ( -20.51735722783412541, 39.42506220197849132, 61.74843859600010632 ) ) ;
#22264 = CARTESIAN_POINT ( 'NONE',  ( 95.99019121356252526, -60.00000000000866152, 204.9761892479625089 ) ) ;
#22265 = AXIS2_PLACEMENT_3D ( 'NONE', #100859, #28083, #93314 ) ;
#22266 = ORIENTED_EDGE ( 'NONE', *, *, #17686, .T. ) ;
#22267 = CARTESIAN_POINT ( 'NONE',  ( 88.20199406385988539, 1.030564683017419500E-14, 0.000000000000000000 ) ) ;
#22268 = CARTESIAN_POINT ( 'NONE',  ( -1.320432766682874540E-15, -16.90625000204838813, 7.188101187500000044 ) ) ;
#22269 = DIRECTION ( 'NONE',  ( -0.000000000000000000, -0.000000000000000000, -1.000000000000000000 ) ) ;
#22270 = EDGE_LOOP ( 'NONE', ( #27367, #4112 ) ) ;
#22271 = CARTESIAN_POINT ( 'NONE',  ( -11.49412716574636306, 45.59192006558699006, 13.79863126508840487 ) ) ;
#22273 = ORIENTED_EDGE ( 'NONE', *, *, #21720, .T. ) ;
#22272 = B_SPLINE_CURVE_WITH_KNOTS ( 'NONE', 3,
 ( #65231, #98123, #41481, #91122, #74369, #72259 ),
 .UNSPECIFIED., .F., .F.,
 ( 4, 2, 4 ),
 ( 0.000000000000000000, 0.0003352299596267586295, 0.0006704599192535172589 ),
 .UNSPECIFIED. ) ;
#22274 = FACE_OUTER_BOUND ( 'NONE', #99264, .T. ) ;
#22275 = CARTESIAN_POINT ( 'NONE',  ( -41.12904442321463705, 485.7386261246312529, -4.649563818468734233 ) ) ;
#22276 = CARTESIAN_POINT ( 'NONE',  ( -47.12223804421648055, -59.99999999999998579, -38.46817206024380909 ) ) ;
#22277 = DIRECTION ( 'NONE',  ( 1.000000000000000000, 0.000000000000000000, 0.000000000000000000 ) ) ;
#22278 = CARTESIAN_POINT ( 'NONE',  ( -7.188101187500002709, -24.68750000204838457, 2.977408999572648707 ) ) ;
#22279 = CARTESIAN_POINT ( 'NONE',  ( 40.34715123528543046, 1.340359594676612611E-15, 0.000000000000000000 ) ) ;
#22280 = CARTESIAN_POINT ( 'NONE',  ( 28.99999999999999645, 0.000000000000000000, 0.000000000000000000 ) ) ;
#22281 = SURFACE_STYLE_FILL_AREA ( #6051 ) ;
#22282 = CARTESIAN_POINT ( 'NONE',  ( 8.737863884120029567, 49.99999999999999289, -79.96381019768851672 ) ) ;
#22283 = CARTESIAN_POINT ( 'NONE',  ( 0.000000000000000000, -4.000000000000003553, 123.0000000000000142 ) ) ;
#22284 = CARTESIAN_POINT ( 'NONE',  ( -36.20959526385565397, 304.3379572843515461, 0.1881653396831703962 ) ) ;
#22285 = EDGE_CURVE ( 'NONE', #42431, #64398, #43491, .T. ) ;
#22286 = CARTESIAN_POINT ( 'NONE',  ( 20.87268443183278421, 302.8961289238256427, -9.990552340451243296 ) ) ;
#22287 = CARTESIAN_POINT ( 'NONE',  ( -39.17226668844914883, -39.51869471205692008, 38.04320566444418006 ) ) ;
#22288 = CIRCLE ( 'NONE', #11927, 4.000000000000000888 ) ;
#22289 = ORIENTED_EDGE ( 'NONE', *, *, #12483, .F. ) ;
#22290 = CARTESIAN_POINT ( 'NONE',  ( -9.769072601666671574, 53.46510771226535041, -2.425000069901109168 ) ) ;
#22291 = CARTESIAN_POINT ( 'NONE',  ( -33.95156263172582101, 464.5083255208627975, 6.608064661821575037 ) ) ;
#22292 = CARTESIAN_POINT ( 'NONE',  ( 33.91238484704524581, -53.36470455789326905, 37.37873827427225848 ) ) ;
#22293 = CARTESIAN_POINT ( 'NONE',  ( -13.60704923275580924, -1.734723475976807094E-15, -10.45706415777457465 ) ) ;
#22294 = ORIENTED_EDGE ( 'NONE', *, *, #59211, .F. ) ;
#22295 = CARTESIAN_POINT ( 'NONE',  ( 6.289692432696756264, -5.239086202715468765, 4.583616368337883884 ) ) ;
#22296 = AXIS2_PLACEMENT_3D ( 'NONE', #104111, #29741, #103073 ) ;
#22297 = CARTESIAN_POINT ( 'NONE',  ( -75.95103116715310421, -38.37491938504500411, 177.9832065501431941 ) ) ;
#22298 = ORIENTED_EDGE ( 'NONE', *, *, #41302, .T. ) ;
#22300 = CARTESIAN_POINT ( 'NONE',  ( 41.58649125062324003, 315.0454808444952732, -5.157136739135766312 ) ) ;
#22299 = CARTESIAN_POINT ( 'NONE',  ( 6.500000000000005329, -3.752776749732582573, -6.177805531629061875 ) ) ;
#22301 = CARTESIAN_POINT ( 'NONE',  ( 58.18888888888888999, 6.915964383211875250E-15, 0.000000000000000000 ) ) ;
#22302 = CARTESIAN_POINT ( 'NONE',  ( 6.394337469123806628, -3.776351736504769629, -6.540833074877204112 ) ) ;
#22303 = CARTESIAN_POINT ( 'NONE',  ( 0.1684239960690284144, 43.17555810750861411, -18.75000000000000711 ) ) ;
#22304 = CARTESIAN_POINT ( 'NONE',  ( -41.20010578034021620, 436.9751675121757444, 5.754626909160545090 ) ) ;
#22305 = FACE_OUTER_BOUND ( 'NONE', #104011, .T. ) ;
#22306 = FACE_OUTER_BOUND ( 'NONE', #90894, .T. ) ;
#22307 = AXIS2_PLACEMENT_3D ( 'NONE', #79549, #38582, #5141 ) ;
#22308 = CARTESIAN_POINT ( 'NONE',  ( 94.17286979174674855, -59.99999999999999289, 42.72536648720843999 ) ) ;
#22309 = B_SPLINE_CURVE_WITH_KNOTS ( 'NONE', 3,
 ( #74074, #23447, #56283, #73537 ),
 .UNSPECIFIED., .F., .F.,
 ( 4, 4 ),
 ( 0.000000000000000000, 0.001448684797825257461 ),
 .UNSPECIFIED. ) ;
#22310 = DIRECTION ( 'NONE',  ( -0.000000000000000000, -1.000000000000000000, -0.000000000000000000 ) ) ;
#22311 = CARTESIAN_POINT ( 'NONE',  ( 23.21751746555303342, 27.38103382803677377, 33.20617127781017075 ) ) ;
#22312 = CARTESIAN_POINT ( 'NONE',  ( 0.000000000000000000, -945.0000000000000000, 0.000000000000000000 ) ) ;
#22313 = VERTEX_POINT ( 'NONE', #10050 ) ;
#22314 = CARTESIAN_POINT ( 'NONE',  ( -63.87591448453517984, -30.00000000000000711, 77.01698376430015003 ) ) ;
#22315 = ORIENTED_EDGE ( 'NONE', *, *, #11495, .T. ) ;
#22316 = AXIS2_PLACEMENT_3D ( 'NONE', #18626, #18081, #25671 ) ;
#22317 = CARTESIAN_POINT ( 'NONE',  ( -9.771805689013445928, -57.46313207252903510, 29.13556849961307194 ) ) ;
#22318 = CARTESIAN_POINT ( 'NONE',  ( -15.38120149534759484, 2.925591750584245698, 2.537117285879322726 ) ) ;
#22319 = CARTESIAN_POINT ( 'NONE',  ( 9.300358455352606413, 11.36566808881823754, 4.999999999998467004 ) ) ;
#22320 = CARTESIAN_POINT ( 'NONE',  ( 32.13489264513381727, 427.2002522300152805, 24.83829134347774215 ) ) ;
#22321 = CARTESIAN_POINT ( 'NONE',  ( 83.26081960998183717, -52.72642717100047349, -16.35834959482691175 ) ) ;
#22322 = CARTESIAN_POINT ( 'NONE',  ( 5.082755093536324154, -30.21875000204838813, 5.082755093536326818 ) ) ;
#22323 = CARTESIAN_POINT ( 'NONE',  ( -18.91791044776116237, 45.00000000000000711, 62.18611311450884926 ) ) ;
#22324 = DIRECTION ( 'NONE',  ( 0.000000000000000000, 0.000000000000000000, 1.000000000000000000 ) ) ;
#22325 = CARTESIAN_POINT ( 'NONE',  ( 34.90210058998459175, 473.1145171525240585, 16.89534907407908548 ) ) ;
#22326 = VERTEX_POINT ( 'NONE', #35428 ) ;
#22327 = VECTOR ( 'NONE', #32080, 1000.000000000000000 ) ;
#22329 = ORIENTED_EDGE ( 'NONE', *, *, #3451, .T. ) ;
#22328 = DIRECTION ( 'NONE',  ( 0.000000000000000000, 0.000000000000000000, -1.000000000000000000 ) ) ;
#22330 = CARTESIAN_POINT ( 'NONE',  ( 78.78750774858497152, -53.37144728722491038, 153.4658605898123369 ) ) ;
#22331 = AXIS2_PLACEMENT_3D ( 'NONE', #55947, #71619, #88361 ) ;
#22332 = DIRECTION ( 'NONE',  ( 0.000000000000000000, 0.000000000000000000, 1.000000000000000000 ) ) ;
#22333 = ORIENTED_EDGE ( 'NONE', *, *, #17766, .T. ) ;
#22334 = CARTESIAN_POINT ( 'NONE',  ( -12.50000000000000178, 40.62314097313324623, -68.19079107895046832 ) ) ;
#22335 = FILL_AREA_STYLE ('',( #104274 ) ) ;
#22336 = CARTESIAN_POINT ( 'NONE',  ( -2.977408999572654480, -10.62500000204838813, 7.188101187499999156 ) ) ;
#22337 = CARTESIAN_POINT ( 'NONE',  ( -33.87510863592373767, -57.69360311548409470, 48.02532427896534983 ) ) ;
#22338 = CARTESIAN_POINT ( 'NONE',  ( 16.93821050485266611, 302.5835677207606409, 9.880234544770994276 ) ) ;
#22339 = EDGE_CURVE ( 'NONE', #6033, #89992, #49187, .T. ) ;
#22340 = ORIENTED_EDGE ( 'NONE', *, *, #35706, .T. ) ;
#22341 = B_SPLINE_CURVE_WITH_KNOTS ( 'NONE', 3,
 ( #72661, #73171, #32225, #84488, #68849, #10055, #100655, #76917, #83944, #19279, #75856, #60760, #59689, #51031, #18718, #101725, #76374, #17637, #85015, #51573, #75312, #42420, #26815, #1409, #44024, #42964 ),
 .UNSPECIFIED., .F., .F.,
 ( 4, 2, 2, 2, 2, 2, 2, 2, 2, 2, 2, 2, 4 ),
 ( 0.003090333073482954759, 0.003342552850341273894, 0.003594772627199593028, 0.003846992404057912162, 0.004099212180916231296, 0.004603651734632862626, 0.004855871511491176989, 0.005108091288349492221, 0.006116970395782750543, 0.006369190172641068376, 0.006621409949499387076, 0.006873629726357705777, 0.007125849503216023610 ),
 .UNSPECIFIED. ) ;
#22342 = ADVANCED_FACE ( 'NONE', ( #77979 ), #29984, .T. ) ;
#22343 = CYLINDRICAL_SURFACE ( 'NONE', #33879, 14.00000000000000178 ) ;
#22344 = CARTESIAN_POINT ( 'NONE',  ( -4.472135954999583163, -10.27411850998327303, -4.000000000000000888 ) ) ;
#22345 = AXIS2_PLACEMENT_3D ( 'NONE', #60801, #33877, #66755 ) ;
#22346 = CARTESIAN_POINT ( 'NONE',  ( 7.087005777346045754, 41.65067221237009676, -59.33604986165270390 ) ) ;
#22347 = EDGE_CURVE ( 'NONE', #45998, #39827, #14407, .T. ) ;
#22348 = FILL_AREA_STYLE ('',( #6114 ) ) ;
#22349 = ORIENTED_EDGE ( 'NONE', *, *, #102055, .F. ) ;
#22350 = CARTESIAN_POINT ( 'NONE',  ( 8.000000000000000000, -12.59375000409676737, -3.313708498984761608 ) ) ;
#22351 = CARTESIAN_POINT ( 'NONE',  ( -7.543428673995849820, -13.25821866003511751, 32.00908194862271472 ) ) ;
#22352 = CARTESIAN_POINT ( 'NONE',  ( 9.151133496030011472, 15.07443463110253923, 4.034557488804340508 ) ) ;
#22353 = ADVANCED_FACE ( 'NONE', ( #37024 ), #98993, .F. ) ;
#22354 = CARTESIAN_POINT ( 'NONE',  ( 1.102560413418700813, 51.47929533831098325, -9.610321672475258481 ) ) ;
#22355 = FACE_OUTER_BOUND ( 'NONE', #33428, .T. ) ;
#22356 = CARTESIAN_POINT ( 'NONE',  ( 8.000000000000000000, -19.99999999999999289, 0.000000000000000000 ) ) ;
#22357 = CARTESIAN_POINT ( 'NONE',  ( 41.88291765283142354, 546.5234784715379419, 200.1325441657795068 ) ) ;
#22358 = CARTESIAN_POINT ( 'NONE',  ( -9.483056940782031319, 32.44387790106576830, -3.177305548492605602 ) ) ;
#22359 = ORIENTED_EDGE ( 'NONE', *, *, #58751, .F. ) ;
#22360 = CARTESIAN_POINT ( 'NONE',  ( 11.53278078296752263, 43.31871327052838438, 14.28168592353131139 ) ) ;
#22361 = EDGE_CURVE ( 'NONE', #106390, #39461, #38747, .T. ) ;
#22362 = CARTESIAN_POINT ( 'NONE',  ( 19.00000000000001421, -4.999999999999999112, 25.00000000000000000 ) ) ;
#22363 = CYLINDRICAL_SURFACE ( 'NONE', #72154, 4.000000000000000000 ) ;
#22364 = CARTESIAN_POINT ( 'NONE',  ( 22.34684471419683760, -26.69134893376664763, -38.45222277864926497 ) ) ;
#22365 = CARTESIAN_POINT ( 'NONE',  ( -82.83519950011617539, -30.00000000000000711, 151.7030435779494439 ) ) ;
#22366 = DIRECTION ( 'NONE',  ( -1.000000000000000000, 0.000000000000000000, 0.000000000000000000 ) ) ;
#22367 = EDGE_CURVE ( 'NONE', #34982, #2439, #78376, .T. ) ;
#22368 = AXIS2_PLACEMENT_3D ( 'NONE', #28919, #21339, #79008 ) ;
#22369 = ORIENTED_EDGE ( 'NONE', *, *, #43312, .T. ) ;
#22370 = VECTOR ( 'NONE', #65024, 1000.000000000000000 ) ;
#22371 = LINE ( 'NONE', #14222, #32397 ) ;
#22372 = CARTESIAN_POINT ( 'NONE',  ( 107.9489589369664202, -57.65951413602503095, 199.0667566530268573 ) ) ;
#22373 = CARTESIAN_POINT ( 'NONE',  ( 67.20503002699381057, -47.40899075066970170, -25.20247587780630383 ) ) ;
#22374 = CARTESIAN_POINT ( 'NONE',  ( -6.878751942472529635, -3.924677726130946009, -6.573129608219094422 ) ) ;
#22375 = CARTESIAN_POINT ( 'NONE',  ( -16.13463197906294155, 21.11076038462449844, 3.387067249032789551 ) ) ;
#22376 = CARTESIAN_POINT ( 'NONE',  ( 65.26738680892601963, 40.83906611471848436, 0.8120011907752979763 ) ) ;
#22377 = CARTESIAN_POINT ( 'NONE',  ( -73.55625695019807608, -60.00000000000001421, 167.7443850725575203 ) ) ;
#22378 = CARTESIAN_POINT ( 'NONE',  ( 1.152188841818234133E-13, -1.200000000000000030E-05, 50.50000000000000000 ) ) ;
#22379 = CARTESIAN_POINT ( 'NONE',  ( 34.83349330513380693, 1.593028355512270962E-15, 0.000000000000000000 ) ) ;
#22380 = AXIS2_PLACEMENT_3D ( 'NONE', #103178, #62723, #14138 ) ;
#22381 = CARTESIAN_POINT ( 'NONE',  ( 53.52139369741866659, 50.00000000000000000, 33.73130704865685914 ) ) ;
#22382 = CARTESIAN_POINT ( 'NONE',  ( -84.16960440523372711, -61.06210287833253147, 192.5424730624227436 ) ) ;
#22383 = ORIENTED_EDGE ( 'NONE', *, *, #26199, .F. ) ;
#22384 = CARTESIAN_POINT ( 'NONE',  ( 35.74123987347093845, 414.7932616781445745, 5.921579997229594383 ) ) ;
#22385 = B_SPLINE_SURFACE_WITH_KNOTS ( 'NONE', 1, 3, ( 
 ( #93893, #45353, #12421, #37281, #20050, #103052, #102516, #37818, #28660, #70676, #29719, #83939, #41352, #66157, #25756, #50491, #18165, #100121, #58615, #98521, #74246, #24667, #67243, #82344, #56993, #26287, #90984, #57520 ),
 ( #90441, #25207, #66698, #99039, #42415, #59148, #51027, #58060, #65635, #322, #91516, #8452, #33285, #81789, #89908, #17631, #10051, #33825, #32764, #17096, #74769, #83404, #1403, #9502, #16550, #49435, #75308, #92031 ) ),
 .UNSPECIFIED., .F., .F., .F.,
 ( 2, 2 ),
 ( 4, 2, 2, 2, 2, 2, 2, 2, 2, 2, 2, 2, 2, 4 ),
 ( 0.000000000000000000, 1.000000000000000000 ),
 ( 0.08901491201581737678, 0.1032490540155679704, 0.1174831960153185778, 0.1317173380150691853, 0.1459514800148197788, 0.1744197640143299588, 0.2028880480138401388, 0.2598246160128514504, 0.3167611840118632616, 0.4306343200098861623, 0.5445074560079088410, 0.6583805920059359051, 0.7722537280039543095, 1.000000000000000000 ),
 .UNSPECIFIED. ) ;
#22386 = CIRCLE ( 'NONE', #3422, 5.000000000000011546 ) ;
#22387 = CARTESIAN_POINT ( 'NONE',  ( 10.67808697578073129, -5.000000000000001776, -77.27709671283406578 ) ) ;
#22388 = ADVANCED_FACE ( 'NONE', ( #3565 ), #94166, .F. ) ;
#22389 = CARTESIAN_POINT ( 'NONE',  ( -81.77152546554842161, -37.79979095042777004, -14.16671787682579087 ) ) ;
#22390 = CIRCLE ( 'NONE', #39616, 4.172000000000009479 ) ;
#22391 = CARTESIAN_POINT ( 'NONE',  ( 32.33349330513379982, 1.593028355512270567E-15, 0.000000000000000000 ) ) ;
#22392 = DIRECTION ( 'NONE',  ( 0.5735764363510468256, 0.8191520442889913545, 0.000000000000000000 ) ) ;
#22393 = ORIENTED_EDGE ( 'NONE', *, *, #4417, .F. ) ;
#22394 = DIRECTION ( 'NONE',  ( -1.000000000000000000, -1.224606353822377258E-16, -0.000000000000000000 ) ) ;
#22395 = DIRECTION ( 'NONE',  ( 0.000000000000000000, 1.000000000000000000, 0.000000000000000000 ) ) ;
#22396 = ADVANCED_FACE ( 'NONE', ( #14818 ), #5991, .T. ) ;
#22397 = CARTESIAN_POINT ( 'NONE',  ( 12.70248734011840597, -4.285714285713678073, -22.03900363279143093 ) ) ;
#22398 = CARTESIAN_POINT ( 'NONE',  ( -35.59180895336101003, 464.2025721804453724, 19.31791767298735252 ) ) ;
#22399 = CARTESIAN_POINT ( 'NONE',  ( 82.45758146611665040, -29.99999999999998579, -23.17547892442675916 ) ) ;
#22400 = CARTESIAN_POINT ( 'NONE',  ( -77.47082139812327739, -60.31520998343973616, 152.1232861070816114 ) ) ;
#22401 = VERTEX_POINT ( 'NONE', #71464 ) ;
#22402 = CARTESIAN_POINT ( 'NONE',  ( 8.555523463203789092, -60.00000000000005684, 41.98724916707659816 ) ) ;
#22403 = CARTESIAN_POINT ( 'NONE',  ( 5.500000036871884213, 42.00000000000000000, -68.91429207046176941 ) ) ;
#22404 = CARTESIAN_POINT ( 'NONE',  ( 75.40687419154917848, -57.56243725155260904, 191.7921977673724996 ) ) ;
#22405 = CARTESIAN_POINT ( 'NONE',  ( 59.16597917554048536, 50.00000000000000711, 21.79159307829888803 ) ) ;
#22406 = CARTESIAN_POINT ( 'NONE',  ( 37.98379125797355016, 307.9909936412415163, 1.091397535864746970 ) ) ;
#22407 = AXIS2_PLACEMENT_3D ( 'NONE', #5118, #79523, #87109 ) ;
#22408 = CARTESIAN_POINT ( 'NONE',  ( 8.595526037062774425E-16, 13.85270131633358304, 7.000000000000011546 ) ) ;
#22409 = VERTEX_POINT ( 'NONE', #32638 ) ;
#22410 = CARTESIAN_POINT ( 'NONE',  ( 19.83349330513379982, -7.703719777548943412E-31, 4.000000000000001776 ) ) ;
#22412 = CARTESIAN_POINT ( 'NONE',  ( -103.7245430960311126, -45.26537689992342450, 163.3981769379987270 ) ) ;
#22411 = CARTESIAN_POINT ( 'NONE',  ( -15.54289451413713152, 36.90012926360033418, 23.41220851048981544 ) ) ;
#22413 = CARTESIAN_POINT ( 'NONE',  ( 4.401442555609581635E-16, -27.78125000204838457, -7.188101187500000044 ) ) ;
#22414 = PLANE ( 'NONE',  #46389 ) ;
#22415 = DIRECTION ( 'NONE',  ( 0.000000000000000000, 0.000000000000000000, 1.000000000000000000 ) ) ;
#22416 = CARTESIAN_POINT ( 'NONE',  ( 6.075720087193105634, 41.99394347255277182, -59.86320241472431292 ) ) ;
#22417 = CARTESIAN_POINT ( 'NONE',  ( -5.420469775605654128, 41.88321586335170821, -59.04137891894603030 ) ) ;
#22418 = EDGE_CURVE ( 'NONE', #17545, #43945, #52500, .T. ) ;
#22419 = CARTESIAN_POINT ( 'NONE',  ( 17.40745463263493065, 43.24839122124123492, -6.411055176082404827 ) ) ;
#22420 = VERTEX_POINT ( 'NONE', #31060 ) ;
#22421 = CARTESIAN_POINT ( 'NONE',  ( 0.5805565836007605673, 3.752776749732565253, 6.499999999999997335 ) ) ;
#22423 = CARTESIAN_POINT ( 'NONE',  ( 25.83843143683618848, -32.52250552547243956, 30.74844871866972085 ) ) ;
#22422 = CARTESIAN_POINT ( 'NONE',  ( -8.181074200006944963, -14.21045842199423603, 34.35486773805523342 ) ) ;
#22424 = CIRCLE ( 'NONE', #53421, 1.999999999999998224 ) ;
#22425 = CARTESIAN_POINT ( 'NONE',  ( -23.38223461712482276, 25.21832460939182852, 33.20617127781060418 ) ) ;
#22426 = ORIENTED_EDGE ( 'NONE', *, *, #56017, .T. ) ;
#22427 = ADVANCED_FACE ( 'NONE', ( #40690 ), #31577, .F. ) ;
#22428 = B_SPLINE_CURVE_WITH_KNOTS ( 'NONE', 3,
 ( #1865, #52548, #85471, #59607, #36427, #67689, #43415, #25675, #51489, #58539, #17555, #83325, #42337, #29902, #87069, #79488, #6118, #21821, #62788, #61196, #71384, #78954, #13143, #4542 ),
 .UNSPECIFIED., .F., .F.,
 ( 4, 2, 2, 2, 2, 2, 2, 2, 2, 2, 2, 4 ),
 ( 0.002907281924855007089, 0.003411952726777704205, 0.003916623528700401320, 0.004168958929661742939, 0.004421294330623083690, 0.004673629731584425309, 0.004925965132545766928, 0.005430635934468451900, 0.005682971335429793519, 0.005935306736391136005, 0.006439977538313801028, 0.006944648340236465184 ),
 .UNSPECIFIED. ) ;
#22429 = UNCERTAINTY_MEASURE_WITH_UNIT (LENGTH_MEASURE( 1.000000000000000082E-05 ), #52356, 'distance_accuracy_value', 'NONE');
#22430 = VERTEX_POINT ( 'NONE', #80613 ) ;
#22432 = CARTESIAN_POINT ( 'NONE',  ( 36.09139106816682130, 461.0566049081365350, 3.057441095446108648 ) ) ;
#22431 =( LENGTH_UNIT ( ) NAMED_UNIT ( * ) SI_UNIT ( .MILLI., .METRE. ) );
#22433 = SURFACE_SIDE_STYLE ('',( #104918 ) ) ;
#22434 = FACE_OUTER_BOUND ( 'NONE', #50276, .T. ) ;
#22435 = ADVANCED_FACE ( 'NONE', ( #48769 ), #33587, .T. ) ;
#22436 = DIRECTION ( 'NONE',  ( -0.000000000000000000, -0.000000000000000000, 1.000000000000000000 ) ) ;
#22437 = CARTESIAN_POINT ( 'NONE',  ( 0.5298411179699548113, 18.60179019596422023, -49.36142467042689219 ) ) ;
#22438 = ORIENTED_EDGE ( 'NONE', *, *, #7810, .F. ) ;
#22439 = CARTESIAN_POINT ( 'NONE',  ( 1.309624450538505291, -60.00000000000000711, -42.63907992752542953 ) ) ;
#22440 = CARTESIAN_POINT ( 'NONE',  ( 59.64050360443124532, -29.99999999999996447, 65.96467207391573595 ) ) ;
#22441 = CARTESIAN_POINT ( 'NONE',  ( -10.27837503968532396, 16.60654002188488221, 10.02334268984631827 ) ) ;
#22442 = CARTESIAN_POINT ( 'NONE',  ( 21.67692307692307452, -4.171999999999999709, 5.616230220889763424E-16 ) ) ;
#22443 = CARTESIAN_POINT ( 'NONE',  ( -10.47796581436744923, -5.000000000000000000, -78.93819186519100128 ) ) ;
#22444 = CARTESIAN_POINT ( 'NONE',  ( 10.41054107240687188, 5.000000000000002665, 0.000000000000000000 ) ) ;
#22445 = ORIENTED_EDGE ( 'NONE', *, *, #77380, .F. ) ;
#22446 = AXIS2_PLACEMENT_3D ( 'NONE', #105031, #58054, #8445 ) ;
#22447 = ORIENTED_EDGE ( 'NONE', *, *, #84517, .T. ) ;
#22448 = ORIENTED_EDGE ( 'NONE', *, *, #86935, .T. ) ;
#22449 = DIRECTION ( 'NONE',  ( 0.5735764363510554853, 0.8191520442889852482, 0.000000000000000000 ) ) ;
#22450 = CYLINDRICAL_SURFACE ( 'NONE', #5806, 1.250000000000001110 ) ;
#22451 = CARTESIAN_POINT ( 'NONE',  ( 0.000000000000000000, 30.00000000000000000, 0.000000000000000000 ) ) ;
#22452 = CARTESIAN_POINT ( 'NONE',  ( 13.86650669486618881, -3.999999999999998224, 0.000000000000000000 ) ) ;
#22453 = SURFACE_STYLE_USAGE ( .BOTH. , #83034 ) ;
#22454 = CARTESIAN_POINT ( 'NONE',  ( -46.00000000000000000, 485.7784312020116886, -0.3394844618430318262 ) ) ;
#22455 = CARTESIAN_POINT ( 'NONE',  ( 8.099999999999999645, -3.752776749732575468, -6.499999999999999112 ) ) ;
#22457 = ORIENTED_EDGE ( 'NONE', *, *, #91161, .F. ) ;
#22456 = AXIS2_PLACEMENT_3D ( 'NONE', #9057, #41436, #98601 ) ;
#22458 = CARTESIAN_POINT ( 'NONE',  ( 2.617478844992369158, 49.99999999999999289, -75.26027323389158141 ) ) ;
#22459 = EDGE_LOOP ( 'NONE', ( #24246, #21018, #1828, #88207, #66665 ) ) ;
#22460 = DIRECTION ( 'NONE',  ( 0.000000000000000000, 0.000000000000000000, 1.000000000000000000 ) ) ;
#22461 = CARTESIAN_POINT ( 'NONE',  ( 32.91522635463719837, 465.6822307888475052, 10.74522530471245041 ) ) ;
#22462 = CARTESIAN_POINT ( 'NONE',  ( -40.83002285428302969, 485.0211005501724912, -4.017563975490292982 ) ) ;
#22463 = CARTESIAN_POINT ( 'NONE',  ( 6.144704265756976369, 301.8764918330675187, -10.02047951298166240 ) ) ;
#22464 = CARTESIAN_POINT ( 'NONE',  ( 64.56574826876759232, -25.57792867474360321, 77.78118918835328088 ) ) ;
#22465 = ORIENTED_EDGE ( 'NONE', *, *, #91432, .T. ) ;
#22466 = VECTOR ( 'NONE', #75326, 1000.000000000000000 ) ;
#22467 = CARTESIAN_POINT ( 'NONE',  ( 40.49255712025206577, 464.0858896352993952, 18.37716086306491903 ) ) ;
#22468 = CARTESIAN_POINT ( 'NONE',  ( 29.68315524077034340, 8.302504244945382084, 42.10535821593451544 ) ) ;
#22469 = CARTESIAN_POINT ( 'NONE',  ( 16.05785784214672773, 4.775831776474238843, 3.710403933782425057 ) ) ;
#22470 = AXIS2_PLACEMENT_3D ( 'NONE', #92426, #101060, #93520 ) ;
#22471 = CARTESIAN_POINT ( 'NONE',  ( -18.99999999999999289, 5.000000000000000888, 25.00000000000000000 ) ) ;
#22472 = ADVANCED_FACE ( 'NONE', ( #96824 ), #83593, .T. ) ;
#22473 = VERTEX_POINT ( 'NONE', #72008 ) ;
#22474 = AXIS2_PLACEMENT_3D ( 'NONE', #36693, #102446, #28591 ) ;
#22475 = CARTESIAN_POINT ( 'NONE',  ( -3.400000000000000355, 4.163799117101001052E-16, -1.876475477074182940 ) ) ;
#22476 = CARTESIAN_POINT ( 'NONE',  ( 70.62474104179052858, -59.99999999999999289, -26.13143283881593604 ) ) ;
#22477 = ADVANCED_FACE ( 'NONE', ( #89260 ), #57803, .T. ) ;
#22478 = DIRECTION ( 'NONE',  ( 0.000000000000000000, 1.000000000000000000, 0.000000000000000000 ) ) ;
#22479 = ADVANCED_FACE ( 'NONE', ( #73578 ), #87092, .T. ) ;
#22480 = CIRCLE ( 'NONE', #17376, 3.309500000000007880 ) ;
#22481 = CARTESIAN_POINT ( 'NONE',  ( 3.313708498984762052, -28.90625000409677270, -8.000000000000000000 ) ) ;
#22482 = CARTESIAN_POINT ( 'NONE',  ( -8.922269033012433681, -5.000000000000000000, 5.219866590718518218 ) ) ;
#22483 = CARTESIAN_POINT ( 'NONE',  ( 86.60940601525219051, -20.70715439809982783, 184.3503468479922276 ) ) ;
#22484 = EDGE_CURVE ( 'NONE', #93970, #65357, #85387, .T. ) ;
#22485 = CARTESIAN_POINT ( 'NONE',  ( -5.293082431914539754, 18.39773536900015216, -37.77701885971370643 ) ) ;
#22486 = CARTESIAN_POINT ( 'NONE',  ( -9.079631412095446663, 13.97901777655708067, 4.999999999999364064 ) ) ;
#22487 =( NAMED_UNIT ( * ) SI_UNIT ( $, .STERADIAN. ) SOLID_ANGLE_UNIT ( ) );
#22488 = ADVANCED_FACE ( 'NONE', ( #64459 ), #88727, .F. ) ;
#22489 = CARTESIAN_POINT ( 'NONE',  ( -42.51305782313426818, 484.3273291304232089, -1.912516135270148743 ) ) ;
#22490 = ORIENTED_EDGE ( 'NONE', *, *, #87474, .T. ) ;
#22491 = DIRECTION ( 'NONE',  ( 0.000000000000000000, 1.000000000000000000, 0.000000000000000000 ) ) ;
#22492 = EDGE_CURVE ( 'NONE', #28856, #87378, #97374, .T. ) ;
#22493 = CARTESIAN_POINT ( 'NONE',  ( 8.000000000000000000, 9.797174393178825657E-16, -9.274828571428571422 ) ) ;
#22494 = CARTESIAN_POINT ( 'NONE',  ( 37.98648538845074540, -60.00000000000001421, 49.46892715370867677 ) ) ;
#22495 = CARTESIAN_POINT ( 'NONE',  ( -101.1095592966768208, -29.99999999999999645, 175.2763840439222633 ) ) ;
#22496 = CARTESIAN_POINT ( 'NONE',  ( 0.000000000000000000, 0.000000000000000000, -4.814498510800145681 ) ) ;
#22497 = CARTESIAN_POINT ( 'NONE',  ( 45.10052333452469497, -57.68305435951591420, 65.38036528418656701 ) ) ;
#22498 = STYLED_ITEM ( 'NONE', ( #100845 ), #92066 ) ;
#22500 = SURFACE_STYLE_USAGE ( .BOTH. , #64008 ) ;
#22499 = DIRECTION ( 'NONE',  ( -1.000000000000000000, -1.224606353822377258E-16, -0.000000000000000000 ) ) ;
#22501 = CARTESIAN_POINT ( 'NONE',  ( -49.55398223496038668, 40.83861519502255533, -42.37453762653911582 ) ) ;
#22502 = VECTOR ( 'NONE', #96965, 1000.000000000000000 ) ;
#22503 = CARTESIAN_POINT ( 'NONE',  ( -17.59947254824060536, 50.00000000000000000, 62.68871018980012622 ) ) ;
#22504 = CARTESIAN_POINT ( 'NONE',  ( -9.240220675753736401, 15.98931925350938243, 3.827754797005848530 ) ) ;
#22505 = CARTESIAN_POINT ( 'NONE',  ( -46.00000000000000000, 437.9690125970931831, 14.09127711025708507 ) ) ;
#22506 = CARTESIAN_POINT ( 'NONE',  ( -12.66494344392306104, -60.00000000000002132, 39.70460679373117330 ) ) ;
#22507 = FACE_OUTER_BOUND ( 'NONE', #32768, .T. ) ;
#22508 = FACE_OUTER_BOUND ( 'NONE', #27577, .T. ) ;
#22509 = ORIENTED_EDGE ( 'NONE', *, *, #11178, .F. ) ;
#22510 = CARTESIAN_POINT ( 'NONE',  ( 17.50000000000003197, 52.00000000000194689, 59.64162155654130260 ) ) ;
#22511 = CARTESIAN_POINT ( 'NONE',  ( -15.72133563019506930, -42.95781215222940830, 31.23342921828535523 ) ) ;
#22512 =( BOUNDED_CURVE ( )  B_SPLINE_CURVE ( 2, ( #87695, #20357, #37045, #78518, #47207, #5180, #53720, #80109, #30535 ),
 .UNSPECIFIED., .F., .F. ) 
 B_SPLINE_CURVE_WITH_KNOTS ( ( 3, 2, 2, 2, 3 ),
 ( 0.6617647058823528106, 0.6691176470588233727, 0.6764705882352941568, 0.6838235294117647189, 0.6911764705882352811 ),
 .UNSPECIFIED. ) 
 CURVE ( )  GEOMETRIC_REPRESENTATION_ITEM ( )  RATIONAL_B_SPLINE_CURVE ( ( 1.000000000000001110, 0.9238795325112856283, 1.000000000000000000, 0.9238795325112867385, 1.000000000000000000, 0.9238795325112867385, 1.000000000000000000, 0.9238795325112867385, 1.000000000000000000 ) ) 
 REPRESENTATION_ITEM ( '' )  );
#22514 = CARTESIAN_POINT ( 'NONE',  ( 96.86866073052655679, 6.123233995736568081E-16, -5.000000000000011546 ) ) ;
#22513 = CARTESIAN_POINT ( 'NONE',  ( -99.12185298998538485, -59.99999999999997868, 109.9295474875607397 ) ) ;
#22515 = EDGE_LOOP ( 'NONE', ( #39895, #28541 ) ) ;
#22516 = LINE ( 'NONE', #102875, #102779 ) ;
#22517 = CARTESIAN_POINT ( 'NONE',  ( -13.41428277683274395, 42.83120269148118098, -92.05841013448643650 ) ) ;
#22518 = CARTESIAN_POINT ( 'NONE',  ( 7.251694438969768619, 41.54830556103024719, -59.82648080958256287 ) ) ;
#22519 = ADVANCED_FACE ( 'NONE', ( #75719 ), #2677, .T. ) ;
#22520 = CARTESIAN_POINT ( 'NONE',  ( 15.51015326906917124, 2.604283801340223192, 0.3849796309686537299 ) ) ;
#22521 = CARTESIAN_POINT ( 'NONE',  ( 61.80701749067248585, -60.00000000000001421, 106.6076082615842040 ) ) ;
#22522 = DIRECTION ( 'NONE',  ( 0.000000000000000000, 0.000000000000000000, 1.000000000000000000 ) ) ;
#22523 = ORIENTED_EDGE ( 'NONE', *, *, #55341, .T. ) ;
#22524 = CARTESIAN_POINT ( 'NONE',  ( -7.228211769744709692, -29.99999999999998224, 2.785121603415316116 ) ) ;
#22525 = CARTESIAN_POINT ( 'NONE',  ( 4.472135954999579610, -85.00000000000000000, -4.000000000000001776 ) ) ;
#22527 = FACE_OUTER_BOUND ( 'NONE', #74051, .T. ) ;
#22526 = CARTESIAN_POINT ( 'NONE',  ( 29.53284356080077444, -60.00000000000004974, 45.26708560465603171 ) ) ;
#22528 = B_SPLINE_CURVE_WITH_KNOTS ( 'NONE', 3,
 ( #60074, #91364, #100494, #26137, #9344, #93487, #17479, #83773, #59529, #68689, #19636, #27726, #19098, #51410, #42796, #50870, #84851, #26651, #10934, #52469, #697, #92397, #33664, #42256 ),
 .UNSPECIFIED., .F., .F.,
 ( 4, 2, 2, 2, 2, 2, 2, 2, 2, 2, 2, 4 ),
 ( 0.000000000000000000, 0.0009738897914509524363, 0.001947779582901903572, 0.003895559165803803674, 0.004869448957254753074, 0.005843338748705703342, 0.007791118331607603011, 0.009738897914509502679, 0.01168667749741140321, 0.01363445708031330375, 0.01460834687176425575, 0.01558223666321520776 ),
 .UNSPECIFIED. ) ;
#22529 = DIRECTION ( 'NONE',  ( -1.000000000000000000, -1.224606353822377258E-16, -0.000000000000000000 ) ) ;
#22530 = SURFACE_STYLE_USAGE ( .BOTH. , #96399 ) ;
#22531 = ORIENTED_EDGE ( 'NONE', *, *, #69165, .T. ) ;
#22532 = AXIS2_PLACEMENT_3D ( 'NONE', #54227, #87164, #86649 ) ;
#22533 = EDGE_LOOP ( 'NONE', ( #84328, #81169, #21359, #64487, #57079 ) ) ;
#22534 = CARTESIAN_POINT ( 'NONE',  ( -28.80272083960844043, 315.1418830885958187, 12.69311001326675736 ) ) ;
#22535 = ORIENTED_EDGE ( 'NONE', *, *, #42754, .F. ) ;
#22536 = CIRCLE ( 'NONE', #50051, 4.000000000000007105 ) ;
#22537 = CARTESIAN_POINT ( 'NONE',  ( 0.000000000000000000, 60.00000000000000000, 0.000000000000000000 ) ) ;
#22538 = ORIENTED_EDGE ( 'NONE', *, *, #91659, .F. ) ;
#22539 = SURFACE_STYLE_USAGE ( .BOTH. , #71052 ) ;
#22540 = DIRECTION ( 'NONE',  ( 1.000000000000000000, 1.224606353822377258E-16, 0.000000000000000000 ) ) ;
#22541 = CARTESIAN_POINT ( 'NONE',  ( -112.1437713539201866, -59.99999999994144417, 141.3908632541163115 ) ) ;
#22542 = CONICAL_SURFACE ( 'NONE', #72470, 4.172000000000009479, 0.9599310885968813656 ) ;
#22543 = CARTESIAN_POINT ( 'NONE',  ( 46.00000000000570566, 485.9629172155148922, 0.8649761565702976940 ) ) ;
#22544 = CARTESIAN_POINT ( 'NONE',  ( 72.76612462108283808, -59.99999999999997868, 160.3201290646432824 ) ) ;
#22545 = PRESENTATION_STYLE_ASSIGNMENT (( #5787 ) ) ;
#22546 = DIRECTION ( 'NONE',  ( 0.000000000000000000, -1.000000000000000000, 0.000000000000000000 ) ) ;
#22548 = CARTESIAN_POINT ( 'NONE',  ( 9.282106017489308414, -46.43475792098434596, 31.63186067789786904 ) ) ;
#22547 = CARTESIAN_POINT ( 'NONE',  ( -113.8519240760089133, -60.00000000000002842, 157.1483645435538108 ) ) ;
#22549 = CARTESIAN_POINT ( 'NONE',  ( 83.27820862095059340, -37.99999999999996447, 29.76319823405992082 ) ) ;
#22550 = CARTESIAN_POINT ( 'NONE',  ( 1.224646799147352665E-15, -79.93083296558610584, -95.00000000000000000 ) ) ;
#22551 = ADVANCED_FACE ( 'NONE', ( #43361 ), #74964, .T. ) ;
#22552 = CARTESIAN_POINT ( 'NONE',  ( -47.02002132585242578, -39.52884493021316104, 46.23036517761990893 ) ) ;
#22553 = CIRCLE ( 'NONE', #15653, 4.000000000000000888 ) ;
#22554 = CARTESIAN_POINT ( 'NONE',  ( -15.30771400658740689, 18.64284798592982639, 35.25047262264921244 ) ) ;
#22555 = ORIENTED_EDGE ( 'NONE', *, *, #40008, .F. ) ;
#22556 = CARTESIAN_POINT ( 'NONE',  ( 40.19525959764776957, 459.8689882208901736, 1.906254677025529531 ) ) ;
#22557 = CARTESIAN_POINT ( 'NONE',  ( 8.099999999999999645, 7.505553499465140277, 0.000000000000000000 ) ) ;
#22558 = CARTESIAN_POINT ( 'NONE',  ( -38.85446894546474539, 460.8903912184078422, 2.218456751110488678 ) ) ;
#22559 = ADVANCED_FACE ( 'NONE', ( #16968 ), #60106, .F. ) ;
#22560 = AXIS2_PLACEMENT_3D ( 'NONE', #2867, #50879, #1797 ) ;
#22561 =( LENGTH_UNIT ( ) NAMED_UNIT ( * ) SI_UNIT ( .MILLI., .METRE. ) );
#22562 = CARTESIAN_POINT ( 'NONE',  ( 30.95643954367146833, 313.8918926584737505, -7.857037206977866006 ) ) ;
#22563 = ORIENTED_EDGE ( 'NONE', *, *, #10884, .F. ) ;
#22564 = CARTESIAN_POINT ( 'NONE',  ( -11.36340450468866337, -9.490057094874892130, 18.81418650344063792 ) ) ;
#22565 = ORIENTED_EDGE ( 'NONE', *, *, #101267, .F. ) ;
#22566 = CARTESIAN_POINT ( 'NONE',  ( 108.0570916867202556, -29.99999999999827693, 188.3392959967954994 ) ) ;
#22567 = PRESENTATION_STYLE_ASSIGNMENT (( #97460 ) ) ;
#22568 = CARTESIAN_POINT ( 'NONE',  ( 5.787518022136032947, 41.99999999999999289, -59.87256586542197567 ) ) ;
#22569 = SURFACE_SIDE_STYLE ('',( #57005 ) ) ;
#22570 = CARTESIAN_POINT ( 'NONE',  ( 97.41453105692403369, -29.99999999999999645, 190.9275840960229118 ) ) ;
#22571 = FACE_OUTER_BOUND ( 'NONE', #32242, .T. ) ;
#22572 = VERTEX_POINT ( 'NONE', #9915 ) ;
#22573 = EDGE_LOOP ( 'NONE', ( #44779, #70757, #54051, #60016 ) ) ;
#22574 = EDGE_LOOP ( 'NONE', ( #45529, #62561, #74926, #7625 ) ) ;
#22575 = LINE ( 'NONE', #105056, #47399 ) ;
#22576 = DIRECTION ( 'NONE',  ( 0.000000000000000000, -1.000000000000000000, 0.000000000000000000 ) ) ;
#22577 = AXIS2_PLACEMENT_3D ( 'NONE', #57908, #75153, #1246 ) ;
#22578 = DIRECTION ( 'NONE',  ( 0.1270361284032394955, -0.9918980905719678720, 0.000000000000000000 ) ) ;
#22579 = VERTEX_POINT ( 'NONE', #1813 ) ;
#22580 = DIRECTION ( 'NONE',  ( -0.000000000000000000, -1.000000000000000000, -0.000000000000000000 ) ) ;
#22581 = AXIS2_PLACEMENT_3D ( 'NONE', #97358, #97896, #56892 ) ;
#22582 = ORIENTED_EDGE ( 'NONE', *, *, #39934, .T. ) ;
#22583 = CARTESIAN_POINT ( 'NONE',  ( 0.000000000000000000, 70.00000000000000000, -10.00000000000000178 ) ) ;
#22584 = CARTESIAN_POINT ( 'NONE',  ( 96.06384290910234824, -38.48472166148474827, 201.2020660132053536 ) ) ;
#22585 = CARTESIAN_POINT ( 'NONE',  ( 11.10339240064335975, 8.425011028989088047, 9.820949472247303191 ) ) ;
#22586 = PRODUCT_RELATED_PRODUCT_CATEGORY ( 'part', '', ( #43795 ) ) ;
#22587 = CARTESIAN_POINT ( 'NONE',  ( 86.94475506094372008, -60.16925933034688967, -3.940419869023602750 ) ) ;
#22588 = CARTESIAN_POINT ( 'NONE',  ( 63.28416903638269275, -38.00000000000000711, 80.42582590836656209 ) ) ;
#22589 = CARTESIAN_POINT ( 'NONE',  ( 35.76362145159366435, 307.1564523868753440, 12.84684258606850271 ) ) ;
#22590 = CARTESIAN_POINT ( 'NONE',  ( 3.313708498984743844, -24.96875000409677625, 8.000000000000017764 ) ) ;
#22591 = CYLINDRICAL_SURFACE ( 'NONE', #20663, 4.000000000000000000 ) ;
#22592 = DIRECTION ( 'NONE',  ( 0.000000000000000000, 1.000000000000000000, 0.000000000000000000 ) ) ;
#22593 = CARTESIAN_POINT ( 'NONE',  ( 72.85555555555556850, 6.915964383211875250E-15, 0.000000000000000000 ) ) ;
#22594 = VERTEX_POINT ( 'NONE', #26680 ) ;
#22595 = DIRECTION ( 'NONE',  ( -0.000000000000000000, -0.000000000000000000, -1.000000000000000000 ) ) ;
#22596 = CARTESIAN_POINT ( 'NONE',  ( -34.05871433650573010, 463.4203836794940230, 6.469249789599879286 ) ) ;
#22597 = AXIS2_PLACEMENT_3D ( 'NONE', #9111, #8051, #49036 ) ;
#22598 = CARTESIAN_POINT ( 'NONE',  ( -2.942711189959360762, 97.39608628791339129, 5.000000000000000000 ) ) ;
#22599 = ORIENTED_EDGE ( 'NONE', *, *, #46210, .T. ) ;
#22600 = PLANE ( 'NONE',  #4487 ) ;
#22601 = CARTESIAN_POINT ( 'NONE',  ( -31.74043077603787921, 299.2833385164202582, 2.924916184740101510 ) ) ;
#22602 = DIRECTION ( 'NONE',  ( 0.000000000000000000, 1.000000000000000000, 0.000000000000000000 ) ) ;
#22603 = UNCERTAINTY_MEASURE_WITH_UNIT (LENGTH_MEASURE( 1.000000000000000082E-05 ), #87873, 'distance_accuracy_value', 'NONE');
#22604 = EDGE_CURVE ( 'NONE', #41058, #72311, #88773, .T. ) ;
#22605 = LINE ( 'NONE', #106113, #71165 ) ;
#22606 = CARTESIAN_POINT ( 'NONE',  ( 4.898587196589412829E-16, -13.62499999999999112, -8.000000000000000000 ) ) ;
#22607 = CARTESIAN_POINT ( 'NONE',  ( 33.70467876106231131, -25.90788300163896452, 41.06987389266631538 ) ) ;
#22608 = EDGE_CURVE ( 'NONE', #89905, #67790, #9261, .T. ) ;
#22609 = CARTESIAN_POINT ( 'NONE',  ( 15.71080878184230301, 303.5558203657541299, 9.874086874886266685 ) ) ;
#22610 = ORIENTED_EDGE ( 'NONE', *, *, #4729, .T. ) ;
#22611 = CARTESIAN_POINT ( 'NONE',  ( 84.82672610503449562, -46.56838776579275674, 187.1272610940604579 ) ) ;
#22612 = CARTESIAN_POINT ( 'NONE',  ( -38.66211280991526422, 27.30187666962869031, 12.83133664711218991 ) ) ;
#22613 = SURFACE_STYLE_USAGE ( .BOTH. , #14999 ) ;
#22614 = VERTEX_POINT ( 'NONE', #9368 ) ;
#22615 = CARTESIAN_POINT ( 'NONE',  ( 94.40918845809700599, -57.67101149516233249, -0.2801014365498262215 ) ) ;
#22616 = AXIS2_PLACEMENT_3D ( 'NONE', #25014, #75109, #24500 ) ;
#22617 = CARTESIAN_POINT ( 'NONE',  ( 59.41111111111111143, 6.915964383211875250E-15, 0.000000000000000000 ) ) ;
#22618 = CARTESIAN_POINT ( 'NONE',  ( 17.82150094932208262, -4.333298119783735913, -1.872127852956306571 ) ) ;
#22619 = EDGE_CURVE ( 'NONE', #96778, #71668, #50867, .T. ) ;
#22620 = VECTOR ( 'NONE', #79458, 1000.000000000000227 ) ;
#22621 = EDGE_CURVE ( 'NONE', #21783, #61515, #78447, .T. ) ;
#22622 = AXIS2_PLACEMENT_3D ( 'NONE', #83484, #33914, #8528 ) ;
#22623 = EDGE_CURVE ( 'NONE', #81976, #19129, #67162, .T. ) ;
#22624 = CARTESIAN_POINT ( 'NONE',  ( -53.26687959709935427, -38.00000000000001421, 56.03731585654522007 ) ) ;
#22625 = AXIS2_PLACEMENT_3D ( 'NONE', #52328, #101948, #19491 ) ;
#22626 = CARTESIAN_POINT ( 'NONE',  ( -8.922269033012433681, -5.000000000000000000, 5.219866590718518218 ) ) ;
#22627 = LINE ( 'NONE', #46854, #61867 ) ;
#22629 = CARTESIAN_POINT ( 'NONE',  ( -14.11595029531626011, 2.410436752329291110, 5.024000119293333455 ) ) ;
#22628 = CARTESIAN_POINT ( 'NONE',  ( 37.50105657201422105, 463.9558240680319159, 19.48687553971743469 ) ) ;
#22630 = FACE_BOUND ( 'NONE', #43366, .T. ) ;
#22631 = LINE ( 'NONE', #105624, #69875 ) ;
#22632 = CARTESIAN_POINT ( 'NONE',  ( 42.98746414932995208, 1.482358050883964840E-15, 0.000000000000000000 ) ) ;
#22633 = CARTESIAN_POINT ( 'NONE',  ( 43.52075891743746894, 484.7805561108181109, 4.063293749111048569 ) ) ;
#22634 = EDGE_LOOP ( 'NONE', ( #42892, #1421, #59889, #46876 ) ) ;
#22635 =( NAMED_UNIT ( * ) SI_UNIT ( $, .STERADIAN. ) SOLID_ANGLE_UNIT ( ) );
#22636 = CARTESIAN_POINT ( 'NONE',  ( -10.05811987131503038, -16.24350643256279625, -34.80807818328759851 ) ) ;
#22638 = CARTESIAN_POINT ( 'NONE',  ( -61.40929618123364264, -47.40892651706064953, -27.09027404592079336 ) ) ;
#22637 =( NAMED_UNIT ( * ) PLANE_ANGLE_UNIT ( ) SI_UNIT ( $, .RADIAN. ) );
#22639 = ORIENTED_EDGE ( 'NONE', *, *, #57916, .T. ) ;
#22640 = CARTESIAN_POINT ( 'NONE',  ( -30.00000000000000000, 0.000000000000000000, -13.00000000000000000 ) ) ;
#22641 = VERTEX_POINT ( 'NONE', #51966 ) ;
#22642 = ADVANCED_FACE ( 'NONE', ( #90850 ), #62988, .T. ) ;
#22643 = DIRECTION ( 'NONE',  ( 0.000000000000000000, 0.000000000000000000, -1.000000000000000000 ) ) ;
#22644 = FACE_OUTER_BOUND ( 'NONE', #67610, .T. ) ;
#22645 = CARTESIAN_POINT ( 'NONE',  ( -92.50385710939508499, -59.99999999999999289, -1.307865944661959601 ) ) ;
#22646 = ORIENTED_EDGE ( 'NONE', *, *, #102470, .F. ) ;
#22647 = CARTESIAN_POINT ( 'NONE',  ( 5.656854249492380582, -27.50000000409677270, -5.656854249492379694 ) ) ;
#22648 = CARTESIAN_POINT ( 'NONE',  ( -7.799656765069284958, 54.21738860527597126, -1.774909779959811473 ) ) ;
#22649 = CARTESIAN_POINT ( 'NONE',  ( 98.35997379234478899, -37.76608977019981239, 192.3278014986217954 ) ) ;
#22650 = DIRECTION ( 'NONE',  ( 0.000000000000000000, -3.466879843239602429E-16, -1.000000000000000000 ) ) ;
#22651 = CARTESIAN_POINT ( 'NONE',  ( -84.67995877784876768, -22.10573975591750795, 157.8301934640955437 ) ) ;
#22652 = VERTEX_POINT ( 'NONE', #724 ) ;
#22653 = ORIENTED_EDGE ( 'NONE', *, *, #586, .T. ) ;
#22654 = ORIENTED_EDGE ( 'NONE', *, *, #51592, .F. ) ;
#22655 = CARTESIAN_POINT ( 'NONE',  ( 32.94330508143927716, -4.999999999999990230, 0.000000000000000000 ) ) ;
#22656 = ADVANCED_FACE ( 'NONE', ( #33692 ), #98911, .F. ) ;
#22657 = CARTESIAN_POINT ( 'NONE',  ( -5.000000000000039968, -13.16121988547070742, 12.48675270919698299 ) ) ;
#22658 = DIRECTION ( 'NONE',  ( 0.000000000000000000, 0.000000000000000000, 1.000000000000000000 ) ) ;
#22659 = ORIENTED_EDGE ( 'NONE', *, *, #9265, .T. ) ;
#22660 = AXIS2_PLACEMENT_3D ( 'NONE', #47727, #15368, #97879 ) ;
#22661 = CARTESIAN_POINT ( 'NONE',  ( -74.79081370483122271, -57.58316160299655451, 190.1003635006443346 ) ) ;
#22662 = CARTESIAN_POINT ( 'NONE',  ( -3.400000000000000355, 4.163799117101001052E-16, -7.259124522925831435 ) ) ;
#22663 = CARTESIAN_POINT ( 'NONE',  ( -52.56483885390523625, 48.00000000000000000, -38.23529411764706509 ) ) ;
#22664 = CARTESIAN_POINT ( 'NONE',  ( 0.000000000000000000, 49.00000000000000000, 66.50000000000000000 ) ) ;
#22665 = FACE_BOUND ( 'NONE', #73274, .T. ) ;
#22666 = CARTESIAN_POINT ( 'NONE',  ( 82.45758146611665040, -29.99999999999998579, -23.17547892442675916 ) ) ;
#22667 = SHAPE_REPRESENTATION ( 'hex flange bolt_din_DIN 6921 - M8 x 30 x 30-S', ( #10728 ), #57385 ) ;
#22668 = CARTESIAN_POINT ( 'NONE',  ( -65.47633411339396048, -60.00000000000000000, 130.5853305762684329 ) ) ;
#22669 = CARTESIAN_POINT ( 'NONE',  ( -52.14842760859697535, -60.31282274427849188, 62.32353961952082955 ) ) ;
#22670 = ORIENTED_EDGE ( 'NONE', *, *, #97534, .F. ) ;
#22671 = CARTESIAN_POINT ( 'NONE',  ( 91.37578371391791165, 1.016364837396684119E-14, 0.000000000000000000 ) ) ;
#22672 = VERTEX_POINT ( 'NONE', #66566 ) ;
#22673 = CARTESIAN_POINT ( 'NONE',  ( -99.43116831379333576, -37.79880016511722118, 191.4274298609611833 ) ) ;
#22674 = CARTESIAN_POINT ( 'NONE',  ( -30.64007947709922419, 12.99638611018202639, -41.66214316769399773 ) ) ;
#22675 = EDGE_CURVE ( 'NONE', #55265, #61594, #93938, .T. ) ;
#22676 = ORIENTED_EDGE ( 'NONE', *, *, #32633, .T. ) ;
#22677 = CARTESIAN_POINT ( 'NONE',  ( 19.27285195068759549, 49.83909218305972644, 61.40325362178533908 ) ) ;
#22679 = AXIS2_PLACEMENT_3D ( 'NONE', #7588, #99252, #89600 ) ;
#22678 = CARTESIAN_POINT ( 'NONE',  ( 108.7231916027115091, -38.35574387428263066, 143.1493928306014709 ) ) ;
#22680 = DIRECTION ( 'NONE',  ( 0.000000000000000000, -1.000000000000000000, 0.000000000000000000 ) ) ;
#22681 = CARTESIAN_POINT ( 'NONE',  ( 6.837824896291514243, 3.947820044545422569, -6.564402953523715389 ) ) ;
#22682 = CIRCLE ( 'NONE', #82933, 5.000000000000002665 ) ;
#22683 = CARTESIAN_POINT ( 'NONE',  ( -7.169728294440821159, 294.7252185496461721, 1.910214800425284132 ) ) ;
#22684 = CARTESIAN_POINT ( 'NONE',  ( 43.52578837347088836, 465.2717874277798842, 9.360669990306849542 ) ) ;
#22685 = CARTESIAN_POINT ( 'NONE',  ( 62.37459373232455562, -30.00000000000000711, 73.01631233425933942 ) ) ;
#22686 = AXIS2_PLACEMENT_3D ( 'NONE', #25251, #40869, #23653 ) ;
#22687 = EDGE_CURVE ( 'NONE', #32439, #16675, #87689, .T. ) ;
#22688 = DIRECTION ( 'NONE',  ( 0.000000000000000000, 0.000000000000000000, 1.000000000000000000 ) ) ;
#22689 = LINE ( 'NONE', #88464, #80205 ) ;
#22690 = CARTESIAN_POINT ( 'NONE',  ( 4.369287899246201867, -48.87003977535613330, 104.3947014718172142 ) ) ;
#22691 = CARTESIAN_POINT ( 'NONE',  ( -37.69506754384124747, 484.8919167041191827, -3.620297613827866190 ) ) ;
#22692 = ORIENTED_EDGE ( 'NONE', *, *, #10150, .F. ) ;
#22693 = ORIENTED_EDGE ( 'NONE', *, *, #65172, .T. ) ;
#22694 = CARTESIAN_POINT ( 'NONE',  ( 48.90658294110461668, -46.43936590027043820, 51.21113800430314456 ) ) ;
#22695 = CARTESIAN_POINT ( 'NONE',  ( 43.10000000000000142, 3.309500000000003439, 4.052968581778167743E-16 ) ) ;
#22696 = COLOUR_RGB ( '', 0.09019608, 0.27058824, 0.51372549) ;
#22697 = CARTESIAN_POINT ( 'NONE',  ( -6.012758288945200924, 14.79064451834496552, -3.586184577130258067 ) ) ;
#22698 = AXIS2_PLACEMENT_3D ( 'NONE', #61332, #45669, #69420 ) ;
#22699 = CARTESIAN_POINT ( 'NONE',  ( -104.3457841577212548, -38.40612335771167807, 198.1033792868130092 ) ) ;
#22700 = ORIENTED_EDGE ( 'NONE', *, *, #79000, .F. ) ;
#22701 = CARTESIAN_POINT ( 'NONE',  ( 91.21127784508071557, -38.35815842224639027, -0.8486547785704385838 ) ) ;
#22702 = CARTESIAN_POINT ( 'NONE',  ( 11.09396121529365509, 10.59760035510856468, -9.714813416437120708 ) ) ;
#22703 = CARTESIAN_POINT ( 'NONE',  ( -19.47693998750411026, 49.99334787011666492, 60.32562116054356949 ) ) ;
#22704 =( NAMED_UNIT ( * ) SI_UNIT ( $, .STERADIAN. ) SOLID_ANGLE_UNIT ( ) );
#22705 = CARTESIAN_POINT ( 'NONE',  ( 99.36430944222280459, -37.84839370588183982, 135.1400454678828567 ) ) ;
#22706 = DIRECTION ( 'NONE',  ( 0.000000000000000000, 0.000000000000000000, -1.000000000000000000 ) ) ;
#22707 = CARTESIAN_POINT ( 'NONE',  ( 33.21585456055980501, 485.3968598104756325, 4.030361751232280909 ) ) ;
#22708 = CARTESIAN_POINT ( 'NONE',  ( 4.898587196589412829E-16, 0.5000000000000000000, 4.000000000000000000 ) ) ;
#22709 = DIRECTION ( 'NONE',  ( 0.000000000000000000, 0.000000000000000000, -1.000000000000000000 ) ) ;
#22710 = CARTESIAN_POINT ( 'NONE',  ( 83.61247817121171977, -59.99999999999999289, 199.2525199516834675 ) ) ;
#22711 = EDGE_CURVE ( 'NONE', #2515, #43471, #58485, .T. ) ;
#22712 = DIRECTION ( 'NONE',  ( 0.000000000000000000, 0.000000000000000000, 1.000000000000000000 ) ) ;
#22713 = ORIENTED_EDGE ( 'NONE', *, *, #63982, .F. ) ;
#22714 = CARTESIAN_POINT ( 'NONE',  ( 56.51965637257737285, -56.85211480795176442, 71.22111066778985844 ) ) ;
#22715 = CARTESIAN_POINT ( 'NONE',  ( -34.86904551647302242, 301.2900558943937881, -8.550442243075442761 ) ) ;
#22716 = CARTESIAN_POINT ( 'NONE',  ( 7.344361273354514275, 32.44560530588525182, -3.175733139645580572 ) ) ;
#22717 = AXIS2_PLACEMENT_3D ( 'NONE', #97690, #24904, #8691 ) ;
#22718 = CARTESIAN_POINT ( 'NONE',  ( -7.413471587080155523, 27.35647840831672895, -3.013058070223542551 ) ) ;
#22719 = EDGE_LOOP ( 'NONE', ( #63136, #84451, #89028, #93403, #57815, #21346, #105398 ) ) ;
#22721 = CARTESIAN_POINT ( 'NONE',  ( -14.77980331624359955, 22.77528010646188505, -2.502200611405557051 ) ) ;
#22720 = CARTESIAN_POINT ( 'NONE',  ( -93.80762359828875674, -38.49308346633976186, 201.2011921042621623 ) ) ;
#22722 = DIRECTION ( 'NONE',  ( -0.000000000000000000, -1.000000000000000000, -0.000000000000000000 ) ) ;
#22723 = CARTESIAN_POINT ( 'NONE',  ( 31.41956315632691599, 380.3354942127950835, 23.41885142240392881 ) ) ;
#22724 = FILL_AREA_STYLE ('',( #46440 ) ) ;
#22725 = CARTESIAN_POINT ( 'NONE',  ( -3.313708498984760720, -31.53124999999999645, -8.000000000000000000 ) ) ;
#22726 = STYLED_ITEM ( 'NONE', ( #80611 ), #93555 ) ;
#22727 = CARTESIAN_POINT ( 'NONE',  ( 9.739726766104318756, -5.000000000001365130, -87.61747884499031613 ) ) ;
#22728 = CARTESIAN_POINT ( 'NONE',  ( 35.59999999999999432, 1.533819458162526451E-15, 0.000000000000000000 ) ) ;
#22729 = ORIENTED_EDGE ( 'NONE', *, *, #1218, .F. ) ;
#22730 = CARTESIAN_POINT ( 'NONE',  ( 83.89975545334559115, -35.96486616408294879, 172.8035680471575972 ) ) ;
#22731 = CARTESIAN_POINT ( 'NONE',  ( 8.959983754892499874, 15.87132973532702174, -2.602085213965211825E-15 ) ) ;
#22732 = DIRECTION ( 'NONE',  ( -1.000000000000000000, -1.224606353822377258E-16, -0.000000000000000000 ) ) ;
#22733 = ORIENTED_EDGE ( 'NONE', *, *, #104657, .T. ) ;
#22734 = CARTESIAN_POINT ( 'NONE',  ( -24.15840962162803507, 303.6456723108300366, -9.828972323003243972 ) ) ;
#22735 = CARTESIAN_POINT ( 'NONE',  ( 7.701342750608461962, -4.999999999995311306, -18.36411236461295360 ) ) ;
#22736 = CARTESIAN_POINT ( 'NONE',  ( 38.85520749938564933, 460.5777845577952689, 2.285580541808310162 ) ) ;
#22737 = CARTESIAN_POINT ( 'NONE',  ( -9.610124387803624657, 50.00000000000001421, -77.63937538513252434 ) ) ;
#22738 = DIRECTION ( 'NONE',  ( -0.000000000000000000, -1.000000000000000000, -0.000000000000000000 ) ) ;
#22739 = EDGE_CURVE ( 'NONE', #8224, #61663, #37431, .T. ) ;
#22740 = FACE_OUTER_BOUND ( 'NONE', #87414, .T. ) ;
#22741 = EDGE_CURVE ( 'NONE', #90030, #37979, #16469, .T. ) ;
#22742 = ORIENTED_EDGE ( 'NONE', *, *, #50278, .T. ) ;
#22743 = APPLICATION_PROTOCOL_DEFINITION ( 'draft international standard', 'automotive_design', 1998, #25254 ) ;
#22744 = ADVANCED_FACE ( 'NONE', ( #62231 ), #43882, .T. ) ;
#22745 = CARTESIAN_POINT ( 'NONE',  ( 38.78863291229748000, 25.16502836992622960, 12.51984068333550759 ) ) ;
#22746 = CARTESIAN_POINT ( 'NONE',  ( 1.249602959316253648, 25.67499641899253859, 39.33778172269227724 ) ) ;
#22748 = CARTESIAN_POINT ( 'NONE',  ( -12.60033841120074527, 9.255502400745754699, -9.287856882556875249 ) ) ;
#22747 = CARTESIAN_POINT ( 'NONE',  ( 0.000000000000000000, 0.9999999999999970024, 0.000000000000000000 ) ) ;
#22749 = CARTESIAN_POINT ( 'NONE',  ( -7.188101187500000044, -21.40625000204838457, -8.802885111219163269E-16 ) ) ;
#22750 = CARTESIAN_POINT ( 'NONE',  ( -29.14590962570478183, 18.82625154611908513, -39.72466805691968972 ) ) ;
#22751 = FILL_AREA_STYLE ('',( #96616 ) ) ;
#22752 = ORIENTED_EDGE ( 'NONE', *, *, #426, .T. ) ;
#22753 = AXIS2_PLACEMENT_3D ( 'NONE', #43269, #92870, #58385 ) ;
#22754 = DIRECTION ( 'NONE',  ( -1.000000000000000000, -1.224606353822377258E-16, -0.000000000000000000 ) ) ;
#22755 = DIRECTION ( 'NONE',  ( 0.000000000000000000, 0.000000000000000000, 1.000000000000000000 ) ) ;
#22756 = CIRCLE ( 'NONE', #5558, 60.50000000000000000 ) ;
#22757 = CARTESIAN_POINT ( 'NONE',  ( -8.972157809163535447, 136.3338258388613440, -5.000000000000003553 ) ) ;
#22758 = DIRECTION ( 'NONE',  ( -1.000000000000000000, -1.224606353822377258E-16, -0.000000000000000000 ) ) ;
#22759 = CARTESIAN_POINT ( 'NONE',  ( 6.644028492724100232, 3.901260126080569712, 6.757180751913672623 ) ) ;
#22760 = ORIENTED_EDGE ( 'NONE', *, *, #88763, .F. ) ;
#22761 = FACE_OUTER_BOUND ( 'NONE', #28101, .T. ) ;
#22762 = CARTESIAN_POINT ( 'NONE',  ( -3.898489618125186240, -9.883538051243510481, 6.752435277548301862 ) ) ;
#22764 = ORIENTED_EDGE ( 'NONE', *, *, #90306, .T. ) ;
#22763 = CONICAL_SURFACE ( 'NONE', #83024, 3.309500000000001663, 0.9599310885968770357 ) ;
#22766 = DIRECTION ( 'NONE',  ( -1.000000000000000000, -1.224606353822377258E-16, -0.000000000000000000 ) ) ;
#22765 = TOROIDAL_SURFACE ( 'NONE', #3809, 15.43455230191221261, 0.5000000000000000000 ) ;
#22767 = EDGE_CURVE ( 'NONE', #95128, #12254, #99137, .T. ) ;
#22768 = CARTESIAN_POINT ( 'NONE',  ( 2.500000000000013767, -30.00000000000000355, -31.87333685190803223 ) ) ;
#22769 = CARTESIAN_POINT ( 'NONE',  ( -112.1928422005939296, -60.00000000000000000, 169.7268788603109897 ) ) ;
#22770 = CARTESIAN_POINT ( 'NONE',  ( 22.91885868373643831, 305.6172567281201964, 10.10309701371861912 ) ) ;
#22771 = CARTESIAN_POINT ( 'NONE',  ( 12.33349330513380693, 1.593028355512270962E-15, 0.000000000000000000 ) ) ;
#22772 = CARTESIAN_POINT ( 'NONE',  ( 0.000000000000000000, 0.000000000000000000, 5.000000000000000000 ) ) ;
#22773 = ADVANCED_FACE ( 'NONE', ( #19665 ), #20739, .F. ) ;
#22774 = CARTESIAN_POINT ( 'NONE',  ( -85.02596717797761983, -28.87890062726760121, 172.9544161691474073 ) ) ;
#22775 = EDGE_LOOP ( 'NONE', ( #42834, #30728 ) ) ;
#22776 = CARTESIAN_POINT ( 'NONE',  ( 4.966176485634622217, 41.64999999999998437, -70.47555195150158625 ) ) ;
#22777 = VERTEX_POINT ( 'NONE', #28275 ) ;
#22778 = FACE_OUTER_BOUND ( 'NONE', #42887, .T. ) ;
#22779 = EDGE_CURVE ( 'NONE', #17532, #3656, #10969, .T. ) ;
#22780 = DIRECTION ( 'NONE',  ( 0.000000000000000000, -1.000000000000000000, 0.000000000000000000 ) ) ;
#22781 = CARTESIAN_POINT ( 'NONE',  ( -82.42609297192525730, -37.83176493496422665, 10.66243034473970397 ) ) ;
#22782 = CARTESIAN_POINT ( 'NONE',  ( -13.25308349978780598, 303.5542394377912956, 9.873748767567704476 ) ) ;
#22783 =( NAMED_UNIT ( * ) PLANE_ANGLE_UNIT ( ) SI_UNIT ( $, .RADIAN. ) );
#22784 = AXIS2_PLACEMENT_3D ( 'NONE', #36248, #92834, #69640 ) ;
#22785 = CARTESIAN_POINT ( 'NONE',  ( 8.441132293727447333, 28.00851920974784548, -5.000000000001228351 ) ) ;
#22786 = CARTESIAN_POINT ( 'NONE',  ( -2.832728918602883450, -6.234773369952756106, -6.171481112545262881 ) ) ;
#22787 = CARTESIAN_POINT ( 'NONE',  ( -3.710639583684274633E-15, 6.732211846623394003, -4.339467034331190298 ) ) ;
#22788 = CARTESIAN_POINT ( 'NONE',  ( 77.57360435794387854, -29.99999999999995026, 180.9683789367223596 ) ) ;
#22789 = CARTESIAN_POINT ( 'NONE',  ( -92.59939171350268339, -30.00000000000003908, 50.96567362325610873 ) ) ;
#22790 = AXIS2_PLACEMENT_3D ( 'NONE', #7594, #7075, #41047 ) ;
#22791 = CARTESIAN_POINT ( 'NONE',  ( -59.99947494157906647, -60.34347021642804521, 82.29587262930701286 ) ) ;
#22792 = ORIENTED_EDGE ( 'NONE', *, *, #87420, .F. ) ;
#22793 = CARTESIAN_POINT ( 'NONE',  ( -58.89672143727629816, 39.42406680342908487, -28.13783362225636608 ) ) ;
#22794 = CARTESIAN_POINT ( 'NONE',  ( 75.17919639455512026, -59.99999999999258904, 192.7260124497774996 ) ) ;
#22795 = ORIENTED_EDGE ( 'NONE', *, *, #33666, .T. ) ;
#22796 = CARTESIAN_POINT ( 'NONE',  ( 3.071111545132248821, -53.39674026084604463, 32.78391494241015636 ) ) ;
#22797 = CARTESIAN_POINT ( 'NONE',  ( -2.977408999572650039, -20.56250000204838813, -7.188101187500000933 ) ) ;
#22798 = VECTOR ( 'NONE', #4509, 1000.000000000000227 ) ;
#22799 = CARTESIAN_POINT ( 'NONE',  ( -4.595881407952572495, -8.933745667986775274, -3.857520671226064568 ) ) ;
#22800 = EDGE_LOOP ( 'NONE', ( #93336, #106381, #35659, #103544 ) ) ;
#22801 = CARTESIAN_POINT ( 'NONE',  ( 3.348045142843516064, -48.90720247195245207, 104.4613934866187179 ) ) ;
#22802 = ORIENTED_EDGE ( 'NONE', *, *, #91691, .F. ) ;
#22803 = CARTESIAN_POINT ( 'NONE',  ( 13.86650669486618881, 1.474610560812782335E-15, 0.000000000000000000 ) ) ;
#22804 = DIRECTION ( 'NONE',  ( -1.000000000000000000, -1.224606353822377258E-16, -0.000000000000000000 ) ) ;
#22805 = CARTESIAN_POINT ( 'NONE',  ( -102.7609246503226359, -60.00000000000000000, 97.23335699513624775 ) ) ;
#22806 = DIRECTION ( 'NONE',  ( 0.000000000000000000, -1.000000000000000000, 0.000000000000000000 ) ) ;
#22807 = CARTESIAN_POINT ( 'NONE',  ( -2.977408999572650039, -26.56250000204838457, -7.188101187500001821 ) ) ;
#22808 = CARTESIAN_POINT ( 'NONE',  ( 32.78741055188843490, 485.3331003366700998, 5.977022408747314053 ) ) ;
#22809 =( BOUNDED_CURVE ( )  B_SPLINE_CURVE ( 2, ( #101819, #37666, #102894 ),
 .UNSPECIFIED., .F., .F. ) 
 B_SPLINE_CURVE_WITH_KNOTS ( ( 3, 3 ),
 ( 0.000000000000000000, 1.000000000000000000 ),
 .UNSPECIFIED. ) 
 CURVE ( )  GEOMETRIC_REPRESENTATION_ITEM ( )  RATIONAL_B_SPLINE_CURVE ( ( 1.000000000000000000, 1.428571428571428825, 1.428571428571429269 ) ) 
 REPRESENTATION_ITEM ( '' )  );
#22810 = CARTESIAN_POINT ( 'NONE',  ( -5.700380315796782504, 53.41403331668362853, -8.464922343797399051 ) ) ;
#22811 = CARTESIAN_POINT ( 'NONE',  ( 5.000000000000000888, -70.02076148470872852, 13.01198664878534750 ) ) ;
#22812 = CARTESIAN_POINT ( 'NONE',  ( -7.996668422904766871, 48.00000000000000000, -91.14546720082618947 ) ) ;
#22813 = ADVANCED_FACE ( 'NONE', ( #12568 ), #23355, .T. ) ;
#22814 = CARTESIAN_POINT ( 'NONE',  ( 11.55222000106535063, -8.857086686608768744, 19.08603404707153217 ) ) ;
#22815 = CARTESIAN_POINT ( 'NONE',  ( -43.28593744481448624, 352.9831048051240714, 11.32485626521906141 ) ) ;
#22816 = CARTESIAN_POINT ( 'NONE',  ( 35.45719195239888677, 325.1427260202198113, -4.543212221563117659 ) ) ;
#22817 = CARTESIAN_POINT ( 'NONE',  ( -38.10162474868671012, -39.51454026084844884, 37.25341933606826217 ) ) ;
#22819 = ADVANCED_FACE ( 'NONE', ( #44428 ), #2881, .T. ) ;
#22818 = ORIENTED_EDGE ( 'NONE', *, *, #95168, .F. ) ;
#22820 = DIRECTION ( 'NONE',  ( -1.000000000000000000, -1.224606353822377258E-16, -0.000000000000000000 ) ) ;
#22821 = CARTESIAN_POINT ( 'NONE',  ( 42.37181301095660757, -46.43334447366678575, 42.48581940379023081 ) ) ;
#22822 = CARTESIAN_POINT ( 'NONE',  ( -19.43146043914380172, -4.830718742626120971E-12, 11.19959342723174522 ) ) ;
#22823 = VERTEX_POINT ( 'NONE', #20195 ) ;
#22824 = EDGE_CURVE ( 'NONE', #55214, #63169, #90533, .T. ) ;
#22825 = CARTESIAN_POINT ( 'NONE',  ( 5.819846122303831137, -4.937269551422891034, 4.448398286272754909 ) ) ;
#22826 = B_SPLINE_CURVE_WITH_KNOTS ( 'NONE', 3,
 ( #16433, #66583, #18593, #84368 ),
 .UNSPECIFIED., .F., .F.,
 ( 4, 4 ),
 ( 2.602085213965210642E-18, 0.001800036990427380601 ),
 .UNSPECIFIED. ) ;
#22827 = CARTESIAN_POINT ( 'NONE',  ( -57.19092749709510315, -38.34444523165630869, 87.83926972307914127 ) ) ;
#22828 = ORIENTED_EDGE ( 'NONE', *, *, #64628, .T. ) ;
#22830 = CARTESIAN_POINT ( 'NONE',  ( -23.96375140441108442, 306.3052962357393199, 10.25885168886986243 ) ) ;
#22829 = CARTESIAN_POINT ( 'NONE',  ( 7.372395903208937895, -5.000000000000000000, -15.53007256938181513 ) ) ;
#22831 = CARTESIAN_POINT ( 'NONE',  ( 40.59999999999999432, 1.533819458162526451E-15, 0.000000000000000000 ) ) ;
#22832 = CARTESIAN_POINT ( 'NONE',  ( 3.313708498984742512, -22.90625000409677270, -8.000000000000019540 ) ) ;
#22833 = FACE_BOUND ( 'NONE', #5958, .T. ) ;
#22834 = CARTESIAN_POINT ( 'NONE',  ( -41.60090381918462299, 436.7951626062874197, 6.075960697891537698 ) ) ;
#22835 = CARTESIAN_POINT ( 'NONE',  ( -49.13563689125227540, 12.95301730162678666, -16.19018188727108409 ) ) ;
#22836 = CARTESIAN_POINT ( 'NONE',  ( 0.4964154566687929981, -8.859816792613649739, 0.6543471694412414941 ) ) ;
#22837 = CARTESIAN_POINT ( 'NONE',  ( 95.37157257520208020, -60.00000000000000711, 51.69444047675210641 ) ) ;
#22838 = B_SPLINE_CURVE_WITH_KNOTS ( 'NONE', 3,
 ( #102773, #13209, #28938, #61810, #37546, #95224, #46138, #79025, #41212, #65498, #40678, #98385, #24534, #82192, #88715, #14806, #105939, #41744, #32624, #81134, #57383, #48754 ),
 .UNSPECIFIED., .F., .F.,
 ( 4, 2, 2, 2, 2, 2, 2, 2, 2, 2, 4 ),
 ( 0.006964068074043574565, 0.007215909760093238735, 0.007467751446142902039, 0.007971434818242223441, 0.008475118190341546578, 0.008726959876391207280, 0.008978801562440866246, 0.009482484934540184179, 0.009986168306639502112, 0.01048985167873882005, 0.01099353505083813798 ),
 .UNSPECIFIED. ) ;
#22840 = FACE_OUTER_BOUND ( 'NONE', #34044, .T. ) ;
#22839 = AXIS2_PLACEMENT_3D ( 'NONE', #64760, #80395, #89036 ) ;
#22841 =( GEOMETRIC_REPRESENTATION_CONTEXT ( 3 ) GLOBAL_UNCERTAINTY_ASSIGNED_CONTEXT ( ( #41927 ) ) GLOBAL_UNIT_ASSIGNED_CONTEXT ( ( #10877, #77231, #28719 ) ) REPRESENTATION_CONTEXT ( 'NONE', 'WORKASPACE' ) );
#22842 = DIRECTION ( 'NONE',  ( 0.000000000000000000, -1.000000000000000000, 0.000000000000000000 ) ) ;
#22843 = CARTESIAN_POINT ( 'NONE',  ( 9.500000025475724641, -4.999999999999998224, -69.85526497429231085 ) ) ;
#22844 = ORIENTED_EDGE ( 'NONE', *, *, #78575, .T. ) ;
#22845 = CARTESIAN_POINT ( 'NONE',  ( -88.76425966579064664, -30.00000000000024514, -15.41591536337368140 ) ) ;
#22846 = ORIENTED_EDGE ( 'NONE', *, *, #90793, .F. ) ;
#22847 = CARTESIAN_POINT ( 'NONE',  ( -3.454253436624922458, -49.15858197120396511, 103.7259032015043090 ) ) ;
#22848 = CARTESIAN_POINT ( 'NONE',  ( 8.986743721356470260, 15.43298062744866961, 4.999999999999999112 ) ) ;
#22849 = CARTESIAN_POINT ( 'NONE',  ( 32.16538097803554308, 380.2609445124364811, 24.62016063048157832 ) ) ;
#22850 = STYLED_ITEM ( 'NONE', ( #61826 ), #20499 ) ;
#22851 = CARTESIAN_POINT ( 'NONE',  ( -7.188101187500002709, -26.18750000204838813, 2.977408999572648707 ) ) ;
#22852 = DIRECTION ( 'NONE',  ( -1.000000000000000000, -0.000000000000000000, -0.000000000000000000 ) ) ;
#22853 = FILL_AREA_STYLE ('',( #97229 ) ) ;
#22854 = CARTESIAN_POINT ( 'NONE',  ( 7.439123282901347167, 41.00341550150766068, -68.91429205944716330 ) ) ;
#22855 = ORIENTED_EDGE ( 'NONE', *, *, #35936, .F. ) ;
#22857 = ORIENTED_EDGE ( 'NONE', *, *, #33609, .T. ) ;
#22856 = CARTESIAN_POINT ( 'NONE',  ( -7.195947757872210637, 41.08281073708428721, -58.60024740043413516 ) ) ;
#22858 = CARTESIAN_POINT ( 'NONE',  ( 81.17915358008252724, -39.49775230550695682, 153.9097520608757463 ) ) ;
#22859 = CARTESIAN_POINT ( 'NONE',  ( 37.33349330513379982, 4.000000000000003553, 0.000000000000000000 ) ) ;
#22860 = EDGE_LOOP ( 'NONE', ( #17628, #91222, #18350, #62927, #26244 ) ) ;
#22861 = CARTESIAN_POINT ( 'NONE',  ( -12.50000000000000355, 27.15417587463127091, -44.69229109533035427 ) ) ;
#22862 = CARTESIAN_POINT ( 'NONE',  ( -0.7799315185232612579, 13.54185226379499696, -51.48129177036200588 ) ) ;
#22863 = CARTESIAN_POINT ( 'NONE',  ( -7.188101187500000044, -15.40625000204838635, -8.802885111219163269E-16 ) ) ;
#22864 = CARTESIAN_POINT ( 'NONE',  ( 43.00000000000000000, 487.9285348210859752, 8.903916466042430145 ) ) ;
#22865 = CARTESIAN_POINT ( 'NONE',  ( 11.51386276761315308, 45.40501555918417864, 14.44555604779037061 ) ) ;
#22866 = CARTESIAN_POINT ( 'NONE',  ( 19.15449903924667652, 294.6774112952710993, 1.900463839854222847 ) ) ;
#22867 = ADVANCED_FACE ( 'NONE', ( #70825 ), #33661, .T. ) ;
#22868 = ORIENTED_EDGE ( 'NONE', *, *, #64773, .F. ) ;
#22869 = SURFACE_STYLE_USAGE ( .BOTH. , #97250 ) ;
#22870 = SURFACE_SIDE_STYLE ('',( #81060 ) ) ;
#22871 = STYLED_ITEM ( 'NONE', ( #70977 ), #94497 ) ;
#22872 = CARTESIAN_POINT ( 'NONE',  ( 1.128238012697730275, 300.0000000000000000, 9.936150108905557943 ) ) ;
#22873 = EDGE_CURVE ( 'NONE', #30622, #3257, #14685, .T. ) ;
#22874 = CARTESIAN_POINT ( 'NONE',  ( 14.62309622339465243, 18.64284798592481351, -35.53993507406291030 ) ) ;
#22875 = CYLINDRICAL_SURFACE ( 'NONE', #87812, 1.250000000000001110 ) ;
#22876 = VERTEX_POINT ( 'NONE', #36899 ) ;
#22877 = CARTESIAN_POINT ( 'NONE',  ( -8.000000000000000000, -12.03125000409677270, -3.313708498984762496 ) ) ;
#22878 = CARTESIAN_POINT ( 'NONE',  ( -5.863289337118752442, -12.99053128498974630, 32.07553765330735018 ) ) ;
#22879 = CARTESIAN_POINT ( 'NONE',  ( 31.08349330513380693, -3.851859888774471706E-31, 4.000000000000001776 ) ) ;
#22880 = CARTESIAN_POINT ( 'NONE',  ( -1.000000000000000000, -40.48763664056765776, -0.7135409870776373564 ) ) ;
#22881 = SURFACE_SIDE_STYLE ('',( #96749 ) ) ;
#22882 = SHAPE_DEFINITION_REPRESENTATION ( #4568, #70207 ) ;
#22883 = CARTESIAN_POINT ( 'NONE',  ( -9.999945253488242258, 33.99986313370533253, -0.2662901834230996800 ) ) ;
#22884 = ORIENTED_EDGE ( 'NONE', *, *, #32925, .F. ) ;
#22885 = CARTESIAN_POINT ( 'NONE',  ( -4.738695502753807354, -47.42796447909066160, 42.87913045825063563 ) ) ;
#22886 = CARTESIAN_POINT ( 'NONE',  ( -4.165977904505307805, 16.00000000000000000, 9.090909090909091717 ) ) ;
#22887 = CARTESIAN_POINT ( 'NONE',  ( -39.21279148650070567, 436.8435004666161490, 5.150741822288940952 ) ) ;
#22888 = CARTESIAN_POINT ( 'NONE',  ( -24.72970151039347186, -27.61749151431341431, -38.39745497380010164 ) ) ;
#22889 = DIRECTION ( 'NONE',  ( -1.000000000000000000, -0.000000000000000000, -0.000000000000000000 ) ) ;
#22890 = CARTESIAN_POINT ( 'NONE',  ( 5.500000000000006217, 42.00000000000000000, -58.09827136975972905 ) ) ;
#22891 = EDGE_CURVE ( 'NONE', #51522, #33537, #881, .T. ) ;
#22892 = ORIENTED_EDGE ( 'NONE', *, *, #80971, .T. ) ;
#22893 = CARTESIAN_POINT ( 'NONE',  ( 0.01678220608715901702, 0.7854258608507265205, -8.000000000000001776 ) ) ;
#22894 = CARTESIAN_POINT ( 'NONE',  ( 101.7050805557714739, -57.63128474202212459, 203.3834090003539643 ) ) ;
#22895 = CARTESIAN_POINT ( 'NONE',  ( 86.17777777777776294, 1.023464760207051730E-14, 0.000000000000000000 ) ) ;
#22896 = CARTESIAN_POINT ( 'NONE',  ( 27.59999999999999787, 4.172000000000003261, 0.000000000000000000 ) ) ;
#22897 = DIRECTION ( 'NONE',  ( 0.000000000000000000, 0.000000000000000000, -1.000000000000000000 ) ) ;
#22898 = CARTESIAN_POINT ( 'NONE',  ( 0.7145311798163198613, -4.618802153516998743, 7.999999999999998224 ) ) ;
#22899 = CARTESIAN_POINT ( 'NONE',  ( -73.77751223451437568, -59.99999999999999289, 169.9644275812541991 ) ) ;
#22900 = CONICAL_SURFACE ( 'NONE', #7379, 5.000000000000010658, 0.9599310885968697082 ) ;
#22901 = CARTESIAN_POINT ( 'NONE',  ( -39.24156521425334176, 307.7088117867400001, -7.003459073692002157 ) ) ;
#22902 = CARTESIAN_POINT ( 'NONE',  ( 46.00000000000000000, 461.9428920847514632, 12.03309428281642823 ) ) ;
#22903 = CARTESIAN_POINT ( 'NONE',  ( -64.91565662648044110, 48.00000000000000000, 6.815324757466639127 ) ) ;
#22904 = CARTESIAN_POINT ( 'NONE',  ( -86.39553218061814732, -17.42288545000702982, 179.1655162981548699 ) ) ;
#22905 =( GEOMETRIC_REPRESENTATION_CONTEXT ( 3 ) GLOBAL_UNCERTAINTY_ASSIGNED_CONTEXT ( ( #83400 ) ) GLOBAL_UNIT_ASSIGNED_CONTEXT ( ( #48821, #34290, #15946 ) ) REPRESENTATION_CONTEXT ( 'NONE', 'WORKASPACE' ) );
#22906 = VERTEX_POINT ( 'NONE', #68718 ) ;
#22907 = CARTESIAN_POINT ( 'NONE',  ( 35.73673605237448214, 338.3594419497471790, -1.628405847195040668 ) ) ;
#22908 = ORIENTED_EDGE ( 'NONE', *, *, #43207, .T. ) ;
#22909 = CARTESIAN_POINT ( 'NONE',  ( 12.36633005457780854, -4.301166014003213078, -76.75180828602340455 ) ) ;
#22910 = EDGE_CURVE ( 'NONE', #84646, #33315, #44056, .T. ) ;
#22911 = CARTESIAN_POINT ( 'NONE',  ( -21.88406739194823913, 304.0791269202651392, -9.951548237181681245 ) ) ;
#22912 = DIRECTION ( 'NONE',  ( -1.000000000000000000, 0.000000000000000000, 0.000000000000000000 ) ) ;
#22913 = CARTESIAN_POINT ( 'NONE',  ( -42.31186848673717549, 465.8659795009672280, 14.28293630011528137 ) ) ;
#22914 = CARTESIAN_POINT ( 'NONE',  ( 4.592425496802573972E-16, 4.000000000000000000, -3.500000000000000000 ) ) ;
#22915 = ORIENTED_EDGE ( 'NONE', *, *, #21101, .T. ) ;
#22916 = CIRCLE ( 'NONE', #64250, 4.000000000000001776 ) ;
#22917 = CARTESIAN_POINT ( 'NONE',  ( 17.95740001248639928, 50.00000000000000711, 61.94476881109564914 ) ) ;
#22918 = CARTESIAN_POINT ( 'NONE',  ( 13.01482060791784967, 23.72313099889873556, 4.353235333136677987 ) ) ;
#22919 = CARTESIAN_POINT ( 'NONE',  ( 5.820808985963070725, 3.863013742957921305E-12, 21.65942590380143074 ) ) ;
#22920 = CARTESIAN_POINT ( 'NONE',  ( -36.55165400673971732, 463.9825939691005487, 19.61553332823773133 ) ) ;
#22921 = CARTESIAN_POINT ( 'NONE',  ( 64.66821620130598092, -14.21045842199433373, -28.81313120037184916 ) ) ;
#22922 = B_SPLINE_CURVE_WITH_KNOTS ( 'NONE', 3,
 ( #74945, #48550, #72823, #48014, #80924, #32940, #99768, #56642, #99221, #81439, #16189, #57694, #90085, #33463 ),
 .UNSPECIFIED., .F., .F.,
 ( 4, 2, 2, 2, 2, 2, 4 ),
 ( -2.637499479246189856E-05, 0.003621852776081119999, 0.007270080546954701961, 0.009094194432391494026, 0.01091830831782828436, 0.01274242220326507642, 0.01456653608870186675 ),
 .UNSPECIFIED. ) ;
#22923 = CARTESIAN_POINT ( 'NONE',  ( -79.28526668511025832, -36.02933522492092777, 138.0984090641172770 ) ) ;
#22924 = ORIENTED_EDGE ( 'NONE', *, *, #87040, .F. ) ;
#22925 = CARTESIAN_POINT ( 'NONE',  ( 1.425929562426998531, -60.00000000000000000, 41.99999999999999289 ) ) ;
#22926 = DIRECTION ( 'NONE',  ( 0.000000000000000000, 1.000000000000000000, 0.000000000000000000 ) ) ;
#22927 = CARTESIAN_POINT ( 'NONE',  ( 91.32027366411901426, -57.61411389006468653, 204.2399109338346932 ) ) ;
#22928 = CARTESIAN_POINT ( 'NONE',  ( 5.523799489093671039E-15, 23.58303312036771615, 45.10524579772351217 ) ) ;
#22929 = CARTESIAN_POINT ( 'NONE',  ( 36.03799849557760382, 304.0525444531467087, 0.1188115607976301946 ) ) ;
#22930 = CARTESIAN_POINT ( 'NONE',  ( -12.28357616224760918, 9.933929378342256200, 9.536270961999530726 ) ) ;
#22931 = VERTEX_POINT ( 'NONE', #69245 ) ;
#22932 = CARTESIAN_POINT ( 'NONE',  ( 7.500000000000000888, 0.7513028741560163759, -0.02472015219302733588 ) ) ;
#22933 = DIRECTION ( 'NONE',  ( 0.000000000000000000, 0.000000000000000000, -1.000000000000000000 ) ) ;
#22935 = CARTESIAN_POINT ( 'NONE',  ( -104.3522526634287857, -60.15517057847299043, 144.3591752484916242 ) ) ;
#22934 = DIRECTION ( 'NONE',  ( 0.000000000000000000, 1.000000000000000000, 0.000000000000000000 ) ) ;
#22936 = CARTESIAN_POINT ( 'NONE',  ( -2.977408999572654480, -18.12500000204838457, 7.188101187499999156 ) ) ;
#22937 = CARTESIAN_POINT ( 'NONE',  ( 43.98494780483915889, 485.1299400071267769, -0.2561545284547621093 ) ) ;
#22938 = AXIS2_PLACEMENT_3D ( 'NONE', #42078, #39585, #23405 ) ;
#22939 = CARTESIAN_POINT ( 'NONE',  ( 6.562874270078298267, -3.301808241302750080, -6.845811579416824166 ) ) ;
#22940 = CARTESIAN_POINT ( 'NONE',  ( 3.643324519380566085E-15, 34.17188553058033307, 29.75000000000000355 ) ) ;
#22941 = ADVANCED_FACE ( 'NONE', ( #101601 ), #87023, .F. ) ;
#22942 = DIRECTION ( 'NONE',  ( 0.5735764363510462704, 0.8191520442889915765, 0.000000000000000000 ) ) ;
#22943 = STYLED_ITEM ( 'NONE', ( #1311 ), #39669 ) ;
#22944 = ORIENTED_EDGE ( 'NONE', *, *, #78118, .F. ) ;
#22945 = CARTESIAN_POINT ( 'NONE',  ( 43.03185303983483578, 485.3613526602389356, 6.073233449168498055 ) ) ;
#22946 = VECTOR ( 'NONE', #12454, 1000.000000000000000 ) ;
#22948 = CARTESIAN_POINT ( 'NONE',  ( 26.15828352856528127, -25.56935877229565790, 29.61310315546906224 ) ) ;
#22947 = CARTESIAN_POINT ( 'NONE',  ( -24.48725402052853184, -14.21045842199434084, 35.52122251240935924 ) ) ;
#22949 = CARTESIAN_POINT ( 'NONE',  ( -5.126331210562743657, 52.11692832490694371, -6.039129629323012338 ) ) ;
#22950 = VERTEX_POINT ( 'NONE', #84882 ) ;
#22951 = ADVANCED_FACE ( 'NONE', ( #27756 ), #40639, .T. ) ;
#22952 = ORIENTED_EDGE ( 'NONE', *, *, #7530, .F. ) ;
#22953 = CARTESIAN_POINT ( 'NONE',  ( -1.250638237768894268, 43.55834836214284422, -17.65405259223556556 ) ) ;
#22954 = PRESENTATION_STYLE_ASSIGNMENT (( #96825 ) ) ;
#22955 = EDGE_CURVE ( 'NONE', #31665, #44273, #6222, .T. ) ;
#22956 = DIRECTION ( 'NONE',  ( -1.000000000000000000, -1.224606353822377258E-16, -0.000000000000000000 ) ) ;
#22957 = CARTESIAN_POINT ( 'NONE',  ( 10.92337230437442841, 2.452739325026194628, 14.79856046833763727 ) ) ;
#22958 = CARTESIAN_POINT ( 'NONE',  ( 56.48317336153285595, 4.898587196589294500E-16, -4.000000000000007105 ) ) ;
#22959 = VERTEX_POINT ( 'NONE', #15231 ) ;
#22960 = CARTESIAN_POINT ( 'NONE',  ( 49.60909704566071099, -60.00000000000000711, -37.98112837208373094 ) ) ;
#22961 = CARTESIAN_POINT ( 'NONE',  ( 83.13875906005428362, -29.99999999999996447, 153.7901336831974390 ) ) ;
#22963 = EDGE_CURVE ( 'NONE', #2886, #34061, #102627, .T. ) ;
#22962 = CARTESIAN_POINT ( 'NONE',  ( 7.500000000000000888, 9.184850993605149917E-16, 0.000000000000000000 ) ) ;
#22964 = CARTESIAN_POINT ( 'NONE',  ( 6.289692432696780244, -0.6618655008720331079, 6.828989928337167115 ) ) ;
#22965 = CARTESIAN_POINT ( 'NONE',  ( -47.90443661882622450, 17.06459462766618529, -14.35535821593460248 ) ) ;
#22966 = ORIENTED_EDGE ( 'NONE', *, *, #71081, .F. ) ;
#22967 = ORIENTED_EDGE ( 'NONE', *, *, #2710, .T. ) ;
#22968 = ORIENTED_EDGE ( 'NONE', *, *, #74725, .T. ) ;
#22969 = FILL_AREA_STYLE_COLOUR ( '', #12448 ) ;
#22970 = CARTESIAN_POINT ( 'NONE',  ( 27.00466673664397632, 41.40534887492042060, -70.25901564828242840 ) ) ;
#22971 = CARTESIAN_POINT ( 'NONE',  ( -41.68589585752227578, 436.0808743425936882, 20.68176223068306285 ) ) ;
#22972 = CARTESIAN_POINT ( 'NONE',  ( 33.13272883738260788, 379.7391572186269855, 24.76066166452115169 ) ) ;
#22973 = CARTESIAN_POINT ( 'NONE',  ( -41.66500103013587619, 324.8107132651804818, 5.306019078252184329 ) ) ;
#22974 = CARTESIAN_POINT ( 'NONE',  ( -3.932591042162086215, -69.40053737951669177, 13.56259061519041964 ) ) ;
#22975 = CARTESIAN_POINT ( 'NONE',  ( -46.00000000000000000, 488.3725375423296668, 3.127739281037493768 ) ) ;
#22976 = CARTESIAN_POINT ( 'NONE',  ( 6.289812543865804351, -5.581224740283312613, 3.991031161979334385 ) ) ;
#22977 = VERTEX_POINT ( 'NONE', #105312 ) ;
#22978 = CARTESIAN_POINT ( 'NONE',  ( 1.224646799147352665E-15, 48.00000000000000000, -75.00000000000001421 ) ) ;
#22979 = ORIENTED_EDGE ( 'NONE', *, *, #1883, .F. ) ;
#22980 = CARTESIAN_POINT ( 'NONE',  ( 20.19615384615384457, 1.411358822780289120E-15, 0.000000000000000000 ) ) ;
#22981 = CARTESIAN_POINT ( 'NONE',  ( -25.60851123679742258, 50.00000000031798919, -75.29411764726208389 ) ) ;
#22982 = DIRECTION ( 'NONE',  ( -1.000000000000000000, -0.000000000000000000, -0.000000000000000000 ) ) ;
#22983 = VECTOR ( 'NONE', #95104, 1000.000000000000000 ) ;
#22984 = LINE ( 'NONE', #97361, #80406 ) ;
#22985 = CARTESIAN_POINT ( 'NONE',  ( 64.70032873768002446, -39.48212153678270653, 85.31995070285097427 ) ) ;
#22986 = VECTOR ( 'NONE', #97671, 1000.000000000000114 ) ;
#22987 = ORIENTED_EDGE ( 'NONE', *, *, #47816, .F. ) ;
#22988 = CARTESIAN_POINT ( 'NONE',  ( -7.320748600891240798, 41.41789230214724427, -68.91429205797308555 ) ) ;
#22989 = STYLED_ITEM ( 'NONE', ( #1763 ), #52434 ) ;
#22990 = CARTESIAN_POINT ( 'NONE',  ( 7.188101187500000933, -28.06250000204838813, -2.977408999572650483 ) ) ;
#22991 = DIRECTION ( 'NONE',  ( 0.000000000000000000, 1.000000000000000000, 0.000000000000000000 ) ) ;
#22992 = ADVANCED_FACE ( 'NONE', ( #87547 ), #16546, .T. ) ;
#22993 = ORIENTED_EDGE ( 'NONE', *, *, #75508, .F. ) ;
#22994 =( LENGTH_UNIT ( ) NAMED_UNIT ( * ) SI_UNIT ( .MILLI., .METRE. ) );
#22995 = CARTESIAN_POINT ( 'NONE',  ( 47.44667293595422564, 16.35698112199397158, 16.71846647949837461 ) ) ;
#22996 = CONICAL_SURFACE ( 'NONE', #36794, 3.309500000000007880, 0.9599310885968770357 ) ;
#22997 = EDGE_CURVE ( 'NONE', #76274, #97524, #37216, .T. ) ;
#22998 = EDGE_CURVE ( 'NONE', #29831, #86195, #100931, .T. ) ;
#22999 = DIRECTION ( 'NONE',  ( -0.000000000000000000, -1.000000000000000000, -0.000000000000000000 ) ) ;
#23000 = CARTESIAN_POINT ( 'NONE',  ( 5.656854249492380582, -32.00000000409676915, -5.656854249492379694 ) ) ;
#23001 = CARTESIAN_POINT ( 'NONE',  ( -5.219866590715411370, -5.000000000000000000, -8.922269033013266792 ) ) ;
#23002 = CARTESIAN_POINT ( 'NONE',  ( 87.02191047559196591, -31.70738880027288431, 187.4629506568093689 ) ) ;
#23003 = UNCERTAINTY_MEASURE_WITH_UNIT (LENGTH_MEASURE( 1.000000000000000082E-05 ), #7295, 'distance_accuracy_value', 'NONE');
#23004 = CARTESIAN_POINT ( 'NONE',  ( -9.596328385228648727, 8.973060046565024095, 0.000000000000000000 ) ) ;
#23005 = CARTESIAN_POINT ( 'NONE',  ( -2.263183130831067924, 6.566419505188279437, -6.208110906918260952 ) ) ;
#23006 =( NAMED_UNIT ( * ) PLANE_ANGLE_UNIT ( ) SI_UNIT ( $, .RADIAN. ) );
#23007 = CARTESIAN_POINT ( 'NONE',  ( 11.62660349859606868, 304.6006130031697126, 9.883607381091580990 ) ) ;
#23008 = VERTEX_POINT ( 'NONE', #6602 ) ;
#23009 = CARTESIAN_POINT ( 'NONE',  ( 7.000000000000000000, 0.000000000000000000, -4.425378966781146950 ) ) ;
#23010 = CARTESIAN_POINT ( 'NONE',  ( 36.54387785002509759, -60.00000000000001421, 47.89680925484002216 ) ) ;
#23011 = CIRCLE ( 'NONE', #93592, 4.000000000000007105 ) ;
#23012 = CARTESIAN_POINT ( 'NONE',  ( -99.80602541531122540, -30.00000000000000355, 186.3886247876614846 ) ) ;
#23013 = EDGE_CURVE ( 'NONE', #67117, #21469, #102491, .T. ) ;
#23014 =( GEOMETRIC_REPRESENTATION_CONTEXT ( 3 ) GLOBAL_UNCERTAINTY_ASSIGNED_CONTEXT ( ( #47826 ) ) GLOBAL_UNIT_ASSIGNED_CONTEXT ( ( #26078, #59474, #10881 ) ) REPRESENTATION_CONTEXT ( 'NONE', 'WORKASPACE' ) );
#23015 = MECHANICAL_DESIGN_GEOMETRIC_PRESENTATION_REPRESENTATION (  '', ( #66232 ), #7482 ) ;
#23016 = MECHANICAL_DESIGN_GEOMETRIC_PRESENTATION_REPRESENTATION (  '', ( #64270 ), #40156 ) ;
#23017 = CARTESIAN_POINT ( 'NONE',  ( -40.05511244076242150, 485.1954865622287230, -4.343528235245400992 ) ) ;
#23018 = CARTESIAN_POINT ( 'NONE',  ( 35.30542147758094274, -57.69548023038977647, 49.46059037094081390 ) ) ;
#23019 = CARTESIAN_POINT ( 'NONE',  ( 6.738100180926640093, 41.71798714554645215, -59.05424661244425266 ) ) ;
#23020 = ADVANCED_FACE ( 'NONE', ( #15763, #23353, #38995, #106351, #40045 ), #64750, .F. ) ;
#23021 = SURFACE_STYLE_USAGE ( .BOTH. , #13289 ) ;
#23022 = CARTESIAN_POINT ( 'NONE',  ( -30.00000000000000355, 461.9590195980672434, 14.34002891082236708 ) ) ;
#23023 = CARTESIAN_POINT ( 'NONE',  ( -9.571198553003730680, 15.30040232763764330, 2.918503601031092742 ) ) ;
#23024 = FACE_OUTER_BOUND ( 'NONE', #25753, .T. ) ;
#23025 = CARTESIAN_POINT ( 'NONE',  ( -8.434902168003450385, -60.00000000000000711, 39.63584717613949948 ) ) ;
#23026 = CARTESIAN_POINT ( 'NONE',  ( 0.3074911254280547346, -69.98475940929637318, 12.98938480846820909 ) ) ;
#23027 = CARTESIAN_POINT ( 'NONE',  ( -86.53663329270624160, -57.41224747399611772, 193.5711379720445109 ) ) ;
#23028 = ORIENTED_EDGE ( 'NONE', *, *, #49698, .T. ) ;
#23029 = CARTESIAN_POINT ( 'NONE',  ( 17.50000000000004619, 51.99872764530864799, 60.15967750825412708 ) ) ;
#23030 = DIRECTION ( 'NONE',  ( -1.000000000000000000, -1.224606353822377258E-16, -0.000000000000000000 ) ) ;
#23031 = CARTESIAN_POINT ( 'NONE',  ( -11.20631249100435589, -29.03129763674975905, 28.75315964071688413 ) ) ;
#23033 = CARTESIAN_POINT ( 'NONE',  ( -36.54024843362181940, 439.8191410655647360, 24.21861018269294163 ) ) ;
#23032 = CARTESIAN_POINT ( 'NONE',  ( -106.4735328932949869, -59.99999999999999289, 175.0934596608935863 ) ) ;
#23034 = ORIENTED_EDGE ( 'NONE', *, *, #40940, .F. ) ;
#23035 = CARTESIAN_POINT ( 'NONE',  ( -43.03357534758885095, 463.2291678140052227, 4.675918524150252331 ) ) ;
#23036 = B_SPLINE_CURVE_WITH_KNOTS ( 'NONE', 3,
 ( #48080, #80982, #7098, #24394, #23860, #90151 ),
 .UNSPECIFIED., .F., .F.,
 ( 4, 2, 4 ),
 ( 2.380731629569274211E-07, 0.002336973833157562908, 0.004673709593152167857 ),
 .UNSPECIFIED. ) ;
#23037 = CARTESIAN_POINT ( 'NONE',  ( -9.536280427380496860, -4.999999999999837463, -20.18661038764972560 ) ) ;
#23038 = DIRECTION ( 'NONE',  ( 0.000000000000000000, -0.9371777605526921961, -0.3488521823429527879 ) ) ;
#23039 = FACE_OUTER_BOUND ( 'NONE', #45294, .T. ) ;
#23040 = CARTESIAN_POINT ( 'NONE',  ( 65.16906654191903669, -60.00000000000000000, 118.9734969953735515 ) ) ;
#23041 = CARTESIAN_POINT ( 'NONE',  ( 1.836601268058450879E-15, 1.005902684993156715, 14.99698745252234566 ) ) ;
#23042 = VERTEX_POINT ( 'NONE', #31971 ) ;
#23043 = CARTESIAN_POINT ( 'NONE',  ( -10.28624191511820207, 43.99263840937192782, 12.90779740156163768 ) ) ;
#23044 = DIRECTION ( 'NONE',  ( 0.000000000000000000, 0.000000000000000000, -1.000000000000000000 ) ) ;
#23045 = AXIS2_PLACEMENT_3D ( 'NONE', #71279, #6006, #38930 ) ;
#23047 = CARTESIAN_POINT ( 'NONE',  ( -7.468836275494362020, -3.123212597911423138, -19.53079664951584959 ) ) ;
#23046 = CARTESIAN_POINT ( 'NONE',  ( 24.85181238201470322, -30.00000000000000000, 38.32581332381749206 ) ) ;
#23048 = DIRECTION ( 'NONE',  ( 0.000000000000000000, 0.000000000000000000, 1.000000000000000000 ) ) ;
#23049 = EDGE_LOOP ( 'NONE', ( #61482, #90044, #42812, #78514, #91405, #55694 ) ) ;
#23050 = CARTESIAN_POINT ( 'NONE',  ( -26.97187310779845504, 311.5034665361333168, 10.53023658691173026 ) ) ;
#23051 = AXIS2_PLACEMENT_3D ( 'NONE', #33256, #66667, #66129 ) ;
#23052 = VERTEX_POINT ( 'NONE', #46544 ) ;
#23053 = DIRECTION ( 'NONE',  ( 0.000000000000000000, 0.000000000000000000, 1.000000000000000000 ) ) ;
#23054 = DIRECTION ( 'NONE',  ( 0.6181567188929438794, 0.3028222199723830110, -0.7253833289913049764 ) ) ;
#23055 = DIRECTION ( 'NONE',  ( -1.000000000000000000, -1.224606353822377258E-16, -0.000000000000000000 ) ) ;
#23056 = ORIENTED_EDGE ( 'NONE', *, *, #97786, .T. ) ;
#23057 = ADVANCED_FACE ( 'NONE', ( #48117 ), #10792, .F. ) ;
#23058 = CARTESIAN_POINT ( 'NONE',  ( 31.08349330513380337, 1.593028355512270567E-15, 0.000000000000000000 ) ) ;
#23059 = CARTESIAN_POINT ( 'NONE',  ( -88.50868962893154901, -59.99999999999261036, 204.1120144510070702 ) ) ;
#23060 = CARTESIAN_POINT ( 'NONE',  ( 45.99999999999428013, 486.2727346241949249, 2.946729464013586597 ) ) ;
#23061 = CARTESIAN_POINT ( 'NONE',  ( 83.70906304977542334, -60.00000000000002132, 199.3180261249159742 ) ) ;
#23062 = CARTESIAN_POINT ( 'NONE',  ( 0.6442865410403176840, 25.22687333464023141, -40.58400936760502731 ) ) ;
#23064 = CARTESIAN_POINT ( 'NONE',  ( 9.379153979492304671, -56.87790722318686676, 33.37334884318637762 ) ) ;
#23063 = CARTESIAN_POINT ( 'NONE',  ( -109.0466421874928074, -29.99999999999997513, 159.8085545269249224 ) ) ;
#23065 = EDGE_CURVE ( 'NONE', #81556, #22579, #66442, .T. ) ;
#23066 = CARTESIAN_POINT ( 'NONE',  ( 97.17332080658498228, -38.00000000000000711, 120.7792972779389373 ) ) ;
#23067 = DIRECTION ( 'NONE',  ( 1.000000000000000000, 0.000000000000000000, 0.000000000000000000 ) ) ;
#23068 = CARTESIAN_POINT ( 'NONE',  ( -46.34968830293420439, -53.35688838113154731, 49.29538158241714996 ) ) ;
#23069 = CARTESIAN_POINT ( 'NONE',  ( -1.220536332002533753, 34.50324530966049963, -28.81383133510943040 ) ) ;
#23070 = EDGE_LOOP ( 'NONE', ( #69990, #47125, #81763, #100163, #24493 ) ) ;
#23071 = CARTESIAN_POINT ( 'NONE',  ( 0.000000000000000000, 0.000000000000000000, -9.078441367943003826 ) ) ;
#23072 = CARTESIAN_POINT ( 'NONE',  ( 33.95156263172584943, 464.5083255208626838, 6.608064661821377861 ) ) ;
#23073 =( LENGTH_UNIT ( ) NAMED_UNIT ( * ) SI_UNIT ( .MILLI., .METRE. ) );
#23074 = CARTESIAN_POINT ( 'NONE',  ( 6.779931853646243844, 303.7378069780689884, -10.02423311839737607 ) ) ;
#23075 = CARTESIAN_POINT ( 'NONE',  ( 0.000000000000000000, -99.99999999999997158, 0.000000000000000000 ) ) ;
#23076 = EDGE_LOOP ( 'NONE', ( #27578, #27723, #22968, #87690 ) ) ;
#23077 = FACE_OUTER_BOUND ( 'NONE', #80910, .T. ) ;
#23078 = VERTEX_POINT ( 'NONE', #38475 ) ;
#23079 = CARTESIAN_POINT ( 'NONE',  ( 86.99672156470798257, -29.99999999998241051, 198.2267927734325497 ) ) ;
#23080 = FACE_OUTER_BOUND ( 'NONE', #96076, .T. ) ;
#23081 = AXIS2_PLACEMENT_3D ( 'NONE', #44470, #63718, #69290 ) ;
#23083 = EDGE_CURVE ( 'NONE', #4914, #74421, #15770, .T. ) ;
#23082 = CARTESIAN_POINT ( 'NONE',  ( 5.430163322397451253, 41.93410894844108583, -59.17461580565397128 ) ) ;
#23084 = CARTESIAN_POINT ( 'NONE',  ( -1.233923992984923027E-14, 18.64316884711714195, -38.36535705883633085 ) ) ;
#23085 = CARTESIAN_POINT ( 'NONE',  ( 98.90563218758491359, -30.00000000000000000, 144.2321003841678646 ) ) ;
#23086 = AXIS2_PLACEMENT_3D ( 'NONE', #68339, #75341, #83440 ) ;
#23087 = CARTESIAN_POINT ( 'NONE',  ( 6.928203230275509661, 104.7347384306741276, 4.000000000000001776 ) ) ;
#23088 = ORIENTED_EDGE ( 'NONE', *, *, #47504, .F. ) ;
#23089 = STYLED_ITEM ( 'NONE', ( #83582 ), #4890 ) ;
#23090 = CIRCLE ( 'NONE', #17989, 4.000000000000002665 ) ;
#23091 = ORIENTED_EDGE ( 'NONE', *, *, #16379, .T. ) ;
#23092 = ORIENTED_EDGE ( 'NONE', *, *, #71051, .F. ) ;
#23094 = DIRECTION ( 'NONE',  ( -1.000000000000000000, -1.224606353822377258E-16, -0.000000000000000000 ) ) ;
#23093 = VECTOR ( 'NONE', #40073, 1000.000000000000000 ) ;
#23095 = CARTESIAN_POINT ( 'NONE',  ( 22.11640175898061855, 26.03333166199414350, 31.35866682975836639 ) ) ;
#23096 = CARTESIAN_POINT ( 'NONE',  ( -46.00000000000000000, 461.5923542530184704, 9.841579728281992345 ) ) ;
#23097 = ORIENTED_EDGE ( 'NONE', *, *, #87507, .T. ) ;
#23098 = DIRECTION ( 'NONE',  ( 0.000000000000000000, 0.000000000000000000, -1.000000000000000000 ) ) ;
#23099 = ORIENTED_EDGE ( 'NONE', *, *, #90307, .F. ) ;
#23100 = FACE_OUTER_BOUND ( 'NONE', #3113, .T. ) ;
#23101 = CARTESIAN_POINT ( 'NONE',  ( 77.91253027013023313, -38.56360447836954108, 187.9343819089818339 ) ) ;
#23102 = CARTESIAN_POINT ( 'NONE',  ( 13.27968648137678542, 3.841854981409799752, 6.905317930445485253 ) ) ;
#23103 = CARTESIAN_POINT ( 'NONE',  ( 84.43118809173812167, -45.28802927494923125, -4.046620873543590235 ) ) ;
#23104 = DIRECTION ( 'NONE',  ( -1.000000000000000000, -1.224606353822377258E-16, -0.000000000000000000 ) ) ;
#23105 = CARTESIAN_POINT ( 'NONE',  ( 27.64945316933048147, 308.2090964242639757, 11.19157541975697967 ) ) ;
#23106 = CARTESIAN_POINT ( 'NONE',  ( 42.15357157744617211, 485.2432036427202320, -2.744622672851878775 ) ) ;
#23107 = DIRECTION ( 'NONE',  ( -1.000000000000000000, 0.000000000000000000, 0.000000000000000000 ) ) ;
#23108 = SURFACE_STYLE_FILL_AREA ( #30677 ) ;
#23109 = CARTESIAN_POINT ( 'NONE',  ( 42.12169488795439776, 344.1724850039262833, 13.56560836097746403 ) ) ;
#23110 = ORIENTED_EDGE ( 'NONE', *, *, #58806, .T. ) ;
#23111 = DIRECTION ( 'NONE',  ( 1.000000000000000000, 1.224606353822377258E-16, 0.000000000000000000 ) ) ;
#23113 = EDGE_CURVE ( 'NONE', #18278, #57508, #18264, .T. ) ;
#23112 = CARTESIAN_POINT ( 'NONE',  ( -38.85446894546556962, 460.8903912184119349, 2.218456751109251890 ) ) ;
#23114 = STYLED_ITEM ( 'NONE', ( #42260 ), #61288 ) ;
#23115 = DIRECTION ( 'NONE',  ( 0.9807128367232246235, 0.000000000000000000, -0.1954541682499656707 ) ) ;
#23116 = VERTEX_POINT ( 'NONE', #57801 ) ;
#23117 = CARTESIAN_POINT ( 'NONE',  ( 6.849999999999999645, 9.237604307034018802, 1.301042606982603546E-15 ) ) ;
#23119 = CARTESIAN_POINT ( 'NONE',  ( -26.95874670891568670, 306.9337786011216167, 10.87796326698635241 ) ) ;
#23118 = SURFACE_SIDE_STYLE ('',( #73214 ) ) ;
#23120 = CARTESIAN_POINT ( 'NONE',  ( -3.668358303306872958, -48.89638946469894876, 104.6014313550541175 ) ) ;
#23121 = LINE ( 'NONE', #7421, #7472 ) ;
#23122 = CARTESIAN_POINT ( 'NONE',  ( 3.313708498984762496, -17.28124999999999645, 7.999999999999998224 ) ) ;
#23123 = CARTESIAN_POINT ( 'NONE',  ( 28.88851691220557072, -31.70747628257775119, 39.94846750239052824 ) ) ;
#23124 = EDGE_CURVE ( 'NONE', #87161, #50002, #97447, .T. ) ;
#23125 = B_SPLINE_CURVE_WITH_KNOTS ( 'NONE', 3,
 ( #69827, #52564, #85489, #28888, #61759, #37498, #62285, #95176, #13160, #103778, #29919, #55215, #55731, #64399, #39064, #73516, #40109, #30450 ),
 .UNSPECIFIED., .F., .F.,
 ( 4, 2, 2, 2, 2, 2, 2, 2, 4 ),
 ( 0.003067497823037675965, 0.003572718754844164939, 0.004077939686650653914, 0.004583160618457140720, 0.004835771084360384990, 0.005088381550263627526, 0.005593602482070121271, 0.006098823413876615883, 0.007109265277489604240 ),
 .UNSPECIFIED. ) ;
#23126 = CARTESIAN_POINT ( 'NONE',  ( 1.469576158976828483E-15, 3.000000000000002665, -12.00000000000003908 ) ) ;
#23127 = VECTOR ( 'NONE', #9183, 1000.000000000000000 ) ;
#23128 = EDGE_LOOP ( 'NONE', ( #64352, #76818, #89230, #27149 ) ) ;
#23129 = CARTESIAN_POINT ( 'NONE',  ( 86.20252288539451513, -21.32135871581905917, 177.4573265017570805 ) ) ;
#23130 =( LENGTH_UNIT ( ) NAMED_UNIT ( * ) SI_UNIT ( .MILLI., .METRE. ) );
#23131 = ORIENTED_EDGE ( 'NONE', *, *, #8406, .F. ) ;
#23132 = AXIS2_PLACEMENT_3D ( 'NONE', #79555, #31047, #79030 ) ;
#23133 = CARTESIAN_POINT ( 'NONE',  ( 94.19233705074088903, -57.67257139432003044, 22.56487249148564089 ) ) ;
#23134 = CARTESIAN_POINT ( 'NONE',  ( 35.31443409317389381, 437.2805527638817011, 5.244185069633229723 ) ) ;
#23135 = DIRECTION ( 'NONE',  ( -1.000000000000000000, -1.224606353822377258E-16, -0.000000000000000000 ) ) ;
#23136 = CARTESIAN_POINT ( 'NONE',  ( 28.98512335478687163, 9.657432045445739632, 41.89946025606963076 ) ) ;
#23137 =( BOUNDED_SURFACE ( )  B_SPLINE_SURFACE ( 3, 2, ( 
 ( #90860, #56873, #32648 ),
 ( #65519, #98407, #41765 ),
 ( #16976, #74121, #99458 ),
 ( #106491, #83287, #24558 ),
 ( #82218, #50904, #735 ),
 ( #97877, #24032, #49853 ),
 ( #91914, #90320, #81671 ),
 ( #33171, #26169, #57404 ) ),
 .UNSPECIFIED., .F., .F., .F. ) 
 B_SPLINE_SURFACE_WITH_KNOTS ( ( 4, 2, 2, 4 ),
 ( 3, 3 ),
 ( 0.006715319241937533351, 0.008391857906702646086, 0.009230127239085202454, 0.01006839657146775882 ),
 ( 0.1556289876074680167, 1.000000000000000000 ),
 .UNSPECIFIED. ) 
 GEOMETRIC_REPRESENTATION_ITEM ( )  RATIONAL_B_SPLINE_SURFACE ( (
 ( 0.9230226209209920762, 0.7526894563075792188, 1.000000000000000000),
 ( 0.9285426880689180429, 0.7704241573834766932, 1.000000000000000000),
 ( 0.9321341943958372234, 0.7819628378765275389, 1.000000000000000000),
 ( 0.9333181995231564221, 0.7857667729451842664, 1.000000000000000000),
 ( 0.9330118842454382388, 0.7847826526908945333, 1.000000000000000000),
 ( 0.9309453891092112077, 0.7781434810044502992, 1.000000000000000000),
 ( 0.9291880512466714759, 0.7724975602490826709, 1.000000000000000000),
 ( 0.9267827504115082604, 0.7647698840875247761, 1.000000000000000000) ) ) 
 REPRESENTATION_ITEM ( '' )  SURFACE ( )  );
#23138 = CARTESIAN_POINT ( 'NONE',  ( 28.65204159835603548, 18.70303032895466089, 40.14586416981808270 ) ) ;
#23139 =( NAMED_UNIT ( * ) SI_UNIT ( $, .STERADIAN. ) SOLID_ANGLE_UNIT ( ) );
#23140 = LINE ( 'NONE', #63595, #22208 ) ;
#23142 = CARTESIAN_POINT ( 'NONE',  ( -14.65137838515496860, 5.949403477195277290, 7.096397616382773776 ) ) ;
#23141 = LINE ( 'NONE', #70079, #46531 ) ;
#23143 = ADVANCED_FACE ( 'NONE', ( #66440 ), #24434, .T. ) ;
#23144 = CARTESIAN_POINT ( 'NONE',  ( 9.766195837854356299, 294.6492712292731539, -2.152655282857795616 ) ) ;
#23145 = CARTESIAN_POINT ( 'NONE',  ( 24.83349330513380337, 1.593028355512270567E-15, 0.000000000000000000 ) ) ;
#23146 = CARTESIAN_POINT ( 'NONE',  ( -27.86837958467689802, 36.37503241011537369, -9.810923704312715543 ) ) ;
#23147 = CARTESIAN_POINT ( 'NONE',  ( -7.665484706731373166, -22.68362488985719239, -30.52813087708529949 ) ) ;
#23148 = DIRECTION ( 'NONE',  ( 1.000000000000000000, 1.224606353822377258E-16, 0.000000000000000000 ) ) ;
#23149 = ADVANCED_FACE ( 'NONE', ( #8731 ), #1694, .F. ) ;
#23150 = CARTESIAN_POINT ( 'NONE',  ( -19.96162532426521352, 302.8116070918646301, 9.928455558879880627 ) ) ;
#23151 = PRESENTATION_LAYER_ASSIGNMENT (  '', '', ( #672 ) ) ;
#23152 = ORIENTED_EDGE ( 'NONE', *, *, #3037, .T. ) ;
#23153 =( LENGTH_UNIT ( ) NAMED_UNIT ( * ) SI_UNIT ( .MILLI., .METRE. ) );
#23154 =( NAMED_UNIT ( * ) PLANE_ANGLE_UNIT ( ) SI_UNIT ( $, .RADIAN. ) );
#23155 = DIRECTION ( 'NONE',  ( 0.9745656835855570632, 0.000000000000000000, -0.2241020490254743425 ) ) ;
#23156 = TOROIDAL_SURFACE ( 'NONE', #35242, 8.000000000000000000, 4.000000000000000000 ) ;
#23158 = CARTESIAN_POINT ( 'NONE',  ( -37.34263480636265342, -21.77016502673909315, -27.75688875962726243 ) ) ;
#23157 = DIRECTION ( 'NONE',  ( 0.5735764363510468256, 0.8191520442889913545, 0.000000000000000000 ) ) ;
#23159 = AXIS2_PLACEMENT_3D ( 'NONE', #68223, #1869, #52025 ) ;
#23160 = EDGE_LOOP ( 'NONE', ( #48641, #93737, #30222 ) ) ;
#23161 = CONICAL_SURFACE ( 'NONE', #79946, 5.000000000000001776, 0.9599310885968803664 ) ;
#23162 = EDGE_LOOP ( 'NONE', ( #51580, #100564, #80187, #70120 ) ) ;
#23163 = CARTESIAN_POINT ( 'NONE',  ( 23.58349330513380337, -4.000000000000000888, 4.898587196589416773E-16 ) ) ;
#23164 = CARTESIAN_POINT ( 'NONE',  ( -90.87915574240211924, -60.00000000000000711, -17.17345031315606718 ) ) ;
#23165 = EDGE_LOOP ( 'NONE', ( #12927, #94759, #77427, #3584, #77461 ) ) ;
#23166 = DIRECTION ( 'NONE',  ( 0.000000000000000000, 1.000000000000000000, 0.000000000000000000 ) ) ;
#23167 = CARTESIAN_POINT ( 'NONE',  ( 97.79202014402906684, -52.81045661888177278, 195.1525401136383380 ) ) ;
#23169 = CARTESIAN_POINT ( 'NONE',  ( 18.58349330513380693, 4.000000000000002665, 0.000000000000000000 ) ) ;
#23168 =( NAMED_UNIT ( * ) PLANE_ANGLE_UNIT ( ) SI_UNIT ( $, .RADIAN. ) );
#23170 = CARTESIAN_POINT ( 'NONE',  ( -80.23351082821501734, -56.88084892736377896, 171.5714587829481275 ) ) ;
#23171 = ORIENTED_EDGE ( 'NONE', *, *, #71011, .F. ) ;
#23172 = ORIENTED_EDGE ( 'NONE', *, *, #7199, .T. ) ;
#23173 = ORIENTED_EDGE ( 'NONE', *, *, #44167, .T. ) ;
#23174 = DIRECTION ( 'NONE',  ( -1.000000000000000000, -1.224606353822377258E-16, -0.000000000000000000 ) ) ;
#23175 = CARTESIAN_POINT ( 'NONE',  ( -5.990115786909033346, -12.91256367767457647, 13.08452859117697642 ) ) ;
#23176 = ORIENTED_EDGE ( 'NONE', *, *, #81317, .T. ) ;
#23177 = EDGE_CURVE ( 'NONE', #6442, #74331, #34649, .T. ) ;
#23178 = CONICAL_SURFACE ( 'NONE', #21425, 4.172000000000009479, 0.9599310885968813656 ) ;
#23179 = DIRECTION ( 'NONE',  ( -1.000000000000000000, -1.224606353822377258E-16, -0.000000000000000000 ) ) ;
#23180 = CARTESIAN_POINT ( 'NONE',  ( 6.499999999999999112, -3.752776749732586126, -6.064240316920402663 ) ) ;
#23181 = CARTESIAN_POINT ( 'NONE',  ( -9.910377230549929806, 15.23810023151366799, -1.510421413154898085 ) ) ;
#23182 = CARTESIAN_POINT ( 'NONE',  ( -107.9249424950986906, -57.65976581800653378, 199.0938304663491749 ) ) ;
#23183 = CARTESIAN_POINT ( 'NONE',  ( -5.192560085536412906, -67.64305442631241760, 3.013051918867556189 ) ) ;
#23184 = CARTESIAN_POINT ( 'NONE',  ( 3.978477517404916064, 5.573260695678952104, -6.171287963165197787 ) ) ;
#23185 = CARTESIAN_POINT ( 'NONE',  ( -1.249962610845875011, 25.55812661083311710, 39.65902825006367749 ) ) ;
#23186 = CARTESIAN_POINT ( 'NONE',  ( 7.149395896920095848E-21, 27.29656849860388235, -40.75000000000000000 ) ) ;
#23187 = CARTESIAN_POINT ( 'NONE',  ( -42.61015704936735915, -60.00000000000002842, -41.65925318937349431 ) ) ;
#23188 = EDGE_CURVE ( 'NONE', #94271, #64087, #92298, .T. ) ;
#23189 = CARTESIAN_POINT ( 'NONE',  ( -21.36131896786188378, -60.00000000000002132, 42.72829597934922674 ) ) ;
#23190 = ADVANCED_FACE ( 'NONE', ( #67519 ), #17382, .F. ) ;
#23191 = CARTESIAN_POINT ( 'NONE',  ( -54.02244926336294384, -36.03399488101162973, 56.88089687501458513 ) ) ;
#23192 = DIRECTION ( 'NONE',  ( 0.000000000000000000, 1.000000000000000000, 0.000000000000000000 ) ) ;
#23193 = AXIS2_PLACEMENT_3D ( 'NONE', #11000, #43394, #93000 ) ;
#23194 = ORIENTED_EDGE ( 'NONE', *, *, #4528, .T. ) ;
#23195 = AXIS2_PLACEMENT_3D ( 'NONE', #78356, #29326, #104221 ) ;
#23196 = CARTESIAN_POINT ( 'NONE',  ( -98.75517273381713323, -60.33577106688449732, 196.3359775619156267 ) ) ;
#23197 = STYLED_ITEM ( 'NONE', ( #17050 ), #55728 ) ;
#23198 = APPLICATION_CONTEXT ( 'automotive_design' ) ;
#23199 = CARTESIAN_POINT ( 'NONE',  ( -5.800920608303504977, 296.2164713808596161, -10.01425861749949320 ) ) ;
#23200 = ORIENTED_EDGE ( 'NONE', *, *, #38606, .T. ) ;
#23201 = CARTESIAN_POINT ( 'NONE',  ( 19.00081985458449552, 49.50573636308028824, 61.91387040241579598 ) ) ;
#23202 = PRESENTATION_LAYER_ASSIGNMENT (  '', '', ( #52423 ) ) ;
#23203 = CARTESIAN_POINT ( 'NONE',  ( 91.32721440143633629, -38.40026762824159334, -10.23153405760255197 ) ) ;
#23204 = CARTESIAN_POINT ( 'NONE',  ( 20.00000000000000711, 4.000000000000000000, -1.500000000000000000 ) ) ;
#23205 = DIRECTION ( 'NONE',  ( -1.000000000000000000, -1.224606353822377258E-16, -0.000000000000000000 ) ) ;
#23207 = EDGE_CURVE ( 'NONE', #18742, #79592, #81968, .T. ) ;
#23206 = CARTESIAN_POINT ( 'NONE',  ( -10.01511786699015438, 294.6430527449200554, 9.892628225130204456 ) ) ;
#23208 = AXIS2_PLACEMENT_3D ( 'NONE', #74812, #9551, #98563 ) ;
#23209 = DIRECTION ( 'NONE',  ( 0.9396926207859143121, 1.150791560227857665E-16, -0.3420201433256525592 ) ) ;
#23210 = CARTESIAN_POINT ( 'NONE',  ( 82.11220676860955336, -29.99999999999999645, 146.7337359989799381 ) ) ;
#23211 = DIRECTION ( 'NONE',  ( 1.000000000000000000, -0.000000000000000000, -0.000000000000000000 ) ) ;
#23212 = CARTESIAN_POINT ( 'NONE',  ( 36.08160016961308969, 491.3801102092154451, 12.28496641016068835 ) ) ;
#23213 = CARTESIAN_POINT ( 'NONE',  ( -0.6464587407298656441, 35.01841617270944340, 27.41698562527900407 ) ) ;
#23214 = CARTESIAN_POINT ( 'NONE',  ( 5.656854249492380582, -24.31249999999999289, -5.656854249492379694 ) ) ;
#23215 = ORIENTED_EDGE ( 'NONE', *, *, #30661, .T. ) ;
#23216 = VERTEX_POINT ( 'NONE', #10321 ) ;
#23217 = CARTESIAN_POINT ( 'NONE',  ( 50.06701392515735449, -46.43829384136844141, 53.18051123607877884 ) ) ;
#23218 = CARTESIAN_POINT ( 'NONE',  ( -10.00000000000000000, -15.00000000000000000, 10.00000000000000178 ) ) ;
#23219 = CARTESIAN_POINT ( 'NONE',  ( -6.242019780568027976, 15.46330733086430875, 3.192545347364962094 ) ) ;
#23220 = CARTESIAN_POINT ( 'NONE',  ( -110.5050194399237000, -38.35611022050278507, 182.3353135514281007 ) ) ;
#23221 = ORIENTED_EDGE ( 'NONE', *, *, #91189, .T. ) ;
#23222 = CARTESIAN_POINT ( 'NONE',  ( 108.7582993695906453, -38.35601099000350445, 143.4284137783402286 ) ) ;
#23223 = CARTESIAN_POINT ( 'NONE',  ( 11.45439866395856221, 9.461585312351356691, -9.377169115924592901 ) ) ;
#23224 = DIRECTION ( 'NONE',  ( 0.000000000000000000, 0.000000000000000000, 1.000000000000000000 ) ) ;
#23225 = CARTESIAN_POINT ( 'NONE',  ( 100.3592460791940368, -52.71701722894771081, 125.2415931128299746 ) ) ;
#23226 = SURFACE_SIDE_STYLE ('',( #13502 ) ) ;
#23227 = CARTESIAN_POINT ( 'NONE',  ( 22.39889803669582236, 27.64071832785176852, 32.90416900124247945 ) ) ;
#23228 = CARTESIAN_POINT ( 'NONE',  ( 32.94021323899735165, 485.0599191339526328, 5.361609822540882142 ) ) ;
#23229 = CYLINDRICAL_SURFACE ( 'NONE', #69027, 1.250000000000001110 ) ;
#23230 = CARTESIAN_POINT ( 'NONE',  ( -30.00000000000000355, 488.7759232732886403, 4.253593570507368860 ) ) ;
#23231 = CARTESIAN_POINT ( 'NONE',  ( 80.14078518684225116, -60.00000000000000711, 196.1583502975230999 ) ) ;
#23232 = CIRCLE ( 'NONE', #88655, 0.5000000000000004441 ) ;
#23233 = SURFACE_STYLE_USAGE ( .BOTH. , #97091 ) ;
#23234 = EDGE_LOOP ( 'NONE', ( #94194, #34806, #43045, #57069, #3780, #57153 ) ) ;
#23235 = CARTESIAN_POINT ( 'NONE',  ( 57.05946111255018849, -46.43605047800132724, 67.94431784311699118 ) ) ;
#23236 = CARTESIAN_POINT ( 'NONE',  ( -31.85803618339147647, 298.6540356601998951, -9.160706982464283499 ) ) ;
#23237 = DIRECTION ( 'NONE',  ( 0.000000000000000000, 0.000000000000000000, -1.000000000000000000 ) ) ;
#23238 = CARTESIAN_POINT ( 'NONE',  ( -7.212994264445060644, 27.98288655659961321, 3.463766307298586256 ) ) ;
#23239 = ORIENTED_EDGE ( 'NONE', *, *, #16456, .T. ) ;
#23241 = CARTESIAN_POINT ( 'NONE',  ( -9.612665144396085992, -50.98869060647467677, 29.76292019730385618 ) ) ;
#23240 = CARTESIAN_POINT ( 'NONE',  ( -94.79426203886504254, -38.48922377310545784, 201.2511363089133738 ) ) ;
#23242 = CARTESIAN_POINT ( 'NONE',  ( 6.990291106834062518, -2.999999999999999556, 4.028951842967195773 ) ) ;
#23243 = CARTESIAN_POINT ( 'NONE',  ( 31.18772345825684056, 357.3324404125347087, 20.56444635957918265 ) ) ;
#23244 = CARTESIAN_POINT ( 'NONE',  ( 0.000000000000000000, 7.511572993685796142E-16, -6.500000000000000888 ) ) ;
#23245 = CARTESIAN_POINT ( 'NONE',  ( 8.000000000000000000, -31.90625000000000000, -3.313708498984761608 ) ) ;
#23246 = CARTESIAN_POINT ( 'NONE',  ( 7.996668422914432028, -4.999999999991826094, -91.14546720080765851 ) ) ;
#23247 = EDGE_CURVE ( 'NONE', #12797, #6938, #57966, .T. ) ;
#23248 = CARTESIAN_POINT ( 'NONE',  ( 2.500000000000002220, -8.000000000000000000, -17.89626171146327138 ) ) ;
#23249 = ORIENTED_EDGE ( 'NONE', *, *, #16840, .F. ) ;
#23250 = CARTESIAN_POINT ( 'NONE',  ( 82.69827821110598620, -46.48414492152276267, 177.5876388581721699 ) ) ;
#23251 = CARTESIAN_POINT ( 'NONE',  ( -46.00000000000000000, 461.5923978621302695, 9.841791816127033243 ) ) ;
#23252 = CARTESIAN_POINT ( 'NONE',  ( -42.19180677453720563, 462.2931784592652207, 3.389262873192004477 ) ) ;
#23253 = ORIENTED_EDGE ( 'NONE', *, *, #87585, .F. ) ;
#23254 = CARTESIAN_POINT ( 'NONE',  ( 25.53945892759312031, 1.340359594676612611E-15, 0.000000000000000000 ) ) ;
#23255 = CARTESIAN_POINT ( 'NONE',  ( 6.689814467814940713, -4.999999999994905409, -16.20004731218675786 ) ) ;
#23256 = DIRECTION ( 'NONE',  ( 0.000000000000000000, 0.000000000000000000, 1.000000000000000000 ) ) ;
#23257 = CARTESIAN_POINT ( 'NONE',  ( -6.061808134820600991, 49.99999999999999289, -74.52203418564695880 ) ) ;
#23258 = CARTESIAN_POINT ( 'NONE',  ( -39.03259858841720131, 42.04011792294609506, -56.83904871932554670 ) ) ;
#23259 = CARTESIAN_POINT ( 'NONE',  ( 0.000000000000000000, 0.000000000000000000, 0.000000000000000000 ) ) ;
#23260 = EDGE_CURVE ( 'NONE', #65105, #104028, #86895, .T. ) ;
#23261 = ORIENTED_EDGE ( 'NONE', *, *, #102731, .T. ) ;
#23262 = AXIS2_PLACEMENT_3D ( 'NONE', #105838, #15772, #97739 ) ;
#23263 = CARTESIAN_POINT ( 'NONE',  ( 38.77580872333679451, 25.24258365861260245, 11.84918804548649618 ) ) ;
#23264 = CARTESIAN_POINT ( 'NONE',  ( -4.781335833249817036, -47.33012453287045673, 102.4226025779373401 ) ) ;
#23266 = CARTESIAN_POINT ( 'NONE',  ( -11.42336277867628880, 14.22106288968689469, -9.929318634850201164 ) ) ;
#23265 = DIRECTION ( 'NONE',  ( -0.000000000000000000, -1.000000000000000000, -0.000000000000000000 ) ) ;
#23267 = VECTOR ( 'NONE', #19074, 1000.000000000000000 ) ;
#23268 = CARTESIAN_POINT ( 'NONE',  ( -7.188101187500000044, -16.90625000204838813, -8.802885111219163269E-16 ) ) ;
#23269 = UNCERTAINTY_MEASURE_WITH_UNIT (LENGTH_MEASURE( 1.000000000000000082E-05 ), #62595, 'distance_accuracy_value', 'NONE');
#23270 = DIRECTION ( 'NONE',  ( -1.000000000000000000, 0.000000000000000000, 0.000000000000000000 ) ) ;
#23271 = MECHANICAL_DESIGN_GEOMETRIC_PRESENTATION_REPRESENTATION (  '', ( #71512 ), #85224 ) ;
#23272 = COLOUR_RGB ( '', 0.31764706, 0.68627451, 0.89019608) ;
#23273 = AXIS2_PLACEMENT_3D ( 'NONE', #26370, #82431, #931 ) ;
#23274 = EDGE_CURVE ( 'NONE', #61302, #54801, #13060, .T. ) ;
#23275 = EDGE_CURVE ( 'NONE', #57839, #59054, #20787, .T. ) ;
#23276 = PRESENTATION_LAYER_ASSIGNMENT (  '', '', ( #42190 ) ) ;
#23277 = ORIENTED_EDGE ( 'NONE', *, *, #12450, .F. ) ;
#23278 = FACE_BOUND ( 'NONE', #6975, .T. ) ;
#23279 = CARTESIAN_POINT ( 'NONE',  ( 0.000000000000000000, 0.000000000000000000, 5.000000000000000888 ) ) ;
#23280 = CARTESIAN_POINT ( 'NONE',  ( -4.072841793016302780, 138.0987898825082709, -5.000000000000000000 ) ) ;
#23281 = DIRECTION ( 'NONE',  ( -1.000000000000000000, -0.000000000000000000, -0.000000000000000000 ) ) ;
#23282 = CARTESIAN_POINT ( 'NONE',  ( -14.71845092680128353, 2.464670597987486111, 2.845879451984156372 ) ) ;
#23283 = ORIENTED_EDGE ( 'NONE', *, *, #9804, .F. ) ;
#23284 = DIRECTION ( 'NONE',  ( 0.000000000000000000, -1.000000000000000000, 0.000000000000000000 ) ) ;
#23285 = LINE ( 'NONE', #56123, #87586 ) ;
#23286 = ORIENTED_EDGE ( 'NONE', *, *, #19466, .T. ) ;
#23287 =( BOUNDED_SURFACE ( )  B_SPLINE_SURFACE ( 3, 2, ( 
 ( #2630, #9121, #42031 ),
 ( #41500, #33435, #27498 ),
 ( #83548, #42558, #60373 ),
 ( #66309, #74913, #84092 ),
 ( #10192, #33978, #34519 ),
 ( #25909, #58765, #91663 ) ),
 .UNSPECIFIED., .F., .F., .T. ) 
 B_SPLINE_SURFACE_WITH_KNOTS ( ( 4, 2, 4 ),
 ( 3, 3 ),
 ( 0.000000000000000000, 0.001801542390204249932, 0.003603084780408499863 ),
 ( 0.000000000000000000, 1.000000000000000000 ),
 .UNSPECIFIED. ) 
 GEOMETRIC_REPRESENTATION_ITEM ( )  RATIONAL_B_SPLINE_SURFACE ( (
 ( 1.000000000000000000, 0.8291561975888502856, 1.000000000000000000),
 ( 1.000000000000000000, 0.8506934603555468266, 1.000000000000000000),
 ( 1.000000000000000000, 0.8671388017648747892, 1.000000000000000000),
 ( 1.000000000000000000, 0.8933560653593087819, 1.000000000000000000),
 ( 1.000000000000000000, 0.9032011672210142894, 1.000000000000000000),
 ( 1.000000000000000000, 0.9115707425106691630, 1.000000000000000000) ) ) 
 REPRESENTATION_ITEM ( '' )  SURFACE ( )  );
#23288 = CARTESIAN_POINT ( 'NONE',  ( -2.499999999999978684, -26.27793898787864890, 28.26590982313834743 ) ) ;
#23289 = CARTESIAN_POINT ( 'NONE',  ( 6.913779129928547817, 41.73441125232163529, -59.30275354417914713 ) ) ;
#23290 = UNCERTAINTY_MEASURE_WITH_UNIT (LENGTH_MEASURE( 1.000000000000000082E-05 ), #19208, 'distance_accuracy_value', 'NONE');
#23291 = CARTESIAN_POINT ( 'NONE',  ( -112.2289492798716566, -60.00000000000000000, 172.3416561640010798 ) ) ;
#23292 = CARTESIAN_POINT ( 'NONE',  ( 29.28883047145494345, 14.13190579697306504, -42.04354307362351761 ) ) ;
#23293 = CARTESIAN_POINT ( 'NONE',  ( 5.513005039581024867E-05, -56.88429987697963952, 33.37036660576565339 ) ) ;
#23294 = DIRECTION ( 'NONE',  ( 0.5735764363510468256, 0.8191520442889913545, 0.000000000000000000 ) ) ;
#23295 = CARTESIAN_POINT ( 'NONE',  ( -12.14072642854974760, 2.000560067487730631, 14.86685304370069538 ) ) ;
#23296 =( BOUNDED_SURFACE ( )  B_SPLINE_SURFACE ( 3, 2, ( 
 ( #59726, #92601, #21276 ),
 ( #67804, #18756, #86538 ),
 ( #4522, #1988, #101240 ),
 ( #27393, #51063, #35471 ),
 ( #93142, #37466, #19312 ),
 ( #92068, #50530, #87055 ),
 ( #42999, #1445, #13127 ),
 ( #46053, #34408, #26856 ),
 ( #5061, #58656, #91558 ),
 ( #100686, #83442, #9545 ),
 ( #42454, #34935, #26329 ),
 ( #10090, #46572, #79467 ),
 ( #96725, #88627, #54641 ),
 ( #6636, #81047, #63306 ),
 ( #14186, #32002, #39026 ),
 ( #80517, #71370, #105340 ) ),
 .UNSPECIFIED., .F., .F., .F. ) 
 B_SPLINE_SURFACE_WITH_KNOTS ( ( 4, 2, 2, 2, 2, 2, 2, 4 ),
 ( 3, 3 ),
 ( 0.01025942932839742430, 0.01330785678258415185, 0.01483207050967751475, 0.01635628423677087939, 0.01788049796386424403, 0.01940471169095760867, 0.02092892541805096984, 0.02245313914514433448 ),
 ( 0.3005395333819582682, 1.000000000000000000 ),
 .UNSPECIFIED. ) 
 GEOMETRIC_REPRESENTATION_ITEM ( )  RATIONAL_B_SPLINE_SURFACE ( (
 ( 0.8980036390038548255, 0.8303112408401241984, 1.000000000000000000),
 ( 0.9116818979159833081, 0.8530674133113587132, 1.000000000000000000),
 ( 0.9228127777806771626, 0.8715855758629514893, 1.000000000000000000),
 ( 0.9345546761373628719, 0.8911202743842321361, 1.000000000000000000),
 ( 0.9375544117806124955, 0.8961108585005606031, 1.000000000000000000),
 ( 0.9415935919673705801, 0.9028307401435932134, 1.000000000000000000),
 ( 0.9426280110962133030, 0.9045516770153625430, 1.000000000000000000),
 ( 0.9426141662316163128, 0.9045286436652386630, 1.000000000000000000),
 ( 0.9415455155260004094, 0.9027507565873051920, 1.000000000000000000),
 ( 0.9374309181788871292, 0.8959054053271698903, 1.000000000000000000),
 ( 0.9344062863249886774, 0.8908734020165530731, 1.000000000000000000),
 ( 0.9266839229612940931, 0.8780259019276379640, 1.000000000000000000),
 ( 0.9219922915688816278, 0.8702205537599312368, 1.000000000000000000),
 ( 0.9110602365935736024, 0.8520331711346073034, 1.000000000000000000),
 ( 0.9047689875052107311, 0.8415665795724794895, 1.000000000000000000),
 ( 0.8980036390038557137, 0.8303112408401255307, 1.000000000000000000) ) ) 
 REPRESENTATION_ITEM ( '' )  SURFACE ( )  );
#23298 = CARTESIAN_POINT ( 'NONE',  ( 35.17658899013087392, 491.5165241545285539, 12.37078523472800207 ) ) ;
#23297 = CARTESIAN_POINT ( 'NONE',  ( 11.99999999999999467, -5.000000000000002665, -83.42920367501479006 ) ) ;
#23299 = CARTESIAN_POINT ( 'NONE',  ( -84.00855389726528699, -35.95715071644597316, 173.7904060909261830 ) ) ;
#23300 = ORIENTED_EDGE ( 'NONE', *, *, #62905, .T. ) ;
#23302 = CARTESIAN_POINT ( 'NONE',  ( 4.852941176470593199, 24.91666666666666430, -70.80672828634229177 ) ) ;
#23301 = B_SPLINE_CURVE_WITH_KNOTS ( 'NONE', 3,
 ( #83439, #3061, #42996, #51602, #93138, #10609, #68338, #101236, #34404, #67798, #67280, #100158, #18207, #34931, #26852, #27389, #60269, #95802 ),
 .UNSPECIFIED., .F., .F.,
 ( 4, 2, 2, 2, 2, 2, 2, 2, 4 ),
 ( 0.005148306559854647947, 0.006154786515368258250, 0.006658026493125070340, 0.006909646482003478120, 0.007161266470881886767, 0.007664506448638707531, 0.008167746426395530029, 0.008670986404152350793, 0.009174226381909171557 ),
 .UNSPECIFIED. ) ;
#23303 = MECHANICAL_DESIGN_GEOMETRIC_PRESENTATION_REPRESENTATION (  '', ( #4348 ), #37107 ) ;
#23304 = EDGE_LOOP ( 'NONE', ( #43859, #60440, #20944, #19016, #56565, #48278 ) ) ;
#23305 = CARTESIAN_POINT ( 'NONE',  ( 29.83349330513380693, 1.593028355512270962E-15, 0.000000000000000000 ) ) ;
#23306 =( LENGTH_UNIT ( ) NAMED_UNIT ( * ) SI_UNIT ( .MILLI., .METRE. ) );
#23307 = DIRECTION ( 'NONE',  ( -0.5735764363510497121, 0.8191520442889892450, 1.003171929053521665E-16 ) ) ;
#23308 = CARTESIAN_POINT ( 'NONE',  ( -16.13590653351237236, 6.313628335805701930, -5.716602451449800171 ) ) ;
#23309 = CARTESIAN_POINT ( 'NONE',  ( 4.323075853814730252, 10.88581780261195142, -5.000000000000000000 ) ) ;
#23310 = LINE ( 'NONE', #82584, #33905 ) ;
#23311 = CARTESIAN_POINT ( 'NONE',  ( 0.000000000000000000, 80.00000000000000000, 0.000000000000000000 ) ) ;
#23312 = CARTESIAN_POINT ( 'NONE',  ( 105.4249980201500136, -14.21045842199437992, 149.5332359265665900 ) ) ;
#23313 = CARTESIAN_POINT ( 'NONE',  ( -102.0721909215208427, -14.21045842199424314, 125.2231725879975954 ) ) ;
#23314 = CARTESIAN_POINT ( 'NONE',  ( -62.57693323230586913, -46.43962359317384170, 82.71524195557942960 ) ) ;
#23315 = EDGE_LOOP ( 'NONE', ( #13490, #58704 ) ) ;
#23316 = CARTESIAN_POINT ( 'NONE',  ( 51.48757442383971039, 38.95383793068617706, -37.45149417477087184 ) ) ;
#23317 = CARTESIAN_POINT ( 'NONE',  ( 47.44420658916666156, -59.99999999998034639, 71.74659173365184017 ) ) ;
#23318 = ORIENTED_EDGE ( 'NONE', *, *, #73101, .F. ) ;
#23319 = CARTESIAN_POINT ( 'NONE',  ( 4.937715695759576327E-05, -53.39687648151041799, 32.78912937318744980 ) ) ;
#23320 = CARTESIAN_POINT ( 'NONE',  ( -1.320432766682874540E-15, -21.40625000204838457, 7.188101187500000044 ) ) ;
#23321 = CARTESIAN_POINT ( 'NONE',  ( -32.64147241561564528, 439.6779429780672217, 24.07034118911103349 ) ) ;
#23322 = VERTEX_POINT ( 'NONE', #99059 ) ;
#23323 = CARTESIAN_POINT ( 'NONE',  ( -11.04556819181654426, 45.87714785467576917, 13.15211296974101174 ) ) ;
#23324 = EDGE_LOOP ( 'NONE', ( #105054, #82435, #86783, #97196, #90671 ) ) ;
#23325 = DIRECTION ( 'NONE',  ( -1.000000000000000000, -1.224606353822377258E-16, -0.000000000000000000 ) ) ;
#23326 = DIRECTION ( 'NONE',  ( 0.000000000000000000, 0.000000000000000000, 1.000000000000000000 ) ) ;
#23327 = CARTESIAN_POINT ( 'NONE',  ( -107.9034470886846293, -59.99999999999998579, 195.8034858462665682 ) ) ;
#23328 = CARTESIAN_POINT ( 'NONE',  ( -3.396360046677147970, -0.8468429378656776585, 103.9790200242172062 ) ) ;
#23329 = CARTESIAN_POINT ( 'NONE',  ( 5.082755093536324154, -28.71875000204838813, 5.082755093536326818 ) ) ;
#23330 = CARTESIAN_POINT ( 'NONE',  ( 8.000000000000000000, 9.797174393178825657E-16, -3.725171428571429022 ) ) ;
#23331 = ADVANCED_FACE ( 'NONE', ( #14552 ), #85468, .T. ) ;
#23332 = CARTESIAN_POINT ( 'NONE',  ( -6.544853860617209307, 53.53209805210580896, -7.402906068179443189 ) ) ;
#23333 = CARTESIAN_POINT ( 'NONE',  ( 5.000000000000000000, -14.29136116388517941, -6.556186629969792179 ) ) ;
#23334 = CARTESIAN_POINT ( 'NONE',  ( 1.224646799147352665E-15, 48.00000000000000000, -75.00000000000001421 ) ) ;
#23335 = EDGE_CURVE ( 'NONE', #43284, #43900, #88847, .T. ) ;
#23336 = CARTESIAN_POINT ( 'NONE',  ( -7.002641335706726977, 106.0508726268083279, 3.868676264653295060 ) ) ;
#23337 = CARTESIAN_POINT ( 'NONE',  ( -43.61009301646220138, 374.8108257898446141, 14.43920481438196468 ) ) ;
#23338 = AXIS2_PLACEMENT_3D ( 'NONE', #64220, #86904, #103597 ) ;
#23339 = CARTESIAN_POINT ( 'NONE',  ( 20.49977525862259142, 302.8459220885798686, -10.00124997875687427 ) ) ;
#23340 = CARTESIAN_POINT ( 'NONE',  ( -34.27342318777111529, -60.30598541217121067, 38.86820545827612960 ) ) ;
#23341 = ORIENTED_EDGE ( 'NONE', *, *, #50288, .T. ) ;
#23342 = CARTESIAN_POINT ( 'NONE',  ( 37.73904784516052047, -32.59126324431009181, 35.55316273275742134 ) ) ;
#23343 = AXIS2_PLACEMENT_3D ( 'NONE', #23352, #23895, #89129 ) ;
#23344 = CARTESIAN_POINT ( 'NONE',  ( 10.45706415777664411, -1.734723475976807094E-15, 13.60704923275374156 ) ) ;
#23345 = EDGE_CURVE ( 'NONE', #70963, #36026, #52723, .T. ) ;
#23346 = EDGE_LOOP ( 'NONE', ( #10983, #83479, #72508 ) ) ;
#23347 = CARTESIAN_POINT ( 'NONE',  ( 34.15253942429875877, 465.0582672257839363, 17.72214182034170094 ) ) ;
#23348 = CARTESIAN_POINT ( 'NONE',  ( -58.38338069927746687, -38.34396774324475388, 91.39933602100487064 ) ) ;
#23349 = CONICAL_SURFACE ( 'NONE', #88771, 4.172000000000001485, 0.9599310885968750373 ) ;
#23350 = EDGE_LOOP ( 'NONE', ( #39609, #22447, #81613, #32035, #17191, #55450 ) ) ;
#23352 = CARTESIAN_POINT ( 'NONE',  ( 19.83349330513379982, 1.593028355512270567E-15, 0.000000000000000000 ) ) ;
#23351 = CARTESIAN_POINT ( 'NONE',  ( 7.146471073273054309, -5.000000000000000000, -15.44879583875536788 ) ) ;
#23353 = FACE_BOUND ( 'NONE', #85068, .T. ) ;
#23354 = CARTESIAN_POINT ( 'NONE',  ( 90.51111111111110574, 1.023464760207051730E-14, 0.000000000000000000 ) ) ;
#23355 = CONICAL_SURFACE ( 'NONE', #73262, 5.000000000000001776, 0.9599310885968803664 ) ;
#23356 = AXIS2_PLACEMENT_3D ( 'NONE', #42518, #3131, #26391 ) ;
#23357 = LINE ( 'NONE', #47061, #26980 ) ;
#23358 = DIRECTION ( 'NONE',  ( -1.000000000000000000, -1.224606353822377258E-16, -0.000000000000000000 ) ) ;
#23359 = CONICAL_SURFACE ( 'NONE', #80209, 46.94949242731048145, 0.3972631705159501148 ) ;
#23360 = CARTESIAN_POINT ( 'NONE',  ( 4.497472161260645862, -85.54222546625945256, -3.972129482042464410 ) ) ;
#23361 = CARTESIAN_POINT ( 'NONE',  ( -5.000000000000000888, -46.00000000000000000, 42.58845726811989607 ) ) ;
#23362 = CARTESIAN_POINT ( 'NONE',  ( 98.38154907885181899, -60.00000000000002132, 71.28785646064007153 ) ) ;
#23363 = AXIS2_PLACEMENT_3D ( 'NONE', #12201, #76941, #92591 ) ;
#23364 = CARTESIAN_POINT ( 'NONE',  ( -43.52075891743668734, 484.7805561108187931, 4.063293749114571085 ) ) ;
#23365 = DIRECTION ( 'NONE',  ( -1.000000000000000000, -0.000000000000000000, -0.000000000000000000 ) ) ;
#23366 = CARTESIAN_POINT ( 'NONE',  ( 7.225703553013920200, -4.999999999999999112, -73.19314196553180807 ) ) ;
#23367 = ORIENTED_EDGE ( 'NONE', *, *, #55553, .T. ) ;
#23368 = CARTESIAN_POINT ( 'NONE',  ( -90.08654180215627605, -30.00000000002151879, -7.787506975155032762 ) ) ;
#23369 = ORIENTED_EDGE ( 'NONE', *, *, #74805, .T. ) ;
#23370 = CARTESIAN_POINT ( 'NONE',  ( 79.82022815836235452, 6.123233995736582872E-16, -5.000000000000011546 ) ) ;
#23371 = CARTESIAN_POINT ( 'NONE',  ( -15.13200660511302864, 3.596720279098536643, -4.250825932781741479 ) ) ;
#23372 = CARTESIAN_POINT ( 'NONE',  ( 4.678819457397437098, 8.078722181090839172, 5.000000000000000000 ) ) ;
#23373 = CARTESIAN_POINT ( 'NONE',  ( 16.14595037822608603, 20.23371447307436810, 4.922994507617730164 ) ) ;
#23374 = DIRECTION ( 'NONE',  ( 0.5564727496918392413, -0.8308658609248569249, 1.930652685263598448E-16 ) ) ;
#23375 = CARTESIAN_POINT ( 'NONE',  ( 5.082755093536325930, -28.34375000204838813, -5.082755093536325042 ) ) ;
#23376 = DIRECTION ( 'NONE',  ( -1.000000000000000000, -1.224606353822377258E-16, -0.000000000000000000 ) ) ;
#23377 = SURFACE_STYLE_FILL_AREA ( #22853 ) ;
#23378 = CARTESIAN_POINT ( 'NONE',  ( 7.425259286936451986, 41.08730335070794126, -69.63985817587276017 ) ) ;
#23379 = ORIENTED_EDGE ( 'NONE', *, *, #79742, .F. ) ;
#23380 = EDGE_CURVE ( 'NONE', #72225, #81898, #15555, .T. ) ;
#23382 = ORIENTED_EDGE ( 'NONE', *, *, #99330, .T. ) ;
#23381 = DIRECTION ( 'NONE',  ( 0.000000000000000000, -0.000000000000000000, 1.000000000000000000 ) ) ;
#23383 = CARTESIAN_POINT ( 'NONE',  ( 79.16796225250830332, -56.84377630782282154, 161.1938245440812238 ) ) ;
#23384 = CARTESIAN_POINT ( 'NONE',  ( -38.81967570215591223, 27.30152829859311225, -12.34949243608158831 ) ) ;
#23385 = EDGE_LOOP ( 'NONE', ( #21441, #32523, #86415, #60832, #81030, #8727, #90650, #50462 ) ) ;
#23386 = DIRECTION ( 'NONE',  ( 0.000000000000000000, -1.000000000000000000, 0.000000000000000000 ) ) ;
#23387 = DIRECTION ( 'NONE',  ( 0.000000000000000000, 0.000000000000000000, -1.000000000000000000 ) ) ;
#23388 = CARTESIAN_POINT ( 'NONE',  ( 2.977408999572650927, -12.87500000204838280, -7.188101187500000933 ) ) ;
#23389 = DIRECTION ( 'NONE',  ( 0.000000000000000000, 0.000000000000000000, -1.000000000000000000 ) ) ;
#23390 = AXIS2_PLACEMENT_3D ( 'NONE', #99113, #49512, #25833 ) ;
#23391 = CARTESIAN_POINT ( 'NONE',  ( -43.09316981551443604, -57.68566503113564892, 61.19926976090692960 ) ) ;
#23392 = CARTESIAN_POINT ( 'NONE',  ( 16.52192859150929749, 294.5714182157683467, 9.877401045508872102 ) ) ;
#23393 = ADVANCED_FACE ( 'NONE', ( #39401 ), #105183, .F. ) ;
#23394 = VERTEX_POINT ( 'NONE', #56063 ) ;
#23395 = SURFACE_STYLE_USAGE ( .BOTH. , #14197 ) ;
#23396 = DIRECTION ( 'NONE',  ( 0.000000000000000000, 0.4999999999999996114, -0.8660254037844388186 ) ) ;
#23397 = CARTESIAN_POINT ( 'NONE',  ( 7.302130867679851534, 41.45639825872783035, -59.68093889946540287 ) ) ;
#23398 = LINE ( 'NONE', #48163, #72322 ) ;
#23399 = VERTEX_POINT ( 'NONE', #89003 ) ;
#23400 = CARTESIAN_POINT ( 'NONE',  ( -3.313708498984760720, -13.71875000409676915, -8.000000000000000000 ) ) ;
#23401 = CARTESIAN_POINT ( 'NONE',  ( -22.41876583820823399, -18.13681534289955621, 31.47717130250301310 ) ) ;
#23402 = CARTESIAN_POINT ( 'NONE',  ( 9.999999999999998224, 15.00000000000000000, 0.7768758660237408131 ) ) ;
#23403 = CARTESIAN_POINT ( 'NONE',  ( 0.000000000000000000, 0.000000000000000000, 0.000000000000000000 ) ) ;
#23404 = EDGE_CURVE ( 'NONE', #96013, #94251, #95793, .T. ) ;
#23405 = DIRECTION ( 'NONE',  ( 0.000000000000000000, 0.000000000000000000, 1.000000000000000000 ) ) ;
#23406 = CARTESIAN_POINT ( 'NONE',  ( 34.01853213578340984, 439.9180697526190897, 24.30896811189926154 ) ) ;
#23407 = AXIS2_PLACEMENT_3D ( 'NONE', #105754, #63197, #80408 ) ;
#23408 = SHAPE_DEFINITION_REPRESENTATION ( #21843, #55690 ) ;
#23409 = CARTESIAN_POINT ( 'NONE',  ( 38.76904556471400554, 27.37270507303107436, 11.85428640503262088 ) ) ;
#23410 = ORIENTED_EDGE ( 'NONE', *, *, #35470, .F. ) ;
#23411 = CARTESIAN_POINT ( 'NONE',  ( -4.825525552038038235, -47.21979206537751139, 40.34253552477181159 ) ) ;
#23412 = CARTESIAN_POINT ( 'NONE',  ( -2.701558353794592193, 15.00000000000000000, 9.999999999999998224 ) ) ;
#23413 = DIRECTION ( 'NONE',  ( -1.000000000000000000, -1.224606353822377258E-16, -0.000000000000000000 ) ) ;
#23414 = CARTESIAN_POINT ( 'NONE',  ( 16.29626706464026142, -24.48722485856961484, -38.53282975460095372 ) ) ;
#23415 = CARTESIAN_POINT ( 'NONE',  ( -54.73325009968991139, -30.00000000000000355, 55.16748736607294035 ) ) ;
#23416 = EDGE_CURVE ( 'NONE', #7097, #2627, #80207, .T. ) ;
#23417 = DIRECTION ( 'NONE',  ( -1.000000000000000000, -0.000000000000000000, -0.000000000000000000 ) ) ;
#23418 = CONICAL_SURFACE ( 'NONE', #90522, 3.309500000000007880, 0.9599310885968770357 ) ;
#23419 = VERTEX_POINT ( 'NONE', #63139 ) ;
#23420 = LINE ( 'NONE', #105890, #58232 ) ;
#23421 = CARTESIAN_POINT ( 'NONE',  ( 102.5075976590412807, -57.63377371069149291, 203.0662124941956108 ) ) ;
#23422 = ADVANCED_FACE ( 'NONE', ( #72795 ), #44118, .T. ) ;
#23423 = CARTESIAN_POINT ( 'NONE',  ( 37.07355662510760652, 464.0045528213532293, 19.58584291727852644 ) ) ;
#23424 = CARTESIAN_POINT ( 'NONE',  ( 6.400000000000000355, 4.618802153517003184, -8.000000000000000000 ) ) ;
#23425 = AXIS2_PLACEMENT_3D ( 'NONE', #92122, #33927, #35527 ) ;
#23426 = CARTESIAN_POINT ( 'NONE',  ( -5.457055012756472756, 53.44272100380801049, 8.531152949374559924 ) ) ;
#23427 = CARTESIAN_POINT ( 'NONE',  ( -73.05702173334942984, -60.00000000000000711, 162.9805030633762613 ) ) ;
#23428 = EDGE_CURVE ( 'NONE', #28900, #47541, #94003, .T. ) ;
#23429 = AXIS2_PLACEMENT_3D ( 'NONE', #10938, #2860, #35814 ) ;
#23430 = CIRCLE ( 'NONE', #76749, 0.9999999999999854561 ) ;
#23431 = CARTESIAN_POINT ( 'NONE',  ( -40.17205142263708240, 310.2804317922712016, -6.358608209523628929 ) ) ;
#23432 = SURFACE_STYLE_USAGE ( .BOTH. , #57875 ) ;
#23433 = CARTESIAN_POINT ( 'NONE',  ( -45.48003679188781234, 379.8448106960472614, 7.220331889307936457 ) ) ;
#23434 = CARTESIAN_POINT ( 'NONE',  ( -84.57188724812456826, -46.57292530288317067, 186.4415227103431505 ) ) ;
#23436 = ADVANCED_FACE ( 'NONE', ( #54476 ), #33740, .F. ) ;
#23435 = ORIENTED_EDGE ( 'NONE', *, *, #4590, .T. ) ;
#23437 = CARTESIAN_POINT ( 'NONE',  ( 20.93475926104522600, 304.9197011768563925, -8.985567749925818859 ) ) ;
#23438 = CIRCLE ( 'NONE', #16561, 15.00000000000000000 ) ;
#23439 = CIRCLE ( 'NONE', #83686, 1.000000000000000888 ) ;
#23440 =( BOUNDED_SURFACE ( )  B_SPLINE_SURFACE ( 2, 3, ( 
 ( #56085, #9144, #42055, #49612 ),
 ( #90615, #99761, #34005, #89026 ),
 ( #15123, #7028, #39946, #105723 ) ),
 .UNSPECIFIED., .F., .F., .T. ) 
 B_SPLINE_SURFACE_WITH_KNOTS ( ( 3, 3 ),
 ( 4, 4 ),
 ( 0.000000000000000000, 1.000000000000000000 ),
 ( 0.04485000000000000792, 0.04800000000000000100 ),
 .UNSPECIFIED. ) 
 GEOMETRIC_REPRESENTATION_ITEM ( )  RATIONAL_B_SPLINE_SURFACE ( (
 ( 1.000000000000000000, 1.000000000000000000, 1.000000000000000000, 1.000000000000000000),
 ( 1.857142857142858317, 1.857142857142858317, 1.857142857142858317, 1.857142857142858317),
 ( 1.000000000000000000, 1.000000000000000000, 1.000000000000000000, 1.000000000000000000) ) ) 
 REPRESENTATION_ITEM ( '' )  SURFACE ( )  );
#23441 = VERTEX_POINT ( 'NONE', #93119 ) ;
#23442 = CARTESIAN_POINT ( 'NONE',  ( -7.344505440741523117, -12.44618927298704314, -3.175463080953006223 ) ) ;
#23443 = CARTESIAN_POINT ( 'NONE',  ( -5.796661515964135868E-15, 60.00000000000000000, 23.66666666666665719 ) ) ;
#23444 = CARTESIAN_POINT ( 'NONE',  ( -85.36974942761283103, -60.20515523833639548, -15.42856006348832310 ) ) ;
#23445 = B_SPLINE_CURVE_WITH_KNOTS ( 'NONE', 3,
 ( #46173, #71489, #79063, #80637 ),
 .UNSPECIFIED., .F., .F.,
 ( 4, 4 ),
 ( 0.000000000000000000, 0.002170046543158816663 ),
 .UNSPECIFIED. ) ;
#23446 = DIRECTION ( 'NONE',  ( -1.000000000000000000, -0.000000000000000000, -0.000000000000000000 ) ) ;
#23448 = CONICAL_SURFACE ( 'NONE', #95810, 8.000000000000000000, 1.047197551196600296 ) ;
#23447 = CARTESIAN_POINT ( 'NONE',  ( 42.91610780537346415, 434.7038292309374015, 17.44089711044166435 ) ) ;
#23449 = ORIENTED_EDGE ( 'NONE', *, *, #87411, .F. ) ;
#23450 = CARTESIAN_POINT ( 'NONE',  ( 6.289812543865803462, 5.581224740283310837, -3.991031161979335273 ) ) ;
#23451 = CARTESIAN_POINT ( 'NONE',  ( 10.19089998482013648, 16.03205744524296605, -10.16805419969074009 ) ) ;
#23452 = CARTESIAN_POINT ( 'NONE',  ( -22.22792991547117936, 27.72626095856944417, 32.73621634624660004 ) ) ;
#23453 = DIRECTION ( 'NONE',  ( -1.000000000000000000, -1.224606353822377258E-16, -0.000000000000000000 ) ) ;
#23454 = CARTESIAN_POINT ( 'NONE',  ( 88.18294634653494768, -59.99999999999992895, -24.85591942078231043 ) ) ;
#23455 = CARTESIAN_POINT ( 'NONE',  ( -78.23156018859863536, -42.96802624942629478, 138.8422877898725858 ) ) ;
#23456 = ORIENTED_EDGE ( 'NONE', *, *, #40686, .T. ) ;
#23457 = CARTESIAN_POINT ( 'NONE',  ( 34.17730524443083340, -14.21045842199440656, 38.95112099893761837 ) ) ;
#23458 = CARTESIAN_POINT ( 'NONE',  ( 63.56127108291158123, 6.975173280561618775E-15, 0.000000000000000000 ) ) ;
#23459 = CARTESIAN_POINT ( 'NONE',  ( 96.75771235523380653, -57.62241948994476104, 204.4691479018955818 ) ) ;
#23460 = CARTESIAN_POINT ( 'NONE',  ( 0.1061556211655340781, 6.421950209808278132, 1.876855952934451510 ) ) ;
#23461 = CARTESIAN_POINT ( 'NONE',  ( 31.00757884493366134, 309.4105030836295782, -8.486170584823613083 ) ) ;
#23462 = DIRECTION ( 'NONE',  ( 0.000000000000000000, 1.000000000000000000, 0.000000000000000000 ) ) ;
#23463 = ORIENTED_EDGE ( 'NONE', *, *, #78011, .F. ) ;
#23464 = CARTESIAN_POINT ( 'NONE',  ( 0.000000000000000000, -4.000000000000000000, 27.00000000000000000 ) ) ;
#23465 = CARTESIAN_POINT ( 'NONE',  ( -12.49999999999999822, 14.91296021360665769, -32.73279218218806363 ) ) ;
#23466 = DIRECTION ( 'NONE',  ( 1.000000000000000000, 0.000000000000000000, -3.673940397442057649E-17 ) ) ;
#23467 = CARTESIAN_POINT ( 'NONE',  ( -7.188101187500000044, -16.90625000204838813, -8.802885111219163269E-16 ) ) ;
#23468 = CARTESIAN_POINT ( 'NONE',  ( -0.3470952277635213634, -8.860649561028106191, -7.493596212620246888 ) ) ;
#23469 = VECTOR ( 'NONE', #83254, 999.9999999999998863 ) ;
#23470 = CARTESIAN_POINT ( 'NONE',  ( 9.380894568449079429, 82.98869366889060473, -3.467341429141157949 ) ) ;
#23471 = CARTESIAN_POINT ( 'NONE',  ( 0.7786400534603282741, 34.26594929026200020, 29.48136253453525768 ) ) ;
#23472 = ADVANCED_FACE ( 'NONE', ( #59704 ), #9674, .T. ) ;
#23473 = CARTESIAN_POINT ( 'NONE',  ( -7.500000000000000000, -0.7583608255792044783, -7.446489218764574147 ) ) ;
#23474 = DIRECTION ( 'NONE',  ( 1.000000000000000000, 1.224606353822377258E-16, 0.000000000000000000 ) ) ;
#23475 = ORIENTED_EDGE ( 'NONE', *, *, #14925, .T. ) ;
#23476 = CARTESIAN_POINT ( 'NONE',  ( -6.701893397842001221, 41.44328394191487774, -70.59544911652842814 ) ) ;
#23478 = CARTESIAN_POINT ( 'NONE',  ( 30.28165720518637372, -49.90556239820476492, 35.08629451775517794 ) ) ;
#23477 = CARTESIAN_POINT ( 'NONE',  ( -34.60361718403136422, -60.00000000000001421, 49.20626982406709971 ) ) ;
#23479 = CARTESIAN_POINT ( 'NONE',  ( -24.46377330976176623, 25.31537439212452867, 32.08272137679946212 ) ) ;
#23480 = EDGE_CURVE ( 'NONE', #48515, #9861, #50512, .T. ) ;
#23481 = ORIENTED_EDGE ( 'NONE', *, *, #74203, .F. ) ;
#23482 = UNCERTAINTY_MEASURE_WITH_UNIT (LENGTH_MEASURE( 1.000000000000000082E-05 ), #79981, 'distance_accuracy_value', 'NONE');
#23483 = VERTEX_POINT ( 'NONE', #26832 ) ;
#23485 = CARTESIAN_POINT ( 'NONE',  ( 38.85446894546156926, 460.8903912184132992, 2.218456751110441605 ) ) ;
#23484 = LINE ( 'NONE', #63410, #24496 ) ;
#23486 = CARTESIAN_POINT ( 'NONE',  ( -44.26701432268654202, 464.1304138491120170, 8.787925729972910105 ) ) ;
#23487 = FILL_AREA_STYLE ('',( #97333 ) ) ;
#23488 = ADVANCED_FACE ( 'NONE', ( #85030 ), #7989, .T. ) ;
#23489 = SURFACE_STYLE_USAGE ( .BOTH. , #103841 ) ;
#23490 = ORIENTED_EDGE ( 'NONE', *, *, #92450, .T. ) ;
#23491 = CARTESIAN_POINT ( 'NONE',  ( 7.700048951879978176, -60.00000000000000000, -42.50223864661403184 ) ) ;
#23492 = CARTESIAN_POINT ( 'NONE',  ( 22.43887874261524473, 26.07878403154861502, -30.97467766248137622 ) ) ;
#23493 = CARTESIAN_POINT ( 'NONE',  ( 3.400000000000000355, 0.000000000000000000, -8.000000000000000000 ) ) ;
#23494 = FACE_BOUND ( 'NONE', #20041, .T. ) ;
#23495 = PLANE ( 'NONE',  #82916 ) ;
#23496 = ORIENTED_EDGE ( 'NONE', *, *, #23188, .T. ) ;
#23497 = PRESENTATION_LAYER_ASSIGNMENT (  '', '', ( #69971 ) ) ;
#23498 = ORIENTED_EDGE ( 'NONE', *, *, #13378, .F. ) ;
#23499 = VERTEX_POINT ( 'NONE', #93660 ) ;
#23500 = CARTESIAN_POINT ( 'NONE',  ( 40.47243798843062734, 40.24842200370380851, -54.85959680779491521 ) ) ;
#23501 = CARTESIAN_POINT ( 'NONE',  ( -34.12291542400680555, 439.1280893533294147, 24.06048014402972512 ) ) ;
#23502 = CARTESIAN_POINT ( 'NONE',  ( 27.81431368193088005, 308.5680772048329459, 11.28096045510426748 ) ) ;
#23503 = VECTOR ( 'NONE', #49623, 999.9999999999998863 ) ;
#23504 = CARTESIAN_POINT ( 'NONE',  ( -43.55139821557366275, 368.5580705440897873, 13.69133376421734383 ) ) ;
#23505 = CARTESIAN_POINT ( 'NONE',  ( -3.578772014706478544, -68.26502216367026676, 13.09484892523241228 ) ) ;
#23506 = CARTESIAN_POINT ( 'NONE',  ( -46.00000000000000000, 487.9627413807708081, 0.8148295974594718105 ) ) ;
#23507 = DIRECTION ( 'NONE',  ( 0.000000000000000000, 0.000000000000000000, 1.000000000000000000 ) ) ;
#23508 = ORIENTED_EDGE ( 'NONE', *, *, #26321, .T. ) ;
#23509 = CARTESIAN_POINT ( 'NONE',  ( -9.203801892612585078, 43.65565976494217892, 14.80297099531582283 ) ) ;
#23510 = ORIENTED_EDGE ( 'NONE', *, *, #105556, .F. ) ;
#23511 = ADVANCED_FACE ( 'NONE', ( #67263, #58637, #19810, #2502, #52116 ), #2829, .T. ) ;
#23512 = DIRECTION ( 'NONE',  ( 0.000000000000000000, -1.000000000000000000, 0.000000000000000000 ) ) ;
#23513 = CARTESIAN_POINT ( 'NONE',  ( -12.13034742782428133, 49.99999999999999289, -93.82352941176471006 ) ) ;
#23514 = CARTESIAN_POINT ( 'NONE',  ( -41.29724588151401576, 485.7091420655430056, -4.558554568099082438 ) ) ;
#23515 = AXIS2_PLACEMENT_3D ( 'NONE', #17763, #75981, #35565 ) ;
#23516 = AXIS2_PLACEMENT_3D ( 'NONE', #24436, #82083, #49180 ) ;
#23517 = AXIS2_PLACEMENT_3D ( 'NONE', #29488, #38108, #87163 ) ;
#23518 = TOROIDAL_SURFACE ( 'NONE', #83744, 17.00000000000000000, 2.000000000000000000 ) ;
#23519 = AXIS2_PLACEMENT_3D ( 'NONE', #24120, #22529, #56428 ) ;
#23520 = DIRECTION ( 'NONE',  ( 0.000000000000000000, -1.000000000000000000, 0.000000000000000000 ) ) ;
#23522 = CARTESIAN_POINT ( 'NONE',  ( 69.47261160691843429, -60.32957453810588788, 112.5472032990401487 ) ) ;
#23521 = PRODUCT_DEFINITION_SHAPE ( 'NONE', 'NONE',  #106799 ) ;
#23523 = AXIS2_PLACEMENT_3D ( 'NONE', #38394, #45936, #54522 ) ;
#23524 = VERTEX_POINT ( 'NONE', #34916 ) ;
#23525 = CARTESIAN_POINT ( 'NONE',  ( 41.74148791219703725, 464.4898036148945266, 17.08834101213432533 ) ) ;
#23526 = AXIS2_PLACEMENT_3D ( 'NONE', #102461, #12371, #54404 ) ;
#23527 = CARTESIAN_POINT ( 'NONE',  ( 7.188101187499999156, -28.25000000204838813, 2.977408999572654924 ) ) ;
#23528 = EDGE_CURVE ( 'NONE', #23394, #95900, #33821, .T. ) ;
#23529 = B_SPLINE_CURVE_WITH_KNOTS ( 'NONE', 3,
 ( #79313, #5436, #15633, #42039, #48526, #25916, #9128, #74920, #8074, #24300, #24821, #33443, #99198, #81417, #57673, #57149, #40446, #91669, #7528, #40982, #90596, #16706, #90062, #73326 ),
 .UNSPECIFIED., .F., .F.,
 ( 4, 2, 2, 2, 2, 2, 2, 2, 2, 2, 2, 4 ),
 ( 2.213902055206457488E-15, 0.002700571958308535525, 0.004050857937461695667, 0.005401143916614856676, 0.006751429895768016817, 0.007426572885344616404, 0.008101715874921215990, 0.008776858864497815577, 0.009452001854074415163, 0.009789573348862707150, 0.01012714484365099567, 0.01080228783322758311 ),
 .UNSPECIFIED. ) ;
#23530 = ORIENTED_EDGE ( 'NONE', *, *, #609, .T. ) ;
#23531 = DIRECTION ( 'NONE',  ( 0.000000000000000000, -1.000000000000000000, 0.000000000000000000 ) ) ;
#23532 = CONICAL_SURFACE ( 'NONE', #101014, 4.000000000000007105, 0.9599310885968835860 ) ;
#23533 = CARTESIAN_POINT ( 'NONE',  ( 6.510002681445791417, 51.36730452995753637, -7.565658405795778307 ) ) ;
#23534 = CARTESIAN_POINT ( 'NONE',  ( 7.999999999999998224, -27.78125000409676915, 3.313708498984766493 ) ) ;
#23535 = FACE_OUTER_BOUND ( 'NONE', #74298, .T. ) ;
#23536 =( NAMED_UNIT ( * ) PLANE_ANGLE_UNIT ( ) SI_UNIT ( $, .RADIAN. ) );
#23537 = CARTESIAN_POINT ( 'NONE',  ( -10.03543110037283093, 7.449399144625810543, 5.000000000000000888 ) ) ;
#23538 = CARTESIAN_POINT ( 'NONE',  ( 7.999912353029504430, -6.000175293969080670, -0.2691822806795008405 ) ) ;
#23539 = CARTESIAN_POINT ( 'NONE',  ( 15.73174254031733987, 303.5560491714110753, 9.874135506282730290 ) ) ;
#23540 = ORIENTED_EDGE ( 'NONE', *, *, #38757, .F. ) ;
#23541 = CARTESIAN_POINT ( 'NONE',  ( 23.58349330513380337, -4.000000000000000000, 4.898587196589415787E-16 ) ) ;
#23542 = DIRECTION ( 'NONE',  ( 0.000000000000000000, 0.000000000000000000, 1.000000000000000000 ) ) ;
#23543 = CIRCLE ( 'NONE', #82090, 4.172000000000009479 ) ;
#23544 = CARTESIAN_POINT ( 'NONE',  ( 15.38671495384722121, -59.99999999999999289, 39.81262336454445006 ) ) ;
#23545 = CARTESIAN_POINT ( 'NONE',  ( -97.65307766490704466, -30.00000000000000000, 190.8028841120875256 ) ) ;
#23546 = ADVANCED_FACE ( 'NONE', ( #67782 ), #25276, .F. ) ;
#23547 = CARTESIAN_POINT ( 'NONE',  ( -39.42128877452295654, 485.2094636432215111, -4.368416090031590926 ) ) ;
#23548 = CARTESIAN_POINT ( 'NONE',  ( 38.78005064836850124, -57.69447179130985859, 53.76168839330274807 ) ) ;
#23550 = CARTESIAN_POINT ( 'NONE',  ( 43.51084452654482249, 465.2903130129674878, 9.421687747984014649 ) ) ;
#23549 = DIRECTION ( 'NONE',  ( -0.000000000000000000, -0.000000000000000000, -1.000000000000000000 ) ) ;
#23551 = EDGE_CURVE ( 'NONE', #21651, #77582, #92369, .T. ) ;
#23552 = CARTESIAN_POINT ( 'NONE',  ( 15.68733860615400033, -24.30949475465576626, -38.52672339115742517 ) ) ;
#23553 = CARTESIAN_POINT ( 'NONE',  ( -10.00000000000000000, 15.00000000000000000, 3.082707893549380351 ) ) ;
#23554 = CARTESIAN_POINT ( 'NONE',  ( -12.56390471583231516, -60.00000000000002132, 39.70168213610190833 ) ) ;
#23555 = CARTESIAN_POINT ( 'NONE',  ( 11.44639037572927620, 14.62121991795728349, 9.874825666010542236 ) ) ;
#23556 = TOROIDAL_SURFACE ( 'NONE', #6263, 7.999999999999998224, 2.000000000000000000 ) ;
#23557 = CARTESIAN_POINT ( 'NONE',  ( -87.19385550499211490, -31.68974481596827175, 187.9067576323665776 ) ) ;
#23558 = ADVANCED_FACE ( 'NONE', ( #91536 ), #69980, .T. ) ;
#23559 = ORIENTED_EDGE ( 'NONE', *, *, #72357, .T. ) ;
#23560 = CARTESIAN_POINT ( 'NONE',  ( 17.50000000000003908, 51.99999999999984368, 59.82664205500665844 ) ) ;
#23561 = FACE_OUTER_BOUND ( 'NONE', #63998, .T. ) ;
#23562 = CARTESIAN_POINT ( 'NONE',  ( -14.39691347112102093, -29.03163114769574449, 28.84164502424407672 ) ) ;
#23563 = LINE ( 'NONE', #56407, #85901 ) ;
#23565 =( NAMED_UNIT ( * ) SI_UNIT ( $, .STERADIAN. ) SOLID_ANGLE_UNIT ( ) );
#23564 = CARTESIAN_POINT ( 'NONE',  ( -102.6649796019329699, -60.00000000000002132, 193.3001960811608626 ) ) ;
#23566 = ORIENTED_EDGE ( 'NONE', *, *, #80750, .F. ) ;
#23567 = CARTESIAN_POINT ( 'NONE',  ( 72.11682663846713126, -1.232595164407830946E-29, 4.000000000000007105 ) ) ;
#23568 = CARTESIAN_POINT ( 'NONE',  ( -5.076160773006212601, -4.320849473519612793, -17.10810059244015946 ) ) ;
#23569 = DIRECTION ( 'NONE',  ( 0.000000000000000000, -1.000000000000000000, 0.000000000000000000 ) ) ;
#23570 = CIRCLE ( 'NONE', #28747, 5.000000000000001776 ) ;
#23571 = DIRECTION ( 'NONE',  ( 0.000000000000000000, 0.000000000000000000, 1.000000000000000000 ) ) ;
#23572 = CARTESIAN_POINT ( 'NONE',  ( -7.413471587080152858, -82.35647840831671829, -3.013058070223548324 ) ) ;
#23573 = CARTESIAN_POINT ( 'NONE',  ( 72.36529781780690485, -59.99999999999998579, 157.0781579372900580 ) ) ;
#23574 = CARTESIAN_POINT ( 'NONE',  ( -45.48126212248870814, 413.7349014071057240, 8.309231847991947362 ) ) ;
#23575 = ORIENTED_EDGE ( 'NONE', *, *, #72818, .T. ) ;
#23576 = CARTESIAN_POINT ( 'NONE',  ( -7.460363399255495409, -29.99999999999998934, 2.207551751280008467 ) ) ;
#23577 = COLOUR_RGB ( '', 0.31764706, 0.68627451, 0.89019608) ;
#23578 = CARTESIAN_POINT ( 'NONE',  ( 0.000000000000000000, 0.000000000000000000, 1.734723475976807094E-15 ) ) ;
#23579 = AXIS2_PLACEMENT_3D ( 'NONE', #8516, #41420, #99109 ) ;
#23581 = DIRECTION ( 'NONE',  ( -1.000000000000000000, -0.000000000000000000, -0.000000000000000000 ) ) ;
#23580 = CARTESIAN_POINT ( 'NONE',  ( 24.48575568784926304, -14.21045842199439946, 35.52093559979998361 ) ) ;
#23582 = CARTESIAN_POINT ( 'NONE',  ( 4.086350204929699359, 138.2877876407195004, -5.000000000000000888 ) ) ;
#23583 =( NAMED_UNIT ( * ) PLANE_ANGLE_UNIT ( ) SI_UNIT ( $, .RADIAN. ) );
#23584 = ORIENTED_EDGE ( 'NONE', *, *, #74108, .T. ) ;
#23585 = AXIS2_PLACEMENT_3D ( 'NONE', #26785, #67738, #101698 ) ;
#23586 = CARTESIAN_POINT ( 'NONE',  ( -26.43366826923012169, 308.0207211451966032, 10.90581097607394057 ) ) ;
#23587 = EDGE_LOOP ( 'NONE', ( #17328, #87800, #87347, #83626, #76462 ) ) ;
#23588 = CARTESIAN_POINT ( 'NONE',  ( 3.487646406148667833, 15.95332971149351842, 9.373884331924859481 ) ) ;
#23589 = DIRECTION ( 'NONE',  ( 0.000000000000000000, -1.000000000000000000, 0.000000000000000000 ) ) ;
#23590 = SURFACE_STYLE_FILL_AREA ( #30084 ) ;
#23591 = VERTEX_POINT ( 'NONE', #27371 ) ;
#23592 = EDGE_CURVE ( 'NONE', #57426, #105955, #17650, .T. ) ;
#23593 = CARTESIAN_POINT ( 'NONE',  ( -65.26738680890619548, 48.00000000000000000, 0.8120011905346659065 ) ) ;
#23594 = CARTESIAN_POINT ( 'NONE',  ( -113.7086509678886443, -59.99999999998047429, 155.4592733101652584 ) ) ;
#23595 = CARTESIAN_POINT ( 'NONE',  ( 6.222802839579465228, -4.089658325571345898, -6.500000000000002665 ) ) ;
#23596 = CARTESIAN_POINT ( 'NONE',  ( 46.21931631244920169, -60.00000000000000000, 63.08554439955615578 ) ) ;
#23597 = PLANE ( 'NONE',  #59758 ) ;
#23598 = DIRECTION ( 'NONE',  ( -0.5735764363510510444, -0.8191520442889883569, 0.000000000000000000 ) ) ;
#23600 = CARTESIAN_POINT ( 'NONE',  ( 15.36438022688010463, -22.06846381147260772, 27.72742713275420101 ) ) ;
#23599 = CARTESIAN_POINT ( 'NONE',  ( -114.5103415054848170, -60.00000000000004263, 177.0886483751272351 ) ) ;
#23601 = CARTESIAN_POINT ( 'NONE',  ( 90.58584440353838829, -38.00000000000000000, 81.86263311294858624 ) ) ;
#23603 = EDGE_CURVE ( 'NONE', #101293, #65538, #82044, .T. ) ;
#23602 = CARTESIAN_POINT ( 'NONE',  ( 1.251548456357452377, 53.70817747035267331, -9.313240114490840327 ) ) ;
#23604 = CARTESIAN_POINT ( 'NONE',  ( -44.99960878686916743, -56.80572573438033857, 48.30738373556244625 ) ) ;
#23605 = CARTESIAN_POINT ( 'NONE',  ( 4.898587196589412829E-16, -16.62499999999999289, -8.000000000000000000 ) ) ;
#23606 = ORIENTED_EDGE ( 'NONE', *, *, #69941, .T. ) ;
#23607 = CARTESIAN_POINT ( 'NONE',  ( 16.13488272710862859, 21.13099985709055062, -3.419103882760960111 ) ) ;
#23608 = CARTESIAN_POINT ( 'NONE',  ( -2.720100412697608494, -69.18718729000897838, 12.97654704113952384 ) ) ;
#23609 = CARTESIAN_POINT ( 'NONE',  ( -5.000000000000000000, -32.50000000000000000, 13.00000000000000178 ) ) ;
#23610 = CARTESIAN_POINT ( 'NONE',  ( 4.478476647430160718, -9.726479208179556579, 3.992942460563205120 ) ) ;
#23611 = CARTESIAN_POINT ( 'NONE',  ( 26.97491686565329161, 307.4599153070161606, -9.420584459367196573 ) ) ;
#23613 = ORIENTED_EDGE ( 'NONE', *, *, #5928, .F. ) ;
#23612 = AXIS2_PLACEMENT_3D ( 'NONE', #70922, #21345, #96798 ) ;
#23614 = CARTESIAN_POINT ( 'NONE',  ( 4.642888266381832274, -47.65716784818645380, 102.5319024079573751 ) ) ;
#23615 = VERTEX_POINT ( 'NONE', #13244 ) ;
#23616 = CARTESIAN_POINT ( 'NONE',  ( 99.42104296369386418, -30.00000000004165557, 199.3229471623391476 ) ) ;
#23617 = DIRECTION ( 'NONE',  ( 0.000000000000000000, 1.000000000000000000, 0.000000000000000000 ) ) ;
#23618 = CARTESIAN_POINT ( 'NONE',  ( 6.359250229816447053, 41.88719966772354297, -59.22188798823055578 ) ) ;
#23619 = FACE_OUTER_BOUND ( 'NONE', #77432, .T. ) ;
#23620 = CARTESIAN_POINT ( 'NONE',  ( 90.42852211739197799, -30.00000000000000000, 90.99945873017442466 ) ) ;
#23621 = CARTESIAN_POINT ( 'NONE',  ( 6.928203230275507885, 105.0000000000000000, -4.000000000000001776 ) ) ;
#23622 = ORIENTED_EDGE ( 'NONE', *, *, #92848, .F. ) ;
#23623 = EDGE_CURVE ( 'NONE', #102776, #214, #45893, .T. ) ;
#23624 = ORIENTED_EDGE ( 'NONE', *, *, #24742, .T. ) ;
#23625 = ORIENTED_EDGE ( 'NONE', *, *, #10486, .F. ) ;
#23626 = CARTESIAN_POINT ( 'NONE',  ( 85.59800593614014019, -4.999999999999980460, 0.000000000000000000 ) ) ;
#23627 = CARTESIAN_POINT ( 'NONE',  ( 45.94900261086841198, -5.000000000000000000, 6.123233995736768255E-16 ) ) ;
#23628 = EDGE_LOOP ( 'NONE', ( #13888, #69538, #68031, #34109 ) ) ;
#23629 = VERTEX_POINT ( 'NONE', #62889 ) ;
#23630 = CARTESIAN_POINT ( 'NONE',  ( 21.08349330513380337, -4.000000000000000000, 4.898587196589415787E-16 ) ) ;
#23631 = CARTESIAN_POINT ( 'NONE',  ( 77.65721028447464391, -38.53209962432212876, 187.0521431165007584 ) ) ;
#23632 = CARTESIAN_POINT ( 'NONE',  ( 24.83349330513380337, -4.000000000000000888, 4.898587196589416773E-16 ) ) ;
#23633 = CARTESIAN_POINT ( 'NONE',  ( 72.13138110526622881, -38.00000000000000711, 108.4011625346426797 ) ) ;
#23634 = CARTESIAN_POINT ( 'NONE',  ( 37.31779904297146544, 312.7144339071508057, 14.24890093005832625 ) ) ;
#23635 = DIRECTION ( 'NONE',  ( -1.000000000000000000, -1.224606353822377258E-16, -0.000000000000000000 ) ) ;
#23636 = CIRCLE ( 'NONE', #58094, 15.00000000000001421 ) ;
#23637 = CARTESIAN_POINT ( 'NONE',  ( 0.4033376246892511618, -4.059728990630809164, -5.968343123267135120 ) ) ;
#23638 = AXIS2_PLACEMENT_3D ( 'NONE', #78935, #69794, #55175 ) ;
#23639 = LINE ( 'NONE', #19309, #7824 ) ;
#23640 = CARTESIAN_POINT ( 'NONE',  ( -4.642888266381816287, -47.65716784818648222, 102.5319024079587393 ) ) ;
#23641 = SURFACE_STYLE_USAGE ( .BOTH. , #81300 ) ;
#23642 = DIRECTION ( 'NONE',  ( -1.000000000000000000, -1.224606353822377258E-16, -0.000000000000000000 ) ) ;
#23643 = VERTEX_POINT ( 'NONE', #87693 ) ;
#23644 = CARTESIAN_POINT ( 'NONE',  ( -35.34812152312258604, 364.3443896332000804, 3.939155806205292265 ) ) ;
#23646 = CARTESIAN_POINT ( 'NONE',  ( -32.64021143431507710, 300.1493399910716562, 3.126861728487528413 ) ) ;
#23645 =( LENGTH_UNIT ( ) NAMED_UNIT ( * ) SI_UNIT ( .MILLI., .METRE. ) );
#23647 = CARTESIAN_POINT ( 'NONE',  ( 79.82022815836235452, 1.016364837396684119E-14, 0.000000000000000000 ) ) ;
#23648 = UNCERTAINTY_MEASURE_WITH_UNIT (LENGTH_MEASURE( 1.000000000000000082E-05 ), #10926, 'distance_accuracy_value', 'NONE');
#23649 = DIRECTION ( 'NONE',  ( 0.000000000000000000, 1.000000000000000000, 0.000000000000000000 ) ) ;
#23650 = CARTESIAN_POINT ( 'NONE',  ( -1.469576158976823947E-15, -12.87499999999999467, 8.000000000000000000 ) ) ;
#23651 = AXIS2_PLACEMENT_3D ( 'NONE', #106158, #50063, #16640 ) ;
#23653 = DIRECTION ( 'NONE',  ( 0.000000000000000000, 0.000000000000000000, 1.000000000000000000 ) ) ;
#23652 = CIRCLE ( 'NONE', #90841, 4.000000000000001776 ) ;
#23654 =( GEOMETRIC_REPRESENTATION_CONTEXT ( 3 ) GLOBAL_UNCERTAINTY_ASSIGNED_CONTEXT ( ( #31055 ) ) GLOBAL_UNIT_ASSIGNED_CONTEXT ( ( #3067, #14189, #84529 ) ) REPRESENTATION_CONTEXT ( 'NONE', 'WORKASPACE' ) );
#23655 = CIRCLE ( 'NONE', #6364, 1.000000000000000000 ) ;
#23656 = MECHANICAL_DESIGN_GEOMETRIC_PRESENTATION_REPRESENTATION (  '', ( #32274 ), #54636 ) ;
#23657 = FACE_BOUND ( 'NONE', #52533, .T. ) ;
#23658 = AXIS2_PLACEMENT_3D ( 'NONE', #87786, #28510, #20448 ) ;
#23659 = ORIENTED_EDGE ( 'NONE', *, *, #96773, .T. ) ;
#23660 = CARTESIAN_POINT ( 'NONE',  ( 83.77195690154300678, -57.39043513791891371, 190.2506195938281621 ) ) ;
#23661 = LINE ( 'NONE', #41405, #48075 ) ;
#23662 = CARTESIAN_POINT ( 'NONE',  ( -4.556959930218859256, 143.1971678044430405, 5.000000000000004441 ) ) ;
#23663 = ORIENTED_EDGE ( 'NONE', *, *, #86406, .F. ) ;
#23664 = CARTESIAN_POINT ( 'NONE',  ( 93.84281965440075624, -57.67495174030868554, 10.52530039810905116 ) ) ;
#23665 = DIRECTION ( 'NONE',  ( -1.000000000000000000, 0.000000000000000000, 0.000000000000000000 ) ) ;
#23666 = SURFACE_SIDE_STYLE ('',( #72193 ) ) ;
#23667 = CONICAL_SURFACE ( 'NONE', #6377, 4.000000000000000000, 0.9599310885968912466 ) ;
#23668 = CARTESIAN_POINT ( 'NONE',  ( 11.36650669486618881, 0.000000000000000000, 4.000000000000000888 ) ) ;
#23669 = AXIS2_PLACEMENT_3D ( 'NONE', #55909, #64580, #89388 ) ;
#23670 = EDGE_CURVE ( 'NONE', #5773, #37427, #44197, .T. ) ;
#23671 = CARTESIAN_POINT ( 'NONE',  ( -82.86493196561585250, -38.00000000000003553, 166.1273331999570928 ) ) ;
#23672 = CARTESIAN_POINT ( 'NONE',  ( 5.219866590719942856, -5.000000000000000000, -8.922269033013279227 ) ) ;
#23673 = CARTESIAN_POINT ( 'NONE',  ( -5.833333333333328596, -46.00000000000000000, 103.8776713793258608 ) ) ;
#23675 = CARTESIAN_POINT ( 'NONE',  ( -13.27937243830230152, 3.845154223814204020, 6.891420024422192370 ) ) ;
#23674 = DIRECTION ( 'NONE',  ( 0.000000000000000000, -1.000000000000000000, 0.000000000000000000 ) ) ;
#23676 = ADVANCED_FACE ( 'NONE', ( #79058 ), #86118, .F. ) ;
#23677 = VERTEX_POINT ( 'NONE', #37582 ) ;
#23678 = AXIS2_PLACEMENT_3D ( 'NONE', #75183, #19140, #1282 ) ;
#23679 = CARTESIAN_POINT ( 'NONE',  ( 42.57704743493903266, 486.1612337113410263, 7.852296464539683107 ) ) ;
#23680 = FACE_OUTER_BOUND ( 'NONE', #85633, .T. ) ;
#23681 = CARTESIAN_POINT ( 'NONE',  ( -28.18085356279351217, 36.45119673881288236, -8.149377185781427002 ) ) ;
#23682 = LINE ( 'NONE', #88923, #45769 ) ;
#23683 = DIRECTION ( 'NONE',  ( 0.000000000000000000, 0.000000000000000000, 1.000000000000000000 ) ) ;
#23684 = CARTESIAN_POINT ( 'NONE',  ( 65.65969153816354265, -29.79516960803964665, -22.78676046141628575 ) ) ;
#23685 = PRESENTATION_LAYER_ASSIGNMENT (  '', '', ( #66702 ) ) ;
#23686 = EDGE_CURVE ( 'NONE', #22931, #40289, #57959, .T. ) ;
#23687 = VERTEX_POINT ( 'NONE', #86648 ) ;
#23688 = FACE_OUTER_BOUND ( 'NONE', #91978, .T. ) ;
#23689 = DIRECTION ( 'NONE',  ( -0.000000000000000000, -1.000000000000000000, -0.000000000000000000 ) ) ;
#23690 = AXIS2_PLACEMENT_3D ( 'NONE', #96444, #22580, #79180 ) ;
#23691 = CARTESIAN_POINT ( 'NONE',  ( 5.192560085536415571, -62.35694557368758950, 3.013051918867554413 ) ) ;
#23693 = CARTESIAN_POINT ( 'NONE',  ( -45.16882421246708645, -60.22825351688758388, -33.02234666222834392 ) ) ;
#23692 = DIRECTION ( 'NONE',  ( -1.000000000000000000, -1.224606353822377258E-16, -0.000000000000000000 ) ) ;
#23694 = ORIENTED_EDGE ( 'NONE', *, *, #11330, .T. ) ;
#23695 = ORIENTED_EDGE ( 'NONE', *, *, #65236, .F. ) ;
#23696 = AXIS2_PLACEMENT_3D ( 'NONE', #50235, #84737, #99847 ) ;
#23697 = DIRECTION ( 'NONE',  ( -1.000000000000000000, 0.000000000000000000, 0.000000000000000000 ) ) ;
#23698 = CARTESIAN_POINT ( 'NONE',  ( -92.64811155113156360, -59.99999999999998579, -3.658885834359205003 ) ) ;
#23699 = ORIENTED_EDGE ( 'NONE', *, *, #26014, .T. ) ;
#23700 = CARTESIAN_POINT ( 'NONE',  ( 0.000000000000000000, 0.000000000000000000, 0.000000000000000000 ) ) ;
#23701 = SURFACE_STYLE_USAGE ( .BOTH. , #54419 ) ;
#23702 = CARTESIAN_POINT ( 'NONE',  ( 95.34251263761402129, -37.71227104075504144, 193.0165489376654477 ) ) ;
#23704 = CARTESIAN_POINT ( 'NONE',  ( -17.64253364725059825, 45.32498240469068662, 6.177274125185036269 ) ) ;
#23703 = FILL_AREA_STYLE ('',( #64156 ) ) ;
#23705 = CARTESIAN_POINT ( 'NONE',  ( -83.46189083830699929, -29.07720453051282661, 157.7181293371499464 ) ) ;
#23706 =( GEOMETRIC_REPRESENTATION_CONTEXT ( 3 ) GLOBAL_UNCERTAINTY_ASSIGNED_CONTEXT ( ( #59125 ) ) GLOBAL_UNIT_ASSIGNED_CONTEXT ( ( #25521, #50792, #51336 ) ) REPRESENTATION_CONTEXT ( 'NONE', 'WORKASPACE' ) );
#23707 = ORIENTED_EDGE ( 'NONE', *, *, #90654, .F. ) ;
#23708 = ORIENTED_EDGE ( 'NONE', *, *, #103537, .F. ) ;
#23709 = ORIENTED_EDGE ( 'NONE', *, *, #25142, .T. ) ;
#23710 = CARTESIAN_POINT ( 'NONE',  ( 31.35087791607053020, 439.7411499371610830, 22.35627675531413061 ) ) ;
#23711 = CARTESIAN_POINT ( 'NONE',  ( -5.000000000000000000, -14.98862091075374003, 12.50620160667438263 ) ) ;
#23712 = SURFACE_STYLE_USAGE ( .BOTH. , #56024 ) ;
#23713 = ORIENTED_EDGE ( 'NONE', *, *, #79485, .F. ) ;
#23714 = EDGE_CURVE ( 'NONE', #39800, #52601, #104382, .T. ) ;
#23715 = LINE ( 'NONE', #65744, #91004 ) ;
#23716 = CARTESIAN_POINT ( 'NONE',  ( -122.4708123290697159, 1.499999999999992450, -61.23540616453487218 ) ) ;
#23717 = PRESENTATION_STYLE_ASSIGNMENT (( #97557 ) ) ;
#23718 = CARTESIAN_POINT ( 'NONE',  ( -101.2734545671114290, -57.63007487344309254, 203.5435050992661843 ) ) ;
#23719 = CARTESIAN_POINT ( 'NONE',  ( 2.103764093714755923, -49.85092038520011215, 102.1576470924498210 ) ) ;
#23720 = DIRECTION ( 'NONE',  ( 1.000000000000000000, 0.000000000000000000, 0.000000000000000000 ) ) ;
#23721 = AXIS2_PLACEMENT_3D ( 'NONE', #35394, #84447, #68263 ) ;
#23722 = DIRECTION ( 'NONE',  ( 0.5735764363510490460, 0.8191520442889896891, 0.000000000000000000 ) ) ;
#23723 = AXIS2_PLACEMENT_3D ( 'NONE', #48480, #72754, #79798 ) ;
#23724 = CARTESIAN_POINT ( 'NONE',  ( 1.250028549308467740, 27.68639675375847986, -39.65926092309576489 ) ) ;
#23725 = CARTESIAN_POINT ( 'NONE',  ( -40.75117554026711275, -14.21045842199432663, -34.22202116092960011 ) ) ;
#23726 = EDGE_CURVE ( 'NONE', #39589, #60803, #39042, .T. ) ;
#23728 = EDGE_CURVE ( 'NONE', #45623, #101469, #70445, .T. ) ;
#23727 = DIRECTION ( 'NONE',  ( 1.000000000000000000, 0.000000000000000000, 0.000000000000000000 ) ) ;
#23729 = CARTESIAN_POINT ( 'NONE',  ( -52.52702786332168472, -49.90965349917357230, 59.15625794695527162 ) ) ;
#23730 = CARTESIAN_POINT ( 'NONE',  ( 5.656854249492378806, -27.68749999999999645, 5.656854249492381470 ) ) ;
#23731 = VECTOR ( 'NONE', #52988, 1000.000000000000000 ) ;
#23733 = ORIENTED_EDGE ( 'NONE', *, *, #79119, .T. ) ;
#23732 = AXIS2_PLACEMENT_3D ( 'NONE', #5101, #87090, #28893 ) ;
#23734 = AXIS2_PLACEMENT_3D ( 'NONE', #13446, #5884, #13974 ) ;
#23735 = CARTESIAN_POINT ( 'NONE',  ( -98.52404613076176076, -37.74647085490894938, 192.2268697399963742 ) ) ;
#23736 = CARTESIAN_POINT ( 'NONE',  ( -31.80704930621334370, 485.2748291366696662, 5.788617803630615732 ) ) ;
#23737 = ORIENTED_EDGE ( 'NONE', *, *, #26486, .T. ) ;
#23738 = LINE ( 'NONE', #73844, #20180 ) ;
#23739 = CARTESIAN_POINT ( 'NONE',  ( 91.44830385819240348, -38.39066018178733231, -8.169144241885213376 ) ) ;
#23740 = LINE ( 'NONE', #58196, #101830 ) ;
#23741 = CARTESIAN_POINT ( 'NONE',  ( -5.082755093536325042, -11.46875000204838635, -5.082755093536325930 ) ) ;
#23742 = CARTESIAN_POINT ( 'NONE',  ( -15.66789899020478849, 294.5588784006489504, 1.874736099250551957 ) ) ;
#23743 = DIRECTION ( 'NONE',  ( 0.000000000000000000, 0.000000000000000000, 1.000000000000000000 ) ) ;
#23745 = CARTESIAN_POINT ( 'NONE',  ( 84.03603373241958252, -30.00000000000000000, 161.3276072815756663 ) ) ;
#23744 = UNCERTAINTY_MEASURE_WITH_UNIT (LENGTH_MEASURE( 1.000000000000000082E-05 ), #26669, 'distance_accuracy_value', 'NONE');
#23746 = AXIS2_PLACEMENT_3D ( 'NONE', #50489, #85008, #83402 ) ;
#23747 = EDGE_CURVE ( 'NONE', #84498, #45468, #104459, .T. ) ;
#23748 = CARTESIAN_POINT ( 'NONE',  ( 33.00000000000000000, 450.0000000000002274, 13.20242257375370976 ) ) ;
#23749 = CARTESIAN_POINT ( 'NONE',  ( 35.46673095356709382, 491.6344107835774366, 12.45081314981930909 ) ) ;
#23750 = CARTESIAN_POINT ( 'NONE',  ( -34.89132489497384171, 463.6439613888530289, 18.89948583901070123 ) ) ;
#23751 = ADVANCED_FACE ( 'NONE', ( #69910 ), #14894, .T. ) ;
#23752 = CIRCLE ( 'NONE', #15087, 7.500000000001509015 ) ;
#23753 = ORIENTED_EDGE ( 'NONE', *, *, #67936, .T. ) ;
#23754 = ORIENTED_EDGE ( 'NONE', *, *, #5978, .T. ) ;
#23755 = CARTESIAN_POINT ( 'NONE',  ( 49.98712176156696785, -49.90156039724934800, 54.21681932135436455 ) ) ;
#23756 = CARTESIAN_POINT ( 'NONE',  ( -2.289807569700440748, 298.7146840682374318, -10.00340823979563609 ) ) ;
#23757 = CARTESIAN_POINT ( 'NONE',  ( 8.876037421300598140, 51.71979065213020732, 1.561582822885281718 ) ) ;
#23758 = ORIENTED_EDGE ( 'NONE', *, *, #99103, .F. ) ;
#23759 = CARTESIAN_POINT ( 'NONE',  ( -90.85419583802016064, -38.34570451894640541, 4.396493097181871867 ) ) ;
#23760 =( GEOMETRIC_REPRESENTATION_CONTEXT ( 3 ) GLOBAL_UNCERTAINTY_ASSIGNED_CONTEXT ( ( #894 ) ) GLOBAL_UNIT_ASSIGNED_CONTEXT ( ( #12427, #76637, #86363 ) ) REPRESENTATION_CONTEXT ( 'NONE', 'WORKASPACE' ) );
#23761 = ORIENTED_EDGE ( 'NONE', *, *, #64252, .F. ) ;
#23762 = CARTESIAN_POINT ( 'NONE',  ( 5.799999999999999822, 0.000000000000000000, 0.000000000000000000 ) ) ;
#23763 = CARTESIAN_POINT ( 'NONE',  ( 90.86170511367741653, -38.35175402733357686, 20.64558181097320144 ) ) ;
#23764 = CARTESIAN_POINT ( 'NONE',  ( 10.83745700209015261, 18.77853125270598156, -9.157543372961134409 ) ) ;
#23765 = CARTESIAN_POINT ( 'NONE',  ( 30.00000000000000711, 464.1062179653382032, 10.70584622103039329 ) ) ;
#23766 = CARTESIAN_POINT ( 'NONE',  ( 100.0259651621010306, -60.15125716094357955, 115.3354766105753555 ) ) ;
#23767 = PRESENTATION_STYLE_ASSIGNMENT (( #14555 ) ) ;
#23768 = CARTESIAN_POINT ( 'NONE',  ( 22.11477862515263126, 27.78277355752726763, 32.62539941293114509 ) ) ;
#23769 = CARTESIAN_POINT ( 'NONE',  ( -31.35792916284521681, 312.3233365065780163, -8.007654514793925316 ) ) ;
#23770 = EDGE_CURVE ( 'NONE', #62199, #56292, #24568, .T. ) ;
#23771 = AXIS2_PLACEMENT_3D ( 'NONE', #59014, #18027, #33688 ) ;
#23772 = CARTESIAN_POINT ( 'NONE',  ( 77.86138069022020147, -60.00000000000000000, 192.5414314693734070 ) ) ;
#23773 = FACE_OUTER_BOUND ( 'NONE', #17023, .T. ) ;
#23775 = VERTEX_POINT ( 'NONE', #73597 ) ;
#23774 =( BOUNDED_SURFACE ( )  B_SPLINE_SURFACE ( 3, 2, ( 
 ( #14959, #47853, #89408 ),
 ( #15503, #67781, #52115 ),
 ( #27905, #60771, #93659 ),
 ( #60250, #101213, #19290 ),
 ( #100670, #1964, #50511 ),
 ( #18183, #59168, #66719 ),
 ( #93118, #85029, #68319 ),
 ( #76386, #11652, #59702 ) ),
 .UNSPECIFIED., .F., .F., .T. ) 
 B_SPLINE_SURFACE_WITH_KNOTS ( ( 4, 2, 2, 4 ),
 ( 3, 3 ),
 ( 0.000000000000000000, 0.002244734355339991771, 0.003367101533009987657, 0.004489468710679983543 ),
 ( 0.000000000000000000, 1.000000000000000000 ),
 .UNSPECIFIED. ) 
 GEOMETRIC_REPRESENTATION_ITEM ( )  RATIONAL_B_SPLINE_SURFACE ( (
 ( 1.000000000000000000, 0.8138888783288348305, 1.000000000000000000),
 ( 1.000000000000000000, 0.8201127045460194775, 1.000000000000000000),
 ( 1.000000000000000000, 0.8211215022295521582, 1.000000000000000000),
 ( 1.000000000000000000, 0.8168533336244402365, 1.000000000000000000),
 ( 1.000000000000000000, 0.8144062529141679052, 1.000000000000000000),
 ( 1.000000000000000000, 0.8072737967831881134, 1.000000000000000000),
 ( 1.000000000000000000, 0.8026171117791235377, 1.000000000000000000),
 ( 1.000000000000000000, 0.7964893136846482591, 1.000000000000000000) ) ) 
 REPRESENTATION_ITEM ( '' )  SURFACE ( )  );
#23776 = CARTESIAN_POINT ( 'NONE',  ( 55.22303882701753253, -49.90717449039305365, 65.08233922066710875 ) ) ;
#23777 = CARTESIAN_POINT ( 'NONE',  ( -29.95916737693520915, 297.7500670450060625, -1.363754256076671334 ) ) ;
#23778 = LINE ( 'NONE', #89017, #66898 ) ;
#23779 = CARTESIAN_POINT ( 'NONE',  ( 27.99999999999999645, 0.000000000000000000, 0.000000000000000000 ) ) ;
#23780 = VERTEX_POINT ( 'NONE', #14835 ) ;
#23782 = CARTESIAN_POINT ( 'NONE',  ( -14.78158836401471099, 22.78085926477313450, 2.483703530589361552 ) ) ;
#23781 = CARTESIAN_POINT ( 'NONE',  ( -47.43396820366045574, -30.00000000002712497, 59.40601916810901173 ) ) ;
#23783 = AXIS2_PLACEMENT_3D ( 'NONE', #5614, #42757, #9309 ) ;
#23784 = CARTESIAN_POINT ( 'NONE',  ( 1.047197551196597631, -3.000000000000000888, 8.000000000000001776 ) ) ;
#23785 = CARTESIAN_POINT ( 'NONE',  ( 23.05647306551357190, 305.6773795875058681, 9.116627575657666682 ) ) ;
#23786 = CARTESIAN_POINT ( 'NONE',  ( 89.99999999999997158, -52.00000000000000000, 194.0238439516549818 ) ) ;
#23787 = CARTESIAN_POINT ( 'NONE',  ( -5.082755093536326818, -9.593750002048384573, 5.082755093536325042 ) ) ;
#23788 = AXIS2_PLACEMENT_3D ( 'NONE', #83948, #66167, #34907 ) ;
#23789 = CARTESIAN_POINT ( 'NONE',  ( -33.50220463782434166, 465.4655183566870846, 16.55182854116007718 ) ) ;
#23790 = CONICAL_SURFACE ( 'NONE', #3123, 13.50000000000000178, 1.047197551196596077 ) ;
#23791 = ORIENTED_EDGE ( 'NONE', *, *, #51268, .F. ) ;
#23792 = CARTESIAN_POINT ( 'NONE',  ( 81.66341672991298140, -57.04221095040819023, 183.2393683767488142 ) ) ;
#23793 = CARTESIAN_POINT ( 'NONE',  ( 5.232798140227933104, -48.02337292624942222, 104.1190344879413914 ) ) ;
#23794 = CARTESIAN_POINT ( 'NONE',  ( 37.40781652519264355, 27.65894600026285843, 13.45617127781008193 ) ) ;
#23795 = ORIENTED_EDGE ( 'NONE', *, *, #101977, .T. ) ;
#23796 = CARTESIAN_POINT ( 'NONE',  ( 33.58349330513379982, 1.593028355512270567E-15, 0.000000000000000000 ) ) ;
#23797 = CARTESIAN_POINT ( 'NONE',  ( 7.499944090891561999, -3.043005460614601532, -20.23003913617544569 ) ) ;
#23798 = DIRECTION ( 'NONE',  ( 0.000000000000000000, -1.000000000000000000, 0.000000000000000000 ) ) ;
#23799 = CARTESIAN_POINT ( 'NONE',  ( 14.97540207516710176, 1.269614109201394614, 0.8865648853246460570 ) ) ;
#23800 = SURFACE_STYLE_FILL_AREA ( #57701 ) ;
#23801 = CARTESIAN_POINT ( 'NONE',  ( -28.77610217197955933, 13.65956388957898682, -39.99200581488092610 ) ) ;
#23802 = ORIENTED_EDGE ( 'NONE', *, *, #68925, .T. ) ;
#23803 = ADVANCED_FACE ( 'NONE', ( #48786 ), #20071, .F. ) ;
#23804 = SHAPE_DEFINITION_REPRESENTATION ( #77403, #22031 ) ;
#23805 = B_SPLINE_CURVE_WITH_KNOTS ( 'NONE', 3,
 ( #17711, #75398, #50571, #93723 ),
 .UNSPECIFIED., .F., .F.,
 ( 4, 4 ),
 ( 0.8039644300567937441, 1.000000000000000000 ),
 .UNSPECIFIED. ) ;
#23806 = VECTOR ( 'NONE', #96506, 1000.000000000000000 ) ;
#23807 = CARTESIAN_POINT ( 'NONE',  ( 7.212994264445060644, 107.0171134434003903, 3.463766307298588032 ) ) ;
#23808 = CARTESIAN_POINT ( 'NONE',  ( 66.26095113931063452, 6.856755485862130937E-15, 0.000000000000000000 ) ) ;
#23809 = EDGE_CURVE ( 'NONE', #44057, #38733, #24040, .T. ) ;
#23811 = CARTESIAN_POINT ( 'NONE',  ( -11.56629382471032663, 7.278338580405791625, -9.335672732236384164 ) ) ;
#23810 = CARTESIAN_POINT ( 'NONE',  ( -15.71980515041875393, -23.09657402895575729, 36.03920351886992535 ) ) ;
#23812 = EDGE_CURVE ( 'NONE', #69611, #8963, #87599, .T. ) ;
#23813 = CARTESIAN_POINT ( 'NONE',  ( -5.082755093536325042, -14.09375000204838457, -5.082755093536325930 ) ) ;
#23814 = COLOUR_RGB ( '', 0.66274510, 0.83137255, 0.94901961) ;
#23815 = CARTESIAN_POINT ( 'NONE',  ( 21.29975379448952211, 294.8969325209483259, -1.990407376643346327 ) ) ;
#23816 = AXIS2_PLACEMENT_3D ( 'NONE', #1822, #34780, #74651 ) ;
#23817 = ADVANCED_FACE ( 'NONE', ( #63955 ), #6209, .F. ) ;
#23818 = CARTESIAN_POINT ( 'NONE',  ( 89.99999999999997158, -60.00000000000000000, 198.0238439516549818 ) ) ;
#23819 = EDGE_CURVE ( 'NONE', #62559, #93551, #16918, .T. ) ;
#23820 = ORIENTED_EDGE ( 'NONE', *, *, #1332, .F. ) ;
#23821 = FACE_OUTER_BOUND ( 'NONE', #3364, .T. ) ;
#23822 = ADVANCED_FACE ( 'NONE', ( #18597 ), #84902, .F. ) ;
#23823 = ADVANCED_FACE ( 'NONE', ( #50383 ), #76968, .F. ) ;
#23824 = CARTESIAN_POINT ( 'NONE',  ( 7.500000000000000000, 3.948247735265644653, -7.349893093596817195 ) ) ;
#23825 = CARTESIAN_POINT ( 'NONE',  ( -9.609486011791425142, 143.0915023496523020, 0.000000000000000000 ) ) ;
#23826 = CARTESIAN_POINT ( 'NONE',  ( -30.00000000000000000, 461.8802764867013479, 14.89328939273681662 ) ) ;
#23827 = CARTESIAN_POINT ( 'NONE',  ( -44.17836536378457168, 435.2619773020560956, 14.65562696767996087 ) ) ;
#23828 = ORIENTED_EDGE ( 'NONE', *, *, #105675, .T. ) ;
#23829 = CARTESIAN_POINT ( 'NONE',  ( -5.093234209761996922, -87.44467773464910465, 3.176141468578046023 ) ) ;
#23830 = CARTESIAN_POINT ( 'NONE',  ( 28.09999999999999787, 1.533819458162526451E-15, 0.000000000000000000 ) ) ;
#23831 = ORIENTED_EDGE ( 'NONE', *, *, #33199, .T. ) ;
#23832 = FILL_AREA_STYLE_COLOUR ( '', #76442 ) ;
#23833 = CYLINDRICAL_SURFACE ( 'NONE', #41581, 10.00000000000000178 ) ;
#23834 = CARTESIAN_POINT ( 'NONE',  ( -24.03027799567535538, 41.61735029016796261, -74.26546206927031335 ) ) ;
#23835 = CARTESIAN_POINT ( 'NONE',  ( -111.5755056577839497, -60.00000000000000000, 158.2576086698429094 ) ) ;
#23836 = CARTESIAN_POINT ( 'NONE',  ( 28.52991250593590777, 16.51520549712911645, -41.35291476382084852 ) ) ;
#23837 = CARTESIAN_POINT ( 'NONE',  ( -8.046879842201352779E-06, -18.58623113382856573, 26.98735514857380480 ) ) ;
#23838 =( NAMED_UNIT ( * ) PLANE_ANGLE_UNIT ( ) SI_UNIT ( $, .RADIAN. ) );
#23839 = DIRECTION ( 'NONE',  ( -1.000000000000000000, -1.224606353822377258E-16, -0.000000000000000000 ) ) ;
#23841 = CARTESIAN_POINT ( 'NONE',  ( -15.12883790376237414, 3.606441264082763887, 4.265930408091180404 ) ) ;
#23840 = CARTESIAN_POINT ( 'NONE',  ( -11.68767211932491179, -5.000000000000002665, -88.14097461399494193 ) ) ;
#23842 = CIRCLE ( 'NONE', #34159, 5.000000000000000888 ) ;
#23843 = CARTESIAN_POINT ( 'NONE',  ( -81.85741221238644982, -53.50462993550565471, 180.4532786401848341 ) ) ;
#23844 = ORIENTED_EDGE ( 'NONE', *, *, #285, .T. ) ;
#23845 = ORIENTED_EDGE ( 'NONE', *, *, #45041, .F. ) ;
#23846 = VERTEX_POINT ( 'NONE', #68181 ) ;
#23847 = DIRECTION ( 'NONE',  ( -1.000000000000000000, -0.000000000000000000, -0.000000000000000000 ) ) ;
#23848 =( NAMED_UNIT ( * ) PLANE_ANGLE_UNIT ( ) SI_UNIT ( $, .RADIAN. ) );
#23849 = DIRECTION ( 'NONE',  ( 0.000000000000000000, -1.000000000000000000, 0.000000000000000000 ) ) ;
#23850 = CIRCLE ( 'NONE', #80698, 8.000000000000000000 ) ;
#23851 = CARTESIAN_POINT ( 'NONE',  ( 8.572527594031475162E-16, -4.000000000000003553, 105.0000000000000000 ) ) ;
#23852 = CARTESIAN_POINT ( 'NONE',  ( 9.609486011791085858, 8.908497650349776364, -5.000000000000000888 ) ) ;
#23853 = DIRECTION ( 'NONE',  ( 0.000000000000000000, 0.000000000000000000, 1.000000000000000000 ) ) ;
#23854 = CARTESIAN_POINT ( 'NONE',  ( -43.03185303983481447, 485.3613526602391630, 6.073233449168583320 ) ) ;
#23855 = CARTESIAN_POINT ( 'NONE',  ( 114.0149080866908946, -60.00000000000002132, 183.4845764411877553 ) ) ;
#23856 = ADVANCED_FACE ( 'NONE', ( #59037 ), #34253, .T. ) ;
#23857 = CARTESIAN_POINT ( 'NONE',  ( -108.5047409391136455, -30.00000000000001776, 153.5997188701533105 ) ) ;
#23858 = CARTESIAN_POINT ( 'NONE',  ( -62.48275913083217858, -53.39271311663005548, 85.99345403212120686 ) ) ;
#23859 = ORIENTED_EDGE ( 'NONE', *, *, #90558, .F. ) ;
#23860 = CARTESIAN_POINT ( 'NONE',  ( -3.577867169202164632E-15, 7.321656987762870550, -3.318518101603009196 ) ) ;
#23861 = CARTESIAN_POINT ( 'NONE',  ( 108.9093010043188343, -60.00000000000492406, 198.5394929600591070 ) ) ;
#23862 = ORIENTED_EDGE ( 'NONE', *, *, #69934, .F. ) ;
#23863 = CARTESIAN_POINT ( 'NONE',  ( 2.040551993176147771, -53.39679212784579931, 32.78650623838447586 ) ) ;
#23864 = CARTESIAN_POINT ( 'NONE',  ( -2.977408999572650039, -11.56250000204838635, -7.188101187500000933 ) ) ;
#23865 = AXIS2_PLACEMENT_3D ( 'NONE', #61813, #44008, #92549 ) ;
#23866 = CARTESIAN_POINT ( 'NONE',  ( 9.250997389131581983, -5.000000000000000000, 0.000000000000000000 ) ) ;
#23867 = VERTEX_POINT ( 'NONE', #9934 ) ;
#23869 = CARTESIAN_POINT ( 'NONE',  ( 35.20565090456888413, 464.3972607891108169, 19.03665261460805169 ) ) ;
#23868 =( GEOMETRIC_REPRESENTATION_CONTEXT ( 3 ) GLOBAL_UNCERTAINTY_ASSIGNED_CONTEXT ( ( #82853 ) ) GLOBAL_UNIT_ASSIGNED_CONTEXT ( ( #93826, #79222, #53364 ) ) REPRESENTATION_CONTEXT ( 'NONE', 'WORKASPACE' ) );
#23870 = ORIENTED_EDGE ( 'NONE', *, *, #71006, .F. ) ;
#23871 = CARTESIAN_POINT ( 'NONE',  ( -46.00000000000000711, 488.0476234683169992, 1.803521264818849668 ) ) ;
#23872 = CARTESIAN_POINT ( 'NONE',  ( 7.188101187499999156, -28.62500000204838813, 2.977408999572654924 ) ) ;
#23873 = CARTESIAN_POINT ( 'NONE',  ( -112.0155942784085710, -59.99999999999998579, 179.5554985363227729 ) ) ;
#23874 = CARTESIAN_POINT ( 'NONE',  ( 9.269408785705698151, -55.04596499575451674, 23.24750950774772562 ) ) ;
#23875 = CARTESIAN_POINT ( 'NONE',  ( 4.401442555609581635E-16, -26.65625000204838813, -7.188101187500000044 ) ) ;
#23876 = CARTESIAN_POINT ( 'NONE',  ( 46.00000000000000000, 460.8575856737739969, 7.929402417993718366 ) ) ;
#23877 = CARTESIAN_POINT ( 'NONE',  ( -11.42862062371675691, 13.43085172858349274, 9.993030149489131375 ) ) ;
#23878 = CARTESIAN_POINT ( 'NONE',  ( -10.49999999997808331, -5.000000000000000000, -12.52300748972991506 ) ) ;
#23879 = FILL_AREA_STYLE ('',( #90171 ) ) ;
#23880 = ADVANCED_FACE ( 'NONE', ( #74658 ), #85627, .T. ) ;
#23881 = FILL_AREA_STYLE ('',( #7638 ) ) ;
#23882 = DIRECTION ( 'NONE',  ( 0.000000000000000000, 0.000000000000000000, 1.000000000000000000 ) ) ;
#23883 = CARTESIAN_POINT ( 'NONE',  ( 90.89309866034619745, -59.99999999999998579, 60.81559558904974239 ) ) ;
#23884 = CARTESIAN_POINT ( 'NONE',  ( -32.49993360873129689, -22.15177377451222540, 30.86871524635706265 ) ) ;
#23885 =( GEOMETRIC_REPRESENTATION_CONTEXT ( 3 ) GLOBAL_UNCERTAINTY_ASSIGNED_CONTEXT ( ( #21365 ) ) GLOBAL_UNIT_ASSIGNED_CONTEXT ( ( #63511, #30088, #79672 ) ) REPRESENTATION_CONTEXT ( 'NONE', 'WORKASPACE' ) );
#23886 = CARTESIAN_POINT ( 'NONE',  ( 37.17835306669755369, -22.20693324183691075, 33.02635006318946154 ) ) ;
#23888 = AXIS2_PLACEMENT_3D ( 'NONE', #67349, #66809, #58172 ) ;
#23887 = DIRECTION ( 'NONE',  ( -0.9639005798659543434, 0.1664520902827338611, 0.2078205326106775386 ) ) ;
#23889 = VERTEX_POINT ( 'NONE', #2371 ) ;
#23890 = AXIS2_PLACEMENT_3D ( 'NONE', #84642, #33998, #66867 ) ;
#23891 = CARTESIAN_POINT ( 'NONE',  ( 43.61263226029653595, 434.4864728595456427, 10.89080223165081662 ) ) ;
#23892 = CARTESIAN_POINT ( 'NONE',  ( -72.86006754029503441, -38.32651382585556377, 151.4076042794326042 ) ) ;
#23893 = VERTEX_POINT ( 'NONE', #37447 ) ;
#23895 = DIRECTION ( 'NONE',  ( -1.000000000000000000, -1.224606353822377258E-16, -0.000000000000000000 ) ) ;
#23894 = FACE_OUTER_BOUND ( 'NONE', #104200, .T. ) ;
#23896 = DIRECTION ( 'NONE',  ( -1.000000000000000000, -1.224606353822377258E-16, -0.000000000000000000 ) ) ;
#23897 = CARTESIAN_POINT ( 'NONE',  ( 6.168902648239645181, 0.6556005035803867953, 6.499999999999999112 ) ) ;
#23898 = CIRCLE ( 'NONE', #56554, 5.000000000000002665 ) ;
#23899 = CARTESIAN_POINT ( 'NONE',  ( 40.02592568779148507, 1.482358050883964840E-15, 0.000000000000000000 ) ) ;
#23900 = CARTESIAN_POINT ( 'NONE',  ( -38.81809298152867882, 25.18270264959180693, 12.26709487888331829 ) ) ;
#23901 = CARTESIAN_POINT ( 'NONE',  ( -29.34015253733962680, 323.3386329294219195, 13.49677481019017478 ) ) ;
#23902 = CARTESIAN_POINT ( 'NONE',  ( 16.96051095573448819, 45.50173602991597477, 6.619600894237273714 ) ) ;
#23903 = EDGE_CURVE ( 'NONE', #27209, #57904, #70316, .T. ) ;
#23904 = CARTESIAN_POINT ( 'NONE',  ( 100.7769336070389983, -59.99999999999999289, 85.59131652555993242 ) ) ;
#23905 = CARTESIAN_POINT ( 'NONE',  ( -5.559241731430971889, -51.12552554554342521, 39.84970532565870371 ) ) ;
#23906 = CARTESIAN_POINT ( 'NONE',  ( 0.5805565836007581249, -3.752776749732553263, 6.499999999999999112 ) ) ;
#23907 = CARTESIAN_POINT ( 'NONE',  ( 6.683837171061803417, 3.955946848495959234, -6.851900933636991375 ) ) ;
#23908 = ORIENTED_EDGE ( 'NONE', *, *, #95507, .F. ) ;
#23909 = CIRCLE ( 'NONE', #37701, 5.999999999999998224 ) ;
#23910 = CARTESIAN_POINT ( 'NONE',  ( -87.74897877105536281, -30.00000000000501998, -17.46874925390407896 ) ) ;
#23911 = EDGE_LOOP ( 'NONE', ( #38593, #102910, #12599, #44600 ) ) ;
#23912 = CARTESIAN_POINT ( 'NONE',  ( -9.442395496852061143, -56.44162292811314074, 30.29618450995123169 ) ) ;
#23913 = CARTESIAN_POINT ( 'NONE',  ( -15.50133110405651315, 2.625676835716459045, -0.7746791666654442299 ) ) ;
#23914 = SURFACE_STYLE_FILL_AREA ( #71891 ) ;
#23915 = LINE ( 'NONE', #56756, #94971 ) ;
#23916 = CARTESIAN_POINT ( 'NONE',  ( -21.96569361886333382, 28.02808497942502441, -31.91099187246642543 ) ) ;
#23917 = CARTESIAN_POINT ( 'NONE',  ( -2.977408999572654480, -24.50000000204839168, 7.188101187499999156 ) ) ;
#23918 = DIRECTION ( 'NONE',  ( 0.000000000000000000, 0.000000000000000000, -1.000000000000000000 ) ) ;
#23919 = CARTESIAN_POINT ( 'NONE',  ( 6.701893401236465486, 41.44328394225253476, -70.59544911815949320 ) ) ;
#23920 = AXIS2_PLACEMENT_3D ( 'NONE', #99051, #20198, #91527 ) ;
#23921 = ORIENTED_EDGE ( 'NONE', *, *, #78440, .F. ) ;
#23922 = CONICAL_SURFACE ( 'NONE', #34305, 3.400000000000000355, 0.9599310885968748153 ) ;
#23923 = PRODUCT_DEFINITION ( 'UNKNOWN', '', #85274, #106061 ) ;
#23924 = PRESENTATION_LAYER_ASSIGNMENT (  '', '', ( #34241 ) ) ;
#23926 = ORIENTED_EDGE ( 'NONE', *, *, #23994, .F. ) ;
#23925 = CARTESIAN_POINT ( 'NONE',  ( 4.448407490268952991, -1.969035902430321894, 102.6871849564181360 ) ) ;
#23927 = CARTESIAN_POINT ( 'NONE',  ( 79.82907406774054948, -56.85525210295124054, 167.4536056965665125 ) ) ;
#23928 = DIRECTION ( 'NONE',  ( 0.000000000000000000, 1.000000000000000000, -1.224646799147353207E-16 ) ) ;
#23929 = CARTESIAN_POINT ( 'NONE',  ( -38.54737907208687631, 27.49609987706101677, -11.41442684321127565 ) ) ;
#23930 = ORIENTED_EDGE ( 'NONE', *, *, #77415, .F. ) ;
#23931 = CARTESIAN_POINT ( 'NONE',  ( -62.90160406446442209, 50.00000000000000711, -3.733639982922376532 ) ) ;
#23932 = CARTESIAN_POINT ( 'NONE',  ( -0.07705973910397148630, 12.91535575337010933, -51.74999999999999289 ) ) ;
#23933 = CARTESIAN_POINT ( 'NONE',  ( -1.320432766682874540E-15, -13.53125000204838457, 7.188101187500000044 ) ) ;
#23934 = DIRECTION ( 'NONE',  ( 0.000000000000000000, 1.000000000000000000, 0.000000000000000000 ) ) ;
#23935 = CARTESIAN_POINT ( 'NONE',  ( -27.27894591530610668, -57.67773572996152609, 43.94474244872281332 ) ) ;
#23936 = B_SPLINE_SURFACE_WITH_KNOTS ( 'NONE', 3, 3, ( 
 ( #73994, #75048, #51306, #49724, #76124, #8733, #84759, #43239 ),
 ( #84229, #2220, #10841, #76, #65913, #98793, #24950, #57804 ),
 ( #90727, #16842, #20616, #4366, #21130, #11377, #94994, #3308 ),
 ( #93915, #62615, #12444, #103072, #2765, #35714, #69642, #52376 ),
 ( #53959, #78253, #77736, #61029, #28683, #44302, #93393, #102536 ),
 ( #61565, #37304, #19539, #70168, #86897, #101995, #20072, #62102 ),
 ( #77196, #85844, #29227, #12970, #94460, #45896, #78772, #4906 ),
 ( #53457, #37836, #70701, #86378, #103591, #52919, #29740, #45371 ),
 ( #95501, #85287, #21644, #54480, #11918, #87427, #43760, #76652 ),
 ( #68591, #101476, #27627, #44846, #3847, #60508, #36777, #36253 ) ),
 .UNSPECIFIED., .F., .F., .F.,
 ( 4, 2, 2, 2, 4 ),
 ( 4, 2, 2, 4 ),
 ( 0.000000000000000000, 0.1250000000000000000, 0.2500000000000000000, 0.5000000000000000000, 1.000000000000000000 ),
 ( 0.000000000000000000, 0.2500000000000000000, 0.5000000000000000000, 1.000000000000000000 ),
 .UNSPECIFIED. ) ;
#23937 = CARTESIAN_POINT ( 'NONE',  ( 18.46952720637950307, 302.6549406408472009, 9.895497875268649324 ) ) ;
#23938 = ORIENTED_EDGE ( 'NONE', *, *, #30692, .F. ) ;
#23939 =( NAMED_UNIT ( * ) SI_UNIT ( $, .STERADIAN. ) SOLID_ANGLE_UNIT ( ) );
#23940 = AXIS2_PLACEMENT_3D ( 'NONE', #26238, #50975, #18665 ) ;
#23941 = LINE ( 'NONE', #14199, #25133 ) ;
#23943 = CARTESIAN_POINT ( 'NONE',  ( 4.852941176470595863, 39.99999999999999289, -70.80672828634229177 ) ) ;
#23942 =( BOUNDED_SURFACE ( )  B_SPLINE_SURFACE ( 3, 2, ( 
 ( #84382, #93545, #35326 ),
 ( #43915, #10471, #34260 ),
 ( #26187, #76802, #60133 ),
 ( #75745, #67132, #42311 ),
 ( #11527, #19690, #92996 ),
 ( #69274, #2381, #84911 ) ),
 .UNSPECIFIED., .F., .F., .T. ) 
 B_SPLINE_SURFACE_WITH_KNOTS ( ( 4, 2, 4 ),
 ( 3, 3 ),
 ( 0.03172058138205609973, 0.03571597378202084894, 0.03971136618198560508 ),
 ( 0.000000000000000000, 1.000000000000000000 ),
 .UNSPECIFIED. ) 
 GEOMETRIC_REPRESENTATION_ITEM ( )  RATIONAL_B_SPLINE_SURFACE ( (
 ( 1.000000000000000000, 0.8047780791350978014, 1.000000000000000000),
 ( 1.000000000000000000, 0.8123796029720886658, 1.000000000000000000),
 ( 1.000000000000000000, 0.8190681660672747277, 1.000000000000000000),
 ( 1.000000000000000000, 0.8192342536573682388, 1.000000000000000000),
 ( 1.000000000000000000, 0.8126124427163601283, 1.000000000000000000),
 ( 1.000000000000000000, 0.8047712715942065831, 1.000000000000000000) ) ) 
 REPRESENTATION_ITEM ( '' )  SURFACE ( )  );
#23944 = ADVANCED_FACE ( 'NONE', ( #53068 ), #21265, .F. ) ;
#23945 = PRESENTATION_STYLE_ASSIGNMENT (( #63322 ) ) ;
#23946 = VERTEX_POINT ( 'NONE', #52519 ) ;
#23947 = CARTESIAN_POINT ( 'NONE',  ( 7.188101187500000044, -29.65625000204838813, 0.000000000000000000 ) ) ;
#23948 = CARTESIAN_POINT ( 'NONE',  ( -27.13328449130634112, -20.30828638014859422, 31.75027141071463888 ) ) ;
#23949 = FILL_AREA_STYLE_COLOUR ( '', #64635 ) ;
#23950 = CARTESIAN_POINT ( 'NONE',  ( 0.3378829312054938971, 51.28040138220650590, -10.21513970828568851 ) ) ;
#23951 = AXIS2_PLACEMENT_3D ( 'NONE', #13691, #80548, #21834 ) ;
#23952 = CARTESIAN_POINT ( 'NONE',  ( 35.05535456316795972, 439.9564985210690224, 24.34373081590672427 ) ) ;
#23953 = APPLICATION_PROTOCOL_DEFINITION ( 'draft international standard', 'automotive_design', 1998, #56217 ) ;
#23954 = CARTESIAN_POINT ( 'NONE',  ( 49.24240974153283901, 8.191948471291036427, 15.29453271768024258 ) ) ;
#23955 = VERTEX_POINT ( 'NONE', #62758 ) ;
#23956 = DIRECTION ( 'NONE',  ( -1.000000000000000000, -1.224606353822377258E-16, -0.000000000000000000 ) ) ;
#23957 = CARTESIAN_POINT ( 'NONE',  ( -4.397168787612346641, 15.00000000000000000, 9.999999999999998224 ) ) ;
#23958 = EDGE_CURVE ( 'NONE', #37118, #44950, #13223, .T. ) ;
#23959 = DIRECTION ( 'NONE',  ( 0.5735764363510554853, 0.8191520442889852482, 0.000000000000000000 ) ) ;
#23960 = CARTESIAN_POINT ( 'NONE',  ( -33.87327693568649778, -30.97787551643977366, -37.97348367960884019 ) ) ;
#23961 = CARTESIAN_POINT ( 'NONE',  ( 9.830769230769229594, 1.411358822780289120E-15, 0.000000000000000000 ) ) ;
#23962 = EDGE_CURVE ( 'NONE', #67861, #23867, #48967, .T. ) ;
#23963 = CARTESIAN_POINT ( 'NONE',  ( 14.90155531838479064, 42.58002643028073919, -90.01374843427898043 ) ) ;
#23964 = ORIENTED_EDGE ( 'NONE', *, *, #12691, .F. ) ;
#23965 = LINE ( 'NONE', #81086, #89197 ) ;
#23966 = CARTESIAN_POINT ( 'NONE',  ( 106.4547888626981944, -57.65150656016882635, 200.5657376461139449 ) ) ;
#23967 = CIRCLE ( 'NONE', #97987, 4.000000000000001776 ) ;
#23968 = CARTESIAN_POINT ( 'NONE',  ( 37.40828998627038970, 463.5731143434501291, 19.60478905908873415 ) ) ;
#23969 = CARTESIAN_POINT ( 'NONE',  ( 1.797717371853386981, 14.26981950330974946, 6.769760908209460304 ) ) ;
#23970 = LINE ( 'NONE', #38671, #42447 ) ;
#23971 = CARTESIAN_POINT ( 'NONE',  ( 34.13947300040292987, 489.1610961117067973, 11.38003656226467619 ) ) ;
#23972 = CARTESIAN_POINT ( 'NONE',  ( -74.34185808010607843, -60.00000000000000000, 175.6139210523332963 ) ) ;
#23973 = AXIS2_PLACEMENT_3D ( 'NONE', #11701, #59219, #51093 ) ;
#23974 = ADVANCED_FACE ( 'NONE', ( #44447 ), #96208, .T. ) ;
#23975 = CARTESIAN_POINT ( 'NONE',  ( -24.37088254901632567, 295.3567874699774620, -9.892597027136796228 ) ) ;
#23976 = CARTESIAN_POINT ( 'NONE',  ( 70.89460441624491693, -4.000000000000000888, 4.898587196589422689E-16 ) ) ;
#23977 = CARTESIAN_POINT ( 'NONE',  ( -45.49982102694234953, 388.3127959276886827, 7.886590035822850453 ) ) ;
#23978 = B_SPLINE_CURVE_WITH_KNOTS ( 'NONE', 3,
 ( #104338, #13733, #39637, #39103, #71982, #89238, #31032, #22930, #104892, #30486, #46641, #97308 ),
 .UNSPECIFIED., .F., .F.,
 ( 4, 2, 2, 2, 2, 4 ),
 ( 0.05939584100412212408, 0.06135403683694420907, 0.06233313475335525849, 0.06331223266976629405, 0.06527042850258839291, 0.06722862433541047789 ),
 .UNSPECIFIED. ) ;
#23979 = CARTESIAN_POINT ( 'NONE',  ( -85.84496634730722064, -28.47654455628507009, 180.7473491047089169 ) ) ;
#23980 = ORIENTED_EDGE ( 'NONE', *, *, #8754, .F. ) ;
#23981 = CARTESIAN_POINT ( 'NONE',  ( 30.40875718013408857, 312.9039625323161431, -7.101849360686649959 ) ) ;
#23982 = EDGE_LOOP ( 'NONE', ( #48901, #57571, #7100 ) ) ;
#23983 = CARTESIAN_POINT ( 'NONE',  ( 16.02333492353055533, 4.076663811953147309, 2.240748598616852938 ) ) ;
#23984 = CARTESIAN_POINT ( 'NONE',  ( -1.469576158976823671E-14, 0.000000000000000000, 60.00000000000000000 ) ) ;
#23985 = CARTESIAN_POINT ( 'NONE',  ( -84.42827057453619943, -45.27066986597937159, -4.045256569822196724 ) ) ;
#23986 = CARTESIAN_POINT ( 'NONE',  ( 10.51296777078104050, 50.00000000000000000, -92.64705882352942012 ) ) ;
#23987 = CARTESIAN_POINT ( 'NONE',  ( 0.000000000000000000, 12.00000000000000000, -2.000000000000000000 ) ) ;
#23988 = ORIENTED_EDGE ( 'NONE', *, *, #93691, .F. ) ;
#23989 = CARTESIAN_POINT ( 'NONE',  ( 27.71624102341542439, 36.65790090521107913, -7.705193261028457918 ) ) ;
#23990 = CARTESIAN_POINT ( 'NONE',  ( 10.52363060357091307, 10.25739784061314630, -10.32240453393743707 ) ) ;
#23991 = CARTESIAN_POINT ( 'NONE',  ( -17.01589776168603407, -1.734723475976807094E-15, 2.227375807157432774 ) ) ;
#23992 = CIRCLE ( 'NONE', #73834, 4.000000000000000888 ) ;
#23993 = CARTESIAN_POINT ( 'NONE',  ( -32.82691535583476394, 485.1045372766794799, 1.724905475514959097 ) ) ;
#23994 = EDGE_CURVE ( 'NONE', #39330, #53832, #11531, .T. ) ;
#23995 = CARTESIAN_POINT ( 'NONE',  ( -69.60683966046387638, -29.99999999999998224, -29.88974110699236775 ) ) ;
#23996 = CARTESIAN_POINT ( 'NONE',  ( -77.18609064198581393, -49.90775283772178028, 139.5545092987445059 ) ) ;
#23997 = VERTEX_POINT ( 'NONE', #1710 ) ;
#23998 = CARTESIAN_POINT ( 'NONE',  ( 20.75554216095374116, -29.99999999999998579, 37.60191050100322485 ) ) ;
#23999 = DIRECTION ( 'NONE',  ( -1.000000000000000000, -0.000000000000000000, -0.000000000000000000 ) ) ;
#24000 = CARTESIAN_POINT ( 'NONE',  ( 91.04805003644649730, -57.66417010318413361, -20.95954831595424039 ) ) ;
#24001 = CYLINDRICAL_SURFACE ( 'NONE', #11296, 5.000000000000002665 ) ;
#24002 = LINE ( 'NONE', #25599, #25304 ) ;
#24003 = ORIENTED_EDGE ( 'NONE', *, *, #73986, .T. ) ;
#24004 = SURFACE_STYLE_USAGE ( .BOTH. , #89240 ) ;
#24005 = CARTESIAN_POINT ( 'NONE',  ( 0.000000000000000000, 0.000000000000000000, -10.00000000000000178 ) ) ;
#24006 = CARTESIAN_POINT ( 'NONE',  ( -5.082755093536325042, -18.59375000204838457, -5.082755093536325930 ) ) ;
#24007 = CARTESIAN_POINT ( 'NONE',  ( 43.65008909229851497, 485.2536725492909682, 3.136905111439891147 ) ) ;
#24008 = CARTESIAN_POINT ( 'NONE',  ( 10.00005432054556742, 80.99986419862088383, 0.2621623937322758446 ) ) ;
#24009 = FILL_AREA_STYLE ('',( #40676 ) ) ;
#24010 = CARTESIAN_POINT ( 'NONE',  ( -7.500000000000000000, -3.160302461882437797, -7.231849989190477501 ) ) ;
#24011 = CYLINDRICAL_SURFACE ( 'NONE', #76593, 1.250000000000001110 ) ;
#24012 = CIRCLE ( 'NONE', #30942, 60.00000000000000000 ) ;
#24013 = ORIENTED_EDGE ( 'NONE', *, *, #97354, .F. ) ;
#24014 = CARTESIAN_POINT ( 'NONE',  ( 28.58349330513380337, 1.593028355512270962E-15, 0.000000000000000000 ) ) ;
#24016 = CARTESIAN_POINT ( 'NONE',  ( 29.80797822681026688, -53.38109471923124261, 35.51269461402811345 ) ) ;
#24015 = FACE_OUTER_BOUND ( 'NONE', #6229, .T. ) ;
#24017 = CARTESIAN_POINT ( 'NONE',  ( 24.42584379203400857, 27.59191556861860661, -31.59852321640943629 ) ) ;
#24018 = CLOSED_SHELL ( 'NONE', ( #41149, #64573, #97270, #16200, #2919, #57972, #24304, #59707, #68940, #76418, #79773, #103755, #86541, #39908, #60051, #92380, #87714, #36965, #9586, #14955, #22642, #68465, #86204, #2971, #47511, #45712, #18252, #20149, #24034, #73207, #14770, #76490, #35537, #25578, #51885, #43736, #33355, #76476, #93140, #51895, #62935, #62982, #41558, #9136, #46188, #63849, #81123, #63284, #28500, #89919, #69275, #59896, #45285, #25155, #25219, #13384, #68295, #48558, #67813, #8887, #19058, #47227, #68828, #15548, #37108, #59228, #38023, #78178, #39613, #65570, #101900, #41412, #38892, #20862, #59544, #386, #82278, #89670, #106729, #61677, #4886, #77597, #75843, #89298, #81624, #61788, #32540, #62111, #59794, #25796, #27101, #10285, #29024, #82066, #86410, #87435, #74866, #38301, #78261, #42150, #75368, #42221, #3282, #20750, #26127, #21059, #46583, #35027, #30239, #30137, #24604, #3996, #83586, #13159, #3316, #23823, #48595, #59164, #49013, #86756, #79998, #19816, #84951, #65819, #40831, #9435, #86820, #93060, #19569, #104472, #15873, #88908, #86708, #6455, #65080, #100131, #26376, #16684, #74127, #54601, #35191, #73124, #72392, #99609, #7031, #67009, #66078, #77104, #52905, #33947, #43581, #69753, #8725, #77976, #105228, #63504, #60577, #67972, #73814, #42497, #6610, #36298, #100508, #74752, #54298, #82123, #53303, #14499, #16908, #56439, #70098, #102597, #49408, #73860, #92622, #57552, #4009, #39556, #51186, #12578, #83073, #59793, #11231, #53631, #12553, #7492, #70895, #62649, #6908, #30855, #24941, #13713, #66732, #6806, #13722, #67172, #22992, #100710, #32443, #22951, #55954, #100000, #63225, #96098, #33488, #98475, #84293, #41865, #76025, #67471, #67527, #90921, #13436, #19203, #96337 ) ) ;
#24019 = ORIENTED_EDGE ( 'NONE', *, *, #38374, .T. ) ;
#24020 = EDGE_LOOP ( 'NONE', ( #37640, #38169, #91803, #59709 ) ) ;
#24022 = CARTESIAN_POINT ( 'NONE',  ( 36.51699212156835017, 461.3945476718891996, 3.425852496309615525 ) ) ;
#24021 = DIRECTION ( 'NONE',  ( 0.000000000000000000, 0.000000000000000000, -1.000000000000000000 ) ) ;
#24023 = DIRECTION ( 'NONE',  ( 1.000000000000000000, 1.224606353822377258E-16, 0.000000000000000000 ) ) ;
#24024 = DIRECTION ( 'NONE',  ( -1.000000000000000000, -1.224606353822377258E-16, -0.000000000000000000 ) ) ;
#24025 = CARTESIAN_POINT ( 'NONE',  ( 42.50585811106661538, 460.9576338508423987, 2.953927975892467472 ) ) ;
#24026 = DIRECTION ( 'NONE',  ( 1.000000000000000000, 0.000000000000000000, 0.000000000000000000 ) ) ;
#24027 = CARTESIAN_POINT ( 'NONE',  ( -7.500000000000000888, 2.575910028905293192, -0.3641256808890049879 ) ) ;
#24028 = EDGE_LOOP ( 'NONE', ( #67486, #16726, #57219, #35315 ) ) ;
#24029 = EDGE_CURVE ( 'NONE', #56766, #36063, #98808, .T. ) ;
#24030 = CARTESIAN_POINT ( 'NONE',  ( 65.87419555395186421, -60.00000000000000711, -33.93111748855666576 ) ) ;
#24031 = CARTESIAN_POINT ( 'NONE',  ( 32.91521444485818648, 465.6822365171199181, 10.74527606630968357 ) ) ;
#24032 = CARTESIAN_POINT ( 'NONE',  ( 30.00000000000035527, 464.1529070875457137, 11.87753652825273143 ) ) ;
#24033 = CARTESIAN_POINT ( 'NONE',  ( -6.061808134762952882, -5.000000000000000000, -95.47796581438812780 ) ) ;
#24034 = ADVANCED_FACE ( 'NONE', ( #616 ), #82645, .T. ) ;
#24035 = CARTESIAN_POINT ( 'NONE',  ( 47.14735620107882141, 13.37129584416865313, -14.71343070694231514 ) ) ;
#24036 = VERTEX_POINT ( 'NONE', #42177 ) ;
#24037 = ORIENTED_EDGE ( 'NONE', *, *, #74896, .T. ) ;
#24038 = ORIENTED_EDGE ( 'NONE', *, *, #57748, .T. ) ;
#24039 = CARTESIAN_POINT ( 'NONE',  ( 0.1682271994785180524, 54.30758622938870417, 7.749999999999998224 ) ) ;
#24040 = LINE ( 'NONE', #89280, #4539 ) ;
#24041 =( LENGTH_UNIT ( ) NAMED_UNIT ( * ) SI_UNIT ( .MILLI., .METRE. ) );
#24042 = CARTESIAN_POINT ( 'NONE',  ( 33.14480304713701742, 382.6980963264236379, 25.00621942273273746 ) ) ;
#24043 = CARTESIAN_POINT ( 'NONE',  ( -42.84559671612151988, 321.7670785502716626, -3.464489948122500884 ) ) ;
#24044 = CARTESIAN_POINT ( 'NONE',  ( -6.125000000000000000, -60.71953810597579348, 14.41094225130411033 ) ) ;
#24046 = DIRECTION ( 'NONE',  ( 0.000000000000000000, 1.000000000000000000, 0.000000000000000000 ) ) ;
#24045 = STYLED_ITEM ( 'NONE', ( #47889 ), #90435 ) ;
#24047 = SURFACE_SIDE_STYLE ('',( #100015 ) ) ;
#24048 = ORIENTED_EDGE ( 'NONE', *, *, #96576, .F. ) ;
#24049 = CARTESIAN_POINT ( 'NONE',  ( -10.12027838911100730, 43.29307385079338388, 15.39942933061531782 ) ) ;
#24050 = ORIENTED_EDGE ( 'NONE', *, *, #1900, .F. ) ;
#24051 = DIRECTION ( 'NONE',  ( -1.000000000000000000, -0.000000000000000000, -0.000000000000000000 ) ) ;
#24052 = CARTESIAN_POINT ( 'NONE',  ( -23.99113157954622366, 50.00000000000000000, -74.11764705887553362 ) ) ;
#24053 = DIRECTION ( 'NONE',  ( 0.3420201433256622736, 1.150791560227853228E-16, 0.9396926207859106484 ) ) ;
#24054 = CARTESIAN_POINT ( 'NONE',  ( -26.99263046833200619, -59.99999999999997868, 35.69452638192248628 ) ) ;
#24055 = CARTESIAN_POINT ( 'NONE',  ( 64.92191423604261047, -36.00617188022724946, 84.15699025978140924 ) ) ;
#24056 = ADVANCED_FACE ( 'NONE', ( #84242 ), #59994, .T. ) ;
#24057 = EDGE_CURVE ( 'NONE', #82194, #60462, #90740, .T. ) ;
#24058 = EDGE_LOOP ( 'NONE', ( #86323, #89254, #60885, #59379, #44454 ) ) ;
#24059 = CARTESIAN_POINT ( 'NONE',  ( 0.4037800551813793826, -7.199367570657615900, -0.5303295852573158831 ) ) ;
#24060 = CARTESIAN_POINT ( 'NONE',  ( -89.99999999999997158, -52.00000000000000000, 196.0238439516549818 ) ) ;
#24061 = ORIENTED_EDGE ( 'NONE', *, *, #22604, .T. ) ;
#24062 = AXIS2_PLACEMENT_3D ( 'NONE', #34337, #52067, #59119 ) ;
#24063 = AXIS2_PLACEMENT_3D ( 'NONE', #82712, #83760, #9868 ) ;
#24064 = CARTESIAN_POINT ( 'NONE',  ( -35.67925427714555298, 491.2490127027255653, 12.19183392504566044 ) ) ;
#24065 = CARTESIAN_POINT ( 'NONE',  ( -8.000000000000000000, -29.93750000409677270, -9.797174393178825657E-16 ) ) ;
#24066 = CARTESIAN_POINT ( 'NONE',  ( -4.175893272572330339, -5.000000000001136868, -7.137815226410158864 ) ) ;
#24067 = CARTESIAN_POINT ( 'NONE',  ( 6.936184427528457874, 0.000000000000000000, 0.000000000000000000 ) ) ;
#24068 = AXIS2_PLACEMENT_3D ( 'NONE', #26662, #92952, #51950 ) ;
#24069 = FILL_AREA_STYLE_COLOUR ( '', #34437 ) ;
#24070 = CARTESIAN_POINT ( 'NONE',  ( -6.016305315790704711, 4.472071644617155783, 4.999999999999999112 ) ) ;
#24071 = CARTESIAN_POINT ( 'NONE',  ( 0.000000000000000000, 23.58303312036771615, -45.10524579772351217 ) ) ;
#24072 = DIRECTION ( 'NONE',  ( 0.05552278246086851665, -4.145567951108498278E-15, 0.9984574205382035217 ) ) ;
#24073 = CARTESIAN_POINT ( 'NONE',  ( -1.510421413154566572, 15.23810023151366977, -9.910377230549926253 ) ) ;
#24074 = ORIENTED_EDGE ( 'NONE', *, *, #93832, .F. ) ;
#24075 = CARTESIAN_POINT ( 'NONE',  ( -4.852941176470598528, -5.000000000000002665, -70.80672828634229177 ) ) ;
#24077 = CARTESIAN_POINT ( 'NONE',  ( 4.449340811590402289, -60.00000000000000000, 39.63040262224204469 ) ) ;
#24076 =( BOUNDED_SURFACE ( )  B_SPLINE_SURFACE ( 2, 3, ( 
 ( #61553, #11905, #28668, #76638, #86364, #94447, #68575, #35701, #78239, #44832 ),
 ( #20605, #26547, #101461, #77183, #100912, #52907, #92282, #3830, #53442, #19526 ),
 ( #20057, #11360, #3294, #4353, #12429, #45359, #67504, #36236, #100386, #18438 ) ),
 .UNSPECIFIED., .F., .F., .F. ) 
 B_SPLINE_SURFACE_WITH_KNOTS ( ( 3, 3 ),
 ( 4, 2, 2, 2, 4 ),
 ( 0.000000000000000000, 1.000000000000000000 ),
 ( 0.2013554496957829509, 0.2052093776119387758, 0.2375733647630427492, 0.2537553583385947498, 0.2699373519141466948 ),
 .UNSPECIFIED. ) 
 GEOMETRIC_REPRESENTATION_ITEM ( )  RATIONAL_B_SPLINE_SURFACE ( (
 ( 1.000000000000000000, 1.000000000000000000, 1.000000000000000000, 1.000000000000000000, 1.000000000000000000, 1.000000000000000000, 1.000000000000000000, 1.000000000000000000, 1.000000000000000000, 1.000000000000000000),
 ( 1.857142857142858317, 1.857142857142858317, 1.857142857142858317, 1.857142857142858317, 1.857142857142858317, 1.857142857142858317, 1.857142857142857428, 1.857142857142857428, 1.857142857142858317, 1.857142857142858317),
 ( 1.000000000000000000, 1.000000000000000000, 1.000000000000000000, 1.000000000000000000, 1.000000000000000000, 1.000000000000000000, 1.000000000000000000, 1.000000000000000000, 1.000000000000000000, 1.000000000000000000) ) ) 
 REPRESENTATION_ITEM ( '' )  SURFACE ( )  );
#24078 = CARTESIAN_POINT ( 'NONE',  ( -98.54871067950367092, -30.00000000000000355, 189.7749550243679835 ) ) ;
#24079 = ADVANCED_FACE ( 'NONE', ( #16856 ), #43897, .F. ) ;
#24080 = CIRCLE ( 'NONE', #89575, 3.000000000000015543 ) ;
#24081 = FACE_OUTER_BOUND ( 'NONE', #100536, .T. ) ;
#24082 = CARTESIAN_POINT ( 'NONE',  ( 44.88275167603845262, -57.68329172827992579, 64.90723355357903301 ) ) ;
#24083 = ADVANCED_FACE ( 'NONE', ( #26581 ), #106218, .T. ) ;
#24085 = CARTESIAN_POINT ( 'NONE',  ( -9.787706584712674740, 7.346100692761604378, 1.606208808826772749 ) ) ;
#24084 = CARTESIAN_POINT ( 'NONE',  ( 5.656854249492380582, -15.50000000409677092, -5.656854249492379694 ) ) ;
#24087 = CARTESIAN_POINT ( 'NONE',  ( 10.12775410031062151, -22.65524328215749605, -38.54261129078143000 ) ) ;
#24086 = AXIS2_PLACEMENT_3D ( 'NONE', #62345, #87148, #90311 ) ;
#24088 = DIRECTION ( 'NONE',  ( 0.000000000000000000, -1.000000000000000000, 0.000000000000000000 ) ) ;
#24089 = CARTESIAN_POINT ( 'NONE',  ( 11.36650669486618881, 1.474610560812782335E-15, 0.000000000000000000 ) ) ;
#24090 = CARTESIAN_POINT ( 'NONE',  ( -21.09521276825200786, -60.00000000000000000, 40.37433778268253803 ) ) ;
#24091 = CARTESIAN_POINT ( 'NONE',  ( 11.54022871740204081, 12.38863196018314383, 9.987975719479239345 ) ) ;
#24092 = AXIS2_PLACEMENT_3D ( 'NONE', #97409, #73126, #23569 ) ;
#24093 = CARTESIAN_POINT ( 'NONE',  ( 37.88504238421471371, 463.4171042825133213, 19.90923349043903556 ) ) ;
#24094 = CARTESIAN_POINT ( 'NONE',  ( -86.75485909622595670, -46.46991862354892078, 190.6011527551186475 ) ) ;
#24095 = ORIENTED_EDGE ( 'NONE', *, *, #50399, .F. ) ;
#24096 = CARTESIAN_POINT ( 'NONE',  ( 17.50000000000004974, 49.61376050339585220, 62.33429930757360182 ) ) ;
#24097 = DIRECTION ( 'NONE',  ( 0.000000000000000000, 0.000000000000000000, -1.000000000000000000 ) ) ;
#24098 = CARTESIAN_POINT ( 'NONE',  ( -6.163436733616805441, -49.92086198580086176, 32.19980418369003417 ) ) ;
#24099 = CARTESIAN_POINT ( 'NONE',  ( 0.5805565836007667846, -3.752776749732578132, -6.500000000000000888 ) ) ;
#24101 = CARTESIAN_POINT ( 'NONE',  ( 5.000000000001647571, -60.71953810597887014, 13.86359191440508809 ) ) ;
#24100 = DIRECTION ( 'NONE',  ( -1.000000000000000000, -1.224606353822377258E-16, -0.000000000000000000 ) ) ;
#24102 = ORIENTED_EDGE ( 'NONE', *, *, #36833, .F. ) ;
#24103 = B_SPLINE_CURVE_WITH_KNOTS ( 'NONE', 3,
 ( #36724, #94401, #78196, #62046 ),
 .UNSPECIFIED., .F., .F.,
 ( 4, 4 ),
 ( 2.693015029076737962E-17, 0.0002092826938343774910 ),
 .UNSPECIFIED. ) ;
#24104 = SURFACE_STYLE_FILL_AREA ( #18125 ) ;
#24105 = CARTESIAN_POINT ( 'NONE',  ( -9.499937800619317585, -5.000000000000002665, -20.18737470931643685 ) ) ;
#24106 = CARTESIAN_POINT ( 'NONE',  ( 15.50701386016346817, 34.82701475167880290, 23.25392551490321225 ) ) ;
#24107 =( GEOMETRIC_REPRESENTATION_CONTEXT ( 3 ) GLOBAL_UNCERTAINTY_ASSIGNED_CONTEXT ( ( #5413 ) ) GLOBAL_UNIT_ASSIGNED_CONTEXT ( ( #8374, #88778, #80664 ) ) REPRESENTATION_CONTEXT ( 'NONE', 'WORKASPACE' ) );
#24108 = CARTESIAN_POINT ( 'NONE',  ( 34.64323721803893363, 301.0516837800478811, -8.606392057058632972 ) ) ;
#24109 = CARTESIAN_POINT ( 'NONE',  ( 4.781335833249817036, -47.33012453287044252, 102.4226025779373259 ) ) ;
#24110 = CARTESIAN_POINT ( 'NONE',  ( -7.045755811259133417, -83.69658396986446292, 3.790843699961855773 ) ) ;
#24111 = CARTESIAN_POINT ( 'NONE',  ( 59.47617687438206957, -60.00000000000000000, 98.79634657976947665 ) ) ;
#24112 = EDGE_CURVE ( 'NONE', #67995, #29093, #17395, .T. ) ;
#24113 = CARTESIAN_POINT ( 'NONE',  ( -32.11411341898570981, 317.7919323371296514, -6.873671351699469412 ) ) ;
#24114 = ORIENTED_EDGE ( 'NONE', *, *, #41556, .F. ) ;
#24115 = CARTESIAN_POINT ( 'NONE',  ( 0.3465236330453798641, -30.00000000000000711, 7.243121741510847755 ) ) ;
#24116 = CARTESIAN_POINT ( 'NONE',  ( 52.56483885390523625, 48.00000000000000000, -38.23529411764706509 ) ) ;
#24117 = CARTESIAN_POINT ( 'NONE',  ( -43.67170302692484540, 434.9885551707871514, 18.57290719901140363 ) ) ;
#24119 = CARTESIAN_POINT ( 'NONE',  ( 0.000000000000000000, 0.000000000000000000, 0.000000000000000000 ) ) ;
#24118 = CARTESIAN_POINT ( 'NONE',  ( 48.02079947780210745, -30.00000000000000711, 60.50169175835635826 ) ) ;
#24120 = CARTESIAN_POINT ( 'NONE',  ( 54.03872891708841308, 6.856755485862130937E-15, 0.000000000000000000 ) ) ;
#24121 = EDGE_CURVE ( 'NONE', #6722, #10424, #82425, .T. ) ;
#24122 = CARTESIAN_POINT ( 'NONE',  ( -4.586789253316293724, -2.224716758486289692, 102.5764008378948091 ) ) ;
#24123 = ORIENTED_EDGE ( 'NONE', *, *, #95248, .F. ) ;
#24124 = CARTESIAN_POINT ( 'NONE',  ( -21.28260013279781759, 304.0447176871748525, 9.978225629331577196 ) ) ;
#24125 = ORIENTED_EDGE ( 'NONE', *, *, #35422, .F. ) ;
#24126 = CARTESIAN_POINT ( 'NONE',  ( 37.82041704037612107, 485.6919130818703252, -4.511470998796305309 ) ) ;
#24127 = FILL_AREA_STYLE ('',( #33267 ) ) ;
#24128 = LINE ( 'NONE', #61121, #25121 ) ;
#24129 = CARTESIAN_POINT ( 'NONE',  ( 5.656854249492380582, -12.50000000409676915, -5.656854249492379694 ) ) ;
#24131 = EDGE_CURVE ( 'NONE', #25935, #80162, #51450, .T. ) ;
#24130 = ORIENTED_EDGE ( 'NONE', *, *, #52543, .F. ) ;
#24132 = CARTESIAN_POINT ( 'NONE',  ( 60.62677696744211175, 49.99999999997998401, 24.18439665018642870 ) ) ;
#24133 = CARTESIAN_POINT ( 'NONE',  ( -8.629057352428841199, 6.505111962821877647, -3.764883966312650987 ) ) ;
#24134 = COLOUR_RGB ( '', 0.08235294, 0.09019608, 0.10196078) ;
#24135 = CARTESIAN_POINT ( 'NONE',  ( -66.01181427793642342, -59.99999999999997868, 132.9137452780753392 ) ) ;
#24136 = CARTESIAN_POINT ( 'NONE',  ( 1.102182119232617714E-15, -14.49999999999999822, 9.000000000000000000 ) ) ;
#24137 = AXIS2_PLACEMENT_3D ( 'NONE', #84935, #4018, #11023 ) ;
#24138 = CARTESIAN_POINT ( 'NONE',  ( 74.66296238351618797, -59.99999999999997868, 178.6152739014907525 ) ) ;
#24140 = CARTESIAN_POINT ( 'NONE',  ( 17.95348893241579091, -42.95395786364728963, 31.37188985704841215 ) ) ;
#24139 = CARTESIAN_POINT ( 'NONE',  ( -106.7878682580589071, -14.21045842199432663, 165.8353880188381027 ) ) ;
#24142 = CARTESIAN_POINT ( 'NONE',  ( 98.86178962493093536, -37.99999999999999289, 192.0563723494719568 ) ) ;
#24141 = UNCERTAINTY_MEASURE_WITH_UNIT (LENGTH_MEASURE( 1.000000000000000082E-05 ), #56916, 'distance_accuracy_value', 'NONE');
#24143 = STYLED_ITEM ( 'NONE', ( #65705 ), #34024 ) ;
#24144 = CARTESIAN_POINT ( 'NONE',  ( -46.29616362358941473, -39.53031546193722079, 45.26312817876173966 ) ) ;
#24145 = CARTESIAN_POINT ( 'NONE',  ( -0.6471460804167578074, 34.23036685099703647, -29.58265817172704004 ) ) ;
#24146 = EDGE_LOOP ( 'NONE', ( #20485, #37850, #79563, #89633, #82590 ) ) ;
#24147 = SURFACE_SIDE_STYLE ('',( #8449 ) ) ;
#24148 = CARTESIAN_POINT ( 'NONE',  ( 16.11155731264993918, 21.67754735133535249, -1.749455090942883206 ) ) ;
#24149 = CARTESIAN_POINT ( 'NONE',  ( 6.022743854525181462, -12.63762613047081196, 12.76172509297427027 ) ) ;
#24150 = FACE_OUTER_BOUND ( 'NONE', #18820, .T. ) ;
#24151 = STYLED_ITEM ( 'NONE', ( #83012 ), #32759 ) ;
#24152 = CARTESIAN_POINT ( 'NONE',  ( 21.23684446602550935, 304.9566545053270943, -9.977713076987674512 ) ) ;
#24153 = ORIENTED_EDGE ( 'NONE', *, *, #84683, .F. ) ;
#24154 = CARTESIAN_POINT ( 'NONE',  ( 5.437321008177347537, -47.65716784822890162, 104.0362115404844729 ) ) ;
#24155 = ORIENTED_EDGE ( 'NONE', *, *, #4678, .F. ) ;
#24156 = CARTESIAN_POINT ( 'NONE',  ( 102.2769841588865205, -30.00000000001111999, 197.9840571922390779 ) ) ;
#24157 = CARTESIAN_POINT ( 'NONE',  ( 23.52347158108310410, 41.65284174216176893, -74.94888205883640353 ) ) ;
#24158 = DIRECTION ( 'NONE',  ( 0.000000000000000000, 1.000000000000000000, 0.000000000000000000 ) ) ;
#24159 = CARTESIAN_POINT ( 'NONE',  ( 100.5419430498661768, -30.00000000000000000, 159.7472965000894192 ) ) ;
#24160 = AXIS2_PLACEMENT_3D ( 'NONE', #62992, #5287, #96941 ) ;
#24161 = EDGE_CURVE ( 'NONE', #76835, #70900, #9747, .T. ) ;
#24162 = CARTESIAN_POINT ( 'NONE',  ( 7.412906595240166041, 102.3581172714774539, 3.014362223629233561 ) ) ;
#24163 = ORIENTED_EDGE ( 'NONE', *, *, #100161, .F. ) ;
#24164 = VECTOR ( 'NONE', #68083, 1000.000000000000000 ) ;
#24165 = ORIENTED_EDGE ( 'NONE', *, *, #84381, .F. ) ;
#24166 = ORIENTED_EDGE ( 'NONE', *, *, #21263, .T. ) ;
#24167 = DIRECTION ( 'NONE',  ( 0.000000000000000000, 0.000000000000000000, 1.000000000000000000 ) ) ;
#24168 = CARTESIAN_POINT ( 'NONE',  ( -4.966176470918028052, 41.64999999999999147, -70.47555194646973575 ) ) ;
#24169 = CARTESIAN_POINT ( 'NONE',  ( -43.00000000000000000, 464.8825480873695710, 15.07585856869431851 ) ) ;
#24170 = EDGE_CURVE ( 'NONE', #81655, #66436, #14210, .T. ) ;
#24171 = ORIENTED_EDGE ( 'NONE', *, *, #79828, .F. ) ;
#24172 = CARTESIAN_POINT ( 'NONE',  ( 43.38684324084172772, 436.1115529209311603, 18.84450155852645636 ) ) ;
#24173 =( GEOMETRIC_REPRESENTATION_CONTEXT ( 3 ) GLOBAL_UNCERTAINTY_ASSIGNED_CONTEXT ( ( #49412 ) ) GLOBAL_UNIT_ASSIGNED_CONTEXT ( ( #95760, #21369, #63413 ) ) REPRESENTATION_CONTEXT ( 'NONE', 'WORKASPACE' ) );
#24174 = EDGE_LOOP ( 'NONE', ( #102724, #74943, #89158, #67615, #2451 ) ) ;
#24175 = DIRECTION ( 'NONE',  ( 0.000000000000000000, 1.000000000000000000, 0.000000000000000000 ) ) ;
#24176 = CARTESIAN_POINT ( 'NONE',  ( 81.61186971388572431, -38.84191813924242354, 195.4159226793195216 ) ) ;
#24177 = CARTESIAN_POINT ( 'NONE',  ( 13.47222701196340466, 5.364671514323175572, 6.505800345027190623 ) ) ;
#24178 = CARTESIAN_POINT ( 'NONE',  ( 36.39978974708674997, 309.1571451204594041, 13.35031817374169805 ) ) ;
#24179 = CARTESIAN_POINT ( 'NONE',  ( -7.000000000000000000, 8.572527594031471218E-16, -11.82492182392400437 ) ) ;
#24180 = AXIS2_PLACEMENT_3D ( 'NONE', #70385, #96264, #78995 ) ;
#24181 = CARTESIAN_POINT ( 'NONE',  ( 13.09999999999999787, 3.309500000000003439, 0.000000000000000000 ) ) ;
#24182 = CARTESIAN_POINT ( 'NONE',  ( -27.42168344121066426, 34.64432298653954945, -7.587308281121087461 ) ) ;
#24183 = CARTESIAN_POINT ( 'NONE',  ( -4.551587301587289858, -48.79941684889506348, 104.4018401814738013 ) ) ;
#24184 = DIRECTION ( 'NONE',  ( -0.000000000000000000, -0.000000000000000000, -1.000000000000000000 ) ) ;
#24185 = DIRECTION ( 'NONE',  ( 0.000000000000000000, 0.000000000000000000, -1.000000000000000000 ) ) ;
#24186 = EDGE_LOOP ( 'NONE', ( #90789, #26175, #84489, #70840 ) ) ;
#24187 = CARTESIAN_POINT ( 'NONE',  ( 1.234146493305849468, -49.99999999999999289, 101.3393031322932245 ) ) ;
#24188 = CARTESIAN_POINT ( 'NONE',  ( -22.15408181022044687, 295.0131836217579462, 1.971301972191277896 ) ) ;
#24189 = DIRECTION ( 'NONE',  ( 0.000000000000000000, 0.000000000000000000, -1.000000000000000000 ) ) ;
#24190 = DIRECTION ( 'NONE',  ( 0.000000000000000000, 0.000000000000000000, -1.000000000000000000 ) ) ;
#24191 = CARTESIAN_POINT ( 'NONE',  ( 7.999999999999998224, -14.09374999999999112, 3.313708498984766493 ) ) ;
#24192 = CARTESIAN_POINT ( 'NONE',  ( 17.36848429690531859, -24.01528219279489917, 36.27201406405939821 ) ) ;
#24193 = CIRCLE ( 'NONE', #70662, 7.500000000000006217 ) ;
#24194 = CARTESIAN_POINT ( 'NONE',  ( -5.000000000000000000, 0.000000000000000000, -1.446714285714285841 ) ) ;
#24195 = ORIENTED_EDGE ( 'NONE', *, *, #88646, .F. ) ;
#24196 = CARTESIAN_POINT ( 'NONE',  ( 85.22412109468345420, -42.93386880055312815, 186.3705244525062028 ) ) ;
#24197 = CARTESIAN_POINT ( 'NONE',  ( 3.826949319562312102, 16.00000000000000000, -9.246271506234595705 ) ) ;
#24198 = DIRECTION ( 'NONE',  ( 0.8257009859295948440, 0.000000000000000000, -0.5641080409238066196 ) ) ;
#24199 = EDGE_LOOP ( 'NONE', ( #105795, #8824, #128, #63445 ) ) ;
#24200 = CARTESIAN_POINT ( 'NONE',  ( 82.30040181591539294, -57.67111186717970384, -28.85252992913370917 ) ) ;
#24201 = CARTESIAN_POINT ( 'NONE',  ( 36.28420329445040693, 437.5777248398098891, 4.256696328373720917 ) ) ;
#24202 = CARTESIAN_POINT ( 'NONE',  ( 29.68315524077034340, 8.302504244945382084, 42.10535821593451544 ) ) ;
#24203 = CARTESIAN_POINT ( 'NONE',  ( -81.42887515339373294, -30.00000000000000355, -2.436421276796028934 ) ) ;
#24204 = EDGE_CURVE ( 'NONE', #91446, #67548, #69136, .T. ) ;
#24205 = AXIS2_PLACEMENT_3D ( 'NONE', #18984, #101978, #87932 ) ;
#24206 = CARTESIAN_POINT ( 'NONE',  ( 29.14590962570505894, 18.82625154611909934, 39.72466805691946234 ) ) ;
#24207 = CARTESIAN_POINT ( 'NONE',  ( -10.00000000000000000, -5.000000000000000000, 2.617993873628187806 ) ) ;
#24208 = DIRECTION ( 'NONE',  ( -1.000000000000000000, -0.000000000000000000, -0.000000000000000000 ) ) ;
#24209 = EDGE_CURVE ( 'NONE', #84434, #62970, #7972, .T. ) ;
#24211 = FACE_OUTER_BOUND ( 'NONE', #29233, .T. ) ;
#24210 = VECTOR ( 'NONE', #59086, 1000.000000000000000 ) ;
#24212 =( LENGTH_UNIT ( ) NAMED_UNIT ( * ) SI_UNIT ( .MILLI., .METRE. ) );
#24213 = CARTESIAN_POINT ( 'NONE',  ( -28.49074715056200802, 18.29855530143744602, 40.46824935483533636 ) ) ;
#24214 = CARTESIAN_POINT ( 'NONE',  ( -12.50000000000000711, -3.000000000000000000, -78.42624373368740009 ) ) ;
#24215 = CARTESIAN_POINT ( 'NONE',  ( 11.69538631874852186, -5.000000000000000000, -81.87730495800397534 ) ) ;
#24216 = CARTESIAN_POINT ( 'NONE',  ( -2.499999999981197707, -21.99834632368703069, -30.53960193249073640 ) ) ;
#24217 = DIRECTION ( 'NONE',  ( -0.000000000000000000, -1.000000000000000000, -0.000000000000000000 ) ) ;
#24218 = CARTESIAN_POINT ( 'NONE',  ( 70.74177944523411554, -29.99609282501852192, -20.32620075006109062 ) ) ;
#24219 = STYLED_ITEM ( 'NONE', ( #68183 ), #81053 ) ;
#24220 = ORIENTED_EDGE ( 'NONE', *, *, #100305, .T. ) ;
#24221 = CARTESIAN_POINT ( 'NONE',  ( 6.222742520105472686, -3.584500230190552639, -6.791463481567640237 ) ) ;
#24222 = CYLINDRICAL_SURFACE ( 'NONE', #84865, 1.250000000000001110 ) ;
#24223 = CARTESIAN_POINT ( 'NONE',  ( -7.046357527897574968, 83.69384349398994516, -3.789683693877208270 ) ) ;
#24224 = CARTESIAN_POINT ( 'NONE',  ( 4.658465013329192494, -63.67636120326903892, 3.783534922165392000 ) ) ;
#24225 = CONICAL_SURFACE ( 'NONE', #17287, 3.309500000000001663, 0.9599310885968770357 ) ;
#24227 = CARTESIAN_POINT ( 'NONE',  ( -63.53617277140842390, -34.58942015808621306, -24.20806359249350592 ) ) ;
#24226 = CARTESIAN_POINT ( 'NONE',  ( 7.770228158362351145, 6.123233995736769241E-16, -5.000000000000002665 ) ) ;
#24228 = ORIENTED_EDGE ( 'NONE', *, *, #66298, .T. ) ;
#24229 = VECTOR ( 'NONE', #51886, 1000.000000000000000 ) ;
#24230 = ORIENTED_EDGE ( 'NONE', *, *, #63694, .F. ) ;
#24231 = LINE ( 'NONE', #9062, #86217 ) ;
#24232 = CARTESIAN_POINT ( 'NONE',  ( -4.903509839974908857, -29.96764154726693974, -6.410198659009853195 ) ) ;
#24233 = AXIS2_PLACEMENT_3D ( 'NONE', #70826, #70299, #103196 ) ;
#24234 = FACE_OUTER_BOUND ( 'NONE', #90721, .T. ) ;
#24235 = CARTESIAN_POINT ( 'NONE',  ( -49.94482164224617549, -59.99999999999999289, -37.91551347345771461 ) ) ;
#24236 = ORIENTED_EDGE ( 'NONE', *, *, #32464, .T. ) ;
#24237 = LINE ( 'NONE', #64664, #46352 ) ;
#24238 = DIRECTION ( 'NONE',  ( 1.000000000000000000, 1.224606353822377258E-16, 0.000000000000000000 ) ) ;
#24239 = CARTESIAN_POINT ( 'NONE',  ( 96.57334640236589962, -45.27060142599663095, 194.0782599365211922 ) ) ;
#24241 = CARTESIAN_POINT ( 'NONE',  ( 13.58349330513380515, -4.000000000000000888, 4.898587196589416773E-16 ) ) ;
#24240 = CARTESIAN_POINT ( 'NONE',  ( 8.929771841637641927, 1.482358050883964840E-15, 0.000000000000000000 ) ) ;
#24242 = AXIS2_PLACEMENT_3D ( 'NONE', #13453, #89489, #47937 ) ;
#24243 = ORIENTED_EDGE ( 'NONE', *, *, #101460, .T. ) ;
#24244 = B_SPLINE_CURVE_WITH_KNOTS ( 'NONE', 3,
 ( #79123, #88813, #80176, #23041 ),
 .UNSPECIFIED., .F., .F.,
 ( 4, 4 ),
 ( 0.02698643027831515440, 0.9670246242088337274 ),
 .UNSPECIFIED. ) ;
#24245 = ORIENTED_EDGE ( 'NONE', *, *, #51210, .T. ) ;
#24246 = ORIENTED_EDGE ( 'NONE', *, *, #16901, .T. ) ;
#24247 = CARTESIAN_POINT ( 'NONE',  ( 31.04372800095298501, 362.9570874249782833, 22.40737358240867749 ) ) ;
#24248 = CARTESIAN_POINT ( 'NONE',  ( -4.999999999999960032, -13.35938963217072128, 12.71467713436390667 ) ) ;
#24249 = DIRECTION ( 'NONE',  ( -0.000000000000000000, 1.000000000000000000, 0.000000000000000000 ) ) ;
#24251 = EDGE_CURVE ( 'NONE', #54847, #68971, #70182, .T. ) ;
#24250 = VERTEX_POINT ( 'NONE', #101491 ) ;
#24252 = CARTESIAN_POINT ( 'NONE',  ( -42.19618372163387221, 487.7264399052799604, 8.629926728122912394 ) ) ;
#24253 = CARTESIAN_POINT ( 'NONE',  ( -121.1901574356003408, 4.501353321498349658, -60.59507871780017751 ) ) ;
#24254 = CARTESIAN_POINT ( 'NONE',  ( -32.81992448453860334, 465.7192846569213884, 11.17271167765305862 ) ) ;
#24255 = CARTESIAN_POINT ( 'NONE',  ( -27.27894591530610668, -57.67773572996152609, 43.94474244872281332 ) ) ;
#24256 = CARTESIAN_POINT ( 'NONE',  ( 5.082755093536324154, -29.84375000204838813, 5.082755093536326818 ) ) ;
#24257 = CARTESIAN_POINT ( 'NONE',  ( 4.733165431326070832E-26, 13.70447791526910919, -49.25000000000000000 ) ) ;
#24258 = CARTESIAN_POINT ( 'NONE',  ( 20.00000000000000000, 12.99999999999999467, -7.500000000000000000 ) ) ;
#24259 = DIRECTION ( 'NONE',  ( -0.000000000000000000, 0.8660254037844387076, 0.4999999999999999445 ) ) ;
#24260 = CARTESIAN_POINT ( 'NONE',  ( -17.09952670627316706, -60.00000000000001421, -44.43607591113852351 ) ) ;
#24261 = CARTESIAN_POINT ( 'NONE',  ( 30.11650669486618881, 1.474610560812782335E-15, 0.000000000000000000 ) ) ;
#24262 = CARTESIAN_POINT ( 'NONE',  ( -53.08102895155478507, -18.70615072099417731, 48.69294712436818884 ) ) ;
#24263 = CIRCLE ( 'NONE', #3533, 2.000000000000011102 ) ;
#24264 = DIRECTION ( 'NONE',  ( 1.000000000000000000, 1.224606353822377258E-16, 0.000000000000000000 ) ) ;
#24265 = ORIENTED_EDGE ( 'NONE', *, *, #2268, .F. ) ;
#24266 = CARTESIAN_POINT ( 'NONE',  ( -99.29599809189417670, -45.25123437682626104, 193.1448974876303168 ) ) ;
#24267 = CARTESIAN_POINT ( 'NONE',  ( -4.598202642515742511, 296.0917469169227729, -10.00877229851206707 ) ) ;
#24268 = VERTEX_POINT ( 'NONE', #93406 ) ;
#24269 = CARTESIAN_POINT ( 'NONE',  ( -34.47678062873981020, 437.1474145881089157, 5.468662283310369077 ) ) ;
#24270 = CARTESIAN_POINT ( 'NONE',  ( 90.59251118385301993, -38.35027144420563161, 14.22736211764586223 ) ) ;
#24271 = CARTESIAN_POINT ( 'NONE',  ( 58.92761780597729881, 4.898587196589294500E-16, -4.000000000000007105 ) ) ;
#24272 = CARTESIAN_POINT ( 'NONE',  ( -7.188101187500000044, -9.781250002048384573, -8.802885111219163269E-16 ) ) ;
#24273 = CARTESIAN_POINT ( 'NONE',  ( -7.218639321055465352, 294.7245701161654665, 9.909955229536505428 ) ) ;
#24274 = DIRECTION ( 'NONE',  ( 0.000000000000000000, 0.000000000000000000, 1.000000000000000000 ) ) ;
#24275 = CARTESIAN_POINT ( 'NONE',  ( 81.12011883507125276, -30.00000000000000711, 140.6539142541519709 ) ) ;
#24276 = CARTESIAN_POINT ( 'NONE',  ( -10.36896828245630431, 43.24042510010813345, -15.40779740156158439 ) ) ;
#24277 = CARTESIAN_POINT ( 'NONE',  ( -29.49710045460171770, 13.37160745013286167, 39.61402429467839426 ) ) ;
#24278 = EDGE_CURVE ( 'NONE', #41862, #104941, #28849, .T. ) ;
#24279 = DIRECTION ( 'NONE',  ( -0.000000000000000000, -1.000000000000000000, -0.000000000000000000 ) ) ;
#24280 = AXIS2_PLACEMENT_3D ( 'NONE', #42020, #72782, #32897 ) ;
#24281 = EDGE_CURVE ( 'NONE', #80206, #82046, #32272, .T. ) ;
#24282 =( GEOMETRIC_REPRESENTATION_CONTEXT ( 3 ) GLOBAL_UNCERTAINTY_ASSIGNED_CONTEXT ( ( #86883 ) ) GLOBAL_UNIT_ASSIGNED_CONTEXT ( ( #92032, #96306, #102253 ) ) REPRESENTATION_CONTEXT ( 'NONE', 'WORKASPACE' ) );
#24283 = ORIENTED_EDGE ( 'NONE', *, *, #50056, .T. ) ;
#24284 = ORIENTED_EDGE ( 'NONE', *, *, #58934, .F. ) ;
#24285 = CARTESIAN_POINT ( 'NONE',  ( 50.52250052960007309, -25.65762928410081400, 46.96345956391975562 ) ) ;
#24286 = DIRECTION ( 'NONE',  ( 0.000000000000000000, -1.000000000000000000, 0.000000000000000000 ) ) ;
#24287 = CARTESIAN_POINT ( 'NONE',  ( 37.56673239365841255, 27.60449318992554169, -13.45617127781092215 ) ) ;
#24288 = EDGE_CURVE ( 'NONE', #86829, #51816, #21660, .T. ) ;
#24289 = ORIENTED_EDGE ( 'NONE', *, *, #79603, .T. ) ;
#24290 = CARTESIAN_POINT ( 'NONE',  ( -107.9473917804004941, -38.35630723407592768, 137.4504611278363768 ) ) ;
#24291 = EDGE_LOOP ( 'NONE', ( #67819, #46767, #16588, #13062 ) ) ;
#24292 = CARTESIAN_POINT ( 'NONE',  ( 45.11650669486618881, 1.474610560812782335E-15, 0.000000000000000000 ) ) ;
#24293 = CARTESIAN_POINT ( 'NONE',  ( 90.86173999633324172, -38.35175481737118020, 20.64625151213274989 ) ) ;
#24294 = CARTESIAN_POINT ( 'NONE',  ( 11.69764828795528011, 11.66347120412247662, -9.914309509057556369 ) ) ;
#24295 = CARTESIAN_POINT ( 'NONE',  ( -6.615709386635189482, 303.7455146892042421, 9.914404184983467871 ) ) ;
#24296 = CARTESIAN_POINT ( 'NONE',  ( 98.65904876352816189, -37.84861505694159689, 130.4062528344186944 ) ) ;
#24297 = CARTESIAN_POINT ( 'NONE',  ( -31.81126046617210434, 439.4148073498083704, 23.49515931950221059 ) ) ;
#24298 =( NAMED_UNIT ( * ) PLANE_ANGLE_UNIT ( ) SI_UNIT ( $, .RADIAN. ) );
#24299 = CARTESIAN_POINT ( 'NONE',  ( -29.30744343150515618, 310.6405753734469499, -7.659872152243718979 ) ) ;
#24300 = CARTESIAN_POINT ( 'NONE',  ( 3.958819230456402050, -67.57662422979727523, 13.13288867614480182 ) ) ;
#24301 = CARTESIAN_POINT ( 'NONE',  ( 74.37097096341283020, -59.99999999999999289, 175.8909987187326749 ) ) ;
#24302 = VECTOR ( 'NONE', #21190, 1000.000000000000000 ) ;
#24304 = ADVANCED_FACE ( 'NONE', ( #61044 ), #61534, .T. ) ;
#24303 = AXIS2_PLACEMENT_3D ( 'NONE', #65401, #98293, #15250 ) ;
#24305 = CARTESIAN_POINT ( 'NONE',  ( 17.60394295411769150, 45.00000000000001421, 63.08992194734121028 ) ) ;
#24306 = CIRCLE ( 'NONE', #48350, 14.78272384904389192 ) ;
#24307 = ORIENTED_EDGE ( 'NONE', *, *, #28464, .F. ) ;
#24308 = CARTESIAN_POINT ( 'NONE',  ( 57.60575626135791083, -18.66803500383183589, 57.28382109102082609 ) ) ;
#24309 = CARTESIAN_POINT ( 'NONE',  ( -21.29121868248358851, 302.9472852280009079, -9.979704577517333419 ) ) ;
#24310 = CARTESIAN_POINT ( 'NONE',  ( 6.849999999999999645, 0.000000000000000000, 0.000000000000000000 ) ) ;
#24311 = CARTESIAN_POINT ( 'NONE',  ( -8.878109361141049760, -5.000000000000000000, -17.03646273725755833 ) ) ;
#24312 = AXIS2_PLACEMENT_3D ( 'NONE', #53765, #12761, #38661 ) ;
#24314 = DIRECTION ( 'NONE',  ( 0.000000000000000000, 0.000000000000000000, -1.000000000000000000 ) ) ;
#24313 = CARTESIAN_POINT ( 'NONE',  ( -77.55597287852873478, -29.99999999981872989, 179.8129485814087900 ) ) ;
#24315 = DIRECTION ( 'NONE',  ( -1.000000000000000000, -1.224606353822377258E-16, -0.000000000000000000 ) ) ;
#24316 = CARTESIAN_POINT ( 'NONE',  ( 31.38879778682737154, 374.5724854738020326, 22.86450524640430615 ) ) ;
#24317 = FACE_OUTER_BOUND ( 'NONE', #92576, .T. ) ;
#24318 = CARTESIAN_POINT ( 'NONE',  ( -1.469576158976823947E-15, -32.37499999999999289, 8.000000000000000000 ) ) ;
#24319 = CARTESIAN_POINT ( 'NONE',  ( 11.08349330513380515, -3.851859888774471706E-31, 4.000000000000001776 ) ) ;
#24320 = STYLED_ITEM ( 'NONE', ( #15050 ), #19158 ) ;
#24321 = CIRCLE ( 'NONE', #56987, 4.000000000000001776 ) ;
#24322 = DIRECTION ( 'NONE',  ( -1.000000000000000000, -1.224606353822377258E-16, -0.000000000000000000 ) ) ;
#24323 = VERTEX_POINT ( 'NONE', #55036 ) ;
#24324 = CARTESIAN_POINT ( 'NONE',  ( 83.30572369024382340, -42.97726960787509398, 177.5867044128110592 ) ) ;
#24325 = CARTESIAN_POINT ( 'NONE',  ( 0.000000000000000000, 0.000000000000000000, 4.000000000000000888 ) ) ;
#24326 = CARTESIAN_POINT ( 'NONE',  ( 4.898587196589412829E-16, -9.312500004096769146, -8.000000000000000000 ) ) ;
#24327 = EDGE_LOOP ( 'NONE', ( #102925, #83103, #100579, #8533, #29293 ) ) ;
#24328 = DIRECTION ( 'NONE',  ( -1.000000000000000000, 0.000000000000000000, 0.000000000000000000 ) ) ;
#24329 = CARTESIAN_POINT ( 'NONE',  ( 6.735051087778345824, -4.346205982510036314, -16.86563398496271660 ) ) ;
#24330 = FACE_OUTER_BOUND ( 'NONE', #96446, .T. ) ;
#24331 = CARTESIAN_POINT ( 'NONE',  ( 14.24907788157470634, 2.189443139869392763, 4.658781708031014546 ) ) ;
#24332 = DIRECTION ( 'NONE',  ( 0.000000000000000000, 0.000000000000000000, 1.000000000000000000 ) ) ;
#24333 = FACE_OUTER_BOUND ( 'NONE', #41251, .T. ) ;
#24334 = ADVANCED_FACE ( 'NONE', ( #5447 ), #104614, .F. ) ;
#24335 = VECTOR ( 'NONE', #15171, 1000.000000000000227 ) ;
#24336 = CONICAL_SURFACE ( 'NONE', #62223, 4.000000000000001776, 0.9599310885968774798 ) ;
#24337 = CARTESIAN_POINT ( 'NONE',  ( 7.414580834929599185, 107.6465628028148132, 3.010264818013836940 ) ) ;
#24338 = CARTESIAN_POINT ( 'NONE',  ( 4.142849616820253082E-15, 32.68727484027578356, 33.82893434829263413 ) ) ;
#24339 = EDGE_CURVE ( 'NONE', #47025, #102776, #90847, .T. ) ;
#24340 = ADVANCED_FACE ( 'NONE', ( #89022 ), #87968, .T. ) ;
#24342 = CARTESIAN_POINT ( 'NONE',  ( -10.93723481929648678, 16.61273572670358689, -9.331603509320386181 ) ) ;
#24341 = CARTESIAN_POINT ( 'NONE',  ( -27.09524894485997493, -30.47611868180892003, 39.10809118615605939 ) ) ;
#24343 = AXIS2_PLACEMENT_3D ( 'NONE', #55421, #88354, #14430 ) ;
#24344 = CARTESIAN_POINT ( 'NONE',  ( -7.188101187500001821, -15.50000000204838635, -2.977408999572651371 ) ) ;
#24345 = CARTESIAN_POINT ( 'NONE',  ( -56.06921707446602454, 40.83906611473297232, -33.41757057980472467 ) ) ;
#24346 = FACE_OUTER_BOUND ( 'NONE', #103085, .T. ) ;
#24347 = EDGE_LOOP ( 'NONE', ( #66022, #98353 ) ) ;
#24348 = CARTESIAN_POINT ( 'NONE',  ( -17.49999999999918643, 49.99999999999941025, 59.71562975593359113 ) ) ;
#24349 = CARTESIAN_POINT ( 'NONE',  ( 24.45707236316964384, 25.45848949702577713, 31.59252836779057816 ) ) ;
#24350 = CARTESIAN_POINT ( 'NONE',  ( -3.739146603194685614, 132.2511161815098149, -5.000000000000002665 ) ) ;
#24351 = DIRECTION ( 'NONE',  ( 0.000000000000000000, 0.000000000000000000, 1.000000000000000000 ) ) ;
#24352 = CARTESIAN_POINT ( 'NONE',  ( 4.044804397649282457, 54.03507251708755632, 7.474846107636844650 ) ) ;
#24353 = EDGE_CURVE ( 'NONE', #102768, #88573, #16766, .T. ) ;
#24354 = CIRCLE ( 'NONE', #79450, 2.000000000000001332 ) ;
#24355 = ORIENTED_EDGE ( 'NONE', *, *, #37468, .F. ) ;
#24356 = CARTESIAN_POINT ( 'NONE',  ( 11.40992495151485464, 13.86395319139118243, -9.971698466393837279 ) ) ;
#24357 = CARTESIAN_POINT ( 'NONE',  ( 29.83349330513380337, -7.703719777548943412E-31, 4.000000000000001776 ) ) ;
#24358 = ORIENTED_EDGE ( 'NONE', *, *, #38802, .F. ) ;
#24359 = EDGE_CURVE ( 'NONE', #81976, #64080, #68452, .T. ) ;
#24360 = CARTESIAN_POINT ( 'NONE',  ( -2.499999999999978684, -29.99999999999999645, 28.88619816519791073 ) ) ;
#24361 = CARTESIAN_POINT ( 'NONE',  ( -19.99877541361295741, 41.84885527536232530, -79.71217436998914252 ) ) ;
#24362 = CARTESIAN_POINT ( 'NONE',  ( -102.3275229563159598, -60.00000000000000000, 94.65514192416549122 ) ) ;
#24363 = CARTESIAN_POINT ( 'NONE',  ( 29.07959870117736756, 18.85554092054059794, -39.75803059074604562 ) ) ;
#24364 = CARTESIAN_POINT ( 'NONE',  ( 3.215662123186951678E-05, -42.95772942492470747, 31.04927153042315524 ) ) ;
#24365 = CARTESIAN_POINT ( 'NONE',  ( 23.61963550967466574, 306.0340374937824777, 10.19690224617928287 ) ) ;
#24366 = CARTESIAN_POINT ( 'NONE',  ( -13.81782546013763024, 1.033440728989090340, 14.96496143817082647 ) ) ;
#24368 = CARTESIAN_POINT ( 'NONE',  ( 4.898587196589412829E-16, -27.12499999999999645, -8.000000000000000000 ) ) ;
#24367 = CARTESIAN_POINT ( 'NONE',  ( -1.308996937480704004, -4.999999999999988454, -95.00000000000001421 ) ) ;
#24369 = B_SPLINE_CURVE_WITH_KNOTS ( 'NONE', 3,
 ( #51399, #27173, #75134, #2308, #78209, #50333, #49810, #20575, #70121, #62060, #94949, #82715, #8819, #41723, #33652, #66532, #99405, #58446 ),
 .UNSPECIFIED., .F., .F.,
 ( 4, 2, 2, 2, 2, 2, 2, 2, 4 ),
 ( 0.000000000000000000, 0.06143467464390223176, 0.1228693492878044635, 0.2457386985756090381, 0.3686080478634136126, 0.4914773971512180761, 0.7372160957268271142, 0.8600854450146315777, 0.9829547943024361523 ),
 .UNSPECIFIED. ) ;
#24370 = CARTESIAN_POINT ( 'NONE',  ( -83.11698702663863969, -42.98028782721130625, 176.1582416638941027 ) ) ;
#24371 = ORIENTED_EDGE ( 'NONE', *, *, #85905, .T. ) ;
#24372 = CARTESIAN_POINT ( 'NONE',  ( 46.00000000000000000, 500.0000000000002274, 12.00000000000000711 ) ) ;
#24373 =( GEOMETRIC_REPRESENTATION_CONTEXT ( 3 ) GLOBAL_UNCERTAINTY_ASSIGNED_CONTEXT ( ( #69632 ) ) GLOBAL_UNIT_ASSIGNED_CONTEXT ( ( #56677, #83092, #16222 ) ) REPRESENTATION_CONTEXT ( 'NONE', 'WORKASPACE' ) );
#24374 = VECTOR ( 'NONE', #101243, 1000.000000000000000 ) ;
#24375 = ORIENTED_EDGE ( 'NONE', *, *, #96113, .T. ) ;
#24376 = MECHANICAL_DESIGN_GEOMETRIC_PRESENTATION_REPRESENTATION (  '', ( #209 ), #8786 ) ;
#24377 = ORIENTED_EDGE ( 'NONE', *, *, #70596, .T. ) ;
#24378 = CARTESIAN_POINT ( 'NONE',  ( 0.000000000000000000, 24.35682532067546902, 0.000000000000000000 ) ) ;
#24380 = B_SPLINE_CURVE_WITH_KNOTS ( 'NONE', 3,
 ( #54278, #14355, #13835, #47267, #104442, #87221, #95839, #55864, #30592, #4707, #39728, #80690, #63482, #6810, #80163, #72606, #13300, #38163 ),
 .UNSPECIFIED., .F., .F.,
 ( 4, 2, 2, 2, 2, 2, 2, 2, 4 ),
 ( 0.000000000000000000, 0.001407658255260105370, 0.002815316510520210740, 0.004222974765780315894, 0.005630633021040421481, 0.007038291276300527068, 0.008445949531560631787, 0.009853607786820737374, 0.01126126604208084296 ),
 .UNSPECIFIED. ) ;
#24379 = VECTOR ( 'NONE', #50052, 1000.000000000000000 ) ;
#24381 = CARTESIAN_POINT ( 'NONE',  ( -3.334877097134691049, 304.8518027755578146, 8.936999414895272054 ) ) ;
#24382 = CARTESIAN_POINT ( 'NONE',  ( 11.89131030317610183, -5.000000000000000000, 6.123233995736768255E-16 ) ) ;
#24383 = SURFACE_SIDE_STYLE ('',( #30881 ) ) ;
#24384 = CARTESIAN_POINT ( 'NONE',  ( 3.996301576407919498, 15.12269148464774737, -5.000000000000000000 ) ) ;
#24385 = CARTESIAN_POINT ( 'NONE',  ( 13.05360465724633912, -5.000000000000000000, -85.14609521163498584 ) ) ;
#24386 = DIRECTION ( 'NONE',  ( 0.8191520442889909104, 1.003171929053523637E-16, -0.5735764363510472696 ) ) ;
#24387 = PRESENTATION_LAYER_ASSIGNMENT (  '', '', ( #72551 ) ) ;
#24388 = CARTESIAN_POINT ( 'NONE',  ( 103.8765618273974951, -14.21045842199444209, 137.3601107225250360 ) ) ;
#24389 = EDGE_CURVE ( 'NONE', #942, #22409, #52963, .T. ) ;
#24390 = CIRCLE ( 'NONE', #53615, 4.000000000000000888 ) ;
#24391 = CARTESIAN_POINT ( 'NONE',  ( -105.4253011914250067, -14.21045842199428222, 149.5333493894512458 ) ) ;
#24392 = CARTESIAN_POINT ( 'NONE',  ( -63.57062938988862300, -36.00914355728743743, 80.26143161827371841 ) ) ;
#24393 = ORIENTED_EDGE ( 'NONE', *, *, #58112, .F. ) ;
#24394 = CARTESIAN_POINT ( 'NONE',  ( 0.06809871960542752956, 7.710219529346609590, -2.645508037661881584 ) ) ;
#24395 = CARTESIAN_POINT ( 'NONE',  ( 94.31441069461205018, -60.00000000001458744, 17.33446251183617903 ) ) ;
#24396 = ORIENTED_EDGE ( 'NONE', *, *, #19350, .T. ) ;
#24397 = CARTESIAN_POINT ( 'NONE',  ( 0.9846689345368905277, -18.58625483750316576, 26.98735909918624287 ) ) ;
#24398 = CARTESIAN_POINT ( 'NONE',  ( 2.977408999572650927, -16.25000000204838457, -7.188101187500000933 ) ) ;
#24399 = CARTESIAN_POINT ( 'NONE',  ( -7.758748231291408892, -5.000000000000000888, -73.00623724569611284 ) ) ;
#24400 = EDGE_LOOP ( 'NONE', ( #18689, #56233, #25292, #28862, #99186 ) ) ;
#24401 = CARTESIAN_POINT ( 'NONE',  ( -10.28624191511820207, 45.38549880562041494, 15.40779740156164124 ) ) ;
#24402 = EDGE_LOOP ( 'NONE', ( #68391, #14616, #85393, #35409, #29965 ) ) ;
#24403 = CARTESIAN_POINT ( 'NONE',  ( -5.600000207755308601, -12.35529564071044817, -1.068955579434926870E-14 ) ) ;
#24404 = CARTESIAN_POINT ( 'NONE',  ( 8.349999999999999645, 4.172000000000003261, 0.000000000000000000 ) ) ;
#24405 = CARTESIAN_POINT ( 'NONE',  ( -107.3823593786986095, -60.00000000000001421, 124.9939677557050430 ) ) ;
#24406 = FILL_AREA_STYLE ('',( #97709 ) ) ;
#24407 = CARTESIAN_POINT ( 'NONE',  ( -7.188101187500000044, -27.78125000204838813, -8.802885111219163269E-16 ) ) ;
#24408 = DIRECTION ( 'NONE',  ( -1.000000000000000000, -0.000000000000000000, -0.000000000000000000 ) ) ;
#24409 = CARTESIAN_POINT ( 'NONE',  ( 17.84534382768862670, 43.24938063751061890, -5.054370945579135466 ) ) ;
#24410 = CARTESIAN_POINT ( 'NONE',  ( 66.00571552735603120, -1.232595164407830946E-29, 4.000000000000007105 ) ) ;
#24411 = CARTESIAN_POINT ( 'NONE',  ( -11.03870218254165181, -4.986327171952302351, -12.57673782977023791 ) ) ;
#24412 = DIRECTION ( 'NONE',  ( 0.000000000000000000, 0.000000000000000000, 1.000000000000000000 ) ) ;
#24413 = CARTESIAN_POINT ( 'NONE',  ( 14.04065140978712911, -8.435331075557439107, 12.41598592279226310 ) ) ;
#24414 = CARTESIAN_POINT ( 'NONE',  ( -28.82368679149679025, 297.0884870745862258, -1.512235082149814946 ) ) ;
#24415 = EDGE_CURVE ( 'NONE', #38226, #9148, #13293, .T. ) ;
#24416 = CARTESIAN_POINT ( 'NONE',  ( 103.3323615576035195, -60.00000000000002132, 136.8515639484661790 ) ) ;
#24417 = CARTESIAN_POINT ( 'NONE',  ( -33.78495839492549635, -56.84029651377081649, 37.95014195405838109 ) ) ;
#24418 = TOROIDAL_SURFACE ( 'NONE', #29574, 9.000000000000000000, 0.5000000000000000000 ) ;
#24419 = EDGE_CURVE ( 'NONE', #74862, #15534, #4701, .T. ) ;
#24420 = CARTESIAN_POINT ( 'NONE',  ( -1.509171067930827448, -49.97508125504521814, 101.6143504438094283 ) ) ;
#24421 = CARTESIAN_POINT ( 'NONE',  ( 42.25895859003348676, -42.97903088149762851, 41.54068014075424742 ) ) ;
#24422 = CIRCLE ( 'NONE', #17465, 4.000000000000001776 ) ;
#24423 = DIRECTION ( 'NONE',  ( -0.000000000000000000, -0.000000000000000000, -1.000000000000000000 ) ) ;
#24424 = ORIENTED_EDGE ( 'NONE', *, *, #93899, .T. ) ;
#24425 = EDGE_CURVE ( 'NONE', #54801, #47728, #7024, .T. ) ;
#24426 = CARTESIAN_POINT ( 'NONE',  ( -6.928203230275510549, 85.00000000000000000, -4.000000000000000000 ) ) ;
#24427 = EDGE_CURVE ( 'NONE', #102845, #58869, #60679, .T. ) ;
#24428 = CIRCLE ( 'NONE', #53640, 4.172000000000009479 ) ;
#24429 = CARTESIAN_POINT ( 'NONE',  ( -81.13099867360766382, -38.83658557384262622, 194.7852543518826849 ) ) ;
#24430 = EDGE_LOOP ( 'NONE', ( #24673, #99861, #57031, #87611 ) ) ;
#24432 = CARTESIAN_POINT ( 'NONE',  ( 45.31383884518383098, 362.9196860876334085, 5.161789940898600548 ) ) ;
#24431 = CARTESIAN_POINT ( 'NONE',  ( 9.797174393178825657E-16, -30.00000000000000000, -8.000000000000000000 ) ) ;
#24433 = CARTESIAN_POINT ( 'NONE',  ( -12.29126969517217205, 22.30877634104236762, 6.406973025524664855 ) ) ;
#24434 = CYLINDRICAL_SURFACE ( 'NONE', #68215, 5.000000000000000888 ) ;
#24435 = DIRECTION ( 'NONE',  ( 0.000000000000000000, 0.000000000000000000, 1.000000000000000000 ) ) ;
#24436 = CARTESIAN_POINT ( 'NONE',  ( 0.000000000000000000, 1.000000000000000888, 0.000000000000000000 ) ) ;
#24437 = CARTESIAN_POINT ( 'NONE',  ( -39.20264847829642463, 436.8475545326365932, 5.145470557645624332 ) ) ;
#24438 = FACE_OUTER_BOUND ( 'NONE', #16397, .T. ) ;
#24439 = CARTESIAN_POINT ( 'NONE',  ( 17.39146662423151568, 45.59957931493300265, 4.393505531746607851 ) ) ;
#24440 = EDGE_CURVE ( 'NONE', #83314, #80759, #14993, .T. ) ;
#24441 = CARTESIAN_POINT ( 'NONE',  ( 110.0499776139819659, -59.99999999999999289, 143.8492112426671667 ) ) ;
#24442 = CARTESIAN_POINT ( 'NONE',  ( -2.404214652066591906, -53.72754880671013211, 40.79389177775365738 ) ) ;
#24443 = EDGE_CURVE ( 'NONE', #47515, #78613, #1412, .T. ) ;
#24444 = EDGE_CURVE ( 'NONE', #38628, #78066, #99444, .T. ) ;
#24445 = EDGE_LOOP ( 'NONE', ( #93399, #106636 ) ) ;
#24446 = CARTESIAN_POINT ( 'NONE',  ( -93.51384743021765189, -30.00000000000006040, 191.2118971003746708 ) ) ;
#24447 = EDGE_LOOP ( 'NONE', ( #77033, #98571, #35812, #87188, #103127, #46671 ) ) ;
#24448 = CARTESIAN_POINT ( 'NONE',  ( -3.347995242091437174, -48.90830061040438181, 104.4601902487057998 ) ) ;
#24449 = CARTESIAN_POINT ( 'NONE',  ( -15.93262767509097877, 3.183098147201662176, -1.443311391221110407 ) ) ;
#24450 =( NAMED_UNIT ( * ) PLANE_ANGLE_UNIT ( ) SI_UNIT ( $, .RADIAN. ) );
#24451 = LINE ( 'NONE', #89683, #81152 ) ;
#24452 = CARTESIAN_POINT ( 'NONE',  ( 9.165151389911681434, 30.00000000000000000, -4.000000000000000000 ) ) ;
#24453 = CARTESIAN_POINT ( 'NONE',  ( 7.188101187500001821, -25.43750000204838813, -2.977408999572650483 ) ) ;
#24454 = DIRECTION ( 'NONE',  ( -1.000000000000000000, -1.224606353822377258E-16, -0.000000000000000000 ) ) ;
#24455 = CARTESIAN_POINT ( 'NONE',  ( 7.326726166330386647, 41.40616545424374806, -69.28044400771726430 ) ) ;
#24456 = VERTEX_POINT ( 'NONE', #79328 ) ;
#24458 = ORIENTED_EDGE ( 'NONE', *, *, #104411, .T. ) ;
#24457 = CARTESIAN_POINT ( 'NONE',  ( 4.861072549008416566, -2.920843450830509891, 102.3606070684416807 ) ) ;
#24459 = CARTESIAN_POINT ( 'NONE',  ( 82.38380642140619159, -29.09073277922306744, 149.5372663468040741 ) ) ;
#24460 = DIRECTION ( 'NONE',  ( -1.000000000000000000, -1.224606353822377258E-16, -0.000000000000000000 ) ) ;
#24461 = CARTESIAN_POINT ( 'NONE',  ( 9.482945380845301031, 87.44333058778930479, 3.177595346755237138 ) ) ;
#24462 = ORIENTED_EDGE ( 'NONE', *, *, #54679, .F. ) ;
#24463 = AXIS2_PLACEMENT_3D ( 'NONE', #36807, #21164, #79344 ) ;
#24464 = CARTESIAN_POINT ( 'NONE',  ( -41.05804556683040829, 49.99999999999998579, 48.04352316237233111 ) ) ;
#24465 = CARTESIAN_POINT ( 'NONE',  ( -2.500000000000002220, 0.000000000000000000, 14.00000000000000000 ) ) ;
#24466 = CARTESIAN_POINT ( 'NONE',  ( 2.977408999572650927, -14.37500000204838280, -7.188101187500000933 ) ) ;
#24467 = DIRECTION ( 'NONE',  ( -1.000000000000000000, -1.224606353822377258E-16, -0.000000000000000000 ) ) ;
#24468 = PRESENTATION_LAYER_ASSIGNMENT (  '', '', ( #21011 ) ) ;
#24469 = CARTESIAN_POINT ( 'NONE',  ( 67.67130416077930022, -59.99999999999999289, -27.26907627581506333 ) ) ;
#24470 = CARTESIAN_POINT ( 'NONE',  ( -33.16850225799807106, 397.3870901570517162, 25.83374077364281973 ) ) ;
#24471 = CARTESIAN_POINT ( 'NONE',  ( -7.500145657655585829, -5.000000000000005329, -20.99858917502733746 ) ) ;
#24472 = VERTEX_POINT ( 'NONE', #71233 ) ;
#24473 = PRESENTATION_STYLE_ASSIGNMENT (( #22869 ) ) ;
#24475 = FACE_OUTER_BOUND ( 'NONE', #33054, .T. ) ;
#24474 = TOROIDAL_SURFACE ( 'NONE', #53690, 60.50000000000000000, 0.5000000000000000000 ) ;
#24476 = CARTESIAN_POINT ( 'NONE',  ( 7.500000000000007105, 39.99999999999970868, -59.88032989331640010 ) ) ;
#24477 = ADVANCED_FACE ( 'NONE', ( #104129 ), #88002, .T. ) ;
#24478 = VECTOR ( 'NONE', #98960, 1000.000000000000000 ) ;
#24479 = CARTESIAN_POINT ( 'NONE',  ( 1.125713873518663366, 34.84991794026092293, -27.86526467689072462 ) ) ;
#24480 = ORIENTED_EDGE ( 'NONE', *, *, #9803, .F. ) ;
#24481 = CARTESIAN_POINT ( 'NONE',  ( -2.977408999572654480, -31.62500000204838813, 7.188101187499999156 ) ) ;
#24482 = CARTESIAN_POINT ( 'NONE',  ( 24.10582191788833484, -28.43080354620355266, 37.96870486749567419 ) ) ;
#24483 = CARTESIAN_POINT ( 'NONE',  ( -39.40891928560527191, 489.7148911633813100, 11.67978059220125076 ) ) ;
#24484 = CARTESIAN_POINT ( 'NONE',  ( 0.1699655916222989060, 51.26930509877139741, -10.25000000000000178 ) ) ;
#24485 = CARTESIAN_POINT ( 'NONE',  ( 39.83339193442425596, 438.7265728230044033, 23.10267571010011878 ) ) ;
#24486 = APPLICATION_PROTOCOL_DEFINITION ( 'draft international standard', 'automotive_design', 1998, #54819 ) ;
#24487 = CARTESIAN_POINT ( 'NONE',  ( 49.18559949472803083, 8.441045694768780194, 15.12439388195326195 ) ) ;
#24488 = ORIENTED_EDGE ( 'NONE', *, *, #62905, .F. ) ;
#24489 = CARTESIAN_POINT ( 'NONE',  ( 34.42407431220851066, 4.999999999999994671, 6.123233995736758394E-16 ) ) ;
#24490 = CARTESIAN_POINT ( 'NONE',  ( 14.25150717306086889, 43.31689343519231983, -90.90741688367272388 ) ) ;
#24491 = FACE_OUTER_BOUND ( 'NONE', #77077, .T. ) ;
#24492 = CIRCLE ( 'NONE', #105376, 5.000000000000002665 ) ;
#24493 = ORIENTED_EDGE ( 'NONE', *, *, #55132, .F. ) ;
#24494 = CARTESIAN_POINT ( 'NONE',  ( -43.51233770565556114, 462.0554640178127670, 4.320559117850118369 ) ) ;
#24495 = CARTESIAN_POINT ( 'NONE',  ( 110.2197559186844131, -57.66896312012423920, 195.6918597009357370 ) ) ;
#24496 = VECTOR ( 'NONE', #89258, 1000.000000000000000 ) ;
#24497 = EDGE_CURVE ( 'NONE', #104741, #18574, #59193, .T. ) ;
#24498 = CARTESIAN_POINT ( 'NONE',  ( 34.68490551323855442, 463.9993046474232301, 18.60480341024936024 ) ) ;
#24499 = STYLED_ITEM ( 'NONE', ( #79632 ), #104485 ) ;
#24500 = DIRECTION ( 'NONE',  ( 0.000000000000000000, 1.000000000000000000, 0.000000000000000000 ) ) ;
#24501 = CARTESIAN_POINT ( 'NONE',  ( 6.683837171061806082, 7.911893696991936231, -4.595687358162529387E-16 ) ) ;
#24502 = CARTESIAN_POINT ( 'NONE',  ( -6.509863194222623051, 53.49549999415722823, 7.566361094272520127 ) ) ;
#24503 = CARTESIAN_POINT ( 'NONE',  ( -74.34326984540557248, -60.00000000000000711, 175.6274979054055336 ) ) ;
#24504 = CARTESIAN_POINT ( 'NONE',  ( -23.43684916743750080, 295.2641918988800285, 10.02474406024658293 ) ) ;
#24505 = EDGE_CURVE ( 'NONE', #10553, #46481, #20302, .T. ) ;
#24506 = CARTESIAN_POINT ( 'NONE',  ( -38.68218982724705057, 320.0845437455996603, 16.10279619727025135 ) ) ;
#24507 = CARTESIAN_POINT ( 'NONE',  ( -84.74621718593478192, -50.19506395242900254, 188.7085204688150952 ) ) ;
#24508 = ORIENTED_EDGE ( 'NONE', *, *, #16300, .F. ) ;
#24509 = CARTESIAN_POINT ( 'NONE',  ( 28.42669129514683135, 309.2334035236105478, -8.000929056396238082 ) ) ;
#24510 = VERTEX_POINT ( 'NONE', #33870 ) ;
#24511 = CARTESIAN_POINT ( 'NONE',  ( 16.04706041842035802, 4.602438919581936183, 3.432847546123024340 ) ) ;
#24512 = CARTESIAN_POINT ( 'NONE',  ( -4.744389013293895729, -1.372925465831638769, 104.3204960233004357 ) ) ;
#24513 = CARTESIAN_POINT ( 'NONE',  ( -85.72632401489656218, -52.73136465668492434, -5.089855646812738499 ) ) ;
#24514 = CARTESIAN_POINT ( 'NONE',  ( 83.28888888888889142, 1.023464760207051730E-14, 0.000000000000000000 ) ) ;
#24515 = DIRECTION ( 'NONE',  ( -1.000000000000000000, -0.000000000000000000, -0.000000000000000000 ) ) ;
#24516 = ORIENTED_EDGE ( 'NONE', *, *, #46803, .F. ) ;
#24517 = CARTESIAN_POINT ( 'NONE',  ( -32.94994279514382640, 464.9549361168403152, 15.12478419439365851 ) ) ;
#24518 = CARTESIAN_POINT ( 'NONE',  ( -5.500000000000006217, 42.00000000000000000, -59.88032989329961708 ) ) ;
#24519 = CARTESIAN_POINT ( 'NONE',  ( 13.60704923275372202, -1.734723475976807094E-15, 10.45706415777666365 ) ) ;
#24520 = CARTESIAN_POINT ( 'NONE',  ( 5.290067270632161645, 53.47475093287481229, -8.531152949374595451 ) ) ;
#24521 = CARTESIAN_POINT ( 'NONE',  ( 48.21450566731007825, -29.99999999999995381, -35.59756164575514958 ) ) ;
#24522 = CARTESIAN_POINT ( 'NONE',  ( -75.09116195550693362, -60.32198986609109426, 137.4145651127319070 ) ) ;
#24523 = ORIENTED_EDGE ( 'NONE', *, *, #38504, .F. ) ;
#24524 = CARTESIAN_POINT ( 'NONE',  ( 16.35858893754161869, -14.21045842199445630, 34.55986707822809478 ) ) ;
#24525 = FILL_AREA_STYLE ('',( #65483 ) ) ;
#24526 = CARTESIAN_POINT ( 'NONE',  ( 93.83421280875700177, -57.67400127416684796, 13.19124553429083058 ) ) ;
#24527 = ORIENTED_EDGE ( 'NONE', *, *, #13257, .T. ) ;
#24528 = DIRECTION ( 'NONE',  ( 0.000000000000000000, -0.2013748291394190093, -0.9795142562459567825 ) ) ;
#24529 = DIRECTION ( 'NONE',  ( -1.000000000000000000, -1.224606353822377258E-16, -0.000000000000000000 ) ) ;
#24530 = EDGE_LOOP ( 'NONE', ( #45944, #67845, #70269, #97050 ) ) ;
#24531 = CARTESIAN_POINT ( 'NONE',  ( 15.42175249681818805, 44.08902557066564754, 5.093581733527382305 ) ) ;
#24532 = CARTESIAN_POINT ( 'NONE',  ( 4.401442555609581635E-16, -21.78125000204838457, -7.188101187500000044 ) ) ;
#24533 = CARTESIAN_POINT ( 'NONE',  ( 44.26939524491439926, 485.3791217652536716, 2.298766312369611153 ) ) ;
#24534 = CARTESIAN_POINT ( 'NONE',  ( -17.89487417552028248, 45.31800925772326138, -5.467316602108599710 ) ) ;
#24535 = DIRECTION ( 'NONE',  ( -0.000000000000000000, 1.000000000000000000, -0.000000000000000000 ) ) ;
#24536 = VERTEX_POINT ( 'NONE', #65141 ) ;
#24537 = EDGE_CURVE ( 'NONE', #36, #78368, #25735, .T. ) ;
#24538 = CARTESIAN_POINT ( 'NONE',  ( -7.452250100395975352, 40.95021212578417646, -69.64366906012794800 ) ) ;
#24539 = PRESENTATION_LAYER_ASSIGNMENT (  '', '', ( #72702 ) ) ;
#24541 = CARTESIAN_POINT ( 'NONE',  ( 31.37193178408734795, -46.43139637310807899, 34.89162135181897639 ) ) ;
#24540 = CARTESIAN_POINT ( 'NONE',  ( 1.295095875561511761E-05, -30.00000000000000000, 37.00000000000000711 ) ) ;
#24542 = CARTESIAN_POINT ( 'NONE',  ( -4.661380720324451943, 51.51205150140802402, -8.373549780453599212 ) ) ;
#24543 = EDGE_LOOP ( 'NONE', ( #28497, #7808, #57613, #12096, #44653, #86501 ) ) ;
#24544 = EDGE_CURVE ( 'NONE', #10763, #51428, #1186, .T. ) ;
#24545 = TOROIDAL_SURFACE ( 'NONE', #38320, 7.999999999999983125, 1.000000000000000888 ) ;
#24546 = ADVANCED_FACE ( 'NONE', ( #69414 ), #3612, .T. ) ;
#24547 = ORIENTED_EDGE ( 'NONE', *, *, #84348, .F. ) ;
#24549 = CARTESIAN_POINT ( 'NONE',  ( 38.11830511241422670, 460.5921607997356659, 2.566192292264859010 ) ) ;
#24548 = CARTESIAN_POINT ( 'NONE',  ( -37.56673239365863282, 25.47613764497371847, -13.45617127781024891 ) ) ;
#24550 = CARTESIAN_POINT ( 'NONE',  ( 0.000000000000000000, 80.00000000000000000, 0.000000000000000000 ) ) ;
#24551 = CARTESIAN_POINT ( 'NONE',  ( -13.28202820877807433, 294.5488970812774596, -10.06438453904008945 ) ) ;
#24552 = DIRECTION ( 'NONE',  ( 0.000000000000000000, -1.000000000000000000, 2.311253228826402606E-16 ) ) ;
#24553 = CARTESIAN_POINT ( 'NONE',  ( 0.1683204496895580327, 45.30680571434964321, 18.74148122118527482 ) ) ;
#24554 = CARTESIAN_POINT ( 'NONE',  ( -35.96642943166444439, 464.0782432590693247, 19.48772549671483389 ) ) ;
#24555 = EDGE_LOOP ( 'NONE', ( #42249, #34272, #85856, #29691 ) ) ;
#24556 = CARTESIAN_POINT ( 'NONE',  ( 33.19500532560861927, -60.00000000000002842, -40.53309893464972902 ) ) ;
#24557 = CARTESIAN_POINT ( 'NONE',  ( -10.12102021413168274, 45.41888843717377000, 15.40779740156163946 ) ) ;
#24558 = CARTESIAN_POINT ( 'NONE',  ( 30.00000000000000355, 462.0200324021747065, 12.95089283449304496 ) ) ;
#24559 = ADVANCED_FACE ( 'NONE', ( #44608 ), #75275, .F. ) ;
#24560 = CARTESIAN_POINT ( 'NONE',  ( 30.59999999999999787, 1.533819458162526451E-15, 0.000000000000000000 ) ) ;
#24561 = CARTESIAN_POINT ( 'NONE',  ( 47.78440564129551404, 10.33446651290970308, -16.83708170412499072 ) ) ;
#24562 = ORIENTED_EDGE ( 'NONE', *, *, #71202, .T. ) ;
#24563 = AXIS2_PLACEMENT_3D ( 'NONE', #99161, #51141, #58180 ) ;
#24564 = DIRECTION ( 'NONE',  ( 1.000000000000000000, -0.000000000000000000, -0.000000000000000000 ) ) ;
#24565 = ORIENTED_EDGE ( 'NONE', *, *, #94745, .T. ) ;
#24566 = ORIENTED_EDGE ( 'NONE', *, *, #68203, .T. ) ;
#24567 = CARTESIAN_POINT ( 'NONE',  ( 0.5667977521132806507, 54.25196811838322475, 7.882806152410106293 ) ) ;
#24568 = LINE ( 'NONE', #98416, #1029 ) ;
#24569 =( NAMED_UNIT ( * ) SI_UNIT ( $, .STERADIAN. ) SOLID_ANGLE_UNIT ( ) );
#24570 = CARTESIAN_POINT ( 'NONE',  ( 28.35254126057398594, 309.9120444834643990, 11.61584289200398956 ) ) ;
#24571 = CARTESIAN_POINT ( 'NONE',  ( -36.70796720182337225, 339.3380366985459773, -1.209698081358119071 ) ) ;
#24572 = CARTESIAN_POINT ( 'NONE',  ( -5.000000000000000000, -60.71953810597472767, 12.61250543006392988 ) ) ;
#24573 = CARTESIAN_POINT ( 'NONE',  ( 12.50000000000000711, 36.63321530731812459, -57.11196096728948390 ) ) ;
#24574 = ORIENTED_EDGE ( 'NONE', *, *, #65521, .F. ) ;
#24575 = CARTESIAN_POINT ( 'NONE',  ( -9.875831867757614901, 44.06546706392215640, 12.97410724739095755 ) ) ;
#24576 = VERTEX_POINT ( 'NONE', #94212 ) ;
#24577 = DIRECTION ( 'NONE',  ( -1.000000000000000000, -1.224606353822377258E-16, -0.000000000000000000 ) ) ;
#24578 = DIRECTION ( 'NONE',  ( 0.000000000000000000, -1.000000000000000000, 0.000000000000000000 ) ) ;
#24579 = DIRECTION ( 'NONE',  ( 0.000000000000000000, -1.000000000000000000, 0.000000000000000000 ) ) ;
#24580 = CARTESIAN_POINT ( 'NONE',  ( -22.92989048780488304, -59.99999999999997158, 34.79415195187766585 ) ) ;
#24581 = CARTESIAN_POINT ( 'NONE',  ( 69.47498401038441784, -25.58548699416417094, 92.27391141522187468 ) ) ;
#24582 = ORIENTED_EDGE ( 'NONE', *, *, #75897, .T. ) ;
#24583 = DIRECTION ( 'NONE',  ( -0.000000000000000000, -0.000000000000000000, -1.000000000000000000 ) ) ;
#24584 = CARTESIAN_POINT ( 'NONE',  ( -44.70137845890145911, -57.67116879762227910, -40.89012893473564958 ) ) ;
#24585 = ORIENTED_EDGE ( 'NONE', *, *, #106117, .F. ) ;
#24586 = CARTESIAN_POINT ( 'NONE',  ( 46.97290287162415012, 17.76084728355337816, 16.28892042402536333 ) ) ;
#24587 = CARTESIAN_POINT ( 'NONE',  ( -36.15790072655923382, 490.9284497187053944, 12.44298047260288165 ) ) ;
#24588 = EDGE_CURVE ( 'NONE', #64324, #73045, #32196, .T. ) ;
#24589 = DIRECTION ( 'NONE',  ( 0.000000000000000000, 0.000000000000000000, 1.000000000000000000 ) ) ;
#24590 = CARTESIAN_POINT ( 'NONE',  ( -8.000000000000000000, -22.43750000409676915, -9.797174393178825657E-16 ) ) ;
#24591 = DIRECTION ( 'NONE',  ( -1.000000000000000000, -1.224606353822377258E-16, -0.000000000000000000 ) ) ;
#24592 = CARTESIAN_POINT ( 'NONE',  ( 9.221216839714889701, 248.9524025183100946, 3.869414262756992517 ) ) ;
#24593 = B_SPLINE_CURVE_WITH_KNOTS ( 'NONE', 3,
 ( #100241, #35017, #28001, #43604, #93758, #51687, #36095, #33954, #59273, #10167, #17750, #35553 ),
 .UNSPECIFIED., .F., .F.,
 ( 4, 2, 2, 2, 2, 4 ),
 ( 0.04761886307670518820, 0.05150820635059603914, 0.05539754962448689701, 0.06317623617226861277, 0.07095492272005031464, 0.07873360926783201652 ),
 .UNSPECIFIED. ) ;
#24594 = DIRECTION ( 'NONE',  ( -1.000000000000000000, 0.000000000000000000, 0.000000000000000000 ) ) ;
#24595 = CARTESIAN_POINT ( 'NONE',  ( -10.16315516181093592, 7.266990280869982222, 5.000000000000000888 ) ) ;
#24596 = CARTESIAN_POINT ( 'NONE',  ( 61.37206225042174879, 4.000000000000015099, 4.898587196589422689E-16 ) ) ;
#24597 = VECTOR ( 'NONE', #52155, 1000.000000000000114 ) ;
#24598 = CARTESIAN_POINT ( 'NONE',  ( -0.7060372491599424816, 15.23416508904354671, -9.999999999999998224 ) ) ;
#24599 = ORIENTED_EDGE ( 'NONE', *, *, #95863, .F. ) ;
#24600 = DIRECTION ( 'NONE',  ( 0.000000000000000000, 1.000000000000000000, 0.000000000000000000 ) ) ;
#24601 = STYLED_ITEM ( 'NONE', ( #69967 ), #51962 ) ;
#24602 = LINE ( 'NONE', #16484, #75528 ) ;
#24603 = CARTESIAN_POINT ( 'NONE',  ( -95.47858839875321735, -29.99999999999999289, 191.3280271152898706 ) ) ;
#24604 = ADVANCED_FACE ( 'NONE', ( #100688 ), #51609, .F. ) ;
#24605 = CARTESIAN_POINT ( 'NONE',  ( 94.26467260280679739, 1.016364837396684119E-14, 0.000000000000000000 ) ) ;
#24606 = AXIS2_PLACEMENT_3D ( 'NONE', #59438, #92304, #19006 ) ;
#24607 = CARTESIAN_POINT ( 'NONE',  ( 73.80742417545810952, -57.62089382719297959, 186.0993484855978579 ) ) ;
#24609 = LINE ( 'NONE', #91972, #24210 ) ;
#24608 = CARTESIAN_POINT ( 'NONE',  ( 3.616665348617805752E-21, 26.07813853931757464, -38.25000000000000000 ) ) ;
#24610 = B_SPLINE_CURVE_WITH_KNOTS ( 'NONE', 3,
 ( #65674, #98558, #24708, #57556, #90482, #16589 ),
 .UNSPECIFIED., .F., .F.,
 ( 4, 2, 4 ),
 ( 0.000000000000000000, 0.0003491763592121705667, 0.0006983527184243411333 ),
 .UNSPECIFIED. ) ;
#24611 = CARTESIAN_POINT ( 'NONE',  ( 19.40646391855202779, -25.62022252646447384, -38.49139321023872640 ) ) ;
#24612 = CARTESIAN_POINT ( 'NONE',  ( -1.249751218086241566, 43.67234525511032217, 17.34011378923078084 ) ) ;
#24613 = CARTESIAN_POINT ( 'NONE',  ( 73.59428447264397732, 6.856755485862130937E-15, 0.000000000000000000 ) ) ;
#24614 = CARTESIAN_POINT ( 'NONE',  ( -12.67931802180743972, -59.99999999999998579, 39.70502876154672123 ) ) ;
#24615 =( REPRESENTATION_RELATIONSHIP ('NONE','NONE', #69581, #25516 ) REPRESENTATION_RELATIONSHIP_WITH_TRANSFORMATION ( #43283 )SHAPE_REPRESENTATION_RELATIONSHIP( ) );
#24616 = CARTESIAN_POINT ( 'NONE',  ( 13.27069161507911588, 19.68838461291719355, 7.441922568579489194 ) ) ;
#24617 = EDGE_CURVE ( 'NONE', #21035, #31964, #93889, .T. ) ;
#24618 = CARTESIAN_POINT ( 'NONE',  ( 6.366644313785284837, 53.78389048455223787, 6.625974567219506284 ) ) ;
#24619 = CARTESIAN_POINT ( 'NONE',  ( -85.77437932991819025, -61.06087370286046934, 194.1425874229156250 ) ) ;
#24620 = VERTEX_POINT ( 'NONE', #32545 ) ;
#24621 = CARTESIAN_POINT ( 'NONE',  ( 17.50000000000004974, 51.99999999999999289, 59.91915230423961702 ) ) ;
#24622 = CARTESIAN_POINT ( 'NONE',  ( 6.393725729381808165, -15.50592724712675086, 14.54168635664702514 ) ) ;
#24623 = CARTESIAN_POINT ( 'NONE',  ( -10.12172432390016752, -25.54964335568536171, 28.15750748029973494 ) ) ;
#24624 = AXIS2_PLACEMENT_3D ( 'NONE', #33343, #9027, #74821 ) ;
#24625 = EDGE_CURVE ( 'NONE', #33590, #106160, #1266, .T. ) ;
#24627 = CARTESIAN_POINT ( 'NONE',  ( -8.239323762215395419, 53.79478660573261095, 3.999901775324819386 ) ) ;
#24626 = CARTESIAN_POINT ( 'NONE',  ( 6.781345014477442312, -3.590342129888872691, -6.122077150241854504 ) ) ;
#24628 = EDGE_LOOP ( 'NONE', ( #65618, #23508, #87225, #96087 ) ) ;
#24629 = CARTESIAN_POINT ( 'NONE',  ( 4.999060825136298014, 41.75164249415627182, -70.37937598343344803 ) ) ;
#24630 = CARTESIAN_POINT ( 'NONE',  ( -8.044970079966896392, -5.000000000000017764, -15.82739658860585941 ) ) ;
#24631 = CARTESIAN_POINT ( 'NONE',  ( -7.999912353029502654, 33.99982470603092821, -0.2691822806795013956 ) ) ;
#24632 = COLOUR_RGB ( '', 0.40784314, 0.44705882, 0.49803922) ;
#24633 = CARTESIAN_POINT ( 'NONE',  ( 33.29811181468569004, 300.4441021725457404, -0.7436061328819506544 ) ) ;
#24634 = LINE ( 'NONE', #58020, #79424 ) ;
#24635 = CARTESIAN_POINT ( 'NONE',  ( -7.986711519608433285, -81.02638096376567489, -0.5300249774147601789 ) ) ;
#24636 = FACE_OUTER_BOUND ( 'NONE', #75925, .T. ) ;
#24637 = CARTESIAN_POINT ( 'NONE',  ( 109.2895958250431931, -30.00000000000001776, 180.5620058458624442 ) ) ;
#24638 = DIRECTION ( 'NONE',  ( 1.000000000000000000, 0.000000000000000000, -1.224646799147353207E-16 ) ) ;
#24639 = ORIENTED_EDGE ( 'NONE', *, *, #85366, .F. ) ;
#24640 = CARTESIAN_POINT ( 'NONE',  ( -7.721181058141405096, -30.00000000000004263, -2.093648267354947912 ) ) ;
#24641 = CARTESIAN_POINT ( 'NONE',  ( -9.221346651730865318, 251.0483402006833842, -3.869102247876019973 ) ) ;
#24642 = CARTESIAN_POINT ( 'NONE',  ( -4.606548227981508425, -6.456511556909262595, -7.591235721156640359 ) ) ;
#24643 = CARTESIAN_POINT ( 'NONE',  ( 4.474623633716955595, 9.480714495128564678, -4.999999999999998224 ) ) ;
#24644 = CARTESIAN_POINT ( 'NONE',  ( 43.58517788116362368, 464.0093709438414180, 6.089361716052055229 ) ) ;
#24645 = ORIENTED_EDGE ( 'NONE', *, *, #17107, .F. ) ;
#24647 = EDGE_CURVE ( 'NONE', #75752, #71001, #55279, .T. ) ;
#24646 = UNCERTAINTY_MEASURE_WITH_UNIT (LENGTH_MEASURE( 1.000000000000000082E-05 ), #17419, 'distance_accuracy_value', 'NONE');
#24648 = ORIENTED_EDGE ( 'NONE', *, *, #58884, .F. ) ;
#24649 = CARTESIAN_POINT ( 'NONE',  ( 35.03683940498239480, 484.2356779365860575, -0.9730041317311258764 ) ) ;
#24650 = CARTESIAN_POINT ( 'NONE',  ( 9.034470188793607193, 46.02977034662632150, 14.11149907944944104 ) ) ;
#24651 = VERTEX_POINT ( 'NONE', #106383 ) ;
#24652 = CARTESIAN_POINT ( 'NONE',  ( 55.22048556080756043, 48.00000000000000000, 34.80214219304977519 ) ) ;
#24653 = CARTESIAN_POINT ( 'NONE',  ( 6.282481257750461623, -11.96849729169402998, 11.22390784433575206 ) ) ;
#24654 = CARTESIAN_POINT ( 'NONE',  ( -69.35185981456076831, -60.00000000005866241, 152.1736452874216639 ) ) ;
#24655 = CARTESIAN_POINT ( 'NONE',  ( 46.00000000000000000, 437.9222508511570595, 13.74115800020442002 ) ) ;
#24656 = ORIENTED_EDGE ( 'NONE', *, *, #40221, .T. ) ;
#24657 = CARTESIAN_POINT ( 'NONE',  ( 91.95750203301783188, -59.99999999999998579, 17.41842218427850497 ) ) ;
#24659 = CARTESIAN_POINT ( 'NONE',  ( 16.83005395452520148, -42.95383171955222679, 31.29264600947682240 ) ) ;
#24658 = CARTESIAN_POINT ( 'NONE',  ( -111.5324017304388207, -60.00000000000003553, 193.8614060841614730 ) ) ;
#24660 = CARTESIAN_POINT ( 'NONE',  ( 16.32074838266548511, 61.49999999999999289, -8.160374191332739002 ) ) ;
#24661 = DIRECTION ( 'NONE',  ( 0.000000000000000000, 0.000000000000000000, -1.000000000000000000 ) ) ;
#24662 = CARTESIAN_POINT ( 'NONE',  ( -43.03151631067254357, -39.52863235512158724, 41.51148371547483151 ) ) ;
#24663 = LINE ( 'NONE', #57516, #98761 ) ;
#24664 = VERTEX_POINT ( 'NONE', #98312 ) ;
#24665 = CARTESIAN_POINT ( 'NONE',  ( 59.89460441624491693, 6.975173280561618775E-15, 0.000000000000000000 ) ) ;
#24666 = CARTESIAN_POINT ( 'NONE',  ( 16.14595037822606827, 20.73037563563847385, -4.193214079404498307 ) ) ;
#24667 = CARTESIAN_POINT ( 'NONE',  ( 40.95595929481465447, 405.2208686710653183, 27.85131585683114963 ) ) ;
#24668 = AXIS2_PLACEMENT_3D ( 'NONE', #77574, #36620, #87264 ) ;
#24669 = DIRECTION ( 'NONE',  ( 0.000000000000000000, -1.000000000000000000, 0.000000000000000000 ) ) ;
#24670 = CARTESIAN_POINT ( 'NONE',  ( -5.656854249492379694, -28.62500000409677270, -5.656854249492380582 ) ) ;
#24671 = CARTESIAN_POINT ( 'NONE',  ( 10.51384838036216784, -0.8794359877124720004, 20.22631812719205868 ) ) ;
#24672 = VERTEX_POINT ( 'NONE', #24465 ) ;
#24673 = ORIENTED_EDGE ( 'NONE', *, *, #45590, .T. ) ;
#24674 = CARTESIAN_POINT ( 'NONE',  ( 73.52265062858249678, -30.00000000000002132, -18.84734495193007220 ) ) ;
#24675 = CARTESIAN_POINT ( 'NONE',  ( 23.95383387565141575, 41.62280648303626407, -74.36842561464139578 ) ) ;
#24676 = CONICAL_SURFACE ( 'NONE', #60847, 4.000000000000000000, 0.9599310885968912466 ) ;
#24677 = CARTESIAN_POINT ( 'NONE',  ( 23.55041599580185974, 25.19295639533963183, -33.17275278237224256 ) ) ;
#24679 = EDGE_CURVE ( 'NONE', #16577, #35268, #30961, .T. ) ;
#24678 = DIRECTION ( 'NONE',  ( 0.000000000000000000, -1.000000000000000000, 0.000000000000000000 ) ) ;
#24680 = CARTESIAN_POINT ( 'NONE',  ( 100.5424548002938252, -30.00000000000000355, 159.7537580344667560 ) ) ;
#24681 = CIRCLE ( 'NONE', #21232, 1.999999999999999778 ) ;
#24682 = EDGE_CURVE ( 'NONE', #21618, #29736, #49488, .T. ) ;
#24683 = DIRECTION ( 'NONE',  ( -1.000000000000000000, -1.224606353822377258E-16, -0.000000000000000000 ) ) ;
#24684 = VERTEX_POINT ( 'NONE', #74027 ) ;
#24685 = ORIENTED_EDGE ( 'NONE', *, *, #26050, .F. ) ;
#24686 = ORIENTED_EDGE ( 'NONE', *, *, #10150, .T. ) ;
#24687 = CARTESIAN_POINT ( 'NONE',  ( 11.36650669486618881, 4.898587196589411843E-16, -4.000000000000000888 ) ) ;
#24688 = CARTESIAN_POINT ( 'NONE',  ( 22.25838323674845043, 26.06530384004942391, 31.15016210260246510 ) ) ;
#24689 = MECHANICAL_DESIGN_GEOMETRIC_PRESENTATION_REPRESENTATION (  '', ( #507 ), #65996 ) ;
#24690 = EDGE_CURVE ( 'NONE', #77058, #25026, #36047, .T. ) ;
#24691 = CARTESIAN_POINT ( 'NONE',  ( -37.67124221001134288, 463.6239404278531993, 19.49545380201589850 ) ) ;
#24692 = ORIENTED_EDGE ( 'NONE', *, *, #90396, .F. ) ;
#24693 = CARTESIAN_POINT ( 'NONE',  ( 9.253800200985681457, 106.3001033108817097, -3.791983798715485410 ) ) ;
#24694 = VERTEX_POINT ( 'NONE', #59466 ) ;
#24695 = CARTESIAN_POINT ( 'NONE',  ( 33.21102376836596903, 438.9613914113129454, 23.92328486949907429 ) ) ;
#24696 = CARTESIAN_POINT ( 'NONE',  ( 79.87769542981580173, -38.77283384872364991, 192.7642698354605670 ) ) ;
#24697 = CARTESIAN_POINT ( 'NONE',  ( 6.333820801331365047, 6.982605850972475103, -0.9057718968918052616 ) ) ;
#24698 = CARTESIAN_POINT ( 'NONE',  ( 29.99982483545057121, 316.1377075229455613, 13.18505363741200753 ) ) ;
#24699 = CARTESIAN_POINT ( 'NONE',  ( 6.162888688655344005, -3.752776749732561257, 6.500000000000000000 ) ) ;
#24700 = FACE_OUTER_BOUND ( 'NONE', #47785, .T. ) ;
#24701 = CIRCLE ( 'NONE', #103891, 8.000000000000000000 ) ;
#24702 = CARTESIAN_POINT ( 'NONE',  ( -27.10511071441193565, 34.75829513984539432, -7.556984339685824281 ) ) ;
#24703 = CARTESIAN_POINT ( 'NONE',  ( -4.586789253316107207, -47.77528324151405315, 102.5764008378948091 ) ) ;
#24704 =( BOUNDED_SURFACE ( )  B_SPLINE_SURFACE ( 3, 2, ( 
 ( #36828, #103122, #62153 ),
 ( #102589, #96089, #104165 ),
 ( #5997, #30307, #22225 ),
 ( #14080, #28738, #38920 ),
 ( #61623, #72335, #48040 ),
 ( #41559, #8652, #24865 ),
 ( #23824, #31382, #97132 ),
 ( #82551, #8118, #57721 ) ),
 .UNSPECIFIED., .F., .F., .F. ) 
 B_SPLINE_SURFACE_WITH_KNOTS ( ( 4, 2, 2, 4 ),
 ( 3, 3 ),
 ( 0.03850042371095790256, 0.04313406099830587037, 0.04545087964197985081, 0.04776769828565383125 ),
 ( 0.000000000000000000, 1.000000000000000000 ),
 .UNSPECIFIED. ) 
 GEOMETRIC_REPRESENTATION_ITEM ( )  RATIONAL_B_SPLINE_SURFACE ( (
 ( 1.000000000000000000, 0.8047781847388131293, 1.000000000000000000),
 ( 1.000000000000000000, 0.8123760230790857406, 1.000000000000000000),
 ( 1.000000000000000000, 0.8190653851699112309, 1.000000000000000000),
 ( 1.000000000000000000, 0.8191940386277110075, 1.000000000000000000),
 ( 1.000000000000000000, 0.8176096570055705337, 1.000000000000000000),
 ( 1.000000000000000000, 0.8122964723277524834, 1.000000000000000000),
 ( 1.000000000000000000, 0.8086312464132838773, 1.000000000000000000),
 ( 1.000000000000000000, 0.8047712192439641088, 1.000000000000000000) ) ) 
 REPRESENTATION_ITEM ( '' )  SURFACE ( )  );
#24705 =( NAMED_UNIT ( * ) SI_UNIT ( $, .STERADIAN. ) SOLID_ANGLE_UNIT ( ) );
#24706 = CARTESIAN_POINT ( 'NONE',  ( 41.08349330513380693, 1.593028355512270567E-15, 0.000000000000000000 ) ) ;
#24707 = ORIENTED_EDGE ( 'NONE', *, *, #11819, .F. ) ;
#24708 = CARTESIAN_POINT ( 'NONE',  ( 6.394343112843833055, 7.552705921139274636, -6.068871123799707842E-16 ) ) ;
#24710 = CARTESIAN_POINT ( 'NONE',  ( -25.05418058866352382, 295.6716560995653822, 2.113063722413087042 ) ) ;
#24709 =( NAMED_UNIT ( * ) SI_UNIT ( $, .STERADIAN. ) SOLID_ANGLE_UNIT ( ) );
#24711 = FILL_AREA_STYLE_COLOUR ( '', #34778 ) ;
#24712 = UNCERTAINTY_MEASURE_WITH_UNIT (LENGTH_MEASURE( 1.000000000000000082E-05 ), #85782, 'distance_accuracy_value', 'NONE');
#24713 = CARTESIAN_POINT ( 'NONE',  ( -13.14242568365673414, 42.00000000000000000, -92.43215185528094935 ) ) ;
#24714 = CARTESIAN_POINT ( 'NONE',  ( -3.093533885184728494, -6.874201416485484550, -7.446478553994769101 ) ) ;
#24715 = PRESENTATION_LAYER_ASSIGNMENT (  '', '', ( #64270 ) ) ;
#24716 = CARTESIAN_POINT ( 'NONE',  ( 35.86397158582656886, -35.96817661624932327, 45.02762458631914200 ) ) ;
#24717 = DIRECTION ( 'NONE',  ( -1.000000000000000000, -1.224606353822377258E-16, -0.000000000000000000 ) ) ;
#24718 = EDGE_CURVE ( 'NONE', #71251, #76425, #97668, .T. ) ;
#24719 = ORIENTED_EDGE ( 'NONE', *, *, #98287, .T. ) ;
#24720 = CARTESIAN_POINT ( 'NONE',  ( 85.72981139660485894, -35.64577651797950608, 184.4330373048933325 ) ) ;
#24721 = CARTESIAN_POINT ( 'NONE',  ( 38.54515645702225868, 6.123233995736772199E-16, -5.000000000000001776 ) ) ;
#24722 = ORIENTED_EDGE ( 'NONE', *, *, #12792, .T. ) ;
#24723 = CARTESIAN_POINT ( 'NONE',  ( 92.77703971953890516, -57.65704708596170747, -17.75489428273840886 ) ) ;
#24724 = DIRECTION ( 'NONE',  ( -0.000000000000000000, -0.000000000000000000, -1.000000000000000000 ) ) ;
#24725 = DIRECTION ( 'NONE',  ( -1.000000000000000000, -0.000000000000000000, -0.000000000000000000 ) ) ;
#24726 = PRESENTATION_STYLE_ASSIGNMENT (( #32819 ) ) ;
#24727 = CARTESIAN_POINT ( 'NONE',  ( -80.75022429576897309, -30.00000000000000711, 11.83902672125366706 ) ) ;
#24728 = EDGE_CURVE ( 'NONE', #68006, #104233, #70135, .T. ) ;
#24729 = CARTESIAN_POINT ( 'NONE',  ( -66.13744702806401676, -38.00000000000000711, 88.79736889982228831 ) ) ;
#24730 = CARTESIAN_POINT ( 'NONE',  ( 22.65267572660716766, 28.20149222899207686, -30.83791392134371989 ) ) ;
#24731 = CARTESIAN_POINT ( 'NONE',  ( 0.000000000000000000, 0.000000000000000000, 0.000000000000000000 ) ) ;
#24732 =( LENGTH_UNIT ( ) NAMED_UNIT ( * ) SI_UNIT ( .MILLI., .METRE. ) );
#24733 = CARTESIAN_POINT ( 'NONE',  ( -17.49999999999997513, 49.85589862348337675, 63.87662473929367479 ) ) ;
#24734 = DIRECTION ( 'NONE',  ( -0.000000000000000000, -0.000000000000000000, -1.000000000000000000 ) ) ;
#24735 = DIRECTION ( 'NONE',  ( 0.000000000000000000, 0.000000000000000000, 1.000000000000000000 ) ) ;
#24736 = CARTESIAN_POINT ( 'NONE',  ( 19.00000000000000711, 4.000000000000000000, -1.500000000000000000 ) ) ;
#24737 = B_SPLINE_CURVE_WITH_KNOTS ( 'NONE', 3,
 ( #86170, #45169, #53767, #4699 ),
 .UNSPECIFIED., .F., .F.,
 ( 4, 4 ),
 ( 2.525795506525165703E-17, 0.0002485318720365765443 ),
 .UNSPECIFIED. ) ;
#24738 = CARTESIAN_POINT ( 'NONE',  ( -22.11582326320239034, 26.03313043097262280, 31.35975099478267225 ) ) ;
#24739 = CARTESIAN_POINT ( 'NONE',  ( 45.59999999999999432, 1.533819458162526451E-15, 0.000000000000000000 ) ) ;
#24740 = CIRCLE ( 'NONE', #491, 5.000000000000011546 ) ;
#24741 = CARTESIAN_POINT ( 'NONE',  ( -101.6436112212510920, -37.99999999999999289, 186.0797090425507463 ) ) ;
#24742 = EDGE_CURVE ( 'NONE', #106540, #77528, #32894, .T. ) ;
#24743 = STYLED_ITEM ( 'NONE', ( #61916 ), #84820 ) ;
#24744 = ORIENTED_EDGE ( 'NONE', *, *, #59478, .F. ) ;
#24745 = CARTESIAN_POINT ( 'NONE',  ( 5.975663821521703056, -4.257391242883674209, -5.625982059626680076 ) ) ;
#24746 = CARTESIAN_POINT ( 'NONE',  ( 0.2690448671709230188, 21.85270131633360435, 7.000000000000021316 ) ) ;
#24747 = CONICAL_SURFACE ( 'NONE', #60932, 4.172000000000009479, 0.9599310885968813656 ) ;
#24748 = FACE_OUTER_BOUND ( 'NONE', #105080, .T. ) ;
#24749 = ADVANCED_FACE ( 'NONE', ( #49754 ), #27136, .T. ) ;
#24751 = CARTESIAN_POINT ( 'NONE',  ( -72.23576987978789532, -60.22812697544318183, -25.48613692067792158 ) ) ;
#24750 = DIRECTION ( 'NONE',  ( 0.000000000000000000, -1.000000000000000000, 0.000000000000000000 ) ) ;
#24752 = VERTEX_POINT ( 'NONE', #99899 ) ;
#24754 = ORIENTED_EDGE ( 'NONE', *, *, #69328, .T. ) ;
#24753 = TOROIDAL_SURFACE ( 'NONE', #90178, 66.00000000000000000, 0.5000000000000000000 ) ;
#24755 = CARTESIAN_POINT ( 'NONE',  ( 0.000000000000000000, -5.629165124598847214, 3.250000000000005329 ) ) ;
#24756 = CARTESIAN_POINT ( 'NONE',  ( 6.249999999999998224, 4.618802153517001408, -8.000000000000000000 ) ) ;
#24757 = FILL_AREA_STYLE ('',( #41443 ) ) ;
#24758 = CARTESIAN_POINT ( 'NONE',  ( -33.67313932047541414, -59.99999999999998579, -40.47465270752430655 ) ) ;
#24760 = ADVANCED_FACE ( 'NONE', ( #58928 ), #17941, .F. ) ;
#24759 = ORIENTED_EDGE ( 'NONE', *, *, #56093, .T. ) ;
#24761 = CARTESIAN_POINT ( 'NONE',  ( 0.2578475836320698322, -4.367703157927325108, 5.434916218090832807 ) ) ;
#24762 = CARTESIAN_POINT ( 'NONE',  ( -8.838593709200374349, 294.6759896675590653, -4.712412173198521792 ) ) ;
#24763 = CARTESIAN_POINT ( 'NONE',  ( 94.65454574660577691, -37.70782373346656868, 193.0112514210578638 ) ) ;
#24764 = CARTESIAN_POINT ( 'NONE',  ( -16.96324018633377051, 45.77154698568145363, 4.157797401561650119 ) ) ;
#24765 = ORIENTED_EDGE ( 'NONE', *, *, #102166, .T. ) ;
#24766 = VECTOR ( 'NONE', #41270, 1000.000000000000000 ) ;
#24767 = VERTEX_POINT ( 'NONE', #83706 ) ;
#24768 = EDGE_LOOP ( 'NONE', ( #16920, #65199, #18030, #67492 ) ) ;
#24769 = CARTESIAN_POINT ( 'NONE',  ( 30.82873539022197562, 330.8540204601990240, 16.52588298193462180 ) ) ;
#24770 = CARTESIAN_POINT ( 'NONE',  ( -4.999999999999921840, -12.28614229754770193, 10.41767341469734376 ) ) ;
#24771 = DIRECTION ( 'NONE',  ( 0.000000000000000000, 0.000000000000000000, 1.000000000000000000 ) ) ;
#24772 = ORIENTED_EDGE ( 'NONE', *, *, #15126, .T. ) ;
#24773 = DIRECTION ( 'NONE',  ( 1.000000000000000000, 0.000000000000000000, 0.000000000000000000 ) ) ;
#24774 = DIRECTION ( 'NONE',  ( 0.000000000000000000, 0.000000000000000000, 1.000000000000000000 ) ) ;
#24775 = CIRCLE ( 'NONE', #74632, 4.000000000000007105 ) ;
#24776 = DIRECTION ( 'NONE',  ( -1.000000000000000000, -1.224606353822377258E-16, -0.000000000000000000 ) ) ;
#24777 = CARTESIAN_POINT ( 'NONE',  ( -35.27718283856832926, -57.69548877625971528, 49.41932622563938793 ) ) ;
#24778 = CARTESIAN_POINT ( 'NONE',  ( -7.188101187500002709, -30.31250000204838813, 2.977408999572648707 ) ) ;
#24779 = CARTESIAN_POINT ( 'NONE',  ( 3.400000000000000355, 0.000000000000000000, -6.418875477074183600 ) ) ;
#24780 = CONICAL_SURFACE ( 'NONE', #33402, 3.309500000000007880, 0.9599310885968770357 ) ;
#24781 = CARTESIAN_POINT ( 'NONE',  ( 4.684274960302871098E-15, 26.07813853931757464, 38.25000000000000000 ) ) ;
#24782 = CARTESIAN_POINT ( 'NONE',  ( 2.701558353794771161, 15.00000000000000000, -9.999999999999998224 ) ) ;
#24783 = CARTESIAN_POINT ( 'NONE',  ( 16.60915088697842990, -29.99999999999996092, -39.45628980158949162 ) ) ;
#24784 = CARTESIAN_POINT ( 'NONE',  ( -16.35964837410663364, -14.21045842199427156, 34.56001531359335388 ) ) ;
#24785 = CARTESIAN_POINT ( 'NONE',  ( -52.77677503717105623, -42.97426568945239467, 57.04412880052729662 ) ) ;
#24786 = ORIENTED_EDGE ( 'NONE', *, *, #16808, .T. ) ;
#24787 = CARTESIAN_POINT ( 'NONE',  ( -101.6154700970077727, -60.23106683408825290, 194.6025349640015918 ) ) ;
#24788 = B_SPLINE_CURVE_WITH_KNOTS ( 'NONE', 3,
 ( #54271, #87213, #34307, #8393, #40759, #9437, #66637, #48838, #24612, #97937, #15958, #67184, #42357, #75244, #16491, #90380, #41825, #17037, #58000, #91459, #74712, #73648 ),
 .UNSPECIFIED., .F., .F.,
 ( 4, 2, 2, 2, 2, 2, 2, 2, 2, 2, 4 ),
 ( 0.007183648798888384208, 0.007687614305072588451, 0.008191579811256791827, 0.008695545317440996069, 0.009199510823625200312, 0.009703476329809404555, 0.01020744183599360880, 0.01045942458908570745, 0.01071140734217780610, 0.01096339009526990475, 0.01121537284836200341 ),
 .UNSPECIFIED. ) ;
#24789 = CARTESIAN_POINT ( 'NONE',  ( -3.250000000000013767, -5.629165124598844550, 1.734723475976807094E-15 ) ) ;
#24790 = CARTESIAN_POINT ( 'NONE',  ( 15.31300439044785655, -0.5304010509286816166, 14.99217175782056444 ) ) ;
#24791 = EDGE_LOOP ( 'NONE', ( #22119, #66003, #100214, #10379 ) ) ;
#24792 = CARTESIAN_POINT ( 'NONE',  ( -17.88804523840099137, 43.18301036189587450, 5.551570213006435495 ) ) ;
#24793 = CARTESIAN_POINT ( 'NONE',  ( 80.29706273292998731, -38.80371450807032119, 193.5207487054061914 ) ) ;
#24794 = DIRECTION ( 'NONE',  ( 0.000000000000000000, -1.000000000000000000, 0.000000000000000000 ) ) ;
#24795 = CARTESIAN_POINT ( 'NONE',  ( -6.488521849125461038, 51.35019745309124772, -7.645917529146642799 ) ) ;
#24796 = CARTESIAN_POINT ( 'NONE',  ( -19.99639985080580118, 294.7507280618032155, 9.915515321361612067 ) ) ;
#24798 = CARTESIAN_POINT ( 'NONE',  ( 84.65172267273683815, -29.99999999999999645, 167.0116762541745743 ) ) ;
#24797 = UNCERTAINTY_MEASURE_WITH_UNIT (LENGTH_MEASURE( 1.000000000000000082E-05 ), #40714, 'distance_accuracy_value', 'NONE');
#24799 = B_SPLINE_SURFACE_WITH_KNOTS ( 'NONE', 1, 3, ( 
 ( #29861, #86506, #29340, #95111, #87022, #94590, #53575, #45503, #93517, #85970, #53049, #102117, #27755, #12040, #13094, #46021, #78903, #95631, #5030, #87546, #21769, #13627, #60629, #19664, #28274, #52497, #11500, #3435 ),
 ( #36380, #69244, #104776, #96693, #64848, #65383, #22830, #97728, #72407, #48643, #80483, #88076, #30925, #88599, #6070, #71871, #6601, #73451, #56191, #106349, #97205, #7652, #5548, #14154, #55662, #96170, #48116, #39530 ) ),
 .UNSPECIFIED., .F., .F., .F.,
 ( 2, 2 ),
 ( 4, 2, 2, 2, 2, 2, 2, 2, 2, 2, 2, 2, 2, 4 ),
 ( 0.000000000000000000, 1.000000000000000000 ),
 ( 0.08901491201581737678, 0.1032490540155679704, 0.1174831960153185778, 0.1317173380150691853, 0.1459514800148197788, 0.1744197640143299588, 0.2028880480138401388, 0.2598246160128514504, 0.3167611840118632616, 0.4306343200098861623, 0.5445074560079088410, 0.6583805920059359051, 0.7722537280039543095, 1.000000000000000000 ),
 .UNSPECIFIED. ) ;
#24800 = CARTESIAN_POINT ( 'NONE',  ( 37.36240688364735973, 491.3429102029600699, 12.25869953513177357 ) ) ;
#24801 = CARTESIAN_POINT ( 'NONE',  ( -29.68315524076989576, 13.12249633091057177, 39.60535821593503414 ) ) ;
#24802 = EDGE_CURVE ( 'NONE', #14947, #101681, #16708, .T. ) ;
#24803 = DIRECTION ( 'NONE',  ( -1.000000000000000000, -1.224606353822377258E-16, -0.000000000000000000 ) ) ;
#24804 = CIRCLE ( 'NONE', #85074, 63.00000000000000000 ) ;
#24805 = VERTEX_POINT ( 'NONE', #21162 ) ;
#24806 = EDGE_LOOP ( 'NONE', ( #22229, #51337, #41074, #66163 ) ) ;
#24807 = CARTESIAN_POINT ( 'NONE',  ( 49.06076903878732764, -36.05571625808668301, 48.12677125807188361 ) ) ;
#24808 = CARTESIAN_POINT ( 'NONE',  ( 6.507454588539320461, 41.74144728082382017, -58.94379944081024547 ) ) ;
#24809 = EDGE_CURVE ( 'NONE', #23008, #81667, #86929, .T. ) ;
#24810 = CARTESIAN_POINT ( 'NONE',  ( 36.44012392015384449, 28.20304403842013841, -11.65813649474542579 ) ) ;
#24811 = ORIENTED_EDGE ( 'NONE', *, *, #80100, .T. ) ;
#24812 = CARTESIAN_POINT ( 'NONE',  ( -95.62104924639133685, -38.35497854891799108, 61.91038439842863284 ) ) ;
#24813 = ORIENTED_EDGE ( 'NONE', *, *, #73673, .F. ) ;
#24814 =( LENGTH_UNIT ( ) NAMED_UNIT ( * ) SI_UNIT ( .MILLI., .METRE. ) );
#24815 = CARTESIAN_POINT ( 'NONE',  ( 92.11484161200772292, -38.35416711761700270, 35.82767016875815358 ) ) ;
#24816 = CARTESIAN_POINT ( 'NONE',  ( 13.46094959822379700, 24.53673296982877261, -2.096148705070425500 ) ) ;
#24817 = CARTESIAN_POINT ( 'NONE',  ( 100.8218116053281648, -60.15118524285145440, 120.1860783564071227 ) ) ;
#24818 = PLANE ( 'NONE',  #70003 ) ;
#24819 = CARTESIAN_POINT ( 'NONE',  ( -32.01559026740443414, 317.5007976905572491, -6.946860387831226724 ) ) ;
#24820 = MECHANICAL_DESIGN_GEOMETRIC_PRESENTATION_REPRESENTATION (  '', ( #90237 ), #59303 ) ;
#24821 = CARTESIAN_POINT ( 'NONE',  ( 3.858655471090992162, -67.78341364078379172, 13.12478365188160367 ) ) ;
#24822 = CARTESIAN_POINT ( 'NONE',  ( 74.08415778415269415, -60.00000000000000711, 173.0691721023521552 ) ) ;
#24823 =( GEOMETRIC_REPRESENTATION_CONTEXT ( 3 ) GLOBAL_UNCERTAINTY_ASSIGNED_CONTEXT ( ( #70761 ) ) GLOBAL_UNIT_ASSIGNED_CONTEXT ( ( #14790, #80583, #46123 ) ) REPRESENTATION_CONTEXT ( 'NONE', 'WORKASPACE' ) );
#24824 = CARTESIAN_POINT ( 'NONE',  ( 0.000000000000000000, 0.000000000000000000, 0.000000000000000000 ) ) ;
#24825 = ORIENTED_EDGE ( 'NONE', *, *, #99117, .F. ) ;
#24826 = CARTESIAN_POINT ( 'NONE',  ( 60.41798261738436082, -53.38619297810041076, 80.04375523387287217 ) ) ;
#24827 = SURFACE_SIDE_STYLE ('',( #89546 ) ) ;
#24828 = ADVANCED_FACE ( 'NONE', ( #78281 ), #37337, .T. ) ;
#24829 = CARTESIAN_POINT ( 'NONE',  ( 9.204646778667628482, -52.70222288520290022, 30.90975160907398234 ) ) ;
#24830 =( NAMED_UNIT ( * ) SI_UNIT ( $, .STERADIAN. ) SOLID_ANGLE_UNIT ( ) );
#24832 = CARTESIAN_POINT ( 'NONE',  ( -38.69275568811735866, 485.6230355318863872, -4.306148472019582840 ) ) ;
#24831 = CARTESIAN_POINT ( 'NONE',  ( -90.03305742383118115, -38.39730272076602091, -15.91574180056000465 ) ) ;
#24833 = CARTESIAN_POINT ( 'NONE',  ( -42.57247758682796501, 361.1230050982096031, 16.58080135936016930 ) ) ;
#24834 = CARTESIAN_POINT ( 'NONE',  ( -2.500000000000000444, -7.216878364870336959, -7.063244554130006847 ) ) ;
#24835 = CARTESIAN_POINT ( 'NONE',  ( -41.32787293365091585, 464.3526374298369888, 17.58299175745637299 ) ) ;
#24836 = CARTESIAN_POINT ( 'NONE',  ( 3.313708498984762052, -28.71874999999999289, -8.000000000000000000 ) ) ;
#24837 =( NAMED_UNIT ( * ) SI_UNIT ( $, .STERADIAN. ) SOLID_ANGLE_UNIT ( ) );
#24838 = EDGE_CURVE ( 'NONE', #20995, #78892, #73406, .T. ) ;
#24839 = CARTESIAN_POINT ( 'NONE',  ( -19.83463548332447601, 303.8035096162418540, 9.926734387303332241 ) ) ;
#24840 = ORIENTED_EDGE ( 'NONE', *, *, #49869, .F. ) ;
#24841 = CARTESIAN_POINT ( 'NONE',  ( 83.51337046645885209, -46.52999516907490118, 182.5729501482931028 ) ) ;
#24842 = CARTESIAN_POINT ( 'NONE',  ( 5.371950044183567030, -47.79483119409569980, 104.0625755208173473 ) ) ;
#24843 = CARTESIAN_POINT ( 'NONE',  ( -43.00000000000000000, 436.5989882784185738, 19.94133085611151301 ) ) ;
#24844 = VERTEX_POINT ( 'NONE', #70196 ) ;
#24845 = CARTESIAN_POINT ( 'NONE',  ( 0.000000000000000000, 6.123233995736770227E-16, -5.000000000000002665 ) ) ;
#24846 = CIRCLE ( 'NONE', #85107, 4.000000000000000888 ) ;
#24847 = CARTESIAN_POINT ( 'NONE',  ( 5.075566108724593128, -4.332661967060489339, -17.09624963492156269 ) ) ;
#24848 = CARTESIAN_POINT ( 'NONE',  ( 22.57792046605466041, 1.340359594676612611E-15, 0.000000000000000000 ) ) ;
#24849 = FILL_AREA_STYLE ('',( #34015 ) ) ;
#24850 = CARTESIAN_POINT ( 'NONE',  ( -41.22850014084250603, 41.73474038525400687, -53.82018319452755151 ) ) ;
#24851 = CARTESIAN_POINT ( 'NONE',  ( 6.849999999999999645, 0.000000000000000000, 8.000000000000000000 ) ) ;
#24852 = AXIS2_PLACEMENT_3D ( 'NONE', #46705, #79601, #53217 ) ;
#24853 = EDGE_CURVE ( 'NONE', #100346, #15839, #1190, .T. ) ;
#24855 = PRESENTATION_LAYER_ASSIGNMENT (  '', '', ( #86830 ) ) ;
#24854 =( NAMED_UNIT ( * ) SI_UNIT ( $, .STERADIAN. ) SOLID_ANGLE_UNIT ( ) );
#24856 = CARTESIAN_POINT ( 'NONE',  ( 38.56016536716844456, 25.19268864103764471, 12.96944895395069786 ) ) ;
#24857 = DIRECTION ( 'NONE',  ( 0.000000000000000000, 0.000000000000000000, 1.000000000000000000 ) ) ;
#24859 = CARTESIAN_POINT ( 'NONE',  ( -15.05945180436592779, 22.32467781490405656, 3.623638290633223846 ) ) ;
#24858 = CARTESIAN_POINT ( 'NONE',  ( -12.33365875486739682, -21.28429137792180370, 35.60179995485724902 ) ) ;
#24860 = CARTESIAN_POINT ( 'NONE',  ( -5.082755093536326818, -15.21875000204838457, 5.082755093536325042 ) ) ;
#24861 = CARTESIAN_POINT ( 'NONE',  ( 19.12955214649078428, 294.6724190044754437, -2.037676829496062769 ) ) ;
#24862 =( LENGTH_UNIT ( ) NAMED_UNIT ( * ) SI_UNIT ( .MILLI., .METRE. ) );
#24863 = EDGE_LOOP ( 'NONE', ( #23733, #5492, #44687, #54649 ) ) ;
#24864 = CARTESIAN_POINT ( 'NONE',  ( -17.49999999999894840, 49.48689581941425075, 62.41113125631201086 ) ) ;
#24865 = CARTESIAN_POINT ( 'NONE',  ( 7.908217798048221781, 3.084840533507049454, -7.795645399445158219 ) ) ;
#24866 = CARTESIAN_POINT ( 'NONE',  ( -3.622206768987289660, 129.3245652911131174, -4.999999999999999112 ) ) ;
#24867 = FACE_OUTER_BOUND ( 'NONE', #23911, .T. ) ;
#24868 = EDGE_CURVE ( 'NONE', #94292, #24694, #44878, .T. ) ;
#24870 = CARTESIAN_POINT ( 'NONE',  ( 69.08232371648826131, -34.58963181410090471, -22.16762132562647380 ) ) ;
#24869 = CARTESIAN_POINT ( 'NONE',  ( 31.84999999999999787, 3.309500000000003439, 4.052968581778167743E-16 ) ) ;
#24871 =( GEOMETRIC_REPRESENTATION_CONTEXT ( 3 ) GLOBAL_UNCERTAINTY_ASSIGNED_CONTEXT ( ( #68821 ) ) GLOBAL_UNIT_ASSIGNED_CONTEXT ( ( #16828, #56732, #66430 ) ) REPRESENTATION_CONTEXT ( 'NONE', 'WORKASPACE' ) );
#24872 = ORIENTED_EDGE ( 'NONE', *, *, #63117, .T. ) ;
#24873 = CARTESIAN_POINT ( 'NONE',  ( 0.000000000000000000, 6.123233995736770227E-16, -5.000000000000002665 ) ) ;
#24874 = CARTESIAN_POINT ( 'NONE',  ( -4.295862021341609882, 51.67716032263838599, 8.055692927004189485 ) ) ;
#24875 = VERTEX_POINT ( 'NONE', #102022 ) ;
#24876 = ADVANCED_FACE ( 'NONE', ( #28183 ), #80411, .F. ) ;
#24877 = CARTESIAN_POINT ( 'NONE',  ( 0.000000000000000000, 0.000000000000000000, -4.425378966781146950 ) ) ;
#24878 = DIRECTION ( 'NONE',  ( -0.000000000000000000, -1.000000000000000000, -0.000000000000000000 ) ) ;
#24879 = CIRCLE ( 'NONE', #74816, 4.000000000000001776 ) ;
#24880 = CARTESIAN_POINT ( 'NONE',  ( -98.09114130456060821, -59.99999999999997158, 69.48956915287729430 ) ) ;
#24881 = CARTESIAN_POINT ( 'NONE',  ( 29.35793203618246139, 13.99620286145417758, -42.06478814971845281 ) ) ;
#24882 = AXIS2_PLACEMENT_3D ( 'NONE', #4351, #62085, #79293 ) ;
#24883 = CARTESIAN_POINT ( 'NONE',  ( -20.21880305278369150, 304.8280059657581660, -9.005058168222323189 ) ) ;
#24884 = CIRCLE ( 'NONE', #42038, 3.309500000000007880 ) ;
#24885 = DIRECTION ( 'NONE',  ( 0.5000000000000022204, 0.8660254037844374864, -0.000000000000000000 ) ) ;
#24886 = CARTESIAN_POINT ( 'NONE',  ( -32.84088564781220043, 464.9638558180865857, 11.24476942535982005 ) ) ;
#24888 = CARTESIAN_POINT ( 'NONE',  ( -15.30754850745070250, 3.114812942706816745, 3.172027124417305721 ) ) ;
#24887 = CARTESIAN_POINT ( 'NONE',  ( 7.374560640985523996, -5.000000000000002665, -94.59600210749707117 ) ) ;
#24889 = CARTESIAN_POINT ( 'NONE',  ( -85.73826008725094994, -21.86594983941249026, 169.1353952584642286 ) ) ;
#24890 = ORIENTED_EDGE ( 'NONE', *, *, #52281, .F. ) ;
#24891 = MECHANICAL_DESIGN_GEOMETRIC_PRESENTATION_REPRESENTATION (  '', ( #97153 ), #98841 ) ;
#24892 = EDGE_CURVE ( 'NONE', #49616, #76580, #67422, .T. ) ;
#24893 = ORIENTED_EDGE ( 'NONE', *, *, #26310, .F. ) ;
#24894 = ORIENTED_EDGE ( 'NONE', *, *, #98891, .F. ) ;
#24895 = CARTESIAN_POINT ( 'NONE',  ( 28.86650669486618881, 4.898587196589411843E-16, -4.000000000000000888 ) ) ;
#24896 = CARTESIAN_POINT ( 'NONE',  ( -27.10511071441192144, -1.200000000000000030E-05, -8.806984339685890006 ) ) ;
#24897 = ORIENTED_EDGE ( 'NONE', *, *, #86985, .F. ) ;
#24898 = CARTESIAN_POINT ( 'NONE',  ( -16.55743558489286826, 303.5680260445984686, 9.876668833592542995 ) ) ;
#24899 = CARTESIAN_POINT ( 'NONE',  ( 0.000000000000000000, 48.50000000000000000, -60.00000000000000000 ) ) ;
#24900 = DIRECTION ( 'NONE',  ( 1.000000000000000000, -0.000000000000000000, -0.000000000000000000 ) ) ;
#24901 = DIRECTION ( 'NONE',  ( 0.000000000000000000, -1.000000000000000000, 0.000000000000000000 ) ) ;
#24902 = DIRECTION ( 'NONE',  ( -1.000000000000000000, -1.224606353822377258E-16, -0.000000000000000000 ) ) ;
#24903 = CARTESIAN_POINT ( 'NONE',  ( 12.86276638840208086, -5.000000000000000000, -82.77022731229634189 ) ) ;
#24904 = DIRECTION ( 'NONE',  ( -1.000000000000000000, -1.224606353822377258E-16, -0.000000000000000000 ) ) ;
#24905 = CARTESIAN_POINT ( 'NONE',  ( 109.5811936024938120, -29.99999999999993250, 174.3369879458943217 ) ) ;
#24906 = CARTESIAN_POINT ( 'NONE',  ( -109.4365443207511390, -30.00000000000002487, 178.4890703142130519 ) ) ;
#24907 = CARTESIAN_POINT ( 'NONE',  ( -63.94872130549475742, -18.62866409033716408, 72.61401410517680688 ) ) ;
#24908 = VERTEX_POINT ( 'NONE', #91696 ) ;
#24909 = CARTESIAN_POINT ( 'NONE',  ( 57.68649645722720010, 38.95207762959029907, -27.56578445358567819 ) ) ;
#24910 = CARTESIAN_POINT ( 'NONE',  ( 95.06272658828241617, -60.00000000001715250, -9.381997069871475858 ) ) ;
#24911 = ORIENTED_EDGE ( 'NONE', *, *, #4682, .F. ) ;
#24912 = CARTESIAN_POINT ( 'NONE',  ( 5.139007685894275923, -53.39669312118982702, 32.77870000778612791 ) ) ;
#24913 = CARTESIAN_POINT ( 'NONE',  ( -100.5925313966044996, -45.26526810289921343, 134.9952907213105675 ) ) ;
#24914 = CARTESIAN_POINT ( 'NONE',  ( 5.082755093536324154, -10.71875000204838457, 5.082755093536326818 ) ) ;
#24915 = CARTESIAN_POINT ( 'NONE',  ( -5.096247963242959145, -4.999999999999997335, -73.00359695307524532 ) ) ;
#24916 = VERTEX_POINT ( 'NONE', #1039 ) ;
#24917 = CARTESIAN_POINT ( 'NONE',  ( 5.432263563190379507, -29.99999999999999645, 4.731163756734333425 ) ) ;
#24918 = ORIENTED_EDGE ( 'NONE', *, *, #16049, .F. ) ;
#24919 = CARTESIAN_POINT ( 'NONE',  ( -46.00000000000000000, 488.0336798547363628, -0.8984331811837280579 ) ) ;
#24920 = STYLED_ITEM ( 'NONE', ( #74172 ), #18564 ) ;
#24921 = CARTESIAN_POINT ( 'NONE',  ( -93.31313149041179145, -59.99999999999997158, 202.5005118382522937 ) ) ;
#24922 = CARTESIAN_POINT ( 'NONE',  ( 9.677640526858340309, -57.01362214985471155, 24.47418066717162333 ) ) ;
#24923 = CARTESIAN_POINT ( 'NONE',  ( -7.188101187500001821, -21.87500000204838813, -2.977408999572651371 ) ) ;
#24924 = CARTESIAN_POINT ( 'NONE',  ( 46.00000000000000000, 460.3195313667369533, 7.040850765614101725 ) ) ;
#24925 = CARTESIAN_POINT ( 'NONE',  ( -23.21751746555280249, 28.11705169068991239, -30.70617127781034839 ) ) ;
#24926 = COLOUR_RGB ( '', 0.66274510, 0.83137255, 0.94901961) ;
#24927 = CARTESIAN_POINT ( 'NONE',  ( -11.77297503979913174, 16.33093105868367800, 9.431242781962609456 ) ) ;
#24928 = CARTESIAN_POINT ( 'NONE',  ( 5.000000000000000888, -32.16482459200685184, -4.060956965592712464 ) ) ;
#24929 = CARTESIAN_POINT ( 'NONE',  ( 32.87547266101574195, 465.6993878536675879, 10.91512469976464850 ) ) ;
#24930 = SURFACE_STYLE_USAGE ( .BOTH. , #32497 ) ;
#24931 = CARTESIAN_POINT ( 'NONE',  ( -29.50656783759020740, 297.4601869455973997, -1.429291789817593861 ) ) ;
#24932 = EDGE_CURVE ( 'NONE', #52531, #45510, #97506, .T. ) ;
#24933 = CARTESIAN_POINT ( 'NONE',  ( 86.13399275866341043, -59.99999999999998579, -13.61178955313006256 ) ) ;
#24934 = AXIS2_PLACEMENT_3D ( 'NONE', #52553, #100046, #50949 ) ;
#24935 = VECTOR ( 'NONE', #2649, 1000.000000000000000 ) ;
#24936 = CARTESIAN_POINT ( 'NONE',  ( -31.80442458140531770, -25.61247349453389788, 31.25873360126171718 ) ) ;
#24937 = B_SPLINE_CURVE_WITH_KNOTS ( 'NONE', 3,
 ( #4986, #60583, #37916, #78328 ),
 .UNSPECIFIED., .F., .F.,
 ( 4, 4 ),
 ( 6.071532165918824830E-18, 0.0006696797651157682238 ),
 .UNSPECIFIED. ) ;
#24938 = CARTESIAN_POINT ( 'NONE',  ( -3.870939636683351726, -48.78526580464421869, 104.2727580839183190 ) ) ;
#24939 = CARTESIAN_POINT ( 'NONE',  ( 41.19214003654240486, -39.52178756432360274, 39.71506556026432122 ) ) ;
#24940 = ORIENTED_EDGE ( 'NONE', *, *, #46512, .F. ) ;
#24941 = ADVANCED_FACE ( 'NONE', ( #10224 ), #63131, .T. ) ;
#24942 = DIRECTION ( 'NONE',  ( 0.3968475291348044776, 0.1146398630990837497, -0.9106973923363477219 ) ) ;
#24943 = CARTESIAN_POINT ( 'NONE',  ( -77.17977131689143278, -38.47780548771186204, 185.1846801741239688 ) ) ;
#24944 = ORIENTED_EDGE ( 'NONE', *, *, #7740, .T. ) ;
#24946 = CARTESIAN_POINT ( 'NONE',  ( 35.76379064120181539, 307.0162303970107587, 12.81051142610679960 ) ) ;
#24945 = DIRECTION ( 'NONE',  ( -0.000000000000000000, 1.000000000000000000, -0.000000000000000000 ) ) ;
#24947 = CARTESIAN_POINT ( 'NONE',  ( -13.01572312192210035, 4.315727270466244825, 7.367595652848586418 ) ) ;
#24948 = DIRECTION ( 'NONE',  ( -0.000000000000000000, -0.000000000000000000, -1.000000000000000000 ) ) ;
#24949 = CARTESIAN_POINT ( 'NONE',  ( -43.99295543319385615, 464.6035880629004282, 10.45302038923090748 ) ) ;
#24950 = CARTESIAN_POINT ( 'NONE',  ( 6.952098966025630489, 40.29466789516767022, -71.12438203459961983 ) ) ;
#24951 = CARTESIAN_POINT ( 'NONE',  ( -39.86396139244069303, 437.4902212974461690, 4.924226175446892562 ) ) ;
#24952 = CARTESIAN_POINT ( 'NONE',  ( -31.44900114652979184, 397.6410742345365747, 24.40761942929495021 ) ) ;
#24953 = CARTESIAN_POINT ( 'NONE',  ( 17.03955750629486943, 45.47802236175360235, 6.596165372994819087 ) ) ;
#24954 = CARTESIAN_POINT ( 'NONE',  ( 110.8877446216819465, -60.00000000000000711, 151.0616722329774007 ) ) ;
#24955 = CARTESIAN_POINT ( 'NONE',  ( -4.210633177350923795, -52.69376427780586170, 40.35640560465288473 ) ) ;
#24956 = CARTESIAN_POINT ( 'NONE',  ( 43.00000000000000000, 436.0987441542287115, 7.567257455462724991 ) ) ;
#24957 = ORIENTED_EDGE ( 'NONE', *, *, #37911, .T. ) ;
#24958 = EDGE_CURVE ( 'NONE', #81281, #71976, #73489, .T. ) ;
#24959 = CONICAL_SURFACE ( 'NONE', #105841, 3.309500000000007880, 0.9599310885968770357 ) ;
#24960 = CARTESIAN_POINT ( 'NONE',  ( -90.75085121845700087, -29.99999999999981171, 190.3706885672457645 ) ) ;
#24961 = VERTEX_POINT ( 'NONE', #59327 ) ;
#24962 = CARTESIAN_POINT ( 'NONE',  ( 27.10511071441176867, 36.60571256639526894, -10.05698433968634653 ) ) ;
#24963 = CARTESIAN_POINT ( 'NONE',  ( 8.642300018659518912, 129.6053270932845294, 5.000000000000000888 ) ) ;
#24964 = CARTESIAN_POINT ( 'NONE',  ( 32.01443999233854498, 362.7175041558164708, 22.60295584479863962 ) ) ;
#24965 = CARTESIAN_POINT ( 'NONE',  ( -33.20902353462242473, 484.6199955813539759, 4.299886535036168134 ) ) ;
#24966 = CARTESIAN_POINT ( 'NONE',  ( 2.977408999572651815, -24.31250000204838813, 7.188101187500000933 ) ) ;
#24967 = CARTESIAN_POINT ( 'NONE',  ( -3.505888691173200566, -0.8815391977514219768, 103.6125332151819975 ) ) ;
#24968 = ADVANCED_FACE ( 'NONE', ( #17282 ), #87229, .T. ) ;
#24969 = CARTESIAN_POINT ( 'NONE',  ( 7.392085842482234881, 40.93519689220327962, -70.13194415493437361 ) ) ;
#24970 = AXIS2_PLACEMENT_3D ( 'NONE', #57223, #82581, #26518 ) ;
#24971 = CIRCLE ( 'NONE', #49019, 4.000000000000001776 ) ;
#24972 = MECHANICAL_DESIGN_GEOMETRIC_PRESENTATION_REPRESENTATION (  '', ( #28454 ), #102409 ) ;
#24974 = ORIENTED_EDGE ( 'NONE', *, *, #103415, .F. ) ;
#24973 = CARTESIAN_POINT ( 'NONE',  ( -7.500000000000006217, 39.99999999999122480, -59.88032989330939415 ) ) ;
#24975 = CARTESIAN_POINT ( 'NONE',  ( 79.57055945170098710, -53.37446314916106616, 159.7373772712091125 ) ) ;
#24976 = VECTOR ( 'NONE', #79270, 1000.000000000000000 ) ;
#24977 = CARTESIAN_POINT ( 'NONE',  ( 89.99999999999997158, -52.00000000000000000, 194.0238439516549818 ) ) ;
#24978 = ORIENTED_EDGE ( 'NONE', *, *, #104303, .T. ) ;
#24979 = CARTESIAN_POINT ( 'NONE',  ( -0.2961983223192701797, 12.99322937314420834, -51.71652672840411924 ) ) ;
#24980 = CARTESIAN_POINT ( 'NONE',  ( 0.000000000000000000, 0.000000000000000000, -8.000000000000000000 ) ) ;
#24981 = CARTESIAN_POINT ( 'NONE',  ( 0.4964154566687888903, -8.859816792613642633, 0.6543471694412403838 ) ) ;
#24982 = AXIS2_PLACEMENT_3D ( 'NONE', #38623, #61298, #62368 ) ;
#24983 = CARTESIAN_POINT ( 'NONE',  ( 73.50474219086036953, -59.99999999999997158, -24.84696050693406022 ) ) ;
#24984 = CARTESIAN_POINT ( 'NONE',  ( -32.88644894021390996, 356.0147610692134776, 21.80302539000014050 ) ) ;
#24985 = FACE_OUTER_BOUND ( 'NONE', #1707, .T. ) ;
#24986 = VERTEX_POINT ( 'NONE', #50157 ) ;
#24987 =( NAMED_UNIT ( * ) PLANE_ANGLE_UNIT ( ) SI_UNIT ( $, .RADIAN. ) );
#24988 = DIRECTION ( 'NONE',  ( -0.5735764363510494901, -0.8191520442889894671, 0.000000000000000000 ) ) ;
#24989 = CARTESIAN_POINT ( 'NONE',  ( 7.109733078360420677, 41.69026692163959069, -59.69141567447950081 ) ) ;
#24990 = CARTESIAN_POINT ( 'NONE',  ( 86.67822773504592249, -50.11939951311777719, 191.5819010267896374 ) ) ;
#24991 = CARTESIAN_POINT ( 'NONE',  ( 1.249862292819393650, 34.73247132126252978, -28.18210478855811019 ) ) ;
#24992 = CARTESIAN_POINT ( 'NONE',  ( -2.977408999572654480, -28.62500000204838457, 7.188101187499999156 ) ) ;
#24993 = CARTESIAN_POINT ( 'NONE',  ( 21.57322603007769146, -26.73334242327893406, 37.22254679213403961 ) ) ;
#24994 = PRESENTATION_STYLE_ASSIGNMENT (( #64898 ) ) ;
#24995 = CARTESIAN_POINT ( 'NONE',  ( 7.561984444596827615, 52.15257306799382775, 2.009849713221146139 ) ) ;
#24996 = DIRECTION ( 'NONE',  ( 0.000000000000000000, -1.000000000000000000, 0.000000000000000000 ) ) ;
#24997 = APPLICATION_PROTOCOL_DEFINITION ( 'draft international standard', 'automotive_design', 1998, #87919 ) ;
#24998 = DIRECTION ( 'NONE',  ( -0.000000000000000000, 0.5000000000000008882, 0.8660254037844381525 ) ) ;
#24999 = EDGE_LOOP ( 'NONE', ( #105560, #4318, #53197, #5521, #42298 ) ) ;
#25000 = CARTESIAN_POINT ( 'NONE',  ( -34.89857526195044102, 437.7187790665907983, 4.586527422595223058 ) ) ;
#25002 = FACE_OUTER_BOUND ( 'NONE', #26825, .T. ) ;
#25001 =( BOUNDED_SURFACE ( )  B_SPLINE_SURFACE ( 2, 3, ( 
 ( #37788, #45321, #53916, #27580, #45846, #93865, #59926, #51794, #28633, #12924, #84707, #61516, #10791, #70649, #92791, #68540, #43710, #78718, #78204, #35662, #60978, #18953 ),
 ( #101429, #86327, #60460, #93338, #19488, #52866, #94408, #52325, #103545, #85239, #53409, #11325, #62057, #44255, #101946, #77146, #3262, #36203, #4854, #12393, #103024, #69070 ),
 ( #20024, #4319, #85796, #11868, #44797, #77686, #37254, #3796, #36733, #70116, #69597, #29179, #94944, #21080, #87899, #22116, #13981, #6958, #5890, #40391, #30748, #56562 ) ),
 .UNSPECIFIED., .F., .F., .F. ) 
 B_SPLINE_SURFACE_WITH_KNOTS ( ( 3, 3 ),
 ( 4, 2, 2, 2, 2, 2, 2, 2, 2, 2, 4 ),
 ( 0.000000000000000000, 1.000000000000000000 ),
 ( 3.594963135488010497, 3.839346969278153665, 4.450306553753511807, 5.061266138228869949, 5.672225722704228090, 6.283185307179586232, 6.894144891654944374, 7.505104476130302515, 8.116064060605660657, 8.727023645081018799, 8.971407478871162411 ),
 .UNSPECIFIED. ) 
 GEOMETRIC_REPRESENTATION_ITEM ( )  RATIONAL_B_SPLINE_SURFACE ( (
 ( 1.000000000000000000, 1.000000000000000000, 1.000000000000000000, 1.000000000000000000, 1.000000000000000000, 1.000000000000000000, 1.000000000000000000, 1.000000000000000000, 1.000000000000000000, 1.000000000000000000, 1.000000000000000000, 1.000000000000000000, 1.000000000000000000, 1.000000000000000000, 1.000000000000000000, 1.000000000000000000, 1.000000000000000000, 1.000000000000000000, 1.000000000000000000, 1.000000000000000000, 1.000000000000000000, 1.000000000000000000),
 ( 1.857142857142858317, 1.857142857142858317, 1.857142857142858317, 1.857142857142858317, 1.857142857142858317, 1.857142857142858317, 1.857142857142858317, 1.857142857142858317, 1.857142857142858317, 1.857142857142858317, 1.857142857142858317, 1.857142857142858317, 1.857142857142858317, 1.857142857142858317, 1.857142857142858317, 1.857142857142858317, 1.857142857142858317, 1.857142857142858317, 1.857142857142858317, 1.857142857142858317, 1.857142857142858317, 1.857142857142858317),
 ( 1.000000000000000000, 1.000000000000000000, 1.000000000000000000, 1.000000000000000000, 1.000000000000000000, 1.000000000000000000, 1.000000000000000000, 1.000000000000000000, 1.000000000000000000, 1.000000000000000000, 1.000000000000000000, 1.000000000000000000, 1.000000000000000000, 1.000000000000000000, 1.000000000000000000, 1.000000000000000000, 1.000000000000000000, 1.000000000000000000, 1.000000000000000000, 1.000000000000000000, 1.000000000000000000, 1.000000000000000000) ) ) 
 REPRESENTATION_ITEM ( '' )  SURFACE ( )  );
#25003 = CIRCLE ( 'NONE', #40449, 4.000000000000000888 ) ;
#25004 = FILL_AREA_STYLE ('',( #90247 ) ) ;
#25005 = CARTESIAN_POINT ( 'NONE',  ( 13.14242568359541607, 42.00000000000000000, -92.43215185542086942 ) ) ;
#25006 = EDGE_CURVE ( 'NONE', #2343, #13350, #9155, .T. ) ;
#25007 = PRODUCT_DEFINITION_FORMATION_WITH_SPECIFIED_SOURCE ( 'ANY', '', #99384, .NOT_KNOWN. ) ;
#25008 = EDGE_LOOP ( 'NONE', ( #91816, #30078, #82145, #34902, #33532 ) ) ;
#25009 =( NAMED_UNIT ( * ) SI_UNIT ( $, .STERADIAN. ) SOLID_ANGLE_UNIT ( ) );
#25010 = DIRECTION ( 'NONE',  ( -0.000000000000000000, 1.000000000000000000, -0.000000000000000000 ) ) ;
#25011 = CARTESIAN_POINT ( 'NONE',  ( 114.2261582128081585, -57.67133197082363694, 172.3102140180382378 ) ) ;
#25012 = ADVANCED_FACE ( 'NONE', ( #9684 ), #3263, .F. ) ;
#25013 = CARTESIAN_POINT ( 'NONE',  ( 35.96642943166446571, 464.0782432590749522, 19.48772549671354781 ) ) ;
#25014 = CARTESIAN_POINT ( 'NONE',  ( 19.00000000000001066, -3.999999999999999112, -1.500000000000000000 ) ) ;
#25015 = FACE_OUTER_BOUND ( 'NONE', #19145, .T. ) ;
#25016 = FACE_OUTER_BOUND ( 'NONE', #38984, .T. ) ;
#25017 = CARTESIAN_POINT ( 'NONE',  ( -77.65926509950536172, -59.99999999999999289, 192.1015713222786871 ) ) ;
#25018 = ADVANCED_FACE ( 'NONE', ( #67942 ), #42401, .F. ) ;
#25019 = CARTESIAN_POINT ( 'NONE',  ( -20.97754405179121662, 294.8763868968453608, 9.942224931492262385 ) ) ;
#25020 = PRESENTATION_STYLE_ASSIGNMENT (( #668 ) ) ;
#25021 = CARTESIAN_POINT ( 'NONE',  ( -60.66923414622394262, 50.00000000000000000, 17.93278245653412384 ) ) ;
#25022 = CARTESIAN_POINT ( 'NONE',  ( -84.07736508537209374, -57.42622439993449746, 190.7929976290621710 ) ) ;
#25023 = EDGE_LOOP ( 'NONE', ( #25639, #64621 ) ) ;
#25024 = CARTESIAN_POINT ( 'NONE',  ( 20.21880305278368439, 304.8280059657581660, -9.005058168222323189 ) ) ;
#25025 = EDGE_CURVE ( 'NONE', #53057, #49120, #90628, .T. ) ;
#25026 = VERTEX_POINT ( 'NONE', #8798 ) ;
#25027 = CARTESIAN_POINT ( 'NONE',  ( 16.01537606005197389, 3.832707337348138843, 1.292662844563333246 ) ) ;
#25028 = VECTOR ( 'NONE', #84765, 1000.000000000000000 ) ;
#25029 = CARTESIAN_POINT ( 'NONE',  ( -85.73889581639751611, -52.73376626706190251, -5.626253082883039269 ) ) ;
#25030 = CARTESIAN_POINT ( 'NONE',  ( -4.524610880512274669, -11.34578236400882112, -9.835134842096833196 ) ) ;
#25031 =( LENGTH_UNIT ( ) NAMED_UNIT ( * ) SI_UNIT ( .MILLI., .METRE. ) );
#25032 = VERTEX_POINT ( 'NONE', #9850 ) ;
#25033 = AXIS2_PLACEMENT_3D ( 'NONE', #43508, #92050, #25777 ) ;
#25034 = DIRECTION ( 'NONE',  ( 1.000000000000000000, 1.224606353822377258E-16, 0.000000000000000000 ) ) ;
#25035 = CARTESIAN_POINT ( 'NONE',  ( 13.02391187303469344, 23.74004891468554490, -4.319434719146233448 ) ) ;
#25036 = CARTESIAN_POINT ( 'NONE',  ( 2.083846472846741813E-15, -1.734723475976807094E-15, 17.01589776168603407 ) ) ;
#25037 = DIRECTION ( 'NONE',  ( -1.000000000000000000, -0.000000000000000000, -0.000000000000000000 ) ) ;
#25038 = CARTESIAN_POINT ( 'NONE',  ( -48.21571607899795708, -30.00000000000001066, -35.59733477200444440 ) ) ;
#25039 = CARTESIAN_POINT ( 'NONE',  ( -76.07387704635563352, -39.49473305854762373, 125.2008553257723804 ) ) ;
#25040 = MECHANICAL_DESIGN_GEOMETRIC_PRESENTATION_REPRESENTATION (  '', ( #14679 ), #85310 ) ;
#25041 = VERTEX_POINT ( 'NONE', #82693 ) ;
#25042 = CARTESIAN_POINT ( 'NONE',  ( 64.81979848413079992, -29.99999999999996803, 107.4021778588664375 ) ) ;
#25043 = CARTESIAN_POINT ( 'NONE',  ( 7.551892080562058851, 88.00987702539381985, 2.647003822403971807 ) ) ;
#25044 = CARTESIAN_POINT ( 'NONE',  ( 111.6759504537514829, -57.67120741609547707, 140.8126062134855658 ) ) ;
#25045 = PRESENTATION_LAYER_ASSIGNMENT (  '', '', ( #71512 ) ) ;
#25047 = ORIENTED_EDGE ( 'NONE', *, *, #67216, .T. ) ;
#25046 = AXIS2_PLACEMENT_3D ( 'NONE', #23, #58299, #82577 ) ;
#25048 = CARTESIAN_POINT ( 'NONE',  ( 0.2578475836320709980, 6.890627091270373761, 1.065083781909174077 ) ) ;
#25049 = CARTESIAN_POINT ( 'NONE',  ( 70.89460441624491693, 6.975173280561618775E-15, 0.000000000000000000 ) ) ;
#25050 = VERTEX_POINT ( 'NONE', #33630 ) ;
#25051 = VECTOR ( 'NONE', #42541, 999.9999999999998863 ) ;
#25052 = CARTESIAN_POINT ( 'NONE',  ( 0.000000000000000000, 34.00000000000000000, 0.000000000000000000 ) ) ;
#25053 = SURFACE_STYLE_FILL_AREA ( #82730 ) ;
#25054 = CARTESIAN_POINT ( 'NONE',  ( 15.43459503591739690, 44.00330752595467487, 5.765235879371150673 ) ) ;
#25055 = CARTESIAN_POINT ( 'NONE',  ( -5.082755093536326818, -15.21875000204838457, 5.082755093536325042 ) ) ;
#25056 = CARTESIAN_POINT ( 'NONE',  ( 19.50011280463133545, 50.00000000000000000, 59.90639435984937222 ) ) ;
#25057 = PRESENTATION_LAYER_ASSIGNMENT (  '', '', ( #83602 ) ) ;
#25058 = CARTESIAN_POINT ( 'NONE',  ( 9.483056940782031319, 82.55612209893422460, -3.177305548492596721 ) ) ;
#25059 = FACE_OUTER_BOUND ( 'NONE', #79029, .T. ) ;
#25060 = DIRECTION ( 'NONE',  ( 0.000000000000000000, 1.000000000000000000, 0.000000000000000000 ) ) ;
#25061 = ADVANCED_FACE ( 'NONE', ( #25015 ), #25565, .F. ) ;
#25062 = ORIENTED_EDGE ( 'NONE', *, *, #30294, .T. ) ;
#25063 = CARTESIAN_POINT ( 'NONE',  ( -7.029557160387159165, 41.29102236549713467, -70.49405803162696316 ) ) ;
#25064 = CARTESIAN_POINT ( 'NONE',  ( 31.02192573903809958, -39.48738554629173336, 33.50131639203233647 ) ) ;
#25065 = CARTESIAN_POINT ( 'NONE',  ( 33.83623258902267850, 330.0920146021361461, -2.810346497816497369 ) ) ;
#25066 = VERTEX_POINT ( 'NONE', #9314 ) ;
#25067 = EDGE_CURVE ( 'NONE', #7599, #26910, #34712, .T. ) ;
#25068 = ADVANCED_FACE ( 'NONE', ( #90257 ), #100994, .T. ) ;
#25069 = ORIENTED_EDGE ( 'NONE', *, *, #90324, .T. ) ;
#25071 = CARTESIAN_POINT ( 'NONE',  ( -9.742892617409784961, -5.000000000000000888, 2.583889972064361107 ) ) ;
#25070 = CARTESIAN_POINT ( 'NONE',  ( 0.01678220608715748352, 0.7854258608507237449, 7.999999999999998224 ) ) ;
#25072 = CARTESIAN_POINT ( 'NONE',  ( 20.06460911473395470, 302.7901891854631913, -10.01309647120555013 ) ) ;
#25073 = CARTESIAN_POINT ( 'NONE',  ( -2.100000000000004530, 0.000000000000000000, 0.000000000000000000 ) ) ;
#25074 = DIRECTION ( 'NONE',  ( -0.000000000000000000, -0.000000000000000000, -1.000000000000000000 ) ) ;
#25075 = DIRECTION ( 'NONE',  ( -1.850371707710400463E-15, 0.000000000000000000, 1.000000000000000000 ) ) ;
#25076 = CARTESIAN_POINT ( 'NONE',  ( -35.85615118283770641, 463.5955582468936882, 19.55698106745636977 ) ) ;
#25077 = EDGE_LOOP ( 'NONE', ( #42233, #105740, #57018, #55842 ) ) ;
#25078 = CARTESIAN_POINT ( 'NONE',  ( 92.74028942188910207, -60.00000000000002132, -6.481442454470473180 ) ) ;
#25079 = CARTESIAN_POINT ( 'NONE',  ( -9.041225629235841055, 45.95386998337555440, 14.35441598012794628 ) ) ;
#25080 = CARTESIAN_POINT ( 'NONE',  ( -15.79974202274673090, -1.614185661296035468, 14.91351826467123587 ) ) ;
#25081 = CARTESIAN_POINT ( 'NONE',  ( 17.08544069068336668, 304.5690947107618740, -10.06009145438461161 ) ) ;
#25082 = AXIS2_PLACEMENT_3D ( 'NONE', #31377, #23270, #72840 ) ;
#25083 = CARTESIAN_POINT ( 'NONE',  ( 6.999999999999999112, 0.000000000000000000, 0.000000000000000000 ) ) ;
#25084 = VERTEX_POINT ( 'NONE', #42224 ) ;
#25085 = ADVANCED_FACE ( 'NONE', ( #33111 ), #50315, .T. ) ;
#25086 = CARTESIAN_POINT ( 'NONE',  ( -36.32038103943577312, 28.15992945091319655, 12.39840696908056294 ) ) ;
#25087 = ORIENTED_EDGE ( 'NONE', *, *, #92182, .T. ) ;
#25088 = ORIENTED_EDGE ( 'NONE', *, *, #11819, .T. ) ;
#25089 = SURFACE_STYLE_USAGE ( .BOTH. , #81160 ) ;
#25090 = CARTESIAN_POINT ( 'NONE',  ( 0.4037800551813707228, 4.058962678540093627, -5.969670414742686226 ) ) ;
#25091 = CARTESIAN_POINT ( 'NONE',  ( 0.000000000000000000, 0.000000000000000000, 0.000000000000000000 ) ) ;
#25092 = CARTESIAN_POINT ( 'NONE',  ( 83.13711729878457390, -37.83719930664555164, -3.006607161073368228 ) ) ;
#25093 = CARTESIAN_POINT ( 'NONE',  ( -37.64383558481692660, 375.6724030661061988, 4.848939086997407166 ) ) ;
#25094 = CARTESIAN_POINT ( 'NONE',  ( -4.410865297923724171, -68.79849255806507813, 13.71221591202026246 ) ) ;
#25095 = CARTESIAN_POINT ( 'NONE',  ( 12.50000000000000533, 39.74439965334176605, -64.98731535703404916 ) ) ;
#25096 = ORIENTED_EDGE ( 'NONE', *, *, #89191, .T. ) ;
#25097 = EDGE_CURVE ( 'NONE', #84262, #73855, #83738, .T. ) ;
#25098 = CARTESIAN_POINT ( 'NONE',  ( -9.326356278839186942, 44.07198551910767037, 13.35271616244774151 ) ) ;
#25099 = VERTEX_POINT ( 'NONE', #24501 ) ;
#25100 = CARTESIAN_POINT ( 'NONE',  ( -7.141975279401744814, -2.999999999999884537, -70.98863559355044117 ) ) ;
#25101 = CARTESIAN_POINT ( 'NONE',  ( -84.83517221518071949, -38.71298880862309488, 198.3806444392209301 ) ) ;
#25102 =( NAMED_UNIT ( * ) SI_UNIT ( $, .STERADIAN. ) SOLID_ANGLE_UNIT ( ) );
#25103 = ADVANCED_FACE ( 'NONE', ( #48714, #91334, #75110, #17974, #17449 ), #83735, .F. ) ;
#25105 = VERTEX_POINT ( 'NONE', #58963 ) ;
#25104 = CARTESIAN_POINT ( 'NONE',  ( -74.60970371152679093, -59.99999999999997158, 134.6542277587269894 ) ) ;
#25106 = CARTESIAN_POINT ( 'NONE',  ( 67.34244021800664370, -56.85823850909442712, 103.2051531002039155 ) ) ;
#25107 = PRESENTATION_LAYER_ASSIGNMENT (  '', '', ( #18171 ) ) ;
#25108 = ORIENTED_EDGE ( 'NONE', *, *, #70750, .T. ) ;
#25109 = CARTESIAN_POINT ( 'NONE',  ( -2.977408999572650039, -29.18750000204839523, -7.188101187500000933 ) ) ;
#25110 = CARTESIAN_POINT ( 'NONE',  ( -94.50453298674098335, -57.65443526055588563, -11.14264577307068294 ) ) ;
#25111 =( GEOMETRIC_REPRESENTATION_CONTEXT ( 3 ) GLOBAL_UNCERTAINTY_ASSIGNED_CONTEXT ( ( #25736 ) ) GLOBAL_UNIT_ASSIGNED_CONTEXT ( ( #63563, #12853, #96457 ) ) REPRESENTATION_CONTEXT ( 'NONE', 'WORKASPACE' ) );
#25112 = ORIENTED_EDGE ( 'NONE', *, *, #42507, .F. ) ;
#25113 = B_SPLINE_CURVE_WITH_KNOTS ( 'NONE', 3,
 ( #30148, #7419, #64624, #39297, #81306, #23120, #63032, #54914 ),
 .UNSPECIFIED., .F., .F.,
 ( 4, 2, 2, 4 ),
 ( 0.000000000000000000, 0.0002494395879357617159, 0.0004988791758715234318, 0.0009977583517430481646 ),
 .UNSPECIFIED. ) ;
#25114 = DIRECTION ( 'NONE',  ( -1.000000000000000000, -1.224606353822377258E-16, -0.000000000000000000 ) ) ;
#25115 = PRESENTATION_LAYER_ASSIGNMENT (  '', '', ( #30275 ) ) ;
#25116 = CIRCLE ( 'NONE', #105990, 5.000000000000011546 ) ;
#25117 = CARTESIAN_POINT ( 'NONE',  ( -83.88445482477082749, -59.99999999999995737, 191.6821729358339610 ) ) ;
#25118 = CARTESIAN_POINT ( 'NONE',  ( 5.656854249492378806, -23.37500000409677270, 5.656854249492381470 ) ) ;
#25119 = AXIS2_PLACEMENT_3D ( 'NONE', #36381, #85971, #29341 ) ;
#25120 = DIRECTION ( 'NONE',  ( 0.000000000000000000, 0.000000000000000000, 1.000000000000000000 ) ) ;
#25121 = VECTOR ( 'NONE', #2325, 1000.000000000000000 ) ;
#25122 = FACE_OUTER_BOUND ( 'NONE', #65, .T. ) ;
#25123 = CONICAL_SURFACE ( 'NONE', #88851, 4.000000000000001776, 0.9599310885968774798 ) ;
#25124 = DIRECTION ( 'NONE',  ( -0.2266275398141938957, 0.09415776302217854221, 0.9694195551258625310 ) ) ;
#25125 = CARTESIAN_POINT ( 'NONE',  ( -9.999586304451581142, 7.500591597932315224, 0.000000000000000000 ) ) ;
#25126 = CARTESIAN_POINT ( 'NONE',  ( -13.68764148674883430, 294.5450735065955996, 9.871802096439328267 ) ) ;
#25127 = CARTESIAN_POINT ( 'NONE',  ( 0.000000000000000000, 0.000000000000000000, 0.000000000000000000 ) ) ;
#25128 = CARTESIAN_POINT ( 'NONE',  ( -3.997425403567602675, 15.99999999372935022, -9.168149550321206931 ) ) ;
#25129 = ORIENTED_EDGE ( 'NONE', *, *, #5359, .F. ) ;
#25131 = AXIS2_PLACEMENT_3D ( 'NONE', #65486, #57902, #98375 ) ;
#25130 = FACE_OUTER_BOUND ( 'NONE', #72917, .T. ) ;
#25132 = CARTESIAN_POINT ( 'NONE',  ( 45.59999999999999432, 1.533819458162526451E-15, 0.000000000000000000 ) ) ;
#25133 = VECTOR ( 'NONE', #73494, 1000.000000000000000 ) ;
#25134 = CARTESIAN_POINT ( 'NONE',  ( -5.000000000000000888, -51.57177412348296031, 8.340224860101702831 ) ) ;
#25135 = CARTESIAN_POINT ( 'NONE',  ( -97.30680262177158113, -30.00000000000000711, 190.9787031741742567 ) ) ;
#25136 = EDGE_CURVE ( 'NONE', #59923, #74667, #92360, .T. ) ;
#25137 = DIRECTION ( 'NONE',  ( 0.000000000000000000, 0.000000000000000000, 1.000000000000000000 ) ) ;
#25138 = CARTESIAN_POINT ( 'NONE',  ( 63.27202089354346271, -57.67868661202842162, 119.5670882431399491 ) ) ;
#25140 = CARTESIAN_POINT ( 'NONE',  ( -7.748578893116479627, 5.864678312211424327, 4.493043914853660503 ) ) ;
#25139 = CARTESIAN_POINT ( 'NONE',  ( -1.098501441293660896, 25.84241065926105207, -38.88218280404267091 ) ) ;
#25141 = EDGE_CURVE ( 'NONE', #80162, #34787, #15364, .T. ) ;
#25142 = EDGE_CURVE ( 'NONE', #96921, #81667, #100464, .T. ) ;
#25143 = CARTESIAN_POINT ( 'NONE',  ( 5.404552530375831054, -21.70842134127357426, -38.54708377808628939 ) ) ;
#25144 = SURFACE_STYLE_USAGE ( .BOTH. , #98977 ) ;
#25145 = SURFACE_SIDE_STYLE ('',( #58561 ) ) ;
#25146 = CARTESIAN_POINT ( 'NONE',  ( -38.60657232694759955, -59.99999999999999289, 50.24250451447390020 ) ) ;
#25147 = CARTESIAN_POINT ( 'NONE',  ( -1.000000000001111777, -69.59657292934927852, 12.76848391599230759 ) ) ;
#25148 = CARTESIAN_POINT ( 'NONE',  ( 0.3378228332940266809, 45.31577368508814629, -18.71500938954003601 ) ) ;
#25149 = B_SPLINE_CURVE_WITH_KNOTS ( 'NONE', 3,
 ( #77246, #13015, #70217, #76699, #52968, #68643, #86948, #85891, #3360, #45423, #21694, #36305, #69691, #4954, #45942, #3891, #78823, #60549 ),
 .UNSPECIFIED., .F., .F.,
 ( 4, 2, 2, 2, 2, 2, 2, 2, 4 ),
 ( 0.000000000000000000, 0.06250000000000005551, 0.1250000000000001110, 0.1875000000000000833, 0.2500000000000000555, 0.3125000000000000555, 0.3750000000000000555, 0.4375000000000000555, 0.5000000000000000000 ),
 .UNSPECIFIED. ) ;
#25150 = CARTESIAN_POINT ( 'NONE',  ( -86.94464142740093848, -28.02521910232672653, 186.6926187431337212 ) ) ;
#25151 = ORIENTED_EDGE ( 'NONE', *, *, #56144, .T. ) ;
#25152 = CARTESIAN_POINT ( 'NONE',  ( 19.49662282918525591, 49.99981527065408216, 59.98277621002879556 ) ) ;
#25153 = CARTESIAN_POINT ( 'NONE',  ( 30.59355846058030082, 12.96027739219345243, 41.71512601614514182 ) ) ;
#25154 = CARTESIAN_POINT ( 'NONE',  ( -7.105946766212089649, -35.99435547297646565, 29.87904593495951389 ) ) ;
#25155 = ADVANCED_FACE ( 'NONE', ( #59496 ), #102940, .T. ) ;
#25156 = CIRCLE ( 'NONE', #68172, 14.00000000000000000 ) ;
#25157 = CARTESIAN_POINT ( 'NONE',  ( 0.000000000000000000, -80.00000000000000000, 41.00000000000000000 ) ) ;
#25159 = CARTESIAN_POINT ( 'NONE',  ( 1.372706959323941156, -69.65664221933762690, 12.80275162964094804 ) ) ;
#25158 = CARTESIAN_POINT ( 'NONE',  ( -0.2259792476677738859, -7.636022678937434804, -6.470294263593375561 ) ) ;
#25160 = ORIENTED_EDGE ( 'NONE', *, *, #68044, .F. ) ;
#25161 = CARTESIAN_POINT ( 'NONE',  ( 25.85852276869992394, 35.03485039546205826, 8.998477900693142573 ) ) ;
#25162 = PRESENTATION_LAYER_ASSIGNMENT (  '', '', ( #81374 ) ) ;
#25163 = CARTESIAN_POINT ( 'NONE',  ( -6.108201232855833496, -4.361520614648816796, -16.81796607653734910 ) ) ;
#25164 = CARTESIAN_POINT ( 'NONE',  ( 15.99032464848354884, 34.48495609265440720, 24.06104333071695223 ) ) ;
#25165 = CARTESIAN_POINT ( 'NONE',  ( 34.73933834331388937, 301.1522517439193507, -8.582803626330811397 ) ) ;
#25166 = DIRECTION ( 'NONE',  ( 1.000000000000000000, 0.000000000000000000, 0.000000000000000000 ) ) ;
#25167 = DIRECTION ( 'NONE',  ( 1.000000000000000000, 0.000000000000000000, 0.000000000000000000 ) ) ;
#25168 =( LENGTH_UNIT ( ) NAMED_UNIT ( * ) SI_UNIT ( .MILLI., .METRE. ) );
#25169 = CARTESIAN_POINT ( 'NONE',  ( 104.4271199315001013, -14.21045842199428932, 141.4133776126798523 ) ) ;
#25170 = DIRECTION ( 'NONE',  ( -1.224646799147349509E-16, 0.000000000000000000, -1.000000000000000000 ) ) ;
#25171 = VERTEX_POINT ( 'NONE', #73520 ) ;
#25172 = DIRECTION ( 'NONE',  ( -1.000000000000000000, -1.224606353822377258E-16, -0.000000000000000000 ) ) ;
#25173 = CARTESIAN_POINT ( 'NONE',  ( 50.94745919686198476, 50.00000000000000000, -37.05882352941176094 ) ) ;
#25174 = SURFACE_STYLE_FILL_AREA ( #74739 ) ;
#25175 = CARTESIAN_POINT ( 'NONE',  ( 93.97977184163765685, 1.030564683017419500E-14, 0.000000000000000000 ) ) ;
#25176 = CARTESIAN_POINT ( 'NONE',  ( 43.63769803434600902, 379.1446434011715496, 14.87092719457540113 ) ) ;
#25177 = DIRECTION ( 'NONE',  ( -0.000000000000000000, 1.000000000000000000, -0.000000000000000000 ) ) ;
#25178 = ORIENTED_EDGE ( 'NONE', *, *, #22687, .F. ) ;
#25179 = CIRCLE ( 'NONE', #6199, 5.000000000000001776 ) ;
#25180 = CARTESIAN_POINT ( 'NONE',  ( -21.07176076349410820, 305.0225856740397035, 9.973527527123424719 ) ) ;
#25181 = ORIENTED_EDGE ( 'NONE', *, *, #8900, .T. ) ;
#25182 = CARTESIAN_POINT ( 'NONE',  ( 34.22523139975753281, 485.0580393423874170, -1.439874417901405135 ) ) ;
#25183 = SURFACE_STYLE_USAGE ( .BOTH. , #56972 ) ;
#25184 = CARTESIAN_POINT ( 'NONE',  ( 32.72014288347716615, 485.4774019870154120, 6.282418260585018288 ) ) ;
#25185 = VERTEX_POINT ( 'NONE', #106421 ) ;
#25186 = CIRCLE ( 'NONE', #2746, 5.000000000000001776 ) ;
#25187 = CARTESIAN_POINT ( 'NONE',  ( 56.06936961865346802, 48.00000000000000000, -33.41736086621895652 ) ) ;
#25188 = CARTESIAN_POINT ( 'NONE',  ( 5.978750298146925601, -13.03636037196968367, 13.21647969580668480 ) ) ;
#25189 = CARTESIAN_POINT ( 'NONE',  ( -62.16730077632442431, -59.99999999996094857, 116.6023417739558425 ) ) ;
#25190 = CARTESIAN_POINT ( 'NONE',  ( 46.00000000000000000, 437.9690125970931831, 14.09127711025715080 ) ) ;
#25191 = ORIENTED_EDGE ( 'NONE', *, *, #17831, .F. ) ;
#25192 = CARTESIAN_POINT ( 'NONE',  ( 95.52617796645279213, -59.99999999999993605, 202.5679377223947029 ) ) ;
#25193 = AXIS2_PLACEMENT_3D ( 'NONE', #83847, #51477, #84392 ) ;
#25195 = CARTESIAN_POINT ( 'NONE',  ( 19.33195322576188246, -53.39568836721204548, 33.25297745405755734 ) ) ;
#25194 = CARTESIAN_POINT ( 'NONE',  ( -80.26890325034752038, -59.99999999999982947, 200.1011331233653721 ) ) ;
#25197 = CARTESIAN_POINT ( 'NONE',  ( -8.572527594031464315E-16, 61.50000000000000000, 6.999999999999992895 ) ) ;
#25196 = UNCERTAINTY_MEASURE_WITH_UNIT (LENGTH_MEASURE( 1.000000000000000082E-05 ), #83193, 'distance_accuracy_value', 'NONE');
#25198 = CARTESIAN_POINT ( 'NONE',  ( 0.4145533582058317235, 53.41936724997551522, -10.18222875895670576 ) ) ;
#25199 = ADVANCED_FACE ( 'NONE', ( #16910 ), #32579, .T. ) ;
#25200 = CARTESIAN_POINT ( 'NONE',  ( -41.65521368984826722, -25.70102211639285628, 36.84734771239409667 ) ) ;
#25201 = CARTESIAN_POINT ( 'NONE',  ( -38.20903166377354410, 18.64284798593150683, 4.122114450676773956 ) ) ;
#25202 = COLOUR_RGB ( '', 0.72549020, 0.75294118, 0.79215686) ;
#25203 = ORIENTED_EDGE ( 'NONE', *, *, #101597, .F. ) ;
#25204 = VECTOR ( 'NONE', #51304, 1000.000000000000000 ) ;
#25205 = AXIS2_PLACEMENT_3D ( 'NONE', #7624, #99840, #65356 ) ;
#25206 = LINE ( 'NONE', #26286, #9441 ) ;
#25207 = CARTESIAN_POINT ( 'NONE',  ( 20.52350613252515643, 304.8999024697870937, 9.947223320822450532 ) ) ;
#25208 = AXIS2_PLACEMENT_3D ( 'NONE', #40264, #21987, #64037 ) ;
#25209 = CARTESIAN_POINT ( 'NONE',  ( -1.469576158976823947E-15, -28.06250000409677270, 8.000000000000000000 ) ) ;
#25210 = DIRECTION ( 'NONE',  ( 0.000000000000000000, 0.000000000000000000, -1.000000000000000000 ) ) ;
#25211 = VERTEX_POINT ( 'NONE', #144 ) ;
#25212 = CARTESIAN_POINT ( 'NONE',  ( 4.526657684027820316, -47.90665221903877580, 103.5746540667394555 ) ) ;
#25213 = ORIENTED_EDGE ( 'NONE', *, *, #70206, .F. ) ;
#25214 = CARTESIAN_POINT ( 'NONE',  ( 81.46863496367946311, -30.00000000000010303, -3.011595879706462142 ) ) ;
#25215 = CARTESIAN_POINT ( 'NONE',  ( 46.81211797174984923, 13.24924033427095971, 15.90734432316328117 ) ) ;
#25216 = CARTESIAN_POINT ( 'NONE',  ( 24.42526964689314184, 25.46411340096914699, -31.59704496624418724 ) ) ;
#25217 = PRESENTATION_LAYER_ASSIGNMENT (  '', '', ( #52733 ) ) ;
#25218 = CARTESIAN_POINT ( 'NONE',  ( 83.32745884141306192, -29.99999999999999289, 45.50778505098266891 ) ) ;
#25219 = ADVANCED_FACE ( 'NONE', ( #65974 ), #6211, .T. ) ;
#25220 = CARTESIAN_POINT ( 'NONE',  ( 7.618844049274128949, 101.8276410107053636, 2.450177051822848284 ) ) ;
#25221 = ORIENTED_EDGE ( 'NONE', *, *, #105350, .F. ) ;
#25222 = EDGE_LOOP ( 'NONE', ( #19105, #47832, #81685, #34511 ) ) ;
#25223 = VERTEX_POINT ( 'NONE', #3375 ) ;
#25224 = CARTESIAN_POINT ( 'NONE',  ( 0.1317522424410015880, 1.959574484677831130, -8.000000000000001776 ) ) ;
#25225 = DIRECTION ( 'NONE',  ( 0.5735764363510470476, -0.8191520442889911324, 1.003171929053524007E-16 ) ) ;
#25226 = DIRECTION ( 'NONE',  ( -1.000000000000000000, -1.224606353822377258E-16, -0.000000000000000000 ) ) ;
#25227 = CARTESIAN_POINT ( 'NONE',  ( -40.97817787413512036, 465.3187661920380265, 16.73602713972349676 ) ) ;
#25228 = CARTESIAN_POINT ( 'NONE',  ( -29.96292276380026465, 332.4061231152326172, 16.64388083012304875 ) ) ;
#25229 = CYLINDRICAL_SURFACE ( 'NONE', #81080, 9.999999999999998224 ) ;
#25230 = ORIENTED_EDGE ( 'NONE', *, *, #85485, .T. ) ;
#25231 = PRESENTATION_STYLE_ASSIGNMENT (( #58087 ) ) ;
#25232 = ORIENTED_EDGE ( 'NONE', *, *, #48689, .F. ) ;
#25233 = DIRECTION ( 'NONE',  ( -1.000000000000000000, -1.224606353822377258E-16, -0.000000000000000000 ) ) ;
#25234 = CARTESIAN_POINT ( 'NONE',  ( 78.81833263833561887, -38.67058111308598001, 190.4994190873096898 ) ) ;
#25235 = CARTESIAN_POINT ( 'NONE',  ( 6.692588830498428898, 7.935834885954428763, 0.04058884017440098774 ) ) ;
#25236 = CARTESIAN_POINT ( 'NONE',  ( 34.53878426067466734, 302.4591013005480136, 3.675451461037441359 ) ) ;
#25237 = EDGE_CURVE ( 'NONE', #65882, #86927, #19069, .T. ) ;
#25238 = ADVANCED_FACE ( 'NONE', ( #76714 ), #80267, .T. ) ;
#25239 = AXIS2_PLACEMENT_3D ( 'NONE', #83380, #9475, #67740 ) ;
#25240 = DIRECTION ( 'NONE',  ( 0.000000000000000000, 0.000000000000000000, 1.000000000000000000 ) ) ;
#25241 = AXIS2_PLACEMENT_3D ( 'NONE', #19642, #2327, #3944 ) ;
#25242 = DIRECTION ( 'NONE',  ( -1.000000000000000000, -1.224606353822377258E-16, -0.000000000000000000 ) ) ;
#25243 = CARTESIAN_POINT ( 'NONE',  ( -5.688569873206840377, -47.04879514976369137, 103.9352763293500743 ) ) ;
#25244 = CARTESIAN_POINT ( 'NONE',  ( 0.000000000000000000, 0.000000000000000000, 0.000000000000000000 ) ) ;
#25245 = PRESENTATION_STYLE_ASSIGNMENT (( #66198 ) ) ;
#25246 = ORIENTED_EDGE ( 'NONE', *, *, #68108, .T. ) ;
#25248 = CARTESIAN_POINT ( 'NONE',  ( -24.37690711297229740, 295.5467921614321085, 10.08613426303809923 ) ) ;
#25247 = SURFACE_STYLE_USAGE ( .BOTH. , #23118 ) ;
#25249 = CARTESIAN_POINT ( 'NONE',  ( 18.13561277374696701, 6.123233995736770227E-16, -5.000000000000002665 ) ) ;
#25250 = CARTESIAN_POINT ( 'NONE',  ( 27.99999999999999645, 0.000000000000000000, 0.000000000000000000 ) ) ;
#25251 = CARTESIAN_POINT ( 'NONE',  ( 0.000000000000000000, -8.000000000000000000, 0.000000000000000000 ) ) ;
#25252 = CARTESIAN_POINT ( 'NONE',  ( -7.002990960197237769, 103.9473318161654163, 3.868040364119524011 ) ) ;
#25253 = CARTESIAN_POINT ( 'NONE',  ( 44.13343456913768392, 464.3829732007686175, 9.622105740879975500 ) ) ;
#25254 = APPLICATION_CONTEXT ( 'automotive_design' ) ;
#25255 = CARTESIAN_POINT ( 'NONE',  ( 85.41732212696841486, -42.91985075306342878, 186.8826177936102795 ) ) ;
#25256 = FILL_AREA_STYLE ('',( #90493 ) ) ;
#25257 = VECTOR ( 'NONE', #97251, 1000.000000000000000 ) ;
#25258 = ORIENTED_EDGE ( 'NONE', *, *, #39843, .T. ) ;
#25259 = CARTESIAN_POINT ( 'NONE',  ( 93.08838507352525937, -57.65565157171307931, -16.99954835227337213 ) ) ;
#25260 = CARTESIAN_POINT ( 'NONE',  ( 0.000000000000000000, 0.000000000000000000, -1.161000000000000032 ) ) ;
#25261 = FACE_OUTER_BOUND ( 'NONE', #13719, .T. ) ;
#25262 = DIRECTION ( 'NONE',  ( 0.000000000000000000, -1.000000000000000000, 0.000000000000000000 ) ) ;
#25263 = CARTESIAN_POINT ( 'NONE',  ( -80.77633485222713716, -30.00000000000000355, 10.02478776459890675 ) ) ;
#25264 = CIRCLE ( 'NONE', #21809, 9.999999999999998224 ) ;
#25265 = B_SPLINE_CURVE_WITH_KNOTS ( 'NONE', 3,
 ( #2399, #35345, #68206, #27263 ),
 .UNSPECIFIED., .F., .F.,
 ( 4, 4 ),
 ( 1.760524696717142919E-15, 0.001000218973296797091 ),
 .UNSPECIFIED. ) ;
#25266 = CIRCLE ( 'NONE', #40777, 4.000000000000007105 ) ;
#25267 = PLANE ( 'NONE',  #72618 ) ;
#25268 = CARTESIAN_POINT ( 'NONE',  ( -7.721181058141405096, -30.00000000000004263, -2.093648267354947912 ) ) ;
#25269 = CARTESIAN_POINT ( 'NONE',  ( 21.84999999999999787, 1.533819458162526451E-15, 0.000000000000000000 ) ) ;
#25270 = CARTESIAN_POINT ( 'NONE',  ( -32.92227116393205932, 439.7404285724725241, 24.14402898922834240 ) ) ;
#25271 = CARTESIAN_POINT ( 'NONE',  ( -17.49999999999997513, 49.02358271864453343, 64.04945205936840580 ) ) ;
#25272 = CARTESIAN_POINT ( 'NONE',  ( -28.79508601474831408, 15.38969543640857474, 41.74367987815701753 ) ) ;
#25273 = PRESENTATION_STYLE_ASSIGNMENT (( #391 ) ) ;
#25274 = CARTESIAN_POINT ( 'NONE',  ( -33.84761347220299399, 488.7471039746336032, 11.01988148152527103 ) ) ;
#25275 = DIRECTION ( 'NONE',  ( -1.000000000000000000, -0.000000000000000000, -0.000000000000000000 ) ) ;
#25276 = CONICAL_SURFACE ( 'NONE', #85552, 4.250000000000000000, 0.9599310885968754814 ) ;
#25277 = AXIS2_PLACEMENT_3D ( 'NONE', #102452, #71138, #54395 ) ;
#25278 = VECTOR ( 'NONE', #65921, 1000.000000000000000 ) ;
#25279 = VECTOR ( 'NONE', #55622, 1000.000000000000000 ) ;
#25280 = CARTESIAN_POINT ( 'NONE',  ( -97.35930377584806195, -38.00000000000000711, 192.7749382691207813 ) ) ;
#25281 = CIRCLE ( 'NONE', #85568, 0.9999999999999961142 ) ;
#25282 = ORIENTED_EDGE ( 'NONE', *, *, #36323, .T. ) ;
#25283 = SPHERICAL_SURFACE ( 'NONE', #94413, 1.000000000000000000 ) ;
#25284 = CARTESIAN_POINT ( 'NONE',  ( 0.000000000000000000, 0.000000000000000000, -8.000000000000000000 ) ) ;
#25285 = VECTOR ( 'NONE', #29416, 999.9999999999998863 ) ;
#25286 = CARTESIAN_POINT ( 'NONE',  ( -7.744168461338432508, 81.53745938284842509, 2.019395720771550273 ) ) ;
#25287 = EDGE_CURVE ( 'NONE', #38837, #88625, #59124, .T. ) ;
#25288 = CARTESIAN_POINT ( 'NONE',  ( -63.25291691186279763, -29.60348520313671727, -23.77066348807526452 ) ) ;
#25289 = EDGE_CURVE ( 'NONE', #100726, #86709, #29284, .T. ) ;
#25291 = LINE ( 'NONE', #83485, #884 ) ;
#25290 = CARTESIAN_POINT ( 'NONE',  ( -6.750000000000018652, 11.69134295108991317, 0.000000000000000000 ) ) ;
#25292 = ORIENTED_EDGE ( 'NONE', *, *, #14629, .T. ) ;
#25293 = ORIENTED_EDGE ( 'NONE', *, *, #48512, .T. ) ;
#25294 = CARTESIAN_POINT ( 'NONE',  ( 0.2578475836320698322, -4.367703157927332214, 5.434916218090831030 ) ) ;
#25295 = CARTESIAN_POINT ( 'NONE',  ( 10.93080612294996712, 43.17347229229180527, -15.24212494374555504 ) ) ;
#25296 = CARTESIAN_POINT ( 'NONE',  ( -3.811597179862317830, 5.304926841629206358, -0.01956314070068032943 ) ) ;
#25297 = CARTESIAN_POINT ( 'NONE',  ( -33.39843217748020265, -60.00000000000000711, -40.50829833586755768 ) ) ;
#25298 = ORIENTED_EDGE ( 'NONE', *, *, #9311, .F. ) ;
#25299 = CARTESIAN_POINT ( 'NONE',  ( 69.78853948234211657, -37.99999999999999289, -22.51057024784411098 ) ) ;
#25300 = DIRECTION ( 'NONE',  ( 0.2276885448027893277, 0.1882482561681191047, 0.9553640775197957957 ) ) ;
#25301 = CARTESIAN_POINT ( 'NONE',  ( 100.0744711941220828, -45.27419155593420896, 192.5344585825728245 ) ) ;
#25303 = CARTESIAN_POINT ( 'NONE',  ( -46.77673112620464480, 13.57592939483832062, 15.58267473267816960 ) ) ;
#25302 = CARTESIAN_POINT ( 'NONE',  ( 28.67833651802481754, -29.89477528201764400, 30.92734934190152885 ) ) ;
#25304 = VECTOR ( 'NONE', #56845, 1000.000000000000000 ) ;
#25305 = ORIENTED_EDGE ( 'NONE', *, *, #93760, .T. ) ;
#25306 = ORIENTED_EDGE ( 'NONE', *, *, #75200, .T. ) ;
#25307 = ORIENTED_EDGE ( 'NONE', *, *, #45660, .F. ) ;
#25308 = CARTESIAN_POINT ( 'NONE',  ( 30.95257640470975602, 348.4999900758657532, 18.99904917110374214 ) ) ;
#25309 = CARTESIAN_POINT ( 'NONE',  ( 0.7777777777777741264, -54.00000000000000711, 40.97837836547555668 ) ) ;
#25310 = CARTESIAN_POINT ( 'NONE',  ( 9.636006000319470743, 53.53718130950936427, 2.125009785464772705 ) ) ;
#25311 = ORIENTED_EDGE ( 'NONE', *, *, #89578, .F. ) ;
#25312 = CARTESIAN_POINT ( 'NONE',  ( -3.857142857142847880, -48.79941684889506348, 103.1763305333244318 ) ) ;
#25313 = DIRECTION ( 'NONE',  ( -0.000000000000000000, -0.000000000000000000, -1.000000000000000000 ) ) ;
#25314 = DIRECTION ( 'NONE',  ( 0.000000000000000000, 0.000000000000000000, -1.000000000000000000 ) ) ;
#25315 = CARTESIAN_POINT ( 'NONE',  ( -53.52971897118871425, -57.67555505732850207, 87.03092276603273092 ) ) ;
#25316 = CARTESIAN_POINT ( 'NONE',  ( 5.082755093536324154, -28.34375000204838813, 5.082755093536326818 ) ) ;
#25317 = CARTESIAN_POINT ( 'NONE',  ( -30.22873954704404298, 12.95661247755296941, 41.98212759391198290 ) ) ;
#25318 = CARTESIAN_POINT ( 'NONE',  ( -20.52350613252515643, 304.8999024697870937, 9.947223320822450532 ) ) ;
#25319 = LINE ( 'NONE', #33946, #46778 ) ;
#25320 = CARTESIAN_POINT ( 'NONE',  ( -56.79577812574758156, -14.21045842199439591, -31.02744264688941556 ) ) ;
#25321 = CARTESIAN_POINT ( 'NONE',  ( -24.48725402052853184, -14.21045842199434084, 35.52122251240935924 ) ) ;
#25322 = EDGE_CURVE ( 'NONE', #20242, #50908, #12872, .T. ) ;
#25323 = CARTESIAN_POINT ( 'NONE',  ( -50.87568867342284307, -36.04944650272992845, 51.03950296323957048 ) ) ;
#25324 = CARTESIAN_POINT ( 'NONE',  ( 43.17545047952468451, 487.6211760455611284, 8.487215481668586747 ) ) ;
#25325 = VERTEX_POINT ( 'NONE', #12506 ) ;
#25326 = CARTESIAN_POINT ( 'NONE',  ( -101.3987088893176889, -60.24204779500730922, 194.8051035594306484 ) ) ;
#25327 = CARTESIAN_POINT ( 'NONE',  ( 1.255263095696489281E-15, 51.26930509877138320, 10.24999999999999822 ) ) ;
#25328 = CARTESIAN_POINT ( 'NONE',  ( 12.82656847843611203, 1.661299769047218655, 14.90831243661676631 ) ) ;
#25329 = VERTEX_POINT ( 'NONE', #19605 ) ;
#25330 = CARTESIAN_POINT ( 'NONE',  ( -17.16215690045858722, 34.18974779370575590, -24.24070848783700427 ) ) ;
#25331 = AXIS2_PLACEMENT_3D ( 'NONE', #94620, #20765, #70326 ) ;
#25332 = CARTESIAN_POINT ( 'NONE',  ( 84.96569581588377673, -38.70379807337806710, 198.4584125899654339 ) ) ;
#25333 = DIRECTION ( 'NONE',  ( 0.000000000000000000, 0.000000000000000000, 1.000000000000000000 ) ) ;
#25334 = DIRECTION ( 'NONE',  ( -1.000000000000000000, -1.224606353822377258E-16, -0.000000000000000000 ) ) ;
#25335 = DIRECTION ( 'NONE',  ( 0.9788760387920804051, 0.000000000000000000, 0.2044546421060805530 ) ) ;
#25336 = CARTESIAN_POINT ( 'NONE',  ( -2.912673042965788187E-14, 42.00000000000000000, -90.56128410203886858 ) ) ;
#25337 = CARTESIAN_POINT ( 'NONE',  ( 84.01303099038503319, -29.99999999999999645, 161.1241072836490957 ) ) ;
#25338 =( BOUNDED_SURFACE ( )  B_SPLINE_SURFACE ( 3, 2, ( 
 ( #82613, #48630, #97191 ),
 ( #64837, #38980, #57 ),
 ( #56176, #90172, #15747 ),
 ( #65893, #40556, #73439 ),
 ( #7115, #89116, #41093 ),
 ( #15213, #106333, #22814 ),
 ( #16275, #40031, #55648 ),
 ( #24413, #14665, #47575 ),
 ( #57252, #39515, #105294 ),
 ( #31440, #9239, #58885 ),
 ( #83655, #43221, #67502 ),
 ( #76104, #92279, #50750 ),
 ( #2744, #9769, #2205 ),
 ( #19523, #35153, #26546 ),
 ( #83142, #10825, #58334 ),
 ( #59959, #27077, #51290 ),
 ( #84210, #10305, #68022 ),
 ( #74507, #91776, #27612 ),
 ( #66972, #100909, #42682 ),
 ( #100384, #42144, #91257 ) ),
 .UNSPECIFIED., .F., .F., .F. ) 
 B_SPLINE_SURFACE_WITH_KNOTS ( ( 4, 2, 2, 2, 2, 2, 2, 2, 2, 4 ),
 ( 3, 3 ),
 ( 0.06021901822288649314, 0.06247022664829056382, 0.06472143507369462756, 0.06697264349909869130, 0.06922385192450275504, 0.07147506034990681878, 0.07260066456260885759, 0.07372626877531088252, 0.07597747720071496014, 0.07822868562611902388 ),
 ( 0.000000000000000000, 1.000000000000000000 ),
 .UNSPECIFIED. ) 
 GEOMETRIC_REPRESENTATION_ITEM ( )  RATIONAL_B_SPLINE_SURFACE ( (
 ( 1.000000000000000000, 0.5207636911093219689, 1.000000000000000000),
 ( 1.000000000000000000, 0.5185382483914372509, 1.000000000000000000),
 ( 1.000000000000000000, 0.5157170609726789978, 1.000000000000000000),
 ( 1.000000000000000000, 0.5095464177491236812, 1.000000000000000000),
 ( 1.000000000000000000, 0.5062011784965128047, 1.000000000000000000),
 ( 1.000000000000000000, 0.4995824849051648808, 1.000000000000000000),
 ( 1.000000000000000000, 0.4963024291608688077, 1.000000000000000000),
 ( 1.000000000000000000, 0.4905153737246681911, 1.000000000000000000),
 ( 1.000000000000000000, 0.4880809317982532369, 1.000000000000000000),
 ( 1.000000000000000000, 0.4846011406799364818, 1.000000000000000000),
 ( 1.000000000000000000, 0.4835584709197799369, 1.000000000000000000),
 ( 1.000000000000000000, 0.4832073097951730123, 1.000000000000000000),
 ( 1.000000000000000000, 0.4832927473445461919, 1.000000000000000000),
 ( 1.000000000000000000, 0.4838416877134147365, 1.000000000000000000),
 ( 1.000000000000000000, 0.4843037014696224829, 1.000000000000000000),
 ( 1.000000000000000000, 0.4861738658104473587, 1.000000000000000000),
 ( 1.000000000000000000, 0.4880704143552366814, 1.000000000000000000),
 ( 1.000000000000000000, 0.4926074442002630338, 1.000000000000000000),
 ( 1.000000000000000000, 0.4952473214787204703, 1.000000000000000000),
 ( 1.000000000000000000, 0.4978121763378770548, 1.000000000000000000) ) ) 
 REPRESENTATION_ITEM ( '' )  SURFACE ( )  );
#25339 = CARTESIAN_POINT ( 'NONE',  ( 36.50840931121960153, 491.4427145161587873, 12.32866606331501202 ) ) ;
#25340 = EDGE_CURVE ( 'NONE', #73687, #80282, #33811, .T. ) ;
#25341 = SURFACE_SIDE_STYLE ('',( #99179 ) ) ;
#25342 = FACE_BOUND ( 'NONE', #40410, .T. ) ;
#25343 = EDGE_LOOP ( 'NONE', ( #13007, #43080, #87794, #2256, #3148 ) ) ;
#25344 = ORIENTED_EDGE ( 'NONE', *, *, #2696, .T. ) ;
#25345 = CARTESIAN_POINT ( 'NONE',  ( 53.50953716884873756, -22.16763606720927626, 50.70318854014821142 ) ) ;
#25346 = CIRCLE ( 'NONE', #75263, 0.9999999999999985567 ) ;
#25347 = CARTESIAN_POINT ( 'NONE',  ( -33.00000000000000000, 464.3970849722209664, 17.41240408234212111 ) ) ;
#25348 = CARTESIAN_POINT ( 'NONE',  ( 8.717882134064298683, 51.77839830771046081, 1.531152949373697281 ) ) ;
#25349 = ORIENTED_EDGE ( 'NONE', *, *, #60644, .T. ) ;
#25350 = CARTESIAN_POINT ( 'NONE',  ( -90.64414275519084185, -38.34462549197198200, 9.748502710164705931 ) ) ;
#25351 = ORIENTED_EDGE ( 'NONE', *, *, #106243, .F. ) ;
#25352 = CARTESIAN_POINT ( 'NONE',  ( 3.313708498984761608, -28.90625000409677270, -8.000000000000000000 ) ) ;
#25353 = CARTESIAN_POINT ( 'NONE',  ( 94.42873002227078416, -38.35542734117505859, 53.97500541993706946 ) ) ;
#25354 = CARTESIAN_POINT ( 'NONE',  ( 13.79682684651001878, 23.00040460847749202, 0.2373010561590335743 ) ) ;
#25355 = CARTESIAN_POINT ( 'NONE',  ( 86.28022341275342910, -60.14323854837493855, 19.05399894497716318 ) ) ;
#25356 = B_SPLINE_CURVE_WITH_KNOTS ( 'NONE', 3,
 ( #68924, #35510, #60310, #78578, #76996, #69970, #68389, #102872, #86179, #61363, #94256, #29037, #52179, #93185, #53777, #19876, #12252, #101282, #77533, #3651, #27432, #11177 ),
 .UNSPECIFIED., .F., .F.,
 ( 4, 2, 2, 2, 2, 2, 2, 2, 2, 2, 4 ),
 ( 0.003244682626514291002, 0.003748712926862984764, 0.004252743227211678960, 0.004756773527560372722, 0.005260803827909066484, 0.005764834128257760246, 0.006016849278432111030, 0.006268864428606461814, 0.006520879578780811731, 0.006772894728955162515, 0.007276925029303863215 ),
 .UNSPECIFIED. ) ;
#25357 = CONICAL_SURFACE ( 'NONE', #85628, 5.000000000000001776, 0.9599310885968803664 ) ;
#25358 = CARTESIAN_POINT ( 'NONE',  ( -31.30848237729719230, 439.0139854832817150, 22.67909095395106789 ) ) ;
#25359 = CARTESIAN_POINT ( 'NONE',  ( -1.250612401299674659, 45.68690097979559539, -17.65351159749431531 ) ) ;
#25361 = PRESENTATION_LAYER_ASSIGNMENT (  '', '', ( #33987 ) ) ;
#25360 = CARTESIAN_POINT ( 'NONE',  ( -27.48025251572867234, 308.0883985054451841, -8.272527303563915524 ) ) ;
#25362 = CARTESIAN_POINT ( 'NONE',  ( 5.299999999999999822, 0.000000000000000000, 0.000000000000000000 ) ) ;
#25363 = CARTESIAN_POINT ( 'NONE',  ( 74.88199338232608682, -60.00000000000000000, 180.3605328980037257 ) ) ;
#25364 = EDGE_CURVE ( 'NONE', #55179, #15045, #52436, .T. ) ;
#25365 = CIRCLE ( 'NONE', #39138, 4.000000000000007105 ) ;
#25366 = AXIS2_PLACEMENT_3D ( 'NONE', #83224, #68664, #43305 ) ;
#25367 = CARTESIAN_POINT ( 'NONE',  ( 18.28855716066948389, 45.00000000000001421, 62.41177028466893972 ) ) ;
#25368 = ORIENTED_EDGE ( 'NONE', *, *, #30661, .F. ) ;
#25369 = CARTESIAN_POINT ( 'NONE',  ( 59.49458740857772909, -56.85954389590153824, 79.18117010720280291 ) ) ;
#25370 = EDGE_CURVE ( 'NONE', #45699, #73133, #91425, .T. ) ;
#25371 = CARTESIAN_POINT ( 'NONE',  ( -23.56457664856237599, 303.4636367812840376, -9.868556678049921871 ) ) ;
#25372 = CARTESIAN_POINT ( 'NONE',  ( 5.799999999999999822, -9.237604307034013473, 1.734723475976807094E-15 ) ) ;
#25373 = CARTESIAN_POINT ( 'NONE',  ( -6.515460109692552848, -4.999999999999999112, -15.35047127641723996 ) ) ;
#25375 = CARTESIAN_POINT ( 'NONE',  ( -4.523211276071191556, 53.69404211156058437, 8.281008664756861037 ) ) ;
#25374 = CARTESIAN_POINT ( 'NONE',  ( -76.12537862032631608, -38.35598417008159799, -28.58435412235101225 ) ) ;
#25376 = CARTESIAN_POINT ( 'NONE',  ( -42.70159805713172574, 373.1387034520102475, 18.11088861087180391 ) ) ;
#25377 = CARTESIAN_POINT ( 'NONE',  ( -37.88570315047687131, 25.64574018102357655, -10.95617127781024003 ) ) ;
#25378 = CARTESIAN_POINT ( 'NONE',  ( 7.000000000000000000, -14.21727251090713828, 9.320362779989000757 ) ) ;
#25379 = CARTESIAN_POINT ( 'NONE',  ( 8.000000000000000000, -27.49999999999999645, 0.000000000000000000 ) ) ;
#25380 = CARTESIAN_POINT ( 'NONE',  ( -1.308996937483428269, -3.000000000000002665, -75.00000000000001421 ) ) ;
#25381 = EDGE_CURVE ( 'NONE', #39874, #25504, #46323, .T. ) ;
#25382 = CARTESIAN_POINT ( 'NONE',  ( 34.42407431220851066, 1.340359594676612611E-15, 0.000000000000000000 ) ) ;
#25383 = ORIENTED_EDGE ( 'NONE', *, *, #94369, .T. ) ;
#25384 = CARTESIAN_POINT ( 'NONE',  ( 83.83469278148253068, -39.45372097025308022, 177.1342842458970495 ) ) ;
#25386 = CIRCLE ( 'NONE', #101198, 3.000000000000013323 ) ;
#25385 = CARTESIAN_POINT ( 'NONE',  ( 30.00000000000000355, 489.0498425200157158, 4.975187970393438519 ) ) ;
#25387 = B_SPLINE_CURVE_WITH_KNOTS ( 'NONE', 3,
 ( #25811, #75354, #58665, #82392, #99090, #91567, #74294, #8498, #9023, #57040, #81312, #90489, #73219, #74815, #33874, #89955, #41401, #66205, #98568, #50538, #1455, #17147, #63168, #48942, #9554, #7424 ),
 .UNSPECIFIED., .F., .F.,
 ( 4, 2, 2, 2, 2, 2, 2, 2, 2, 2, 2, 2, 4 ),
 ( 6.942281208919283290E-18, 0.001948376510295373376, 0.002922564765443056919, 0.003896753020590740680, 0.005845129530886042715, 0.007793506041181345184, 0.009741882551476647653, 0.01169025906177195012, 0.01266444731691965947, 0.01363863557206736535, 0.01461282382721507296, 0.01509991795478892590, 0.01558701208236277884 ),
 .UNSPECIFIED. ) ;
#25388 = CARTESIAN_POINT ( 'NONE',  ( 0.000000000000000000, 0.000000000000000000, 63.00000000000000000 ) ) ;
#25389 = VERTEX_POINT ( 'NONE', #104711 ) ;
#25390 = FACE_OUTER_BOUND ( 'NONE', #105657, .T. ) ;
#25391 = CARTESIAN_POINT ( 'NONE',  ( 43.11534632275463963, 435.4435433140298528, 9.329549855361591426 ) ) ;
#25392 = DIRECTION ( 'NONE',  ( 0.000000000000000000, -1.000000000000000000, 0.000000000000000000 ) ) ;
#25393 = FACE_OUTER_BOUND ( 'NONE', #44709, .T. ) ;
#25394 = CARTESIAN_POINT ( 'NONE',  ( -43.42270916030687289, 41.45355254419347801, -50.80364451785244739 ) ) ;
#25395 = CONICAL_SURFACE ( 'NONE', #97637, 5.000000000000010658, 0.9599310885968697082 ) ;
#25396 = CARTESIAN_POINT ( 'NONE',  ( -27.77263666253245589, -28.74976145023062557, -38.27455432825868087 ) ) ;
#25397 = CARTESIAN_POINT ( 'NONE',  ( -9.118966701651679330, -0.3497226616077714345, 19.74305553042258055 ) ) ;
#25398 = B_SPLINE_CURVE_WITH_KNOTS ( 'NONE', 3,
 ( #83905, #19237, #34866, #11064 ),
 .UNSPECIFIED., .F., .F.,
 ( 4, 4 ),
 ( 0.000000000000000000, 0.4999999999999988898 ),
 .UNSPECIFIED. ) ;
#25399 = CARTESIAN_POINT ( 'NONE',  ( 43.69737412773557850, -60.00000000000000000, 58.12383163124780339 ) ) ;
#25400 = CARTESIAN_POINT ( 'NONE',  ( 26.69900261086841198, 1.482358050883964840E-15, 0.000000000000000000 ) ) ;
#25401 = CARTESIAN_POINT ( 'NONE',  ( 26.89082867329939575, -20.19349464338415601, 31.72560904215549726 ) ) ;
#25402 = AXIS2_PLACEMENT_3D ( 'NONE', #103053, #94439, #52355 ) ;
#25404 = CARTESIAN_POINT ( 'NONE',  ( -14.20583055102296477, 21.14383427519521419, -5.809807938884436140 ) ) ;
#25403 = CARTESIAN_POINT ( 'NONE',  ( -14.80423426860585678, -22.57669348423709721, 35.90345806391073324 ) ) ;
#25405 = CARTESIAN_POINT ( 'NONE',  ( 5.082755093536325930, -11.46875000204838635, -5.082755093536325042 ) ) ;
#25406 = SURFACE_STYLE_FILL_AREA ( #74963 ) ;
#25407 = FILL_AREA_STYLE ('',( #65828 ) ) ;
#25408 = CIRCLE ( 'NONE', #52940, 7.000000000000000000 ) ;
#25409 = ORIENTED_EDGE ( 'NONE', *, *, #32973, .T. ) ;
#25410 = CARTESIAN_POINT ( 'NONE',  ( -17.49999999999995737, 47.99999999999996447, 64.09945636502659738 ) ) ;
#25411 = DIRECTION ( 'NONE',  ( 1.000000000000000000, 1.224606353822377258E-16, 0.000000000000000000 ) ) ;
#25412 = DIRECTION ( 'NONE',  ( -1.000000000000000000, -1.224606353822377258E-16, -0.000000000000000000 ) ) ;
#25413 = ADVANCED_FACE ( 'NONE', ( #30864 ), #59745, .F. ) ;
#25415 = CARTESIAN_POINT ( 'NONE',  ( 22.10411833928789349, -34.58974732179735412, -31.65657241835295110 ) ) ;
#25414 = LINE ( 'NONE', #91199, #7021 ) ;
#25416 = VERTEX_POINT ( 'NONE', #7070 ) ;
#25417 = CARTESIAN_POINT ( 'NONE',  ( 11.76826524265346841, 16.33356993944290991, -9.436846598424574850 ) ) ;
#25418 = CARTESIAN_POINT ( 'NONE',  ( -4.044492309121838325, 51.90729595881780511, 7.473210932956116714 ) ) ;
#25419 = STYLED_ITEM ( 'NONE', ( #27316 ), #26428 ) ;
#25420 = AXIS2_PLACEMENT_3D ( 'NONE', #24514, #6154, #8280 ) ;
#25421 = ORIENTED_EDGE ( 'NONE', *, *, #92257, .T. ) ;
#25422 = EDGE_CURVE ( 'NONE', #57770, #82322, #14902, .T. ) ;
#25423 = DIRECTION ( 'NONE',  ( 0.000000000000000000, -1.000000000000000000, 0.000000000000000000 ) ) ;
#25424 = DIRECTION ( 'NONE',  ( -1.000000000000000000, -0.000000000000000000, -0.000000000000000000 ) ) ;
#25425 = CARTESIAN_POINT ( 'NONE',  ( -26.32519096281068727, 41.43537210829613571, -71.18657295512365124 ) ) ;
#25426 = CARTESIAN_POINT ( 'NONE',  ( -101.0097921112870836, -59.99999999999998579, 86.95724220043298658 ) ) ;
#25427 = VECTOR ( 'NONE', #79852, 1000.000000000000000 ) ;
#25428 = PRESENTATION_LAYER_ASSIGNMENT (  '', '', ( #9914 ) ) ;
#25429 = CARTESIAN_POINT ( 'NONE',  ( 4.898587196589412829E-16, -21.31250000409676915, -8.000000000000000000 ) ) ;
#25430 = VECTOR ( 'NONE', #86720, 1000.000000000000341 ) ;
#25431 = CARTESIAN_POINT ( 'NONE',  ( -89.99999999999997158, -38.00000000001091394, 188.5238439516623146 ) ) ;
#25432 = STYLED_ITEM ( 'NONE', ( #19113 ), #37977 ) ;
#25433 = CARTESIAN_POINT ( 'NONE',  ( 34.94338628507543376, 342.5355909536760350, -0.9693026116843473927 ) ) ;
#25434 = CARTESIAN_POINT ( 'NONE',  ( 40.90837589346737957, 460.4813280201769885, 2.460853848284856760 ) ) ;
#25435 = EDGE_CURVE ( 'NONE', #56430, #77058, #6007, .T. ) ;
#25437 = DIRECTION ( 'NONE',  ( -0.000000000000000000, -0.000000000000000000, -1.000000000000000000 ) ) ;
#25436 = CARTESIAN_POINT ( 'NONE',  ( -8.737863884125482983, -4.999999999994546585, -90.03618980230058355 ) ) ;
#25438 = CARTESIAN_POINT ( 'NONE',  ( -85.53824590343933210, -21.95572400392595469, 166.5517161537221682 ) ) ;
#25439 = VERTEX_POINT ( 'NONE', #79898 ) ;
#25440 = CARTESIAN_POINT ( 'NONE',  ( 23.58349330513380337, 4.000000000000002665, 0.000000000000000000 ) ) ;
#25441 = B_SPLINE_CURVE_WITH_KNOTS ( 'NONE', 3,
 ( #16273, #30906, #63787, #72386 ),
 .UNSPECIFIED., .F., .F.,
 ( 4, 4 ),
 ( 1.600194022572398637E-15, 0.0002604505668095903267 ),
 .UNSPECIFIED. ) ;
#25442 = ORIENTED_EDGE ( 'NONE', *, *, #6526, .F. ) ;
#25443 = VERTEX_POINT ( 'NONE', #71802 ) ;
#25444 = CIRCLE ( 'NONE', #21972, 8.000000000000000000 ) ;
#25445 = CARTESIAN_POINT ( 'NONE',  ( 27.10511071441197117, 34.47735702144345282, 10.05698433968570704 ) ) ;
#25446 = EDGE_CURVE ( 'NONE', #71944, #52979, #3915, .T. ) ;
#25447 = DIRECTION ( 'NONE',  ( 0.8191520442889884679, 0.000000000000000000, 0.5735764363510508224 ) ) ;
#25448 = ORIENTED_EDGE ( 'NONE', *, *, #47726, .F. ) ;
#25449 = CARTESIAN_POINT ( 'NONE',  ( -18.20176702087010057, 303.6397689725556575, 9.891910795295462577 ) ) ;
#25450 = CARTESIAN_POINT ( 'NONE',  ( -36.37294538904226471, -57.67119865010090507, -42.13310955380372747 ) ) ;
#25451 = CARTESIAN_POINT ( 'NONE',  ( 2.499999999999997780, -18.83380486180452706, 27.02532357426314036 ) ) ;
#25452 = CARTESIAN_POINT ( 'NONE',  ( -7.150931910075641440, -63.21374201477737387, -3.588457848165359731 ) ) ;
#25453 = DIRECTION ( 'NONE',  ( -0.5735764363510461594, 0.8191520442889916875, 1.003171929053524870E-16 ) ) ;
#25454 = CARTESIAN_POINT ( 'NONE',  ( -32.15310320217076878, 439.7024266304582625, 23.94087012106557211 ) ) ;
#25455 = CARTESIAN_POINT ( 'NONE',  ( 74.56127108291157413, 4.898587196589294500E-16, -4.000000000000007105 ) ) ;
#25456 = CARTESIAN_POINT ( 'NONE',  ( 106.4854190881680154, -14.21045842199434439, 182.1792229330528983 ) ) ;
#25457 = CARTESIAN_POINT ( 'NONE',  ( -107.9655701563618067, -29.99999999999997158, 188.7577781645654795 ) ) ;
#25458 = EDGE_CURVE ( 'NONE', #67117, #36789, #66964, .T. ) ;
#25459 = CARTESIAN_POINT ( 'NONE',  ( -58.04404759258189728, -56.86246254669144662, 75.20273737405429415 ) ) ;
#25460 = CIRCLE ( 'NONE', #16797, 3.400000000000000355 ) ;
#25461 = ORIENTED_EDGE ( 'NONE', *, *, #32033, .F. ) ;
#25462 = CARTESIAN_POINT ( 'NONE',  ( 61.88407606007120165, 38.95394859066640691, 15.24418052639449073 ) ) ;
#25463 = CARTESIAN_POINT ( 'NONE',  ( 114.2077509676909557, -59.99999999999023004, 161.8867648380875153 ) ) ;
#25464 = VERTEX_POINT ( 'NONE', #75529 ) ;
#25465 = CARTESIAN_POINT ( 'NONE',  ( 4.074124056600999744, -46.43456338532926964, 31.62120482653921982 ) ) ;
#25466 = CARTESIAN_POINT ( 'NONE',  ( -98.65422846995242878, -37.82071831846016607, 130.4055507037949155 ) ) ;
#25467 = CARTESIAN_POINT ( 'NONE',  ( -2.977408999572654480, -15.50000000204838635, 7.188101187499999156 ) ) ;
#25468 = DIRECTION ( 'NONE',  ( 0.000000000000000000, -0.3420201433256727652, -0.9396926207859068736 ) ) ;
#25469 = VERTEX_POINT ( 'NONE', #64787 ) ;
#25470 = CARTESIAN_POINT ( 'NONE',  ( -64.44341639718678039, -59.99999999999998579, 116.0066787658274308 ) ) ;
#25471 = CARTESIAN_POINT ( 'NONE',  ( -5.082755093536325042, -23.46875000204838457, -5.082755093536325930 ) ) ;
#25472 = CARTESIAN_POINT ( 'NONE',  ( 46.00000000000000000, 461.1597079622285946, 8.544206286667911598 ) ) ;
#25473 = AXIS2_PLACEMENT_3D ( 'NONE', #4256, #85722, #84643 ) ;
#25474 = CARTESIAN_POINT ( 'NONE',  ( 17.01594651245413203, -0.000000000000000000, -1.113195845613775381 ) ) ;
#25475 = CARTESIAN_POINT ( 'NONE',  ( 13.50000000000000178, 0.000000000000000000, -13.00000000000000000 ) ) ;
#25476 = FACE_OUTER_BOUND ( 'NONE', #12074, .T. ) ;
#25477 = CARTESIAN_POINT ( 'NONE',  ( -10.28624191511830155, 43.99263840937192782, -12.90779740156156841 ) ) ;
#25478 = EDGE_CURVE ( 'NONE', #65653, #68930, #16223, .T. ) ;
#25479 = CARTESIAN_POINT ( 'NONE',  ( -34.71762651478146466, 302.0735516083713037, -0.3584149496404396840 ) ) ;
#25480 = CARTESIAN_POINT ( 'NONE',  ( 12.79230769230769305, 4.172000000000003261, 5.109226446042759579E-16 ) ) ;
#25481 = CARTESIAN_POINT ( 'NONE',  ( -31.71388525929565816, -18.67330243560268954, 29.92571452508646601 ) ) ;
#25482 =( NAMED_UNIT ( * ) PLANE_ANGLE_UNIT ( ) SI_UNIT ( $, .RADIAN. ) );
#25483 = CARTESIAN_POINT ( 'NONE',  ( 46.35797818206071241, -56.80661940937356746, 50.30410939637813073 ) ) ;
#25484 = DIRECTION ( 'NONE',  ( -1.000000000000000000, -0.000000000000000000, -0.000000000000000000 ) ) ;
#25485 = VERTEX_POINT ( 'NONE', #89601 ) ;
#25487 = CIRCLE ( 'NONE', #37588, 0.9999999999999966693 ) ;
#25486 = CARTESIAN_POINT ( 'NONE',  ( 44.34415387544843412, 435.2422591719042657, 12.20585227837244702 ) ) ;
#25488 = CARTESIAN_POINT ( 'NONE',  ( -78.45413196039172021, -38.62859691719035027, 189.5535229323872386 ) ) ;
#25489 = B_SPLINE_CURVE_WITH_KNOTS ( 'NONE', 3,
 ( #106746, #17764, #57655, #58203, #65238, #32365, #106202, #57130, #42546, #65771, #56598, #7509, #40428, #89520, #31826, #83017, #40964, #74902, #25897, #98129, #41486, #82486, #73852, #50619, #33424, #17239, #15614, #24277, #90039, #24801 ),
 .UNSPECIFIED., .F., .F.,
 ( 4, 2, 2, 2, 2, 2, 2, 2, 2, 2, 2, 2, 2, 2, 4 ),
 ( 0.0004001071830457966967, 0.0008634720163662918963, 0.001326836849686787150, 0.002253566516327772454, 0.003180296182968758191, 0.004107025849609744796, 0.005033755516250729665, 0.005497120349571219498, 0.005960485182891710199, 0.006423850016212200031, 0.006655532432872437142, 0.006887214849532674252, 0.007118897266192911362, 0.007350579682853147605, 0.007813944516173620958 ),
 .UNSPECIFIED. ) ;
#25490 = ORIENTED_EDGE ( 'NONE', *, *, #56013, .F. ) ;
#25492 = CARTESIAN_POINT ( 'NONE',  ( 99.75754961941544252, 5.000000000000021316, 0.000000000000000000 ) ) ;
#25491 = DIRECTION ( 'NONE',  ( -1.000000000000000000, -0.000000000000000000, -0.000000000000000000 ) ) ;
#25493 = CARTESIAN_POINT ( 'NONE',  ( 8.351634798667673110, -59.99999999999998579, 33.88072871824981291 ) ) ;
#25494 = DIRECTION ( 'NONE',  ( 1.000000000000000000, -0.000000000000000000, -0.000000000000000000 ) ) ;
#25495 = CARTESIAN_POINT ( 'NONE',  ( 6.568242156162281908, 3.336471507263022218, 6.846117829660598453 ) ) ;
#25496 = CARTESIAN_POINT ( 'NONE',  ( 33.51920064736375338, 462.9438705373632388, 5.599630057702720265 ) ) ;
#25497 = DIRECTION ( 'NONE',  ( -0.000000000000000000, 1.000000000000000000, -0.000000000000000000 ) ) ;
#25498 = CARTESIAN_POINT ( 'NONE',  ( -29.90889627134798090, 328.9483774411300487, 14.84562707069868637 ) ) ;
#25499 = CARTESIAN_POINT ( 'NONE',  ( 17.25516560787562881, 45.65538004793684479, 4.306155947793937955 ) ) ;
#25500 = CARTESIAN_POINT ( 'NONE',  ( 108.9153292171738059, -59.99999999999999289, 135.3754215099987732 ) ) ;
#25501 = CIRCLE ( 'NONE', #78801, 2.000000000000000000 ) ;
#25502 = DIRECTION ( 'NONE',  ( 0.000000000000000000, -1.000000000000000000, 0.000000000000000000 ) ) ;
#25503 = CARTESIAN_POINT ( 'NONE',  ( -33.78214696080224400, 461.9283447517260015, 7.821959111644967599 ) ) ;
#25504 = VERTEX_POINT ( 'NONE', #15694 ) ;
#25505 = EDGE_CURVE ( 'NONE', #15460, #52539, #70055, .T. ) ;
#25506 = CARTESIAN_POINT ( 'NONE',  ( -94.47165723176175334, -29.99999999999987210, 191.3277322571271100 ) ) ;
#25507 = VERTEX_POINT ( 'NONE', #49111 ) ;
#25508 = DIRECTION ( 'NONE',  ( 1.000000000000000000, 1.224606353822377258E-16, 0.000000000000000000 ) ) ;
#25509 = CARTESIAN_POINT ( 'NONE',  ( 42.63927665717513804, 462.0185602173703501, 4.112661701976962902 ) ) ;
#25510 = CARTESIAN_POINT ( 'NONE',  ( 30.93990408052894381, 332.3813973617133684, 16.87533365184100376 ) ) ;
#25512 = CARTESIAN_POINT ( 'NONE',  ( 9.176855344542989457, 29.47039573022589565, -3.973472207155926750 ) ) ;
#25511 = CIRCLE ( 'NONE', #15142, 4.000000000000000888 ) ;
#25513 = AXIS2_PLACEMENT_3D ( 'NONE', #103549, #21602, #10797 ) ;
#25514 = CARTESIAN_POINT ( 'NONE',  ( -5.082755093536326818, -18.59375000204838457, 5.082755093536325042 ) ) ;
#25515 = CARTESIAN_POINT ( 'NONE',  ( 10.41054107240687188, 1.482358050883964840E-15, 0.000000000000000000 ) ) ;
#25516 = SHAPE_REPRESENTATION ( 'hex flange nut_din_Hexagon Flange Nut DIN 6923 - M8 - S', ( #10728 ), #3983 ) ;
#25518 = EDGE_CURVE ( 'NONE', #87879, #34686, #78657, .T. ) ;
#25517 = CARTESIAN_POINT ( 'NONE',  ( 16.11174065067145733, 37.20923313995305648, -21.98001889856152147 ) ) ;
#25519 = AXIS2_PLACEMENT_3D ( 'NONE', #16911, #82694, #41707 ) ;
#25520 = CIRCLE ( 'NONE', #97841, 4.000000000000000888 ) ;
#25522 = ORIENTED_EDGE ( 'NONE', *, *, #87679, .T. ) ;
#25521 =( LENGTH_UNIT ( ) NAMED_UNIT ( * ) SI_UNIT ( .MILLI., .METRE. ) );
#25523 = CARTESIAN_POINT ( 'NONE',  ( 82.82954590797592687, -39.48843416255702010, 168.2668317262558446 ) ) ;
#25524 = CARTESIAN_POINT ( 'NONE',  ( -6.645513941704877858, 41.91298746401114528, -59.84148600730080858 ) ) ;
#25525 = CARTESIAN_POINT ( 'NONE',  ( -5.290067270632216712, -1.200000000000000030E-05, 7.281152949374556371 ) ) ;
#25526 = ORIENTED_EDGE ( 'NONE', *, *, #31589, .F. ) ;
#25527 = ADVANCED_FACE ( 'NONE', ( #3782 ), #20009, .F. ) ;
#25528 = CARTESIAN_POINT ( 'NONE',  ( -62.57092854446853636, 49.99999999999999289, -7.449143581871620512 ) ) ;
#25529 = CARTESIAN_POINT ( 'NONE',  ( -46.79169002450407788, 18.53182619689688693, 15.81978731893011947 ) ) ;
#25530 = CARTESIAN_POINT ( 'NONE',  ( 4.852941176470592310, -3.000000000000002665, -70.80672828634229177 ) ) ;
#25531 = DIRECTION ( 'NONE',  ( 0.000000000000000000, 0.000000000000000000, 1.000000000000000000 ) ) ;
#25532 = CARTESIAN_POINT ( 'NONE',  ( -5.191472769733070258, 252.6409157671893979, -3.014900733016763645 ) ) ;
#25533 = CARTESIAN_POINT ( 'NONE',  ( -33.15394466697068054, 409.2619214805569641, 25.87672194516226654 ) ) ;
#25534 = CYLINDRICAL_SURFACE ( 'NONE', #69325, 1.250000000000001110 ) ;
#25535 = ORIENTED_EDGE ( 'NONE', *, *, #74814, .F. ) ;
#25536 = SHAPE_REPRESENTATION_RELATIONSHIP ( 'NONE' , 'NONE' ,  #70207, #51084 ) ;
#25537 = AXIS2_PLACEMENT_3D ( 'NONE', #40904, #16092, #73789 ) ;
#25538 = CARTESIAN_POINT ( 'NONE',  ( -1.407990191586397932, 302.0882495255234517, 9.900872584904373497 ) ) ;
#25539 = FILL_AREA_STYLE_COLOUR ( '', #13349 ) ;
#25540 = CARTESIAN_POINT ( 'NONE',  ( 85.88830989802964666, -61.04876075054228579, 194.2276438132367673 ) ) ;
#25541 = CARTESIAN_POINT ( 'NONE',  ( 0.9542196423401080319, 34.32584019461168623, -29.31154340995110985 ) ) ;
#25542 = AXIS2_PLACEMENT_3D ( 'NONE', #66020, #65499, #66553 ) ;
#25543 = CARTESIAN_POINT ( 'NONE',  ( 7.188101187500000044, -31.15625000204838813, 0.000000000000000000 ) ) ;
#25544 = FACE_OUTER_BOUND ( 'NONE', #82118, .T. ) ;
#25545 = CARTESIAN_POINT ( 'NONE',  ( 8.559508646656405872, 51.55638410492942825, 4.031152949374444461 ) ) ;
#25546 = CIRCLE ( 'NONE', #87572, 3.309500000000007880 ) ;
#25547 = CARTESIAN_POINT ( 'NONE',  ( 38.08110185299304362, 439.4416046545700851, 23.85860822400425363 ) ) ;
#25548 = LINE ( 'NONE', #58407, #38452 ) ;
#25549 = ORIENTED_EDGE ( 'NONE', *, *, #71667, .T. ) ;
#25550 = DIRECTION ( 'NONE',  ( 0.000000000000000000, 0.000000000000000000, 1.000000000000000000 ) ) ;
#25551 = CYLINDRICAL_SURFACE ( 'NONE', #1525, 4.000000000000000000 ) ;
#25552 = CARTESIAN_POINT ( 'NONE',  ( 13.00569724287416307, 42.57699280172521128, -92.62012237565519968 ) ) ;
#25553 = EDGE_CURVE ( 'NONE', #7953, #49541, #18407, .T. ) ;
#25554 = B_SPLINE_CURVE_WITH_KNOTS ( 'NONE', 3,
 ( #65751, #71696, #7488, #32874, #72245, #81911, #97046, #31289, #89500, #23724, #38832, #73831, #106725, #104607, #64175, #98631, #90555, #46898, #79804, #96533, #5901, #23186 ),
 .UNSPECIFIED., .F., .F.,
 ( 4, 2, 2, 2, 2, 2, 2, 2, 2, 2, 4 ),
 ( 0.003250743696380571646, 0.003754779946395551526, 0.004258816196410531406, 0.004762852446425511720, 0.005266888696440491166, 0.005770924946455471480, 0.006022943071462952963, 0.006274961196470434446, 0.006526979321477914195, 0.006778997446485395678, 0.007283033696500349971 ),
 .UNSPECIFIED. ) ;
#25555 = ORIENTED_EDGE ( 'NONE', *, *, #13692, .F. ) ;
#25556 = CARTESIAN_POINT ( 'NONE',  ( 46.00000000000001421, 487.9843608680976104, -0.2179797824887820534 ) ) ;
#25557 = PRESENTATION_LAYER_ASSIGNMENT (  '', '', ( #97799 ) ) ;
#25558 = CARTESIAN_POINT ( 'NONE',  ( -37.56673239365849781, -1.200000000000000030E-05, 12.20617127781066102 ) ) ;
#25559 = CARTESIAN_POINT ( 'NONE',  ( -42.63927665720805749, 462.0185602173216353, 4.112661701945640402 ) ) ;
#25560 = CARTESIAN_POINT ( 'NONE',  ( 107.6015356060339911, -57.67123274086495854, 114.0084083295923563 ) ) ;
#25561 = EDGE_CURVE ( 'NONE', #33830, #39671, #60446, .T. ) ;
#25562 = AXIS2_PLACEMENT_3D ( 'NONE', #60764, #86641, #101205 ) ;
#25563 = CARTESIAN_POINT ( 'NONE',  ( 36.69926874265758698, 463.5184712008513657, 19.71956904107949882 ) ) ;
#25564 = DIRECTION ( 'NONE',  ( 0.000000000000000000, -1.000000000000000000, 0.000000000000000000 ) ) ;
#25565 = CYLINDRICAL_SURFACE ( 'NONE', #88911, 5.000000000000000888 ) ;
#25566 = CARTESIAN_POINT ( 'NONE',  ( 31.35596682365711274, 438.0939828603570732, 22.55458131664589061 ) ) ;
#25567 = CARTESIAN_POINT ( 'NONE',  ( -86.42863255622134488, -60.00000000000000000, 200.7652140804842134 ) ) ;
#25568 = CARTESIAN_POINT ( 'NONE',  ( 9.643395340371860414, 44.08772782729035100, -13.07263357742781196 ) ) ;
#25570 = CONICAL_SURFACE ( 'NONE', #99580, 4.172000000000001485, 0.9599310885968750373 ) ;
#25569 = DIRECTION ( 'NONE',  ( 0.000000000000000000, 0.000000000000000000, -1.000000000000000000 ) ) ;
#25571 = CARTESIAN_POINT ( 'NONE',  ( -58.76133767616301640, 50.00000000000000000, 23.44026136864787446 ) ) ;
#25572 = CONICAL_SURFACE ( 'NONE', #80647, 3.309500000000001663, 0.9599310885968770357 ) ;
#25573 = CARTESIAN_POINT ( 'NONE',  ( -84.96946970298199631, -35.81198127296185163, 180.8558154136740939 ) ) ;
#25574 = ORIENTED_EDGE ( 'NONE', *, *, #60303, .T. ) ;
#25575 = CARTESIAN_POINT ( 'NONE',  ( 28.98194489702799004, 310.1023937361698017, -7.790637802078380858 ) ) ;
#25576 = ORIENTED_EDGE ( 'NONE', *, *, #54281, .T. ) ;
#25577 = CARTESIAN_POINT ( 'NONE',  ( -6.928203230275509661, -10.00000000000000888, 4.000000000000000000 ) ) ;
#25578 = ADVANCED_FACE ( 'NONE', ( #101929 ), #95932, .T. ) ;
#25579 = CARTESIAN_POINT ( 'NONE',  ( -5.833333333333328596, -4.000000000000003553, 103.8776713793258608 ) ) ;
#25580 = CARTESIAN_POINT ( 'NONE',  ( -85.58543702643984830, -52.75005472265036843, -10.05567657277402382 ) ) ;
#25581 = AXIS2_PLACEMENT_3D ( 'NONE', #12155, #77965, #62329 ) ;
#25582 = DIRECTION ( 'NONE',  ( 0.000000000000000000, -1.000000000000000000, 0.000000000000000000 ) ) ;
#25583 = FACE_OUTER_BOUND ( 'NONE', #91922, .T. ) ;
#25585 = DIRECTION ( 'NONE',  ( -1.000000000000000000, -0.000000000000000000, -0.000000000000000000 ) ) ;
#25584 = CIRCLE ( 'NONE', #85864, 5.000000000000002665 ) ;
#25586 = CARTESIAN_POINT ( 'NONE',  ( 10.07445889136302419, 12.82167443387120720, -10.57244230701620857 ) ) ;
#25587 = CIRCLE ( 'NONE', #82437, 8.750000000000033751 ) ;
#25588 = CARTESIAN_POINT ( 'NONE',  ( 3.454253436624935336, -0.8414180287960453253, 103.7259032015043232 ) ) ;
#25589 = CARTESIAN_POINT ( 'NONE',  ( -35.73700087854410867, 437.1201388800316181, 4.567739269148499481 ) ) ;
#25590 = CARTESIAN_POINT ( 'NONE',  ( 49.63358250961842799, -60.00000000000001421, -40.41868810089377462 ) ) ;
#25591 = CARTESIAN_POINT ( 'NONE',  ( -79.25090170193163885, -32.55892561338175284, 134.6608944345848329 ) ) ;
#25592 = ORIENTED_EDGE ( 'NONE', *, *, #5535, .T. ) ;
#25593 = CARTESIAN_POINT ( 'NONE',  ( 77.10949051821226874, -30.00000000000007461, 176.8385238405566326 ) ) ;
#25594 = CARTESIAN_POINT ( 'NONE',  ( 7.986711519608433285, 88.97361903623433932, -0.5300249774147592907 ) ) ;
#25595 = CARTESIAN_POINT ( 'NONE',  ( 94.44279491447446162, -57.67056076577856771, -0.6735058548411319013 ) ) ;
#25596 = AXIS2_PLACEMENT_3D ( 'NONE', #57830, #90218, #49753 ) ;
#25597 = ORIENTED_EDGE ( 'NONE', *, *, #51259, .T. ) ;
#25598 = CARTESIAN_POINT ( 'NONE',  ( 7.350234075050753546, 52.09155505363125371, -3.136924920048258070 ) ) ;
#25599 = CARTESIAN_POINT ( 'NONE',  ( 32.33349330513379982, -4.000000000000000000, 4.898587196589415787E-16 ) ) ;
#25600 = ORIENTED_EDGE ( 'NONE', *, *, #61740, .F. ) ;
#25601 = CARTESIAN_POINT ( 'NONE',  ( 3.337162542380456721E-15, 35.08181111624585213, 27.25000000000000000 ) ) ;
#25602 = DIRECTION ( 'NONE',  ( 0.000000000000000000, 0.000000000000000000, -1.000000000000000000 ) ) ;
#25603 = CARTESIAN_POINT ( 'NONE',  ( 7.500000000000000000, 4.330127018922189208, -10.00000000000000000 ) ) ;
#25604 = CARTESIAN_POINT ( 'NONE',  ( -5.082755093536325042, -15.59375000204838635, -5.082755093536325930 ) ) ;
#25605 = CARTESIAN_POINT ( 'NONE',  ( 7.112481253775658985, -4.553861071372089064, -7.781689322727664226 ) ) ;
#25606 = CARTESIAN_POINT ( 'NONE',  ( 1.116646360188462639, -0.001721104702690063248, 101.1925744066307402 ) ) ;
#25607 = DIRECTION ( 'NONE',  ( 0.000000000000000000, -1.000000000000000000, 0.000000000000000000 ) ) ;
#25608 = CARTESIAN_POINT ( 'NONE',  ( 23.09999999999999432, 1.533819458162526451E-15, 0.000000000000000000 ) ) ;
#25609 = CARTESIAN_POINT ( 'NONE',  ( 27.99999999999999645, 0.000000000000000000, 9.000000000000000000 ) ) ;
#25610 = CARTESIAN_POINT ( 'NONE',  ( -4.644559862127823457, 47.99999999999999289, -99.31133601631378838 ) ) ;
#25611 = AXIS2_PLACEMENT_3D ( 'NONE', #88017, #95059, #21193 ) ;
#25612 = ORIENTED_EDGE ( 'NONE', *, *, #26556, .F. ) ;
#25613 = CARTESIAN_POINT ( 'NONE',  ( -7.159011624722488421, 41.04792457232633751, -70.58264774317923695 ) ) ;
#25615 = CARTESIAN_POINT ( 'NONE',  ( 32.05687126736489745, -60.31738256606855231, 37.68480598271252546 ) ) ;
#25614 = SURFACE_SIDE_STYLE ('',( #8843 ) ) ;
#25616 = CARTESIAN_POINT ( 'NONE',  ( 21.67097115919219519, 305.0473406493022139, -8.958495691138132599 ) ) ;
#25617 = ORIENTED_EDGE ( 'NONE', *, *, #7280, .F. ) ;
#25618 = CARTESIAN_POINT ( 'NONE',  ( -0.07765829730716486412, 12.91535575337015196, 51.74999999999997868 ) ) ;
#25619 = PRESENTATION_LAYER_ASSIGNMENT (  '', '', ( #72070 ) ) ;
#25620 = ORIENTED_EDGE ( 'NONE', *, *, #605, .T. ) ;
#25622 = CARTESIAN_POINT ( 'NONE',  ( -0.6448886116837295734, 44.02064573959138016, -16.41618173662891778 ) ) ;
#25621 = CARTESIAN_POINT ( 'NONE',  ( 0.05533025579362249591, -6.264553569211843254, 2.149474931388136945 ) ) ;
#25623 = DIRECTION ( 'NONE',  ( 0.000000000000000000, -1.000000000000000000, 0.000000000000000000 ) ) ;
#25624 = CARTESIAN_POINT ( 'NONE',  ( -15.42316984156294168, 294.5569238556877849, -2.062679335141809123 ) ) ;
#25625 = SURFACE_STYLE_USAGE ( .BOTH. , #68166 ) ;
#25626 = CARTESIAN_POINT ( 'NONE',  ( 0.7848998160350572073, 45.39389416767541263, 18.48651031598092587 ) ) ;
#25627 = CARTESIAN_POINT ( 'NONE',  ( 2.607260012660386551E-19, 12.91535575337012354, -51.75000000000000711 ) ) ;
#25629 = ORIENTED_EDGE ( 'NONE', *, *, #49192, .T. ) ;
#25628 = MECHANICAL_DESIGN_GEOMETRIC_PRESENTATION_REPRESENTATION (  '', ( #11788 ), #4955 ) ;
#25630 = CARTESIAN_POINT ( 'NONE',  ( 84.25014938015986843, -60.00000000000002132, -25.16421652135344544 ) ) ;
#25631 = CARTESIAN_POINT ( 'NONE',  ( -10.28624191512074226, 46.12099395432516502, 12.90779740155501187 ) ) ;
#25632 = SURFACE_SIDE_STYLE ('',( #33700 ) ) ;
#25633 = CARTESIAN_POINT ( 'NONE',  ( 0.000000000000000000, 0.000000000000000000, -6.838999999999999524 ) ) ;
#25634 = FACE_OUTER_BOUND ( 'NONE', #27720, .T. ) ;
#25635 = ORIENTED_EDGE ( 'NONE', *, *, #84151, .T. ) ;
#25636 = ADVANCED_FACE ( 'NONE', ( #10260 ), #68366, .T. ) ;
#25637 = CARTESIAN_POINT ( 'NONE',  ( -46.00000000000000000, 438.3878896346936358, 16.22878885428542262 ) ) ;
#25638 = ORIENTED_EDGE ( 'NONE', *, *, #33068, .T. ) ;
#25639 = ORIENTED_EDGE ( 'NONE', *, *, #80510, .T. ) ;
#25640 = CYLINDRICAL_SURFACE ( 'NONE', #98594, 8.000000000000000000 ) ;
#25641 = CARTESIAN_POINT ( 'NONE',  ( 7.897836333153806621, 1.530409084195003100, -7.633857274177628049 ) ) ;
#25642 = DIRECTION ( 'NONE',  ( -1.000000000000000000, -1.224606353822377258E-16, -0.000000000000000000 ) ) ;
#25643 = CARTESIAN_POINT ( 'NONE',  ( 83.22070310856115327, -37.82803493101771153, -4.681492691623674318 ) ) ;
#25644 = CARTESIAN_POINT ( 'NONE',  ( -30.75264184865481809, 308.9867225161979718, -8.589175589975059921 ) ) ;
#25645 = DIRECTION ( 'NONE',  ( -1.000000000000000000, -1.224606353822377258E-16, -0.000000000000000000 ) ) ;
#25646 = CARTESIAN_POINT ( 'NONE',  ( 12.50000000000000533, 27.20503041222523066, -44.74618841300883076 ) ) ;
#25647 = CONICAL_SURFACE ( 'NONE', #10044, 3.309500000000001663, 0.9599310885968770357 ) ;
#25648 = ORIENTED_EDGE ( 'NONE', *, *, #14860, .F. ) ;
#25650 = EDGE_CURVE ( 'NONE', #79080, #78182, #53394, .T. ) ;
#25649 = CARTESIAN_POINT ( 'NONE',  ( 6.500000000000000000, 0.3213925021621148459, 3.091246741004567904E-15 ) ) ;
#25651 = EDGE_LOOP ( 'NONE', ( #50758, #83381, #76385, #43658, #92654, #57045 ) ) ;
#25652 = DIRECTION ( 'NONE',  ( 0.000000000000000000, 1.000000000000000000, -0.000000000000000000 ) ) ;
#25653 = DIRECTION ( 'NONE',  ( -1.000000000000000000, -1.224606353822377258E-16, -0.000000000000000000 ) ) ;
#25654 = CIRCLE ( 'NONE', #54840, 0.5000000000000004441 ) ;
#25656 = ORIENTED_EDGE ( 'NONE', *, *, #35012, .F. ) ;
#25655 = DIRECTION ( 'NONE',  ( -1.000000000000000000, -1.224606353822377258E-16, -0.000000000000000000 ) ) ;
#25657 = CARTESIAN_POINT ( 'NONE',  ( 76.83599883816330589, -18.66163333761462439, 113.2182193956237057 ) ) ;
#25658 = AXIS2_PLACEMENT_3D ( 'NONE', #88659, #14220, #62803 ) ;
#25659 = VERTEX_POINT ( 'NONE', #10777 ) ;
#25660 = EDGE_CURVE ( 'NONE', #96955, #23524, #25266, .T. ) ;
#25661 = FACE_OUTER_BOUND ( 'NONE', #66673, .T. ) ;
#25662 = CARTESIAN_POINT ( 'NONE',  ( 2.977408999572652260, -22.43750000204838813, 7.188101187500000044 ) ) ;
#25663 =( BOUNDED_SURFACE ( )  B_SPLINE_SURFACE ( 3, 2, ( 
 ( #25253, #33875, #41933 ),
 ( #27405, #1996, #60283 ),
 ( #66752, #93152, #67292 ),
 ( #58667, #99091, #75899 ) ),
 .UNSPECIFIED., .F., .F., .T. ) 
 B_SPLINE_SURFACE_WITH_KNOTS ( ( 4, 4 ),
 ( 3, 3 ),
 ( 0.01114851999726041223, 0.01303042415394033669 ),
 ( 0.1618064000426147064, 1.000000000000000000 ),
 .UNSPECIFIED. ) 
 GEOMETRIC_REPRESENTATION_ITEM ( )  RATIONAL_B_SPLINE_SURFACE ( (
 ( 0.9362898844563825040, 0.8031285674520963758, 1.000000000000000000),
 ( 0.9312276682860366472, 0.7874857493404125997, 1.000000000000000000),
 ( 0.9259581024412342209, 0.7712021973813599773, 1.000000000000000000),
 ( 0.9205526622925819247, 0.7544987785202129649, 1.000000000000000000) ) ) 
 REPRESENTATION_ITEM ( '' )  SURFACE ( )  );
#25664 = CARTESIAN_POINT ( 'NONE',  ( -80.00483118099813851, -57.67118036264142944, -30.22182926596574148 ) ) ;
#25665 = EDGE_CURVE ( 'NONE', #11792, #82981, #86315, .T. ) ;
#25666 = VERTEX_POINT ( 'NONE', #59907 ) ;
#25667 = CARTESIAN_POINT ( 'NONE',  ( 6.575918192882429736, -7.701766175471821185, 1.336937141848248750E-15 ) ) ;
#25668 = CONICAL_SURFACE ( 'NONE', #54858, 3.309500000000001663, 0.9599310885968770357 ) ;
#25669 = CARTESIAN_POINT ( 'NONE',  ( 103.8601077188106672, -45.28281436907764146, 165.7359996305474112 ) ) ;
#25670 = CARTESIAN_POINT ( 'NONE',  ( -36.47828316237969659, 491.8387149836262324, 12.58546224878396735 ) ) ;
#25671 = DIRECTION ( 'NONE',  ( 0.000000000000000000, -1.000000000000000000, 0.000000000000000000 ) ) ;
#25672 = CARTESIAN_POINT ( 'NONE',  ( 5.656854249492380582, -26.00000000409677270, -5.656854249492379694 ) ) ;
#25673 = DIRECTION ( 'NONE',  ( 0.000000000000000000, -1.000000000000000000, 0.000000000000000000 ) ) ;
#25674 = MECHANICAL_DESIGN_GEOMETRIC_PRESENTATION_REPRESENTATION (  '', ( #91086 ), #56706 ) ;
#25675 = CARTESIAN_POINT ( 'NONE',  ( -36.49843703712726750, 25.91515891220674206, 12.86019707471129436 ) ) ;
#25676 = DIRECTION ( 'NONE',  ( 0.000000000000000000, -1.000000000000000000, 0.000000000000000000 ) ) ;
#25677 = CARTESIAN_POINT ( 'NONE',  ( 9.699121749566360862, 33.17668760275819295, 2.444499528233558205 ) ) ;
#25678 = DIRECTION ( 'NONE',  ( -1.000000000000000000, -1.224606353822377258E-16, -0.000000000000000000 ) ) ;
#25679 = CARTESIAN_POINT ( 'NONE',  ( -0.5170823471680870975, 572.1183258647163257, 155.1969486012868629 ) ) ;
#25680 = CARTESIAN_POINT ( 'NONE',  ( 0.000000000000000000, 15.00000000000000000, -9.999999999999998224 ) ) ;
#25681 = VERTEX_POINT ( 'NONE', #12380 ) ;
#25682 = FILL_AREA_STYLE ('',( #17024 ) ) ;
#25683 = CARTESIAN_POINT ( 'NONE',  ( 1.224646799147353256E-15, 115.0000000000000000, 10.00000000000000000 ) ) ;
#25684 = CARTESIAN_POINT ( 'NONE',  ( -4.999999999999999112, -46.02080548338511790, 5.909847384900872136 ) ) ;
#25685 = CARTESIAN_POINT ( 'NONE',  ( -92.68948487369793554, -30.00000000000000355, 191.0483739415028310 ) ) ;
#25686 = EDGE_CURVE ( 'NONE', #76857, #20022, #6276, .T. ) ;
#25687 = COLOUR_RGB ( '', 0.31764706, 0.68627451, 0.89019608) ;
#25688 = ORIENTED_EDGE ( 'NONE', *, *, #92514, .T. ) ;
#25689 = AXIS2_PLACEMENT_3D ( 'NONE', #47380, #40890, #106133 ) ;
#25690 = CARTESIAN_POINT ( 'NONE',  ( 6.231493956936422940, 4.173545622688802581, 0.000000000000000000 ) ) ;
#25691 = CARTESIAN_POINT ( 'NONE',  ( 63.69210850852088868, -57.67891201327802975, 121.2445212169528475 ) ) ;
#25693 = CARTESIAN_POINT ( 'NONE',  ( -9.554383626907007709, 53.41962121727333823, 3.542541134239667766 ) ) ;
#25692 = CARTESIAN_POINT ( 'NONE',  ( 80.00000000000000000, -52.00000000000000000, -21.09707704303352926 ) ) ;
#25694 = EDGE_CURVE ( 'NONE', #68832, #81828, #18938, .T. ) ;
#25695 = EDGE_CURVE ( 'NONE', #36026, #44445, #43174, .T. ) ;
#25696 = CONICAL_SURFACE ( 'NONE', #94588, 8.000000000000000000, 1.047197551196600296 ) ;
#25697 = AXIS2_PLACEMENT_3D ( 'NONE', #33220, #17026, #74700 ) ;
#25698 = CARTESIAN_POINT ( 'NONE',  ( 20.69727557552225505, -26.09496662598620276, -38.47203802730707878 ) ) ;
#25699 = CARTESIAN_POINT ( 'NONE',  ( -7.500000000000000000, -3.988190556646209917, -0.8526458641284285767 ) ) ;
#25700 = CARTESIAN_POINT ( 'NONE',  ( -42.08762648273019380, 487.0030674539066808, 9.106351919860241395 ) ) ;
#25701 = CARTESIAN_POINT ( 'NONE',  ( -36.13861969606174540, -60.00000000000002132, 47.48874267815981653 ) ) ;
#25702 = DIRECTION ( 'NONE',  ( -0.5735764363510461594, 0.8191520442889916875, 1.003171929053524870E-16 ) ) ;
#25703 = CONICAL_SURFACE ( 'NONE', #72164, 4.999999999999999112, 0.7853981633974543852 ) ;
#25704 = CARTESIAN_POINT ( 'NONE',  ( 1.250306967194193764, 45.68544320488086896, -17.65754872500330208 ) ) ;
#25705 = CARTESIAN_POINT ( 'NONE',  ( -86.86729174969509870, -24.34025208997100620, 185.9213970984535820 ) ) ;
#25706 = ORIENTED_EDGE ( 'NONE', *, *, #27043, .F. ) ;
#25707 = CARTESIAN_POINT ( 'NONE',  ( 5.656854249492380582, -12.31249999999999289, -5.656854249492379694 ) ) ;
#25708 = CARTESIAN_POINT ( 'NONE',  ( -6.226963257687841313, -60.36578172299497425, 33.94043655557382522 ) ) ;
#25709 = DIRECTION ( 'NONE',  ( -1.000000000000000000, -0.000000000000000000, -0.000000000000000000 ) ) ;
#25710 = SURFACE_STYLE_USAGE ( .BOTH. , #33775 ) ;
#25712 = CARTESIAN_POINT ( 'NONE',  ( 4.899502675980784261, -65.60435911681314280, 13.86139633465681698 ) ) ;
#25711 = CARTESIAN_POINT ( 'NONE',  ( -0.2813450144774510275, -7.667988119308891903, -6.122077150241868715 ) ) ;
#25713 = ORIENTED_EDGE ( 'NONE', *, *, #41767, .F. ) ;
#25714 = EDGE_CURVE ( 'NONE', #98133, #76468, #42474, .T. ) ;
#25715 =( LENGTH_UNIT ( ) NAMED_UNIT ( * ) SI_UNIT ( .MILLI., .METRE. ) );
#25716 = AXIS2_PLACEMENT_3D ( 'NONE', #89561, #57173, #65810 ) ;
#25717 = CARTESIAN_POINT ( 'NONE',  ( -9.544165109479243014, -4.999999999999968026, -19.39317919831048442 ) ) ;
#25718 = CARTESIAN_POINT ( 'NONE',  ( -8.000086790516059310, 34.00017358106006071, 0.2639471549312804033 ) ) ;
#25719 = CARTESIAN_POINT ( 'NONE',  ( 27.02761694636049583, 305.0378212988403561, -9.518998403309037570 ) ) ;
#25720 = CARTESIAN_POINT ( 'NONE',  ( 27.33349330513380337, 1.593028355512270567E-15, 0.000000000000000000 ) ) ;
#25721 = ADVANCED_FACE ( 'NONE', ( #51780 ), #80347, .T. ) ;
#25722 = CARTESIAN_POINT ( 'NONE',  ( 0.000000000000000000, 0.000000000000000000, -12.97459999999999525 ) ) ;
#25723 = CARTESIAN_POINT ( 'NONE',  ( 4.250000000000000000, 0.000000000000000000, -9.078441367943003826 ) ) ;
#25724 = CARTESIAN_POINT ( 'NONE',  ( 114.5768552918926986, -59.99999999999997868, 170.6725192690976485 ) ) ;
#25725 = CARTESIAN_POINT ( 'NONE',  ( -82.36662456894917739, -36.02719610116624693, 158.6189278519784409 ) ) ;
#25726 = ORIENTED_EDGE ( 'NONE', *, *, #102568, .T. ) ;
#25727 = DIRECTION ( 'NONE',  ( 1.000000000000000000, 0.000000000000000000, 0.000000000000000000 ) ) ;
#25728 = CARTESIAN_POINT ( 'NONE',  ( -9.221216839714882596, 251.0475974816896496, 3.869414262757008505 ) ) ;
#25729 = CARTESIAN_POINT ( 'NONE',  ( 6.683837171061806082, -3.955946848495971668, -6.851900933636991375 ) ) ;
#25730 = EDGE_CURVE ( 'NONE', #66061, #66358, #97021, .T. ) ;
#25731 = CARTESIAN_POINT ( 'NONE',  ( 3.168296453696544557, 39.18458251124699387, -5.000000000000000000 ) ) ;
#25732 = AXIS2_PLACEMENT_3D ( 'NONE', #106274, #72847, #41033 ) ;
#25733 = DIRECTION ( 'NONE',  ( -1.000000000000000000, -1.224606353822377258E-16, -0.000000000000000000 ) ) ;
#25734 = ORIENTED_EDGE ( 'NONE', *, *, #2446, .T. ) ;
#25735 = B_SPLINE_CURVE_WITH_KNOTS ( 'NONE', 3,
 ( #16055, #40863, #73755, #63310, #2524, #93684, #30416, #71373 ),
 .UNSPECIFIED., .F., .F.,
 ( 4, 2, 2, 4 ),
 ( 0.000000000000000000, 0.2500000000000000000, 0.5000000000000000000, 1.000000000000000000 ),
 .UNSPECIFIED. ) ;
#25736 = UNCERTAINTY_MEASURE_WITH_UNIT (LENGTH_MEASURE( 1.000000000000000082E-05 ), #63563, 'distance_accuracy_value', 'NONE');
#25737 = CARTESIAN_POINT ( 'NONE',  ( -5.656854249492379694, -22.43749999999999289, -5.656854249492380582 ) ) ;
#25738 = VERTEX_POINT ( 'NONE', #30736 ) ;
#25739 = CARTESIAN_POINT ( 'NONE',  ( 37.33349330513379982, 1.593028355512270567E-15, 0.000000000000000000 ) ) ;
#25740 = CARTESIAN_POINT ( 'NONE',  ( 4.165977904505311358, 15.00000000000000000, 9.090909090909089940 ) ) ;
#25741 = CARTESIAN_POINT ( 'NONE',  ( 31.96724538747933764, 486.9512181893505272, 7.078368790602016070 ) ) ;
#25742 = CARTESIAN_POINT ( 'NONE',  ( -43.69716417794982277, 48.00000000000000000, 48.48761666242421597 ) ) ;
#25743 = CARTESIAN_POINT ( 'NONE',  ( 5.000000000000000000, -15.62228920881129746, 12.61250543006183733 ) ) ;
#25744 = B_SPLINE_CURVE_WITH_KNOTS ( 'NONE', 3,
 ( #29292, #102609, #77805, #46493, #38427, #47009, #20686, #38941, #54030, #30329, #21717, #5504, #12515, #96112, #3917, #63221, #30874, #52998, #61645, #36849, #45446, #78321, #54558, #22246, #95581, #37908, #103664, #55093, #11990, #85917, #44920, #45971, #69715, #79383, #104721, #28765, #88023, #79908, #14103, #6017, #95064, #94537, #71292, #4437, #37381, #29814, #71818, #70242, #63753, #103144, #13577, #62174 ),
 .UNSPECIFIED., .F., .F.,
 ( 4, 1, 1, 1, 1, 1, 1, 1, 1, 1, 2, 2, 1, 1, 1, 1, 1, 1, 1, 1, 2, 2, 1, 1, 1, 1, 1, 1, 1, 1, 1, 2, 2, 1, 1, 1, 1, 1, 1, 2, 2, 4 ),
 ( 0.000000000000000000, 0.1250000000003060330, 0.1875000000004590495, 0.2187500000005354606, 0.2343750000005737633, 0.2421875000005931089, 0.2460937500006027678, 0.2480468750006076251, 0.2490234375006100398, 0.2495117187506111223, 0.2497558593756118717, 0.2500000000006126211, 0.3125000000007527312, 0.3437500000008228418, 0.3593750000008577583, 0.3671875000008750778, 0.3710937500008839041, 0.3730468750008880674, 0.3740234375008901768, 0.3745117187508911205, 0.3747558593758917311, 0.3750000000008923418, 0.4375000000010839107, 0.4687500000011795565, 0.4843750000012275736, 0.4921875000012514989, 0.4960937500012632118, 0.4980468750012684298, 0.4990234375012703727, 0.4995117187512707058, 0.4997558593762702062, 0.4998779296887702062, 0.5000000000012702062, 0.6250000000009643397, 0.6875000000008114620, 0.7187500000007353007, 0.7343750000006972201, 0.7421875000006779022, 0.7460937500006681322, 0.7480468750006629142, 0.7500000000006576961, 1.000000000000000000 ),
 .UNSPECIFIED. ) ;
#25745 = CARTESIAN_POINT ( 'NONE',  ( 46.00000000000000000, 437.8919113138612147, 12.69150955564872874 ) ) ;
#25746 = EDGE_LOOP ( 'NONE', ( #86958, #48012, #106109, #9469, #68177, #3623 ) ) ;
#25747 = CARTESIAN_POINT ( 'NONE',  ( 103.9293398954433201, -60.00000000000001421, 200.0405719490170213 ) ) ;
#25749 = CARTESIAN_POINT ( 'NONE',  ( 15.30468211099681319, -18.58757702105601339, 27.14322304785206441 ) ) ;
#25748 = CARTESIAN_POINT ( 'NONE',  ( -75.43392636619238090, -30.00000000000003553, 160.3050061908775206 ) ) ;
#25750 = CARTESIAN_POINT ( 'NONE',  ( 82.23886140992384242, -37.99999999999997868, -13.37499424629273292 ) ) ;
#25751 = CARTESIAN_POINT ( 'NONE',  ( -39.23155690887019631, -18.76732848933246700, 33.52670975879949822 ) ) ;
#25752 = CARTESIAN_POINT ( 'NONE',  ( 101.4868948250290259, 1.016364837396684119E-14, 0.000000000000000000 ) ) ;
#25753 = EDGE_LOOP ( 'NONE', ( #40389, #12120, #78299, #82905 ) ) ;
#25754 = CARTESIAN_POINT ( 'NONE',  ( -6.539732759932832096, -4.285714285714296246, 24.41571844174603001 ) ) ;
#25755 = CARTESIAN_POINT ( 'NONE',  ( 7.308143880813624094, 54.29032144469603338, 2.719777064722692650 ) ) ;
#25756 = CARTESIAN_POINT ( 'NONE',  ( 39.13885763974980136, 324.4948203046521371, 17.18769520460729439 ) ) ;
#25757 = MECHANICAL_DESIGN_GEOMETRIC_PRESENTATION_REPRESENTATION (  '', ( #1579 ), #49792 ) ;
#25758 = FILL_AREA_STYLE ('',( #99581 ) ) ;
#25759 = CARTESIAN_POINT ( 'NONE',  ( 20.24579557674104890, 304.8297271373346575, -10.00469232190994084 ) ) ;
#25760 = CARTESIAN_POINT ( 'NONE',  ( -32.10528697966012857, 486.1671898930081852, 5.449875171704860577 ) ) ;
#25761 = ORIENTED_EDGE ( 'NONE', *, *, #89741, .F. ) ;
#25762 = CARTESIAN_POINT ( 'NONE',  ( -46.09313609967871628, -38.31867567570748179, 60.02686483055563826 ) ) ;
#25763 = DIRECTION ( 'NONE',  ( 0.000000000000000000, -1.000000000000000000, 0.000000000000000000 ) ) ;
#25764 = ORIENTED_EDGE ( 'NONE', *, *, #64330, .F. ) ;
#25765 = CARTESIAN_POINT ( 'NONE',  ( 80.80396565660879560, -29.99999999999999289, -12.40573726492647744 ) ) ;
#25766 = CARTESIAN_POINT ( 'NONE',  ( 47.57454933833927413, 12.59078750739571184, 14.43852527042908918 ) ) ;
#25767 = UNCERTAINTY_MEASURE_WITH_UNIT (LENGTH_MEASURE( 1.000000000000000082E-05 ), #98562, 'distance_accuracy_value', 'NONE');
#25768 = CARTESIAN_POINT ( 'NONE',  ( 23.54584815914472884, 25.90672388542958871, -30.73942196852247122 ) ) ;
#25769 = CARTESIAN_POINT ( 'NONE',  ( 14.33580413386840213, 42.00000000000000000, -89.41414995614803729 ) ) ;
#25770 = CARTESIAN_POINT ( 'NONE',  ( 82.65538836485218610, -30.00000000000001421, 40.06710242176322367 ) ) ;
#25771 = CARTESIAN_POINT ( 'NONE',  ( -32.18152649027052803, 409.5700136857448683, 25.68904360494498462 ) ) ;
#25772 = ORIENTED_EDGE ( 'NONE', *, *, #94239, .F. ) ;
#25773 = ADVANCED_FACE ( 'NONE', ( #46359 ), #13966, .T. ) ;
#25774 = AXIS2_PLACEMENT_3D ( 'NONE', #89479, #90532, #41446 ) ;
#25775 = VERTEX_POINT ( 'NONE', #87358 ) ;
#25776 = EDGE_LOOP ( 'NONE', ( #58240, #7146, #104042, #98660, #86592 ) ) ;
#25777 = DIRECTION ( 'NONE',  ( 1.000000000000000000, 0.000000000000000000, 0.000000000000000000 ) ) ;
#25778 = CARTESIAN_POINT ( 'NONE',  ( -6.406311626395538639, 41.42610740534730240, -70.78720125084922188 ) ) ;
#25779 = CARTESIAN_POINT ( 'NONE',  ( 86.17777777777776294, -4.171999999999998820, 0.000000000000000000 ) ) ;
#25780 = CARTESIAN_POINT ( 'NONE',  ( 5.191144708981717315, -12.64030085521269342, 3.015512395308848070 ) ) ;
#25781 = CARTESIAN_POINT ( 'NONE',  ( -30.38822253705984977, 339.6140856355796132, 18.22937297894274522 ) ) ;
#25782 = EDGE_CURVE ( 'NONE', #13321, #86116, #104580, .T. ) ;
#25783 =( NAMED_UNIT ( * ) SI_UNIT ( $, .STERADIAN. ) SOLID_ANGLE_UNIT ( ) );
#25785 = VERTEX_POINT ( 'NONE', #96511 ) ;
#25784 = STYLED_ITEM ( 'NONE', ( #95036 ), #33976 ) ;
#25787 = EDGE_CURVE ( 'NONE', #63799, #35905, #80869, .T. ) ;
#25786 = CARTESIAN_POINT ( 'NONE',  ( 42.73089261237365832, 435.7309723475635224, 18.11242468272458339 ) ) ;
#25788 = ORIENTED_EDGE ( 'NONE', *, *, #73923, .T. ) ;
#25789 = FACE_OUTER_BOUND ( 'NONE', #14170, .T. ) ;
#25790 = CARTESIAN_POINT ( 'NONE',  ( 75.07689429088097199, -38.33936338830137203, 170.2545699534454400 ) ) ;
#25791 = LINE ( 'NONE', #100153, #12997 ) ;
#25792 = CARTESIAN_POINT ( 'NONE',  ( 24.42072771677381127, 304.1864907082163541, 10.22967129747842385 ) ) ;
#25793 = AXIS2_PLACEMENT_3D ( 'NONE', #74504, #42141, #76101 ) ;
#25794 = EDGE_CURVE ( 'NONE', #86992, #82401, #5878, .T. ) ;
#25795 = DIRECTION ( 'NONE',  ( -0.8191520442889884679, 1.003171929053520679E-16, 0.5735764363510509334 ) ) ;
#25796 = ADVANCED_FACE ( 'NONE', ( #103529 ), #8056, .T. ) ;
#25797 = ORIENTED_EDGE ( 'NONE', *, *, #105393, .F. ) ;
#25798 = ADVANCED_FACE ( 'NONE', ( #22644 ), #35670, .F. ) ;
#25799 = CARTESIAN_POINT ( 'NONE',  ( 4.551587301587304957, -1.200583151104947843, 104.4018401814738155 ) ) ;
#25800 = CARTESIAN_POINT ( 'NONE',  ( 33.96616553272742323, 301.6615848611037904, 3.484217928160723954 ) ) ;
#25801 = DIRECTION ( 'NONE',  ( 0.2042951644570906167, 0.03948950745688053349, 0.9781125009835337503 ) ) ;
#25802 = DIRECTION ( 'NONE',  ( 1.000000000000000000, 0.000000000000000000, 0.000000000000000000 ) ) ;
#25803 = ORIENTED_EDGE ( 'NONE', *, *, #511, .F. ) ;
#25804 = AXIS2_PLACEMENT_3D ( 'NONE', #1862, #58536, #57436 ) ;
#25805 = CARTESIAN_POINT ( 'NONE',  ( -25.49348957563488227, 295.8024135625230429, 2.141455523061916999 ) ) ;
#25806 = CARTESIAN_POINT ( 'NONE',  ( 28.58349330513380337, 1.593028355512270567E-15, 0.000000000000000000 ) ) ;
#25807 = UNCERTAINTY_MEASURE_WITH_UNIT (LENGTH_MEASURE( 1.000000000000000082E-05 ), #106682, 'distance_accuracy_value', 'NONE');
#25808 = DIRECTION ( 'NONE',  ( 0.5735764363510468256, 0.8191520442889913545, 0.000000000000000000 ) ) ;
#25809 = DIRECTION ( 'NONE',  ( -1.000000000000000000, -1.224606353822377258E-16, -0.000000000000000000 ) ) ;
#25810 = CARTESIAN_POINT ( 'NONE',  ( 33.00000000000000000, 500.0000000000002274, 0.000000000000000000 ) ) ;
#25811 = CARTESIAN_POINT ( 'NONE',  ( 9.819056950928633398, 294.6481068335447731, 1.893705519456528208 ) ) ;
#25812 = CIRCLE ( 'NONE', #53325, 0.5000000000000000000 ) ;
#25813 = DIRECTION ( 'NONE',  ( 0.000000000000000000, 0.000000000000000000, 1.000000000000000000 ) ) ;
#25814 = CARTESIAN_POINT ( 'NONE',  ( 85.02982003489246665, -46.56546437767619295, 187.6125479875748283 ) ) ;
#25815 = CARTESIAN_POINT ( 'NONE',  ( 43.71037717921923615, 462.3391554988761527, 4.824299547763561513 ) ) ;
#25816 = DIRECTION ( 'NONE',  ( 0.000000000000000000, -1.000000000000000000, 0.000000000000000000 ) ) ;
#25817 = ORIENTED_EDGE ( 'NONE', *, *, #27362, .T. ) ;
#25818 = CARTESIAN_POINT ( 'NONE',  ( 85.03610603180797511, -57.67078060003379392, -26.99171295196738285 ) ) ;
#25819 = CARTESIAN_POINT ( 'NONE',  ( 0.000000000000000000, 0.000000000000000000, 0.000000000000000000 ) ) ;
#25820 = LINE ( 'NONE', #67822, #9321 ) ;
#25821 = FILL_AREA_STYLE ('',( #33347 ) ) ;
#25822 = CARTESIAN_POINT ( 'NONE',  ( -80.80785939509713955, -29.99999999999999645, 8.456651002378157145 ) ) ;
#25823 = CARTESIAN_POINT ( 'NONE',  ( -6.763062896852164663, 41.48827110272769403, -70.48955655162545497 ) ) ;
#25824 = CARTESIAN_POINT ( 'NONE',  ( -4.406466114815700941, 6.116179640280957841, -7.446478553995463656 ) ) ;
#25825 = CIRCLE ( 'NONE', #1650, 3.309500000000001663 ) ;
#25827 = CARTESIAN_POINT ( 'NONE',  ( 24.34999999999999787, 1.533819458162526451E-15, 0.000000000000000000 ) ) ;
#25826 = DIRECTION ( 'NONE',  ( 0.000000000000000000, 0.000000000000000000, -1.000000000000000000 ) ) ;
#25828 = EDGE_CURVE ( 'NONE', #66609, #92310, #54540, .T. ) ;
#25829 = DIRECTION ( 'NONE',  ( -1.000000000000000000, -1.224606353822377258E-16, -0.000000000000000000 ) ) ;
#25830 = CARTESIAN_POINT ( 'NONE',  ( -31.62289491507650041, 439.0131222673971365, 23.39481604279367488 ) ) ;
#25831 = FACE_OUTER_BOUND ( 'NONE', #46177, .T. ) ;
#25832 = CARTESIAN_POINT ( 'NONE',  ( 5.093082057083965886, -82.55553793578430088, -3.176439207277721000 ) ) ;
#25833 = DIRECTION ( 'NONE',  ( 0.7611201562151608258, 0.000000000000000000, -0.6486109063244381856 ) ) ;
#25834 = CARTESIAN_POINT ( 'NONE',  ( 44.51476414916738378, 462.1216129963507910, 5.766699645629802973 ) ) ;
#25835 = CIRCLE ( 'NONE', #20681, 6.000000000000000888 ) ;
#25836 = CARTESIAN_POINT ( 'NONE',  ( 33.94783393359901424, 484.1261039197349305, 1.321740980884986039 ) ) ;
#25837 = ORIENTED_EDGE ( 'NONE', *, *, #101853, .T. ) ;
#25838 = DIRECTION ( 'NONE',  ( -1.000000000000000000, -1.224606353822377258E-16, -0.000000000000000000 ) ) ;
#25839 = CARTESIAN_POINT ( 'NONE',  ( -6.944031699373469202, 84.46539345443871127, 3.972913591453821613 ) ) ;
#25840 = CARTESIAN_POINT ( 'NONE',  ( 0.000000000000000000, 0.000000000000000000, 8.500000000000000000 ) ) ;
#25842 = CARTESIAN_POINT ( 'NONE',  ( -68.05023500849456752, -60.22824080543345104, -27.16814012153120927 ) ) ;
#25841 = FACE_OUTER_BOUND ( 'NONE', #6437, .T. ) ;
#25843 = VERTEX_POINT ( 'NONE', #55479 ) ;
#25844 = VECTOR ( 'NONE', #50091, 1000.000000000000000 ) ;
#25845 = DIRECTION ( 'NONE',  ( -1.000000000000000000, -1.224606353822377258E-16, -0.000000000000000000 ) ) ;
#25846 = CIRCLE ( 'NONE', #87784, 5.000000000000011546 ) ;
#25847 = ORIENTED_EDGE ( 'NONE', *, *, #13288, .F. ) ;
#25848 = CARTESIAN_POINT ( 'NONE',  ( 13.58349330513380160, 1.593028355512270567E-15, 0.000000000000000000 ) ) ;
#25849 = STYLED_ITEM ( 'NONE', ( #96883 ), #34362 ) ;
#25850 = EDGE_CURVE ( 'NONE', #6296, #106169, #20218, .T. ) ;
#25851 = CARTESIAN_POINT ( 'NONE',  ( -5.450967621166013188, 4.358435876040994472, -0.3607371497494452073 ) ) ;
#25852 = CARTESIAN_POINT ( 'NONE',  ( -66.22057664901657859, -60.00000000000000000, -33.82046026944324524 ) ) ;
#25853 = EDGE_LOOP ( 'NONE', ( #90153, #7922 ) ) ;
#25854 = DIRECTION ( 'NONE',  ( -2.742080092235280244E-17, 0.000000000000000000, 1.000000000000000000 ) ) ;
#25855 = CARTESIAN_POINT ( 'NONE',  ( -7.312676561755618643, 54.25590764141821154, -2.971987819145548215 ) ) ;
#25856 = CARTESIAN_POINT ( 'NONE',  ( 99.66320498351910828, -45.27082587009371650, 192.8921995371364631 ) ) ;
#25858 = CARTESIAN_POINT ( 'NONE',  ( -17.89160253087132801, 45.33672951329189260, 5.299667771043163000 ) ) ;
#25857 = CARTESIAN_POINT ( 'NONE',  ( 9.730534315287435732, 294.6502823553246344, -2.323512206574427807 ) ) ;
#25859 = AXIS2_PLACEMENT_3D ( 'NONE', #32362, #81393, #15080 ) ;
#25860 = ADVANCED_FACE ( 'NONE', ( #88939 ), #96001, .T. ) ;
#25861 = ORIENTED_EDGE ( 'NONE', *, *, #101597, .T. ) ;
#25862 = ORIENTED_EDGE ( 'NONE', *, *, #41792, .T. ) ;
#25863 = VERTEX_POINT ( 'NONE', #95436 ) ;
#25864 = CARTESIAN_POINT ( 'NONE',  ( 28.39284659809811373, 318.1946778488376140, 13.22144771204134095 ) ) ;
#25865 = AXIS2_PLACEMENT_3D ( 'NONE', #72533, #54209, #5162 ) ;
#25866 = DIRECTION ( 'NONE',  ( 0.000000000000000000, 0.000000000000000000, 1.000000000000000000 ) ) ;
#25867 = CARTESIAN_POINT ( 'NONE',  ( 15.89400772911373672, 45.88919441563187718, 6.421120341668727249 ) ) ;
#25868 = VERTEX_POINT ( 'NONE', #23163 ) ;
#25869 = CARTESIAN_POINT ( 'NONE',  ( 15.54898481255689724, 46.20784644949144848, -4.780735607413824084 ) ) ;
#25870 = CARTESIAN_POINT ( 'NONE',  ( -32.66130572512955865, 465.7845731394322115, 12.51261058353286515 ) ) ;
#25871 = CARTESIAN_POINT ( 'NONE',  ( -38.25590479036647906, -57.69571505705692260, 53.01769594715635492 ) ) ;
#25872 = CARTESIAN_POINT ( 'NONE',  ( 7.188101187499999156, -28.25000000204838813, 2.977408999572654924 ) ) ;
#25873 = AXIS2_PLACEMENT_3D ( 'NONE', #81576, #74569, #67031 ) ;
#25874 = CARTESIAN_POINT ( 'NONE',  ( 20.59999999999999787, -3.309499999999999886, 0.000000000000000000 ) ) ;
#25875 = CARTESIAN_POINT ( 'NONE',  ( -35.56416567323501710, 480.2820146177156175, -4.363888856302766683 ) ) ;
#25876 = CARTESIAN_POINT ( 'NONE',  ( -6.802270553527478114, 41.53789085414797455, -58.74929071759987664 ) ) ;
#25877 = CARTESIAN_POINT ( 'NONE',  ( -76.02716361407355805, -14.21045842199433018, -24.18402117868763312 ) ) ;
#25878 = FACE_OUTER_BOUND ( 'NONE', #20994, .T. ) ;
#25879 = CARTESIAN_POINT ( 'NONE',  ( -49.80859045805021168, -29.12840406359013556, 47.03773477635749600 ) ) ;
#25880 = COLOUR_RGB ( '', 0.72549020, 0.75294118, 0.79215686) ;
#25881 = CARTESIAN_POINT ( 'NONE',  ( 21.84999999999999787, 3.309500000000003439, 0.000000000000000000 ) ) ;
#25882 = PRODUCT_DEFINITION ( 'UNKNOWN', '', #48979, #93092 ) ;
#25883 = VERTEX_POINT ( 'NONE', #53904 ) ;
#25884 = CARTESIAN_POINT ( 'NONE',  ( 35.98123173773587524, 437.4058846046290796, 4.371064750171454349 ) ) ;
#25885 = CARTESIAN_POINT ( 'NONE',  ( -9.398978598902781201, 294.6597737643588744, -3.429745804552094324 ) ) ;
#25886 = AXIS2_PLACEMENT_3D ( 'NONE', #101685, #11591, #86057 ) ;
#25887 = DIRECTION ( 'NONE',  ( 0.000000000000000000, 0.000000000000000000, 1.000000000000000000 ) ) ;
#25888 = ORIENTED_EDGE ( 'NONE', *, *, #15030, .T. ) ;
#25889 = CARTESIAN_POINT ( 'NONE',  ( 94.26467260280679739, 5.000000000000023093, 6.123233995736781074E-16 ) ) ;
#25890 = CARTESIAN_POINT ( 'NONE',  ( 95.01222379904187676, -38.48886571037592574, 201.2294609025024670 ) ) ;
#25891 = CARTESIAN_POINT ( 'NONE',  ( 49.07537269081996811, 14.00518788141342164, 14.91829442325235000 ) ) ;
#25892 = CARTESIAN_POINT ( 'NONE',  ( 27.59999999999999787, 1.411358822780289120E-15, 0.000000000000000000 ) ) ;
#25893 = DIRECTION ( 'NONE',  ( -0.2042951644570322467, 0.03948950745649387750, 0.9781125009835615058 ) ) ;
#25894 = SURFACE_STYLE_USAGE ( .BOTH. , #50106 ) ;
#25895 = CARTESIAN_POINT ( 'NONE',  ( 89.33714348230114410, -30.00000000000000355, 189.1719500048700979 ) ) ;
#25896 = FACE_OUTER_BOUND ( 'NONE', #80628, .T. ) ;
#25897 = CARTESIAN_POINT ( 'NONE',  ( -28.61418328824325030, 13.49088233573900553, 40.19504096224933676 ) ) ;
#25898 = DIRECTION ( 'NONE',  ( -1.000000000000000000, -0.000000000000000000, -0.000000000000000000 ) ) ;
#25899 = ADVANCED_FACE ( 'NONE', ( #71673 ), #54957, .F. ) ;
#25900 = EDGE_LOOP ( 'NONE', ( #67924, #82926, #68273, #37402 ) ) ;
#25901 = VERTEX_POINT ( 'NONE', #105125 ) ;
#25902 = CARTESIAN_POINT ( 'NONE',  ( 52.74007187349189962, -56.84010683540350328, 62.26390772461709844 ) ) ;
#25903 = CARTESIAN_POINT ( 'NONE',  ( -4.023896803983132209, 300.5161690456517363, -10.00978837624883155 ) ) ;
#25904 = DIRECTION ( 'NONE',  ( 0.000000000000000000, -1.000000000000000000, 0.000000000000000000 ) ) ;
#25905 = EDGE_CURVE ( 'NONE', #33663, #85296, #31266, .T. ) ;
#25906 = ORIENTED_EDGE ( 'NONE', *, *, #3473, .F. ) ;
#25907 = CARTESIAN_POINT ( 'NONE',  ( -90.66182577935869347, -38.34383351580818555, 8.928474947456855659 ) ) ;
#25908 = ORIENTED_EDGE ( 'NONE', *, *, #60818, .F. ) ;
#25909 = CARTESIAN_POINT ( 'NONE',  ( 15.05785784214676326, 3.824195276769945639, 4.604276673498420180 ) ) ;
#25910 = CARTESIAN_POINT ( 'NONE',  ( 106.9867655987633839, -38.36460303376994574, 194.8700637373434859 ) ) ;
#25911 = CARTESIAN_POINT ( 'NONE',  ( 13.42164844308434546, 22.37475377612458161, -3.539341413710700657 ) ) ;
#25912 = CARTESIAN_POINT ( 'NONE',  ( 90.29360518614763009, -60.15064404123215525, 56.70420316085070311 ) ) ;
#25913 = CARTESIAN_POINT ( 'NONE',  ( -31.43208348565051935, 438.4707862388146395, 22.17802677911202380 ) ) ;
#25914 = CARTESIAN_POINT ( 'NONE',  ( 32.75411547143891511, 465.7435926370463903, 11.50418982276139879 ) ) ;
#25915 = CARTESIAN_POINT ( 'NONE',  ( -28.76324779970338241, 309.5459823743811398, -8.926984934462732113 ) ) ;
#25916 = CARTESIAN_POINT ( 'NONE',  ( 4.671142383340135318, -65.18523764613235016, 13.09013483307534464 ) ) ;
#25917 = CARTESIAN_POINT ( 'NONE',  ( 76.40233392909763666, -60.00000000000000711, 188.5393174096115843 ) ) ;
#25918 = DIRECTION ( 'NONE',  ( -1.000000000000000000, -1.224606353822377258E-16, -0.000000000000000000 ) ) ;
#25919 = EDGE_CURVE ( 'NONE', #101089, #6033, #103006, .T. ) ;
#25920 = CARTESIAN_POINT ( 'NONE',  ( -43.86611073477271816, 435.5752409525268831, 9.535927547476964250 ) ) ;
#25921 = EDGE_LOOP ( 'NONE', ( #51729, #22818, #3768, #98338 ) ) ;
#25922 = CARTESIAN_POINT ( 'NONE',  ( 60.71647413655895065, -36.01272182586236426, 72.46326076516903925 ) ) ;
#25923 = ADVANCED_FACE ( 'NONE', ( #94930 ), #21066, .T. ) ;
#25924 = LINE ( 'NONE', #74930, #39582 ) ;
#25925 = CIRCLE ( 'NONE', #86182, 4.000000000000000888 ) ;
#25926 = LINE ( 'NONE', #31858, #86623 ) ;
#25927 = EDGE_CURVE ( 'NONE', #9982, #90846, #9822, .T. ) ;
#25928 = CARTESIAN_POINT ( 'NONE',  ( -33.10739874314164410, 427.7875163274654255, 25.07383443705004922 ) ) ;
#25929 = CARTESIAN_POINT ( 'NONE',  ( -32.86259851300427215, 485.9239370913668949, 5.440925357814620611 ) ) ;
#25930 = CARTESIAN_POINT ( 'NONE',  ( 4.898587196589412829E-16, -22.62499999999999289, -8.000000000000000000 ) ) ;
#25931 = CARTESIAN_POINT ( 'NONE',  ( -8.000000000000001776, -25.15624999999999645, 3.313708498984758943 ) ) ;
#25932 = CARTESIAN_POINT ( 'NONE',  ( -50.84467228568406227, -29.86834801596571154, 47.91031235514574149 ) ) ;
#25933 =( GEOMETRIC_REPRESENTATION_CONTEXT ( 3 ) GLOBAL_UNCERTAINTY_ASSIGNED_CONTEXT ( ( #103321 ) ) GLOBAL_UNIT_ASSIGNED_CONTEXT ( ( #47253, #97389, #95829 ) ) REPRESENTATION_CONTEXT ( 'NONE', 'WORKASPACE' ) );
#25934 = CARTESIAN_POINT ( 'NONE',  ( 15.64449080980709361, 44.06115359459996483, -4.637972761859016302 ) ) ;
#25935 = VERTEX_POINT ( 'NONE', #73257 ) ;
#25936 = CARTESIAN_POINT ( 'NONE',  ( 83.34764017132830816, -46.52104804447979092, 181.7006552018694094 ) ) ;
#25937 = DIRECTION ( 'NONE',  ( -1.000000000000000000, -1.224606353822377258E-16, -0.000000000000000000 ) ) ;
#25938 = VERTEX_POINT ( 'NONE', #6944 ) ;
#25939 = DIRECTION ( 'NONE',  ( 1.000000000000000000, 0.000000000000000000, 0.000000000000000000 ) ) ;
#25940 = AXIS2_PLACEMENT_3D ( 'NONE', #48324, #64537, #89866 ) ;
#25941 = CARTESIAN_POINT ( 'NONE',  ( 43.51047069090565600, 435.7684321374258616, 8.546621873845968054 ) ) ;
#25942 = DIRECTION ( 'NONE',  ( 0.000000000000000000, 0.000000000000000000, 1.000000000000000000 ) ) ;
#25943 = SURFACE_STYLE_FILL_AREA ( #24849 ) ;
#25944 = CARTESIAN_POINT ( 'NONE',  ( 6.544091414538025120, -3.000000000000002665, -98.56434427384034791 ) ) ;
#25945 = CARTESIAN_POINT ( 'NONE',  ( -14.11945738078545709, -23.79845479901861083, -38.53423393589877577 ) ) ;
#25946 =( NAMED_UNIT ( * ) SI_UNIT ( $, .STERADIAN. ) SOLID_ANGLE_UNIT ( ) );
#25947 = FILL_AREA_STYLE ('',( #99778 ) ) ;
#25948 = CONICAL_SURFACE ( 'NONE', #29403, 18.72828050308589454, 0.7292773806962717931 ) ;
#25949 = CARTESIAN_POINT ( 'NONE',  ( 50.87433458991679203, -60.00000000000000000, 74.01426795907130440 ) ) ;
#25950 = LINE ( 'NONE', #84137, #104746 ) ;
#25951 =( LENGTH_UNIT ( ) NAMED_UNIT ( * ) SI_UNIT ( .MILLI., .METRE. ) );
#25953 = CARTESIAN_POINT ( 'NONE',  ( -13.42196180547802875, 22.37528182222316886, -3.537684213275340550 ) ) ;
#25952 = CARTESIAN_POINT ( 'NONE',  ( -8.680069730182619736, -19.69849086824678608, 35.28136294433512887 ) ) ;
#25954 = EDGE_CURVE ( 'NONE', #16368, #16675, #14003, .T. ) ;
#25955 = CIRCLE ( 'NONE', #103435, 8.750000000000023093 ) ;
#25956 = CARTESIAN_POINT ( 'NONE',  ( 23.73746414932995208, 5.000000000000002665, 0.000000000000000000 ) ) ;
#25957 = CARTESIAN_POINT ( 'NONE',  ( 7.188101187499999156, -14.75000000204838457, 2.977408999572654924 ) ) ;
#25958 = CARTESIAN_POINT ( 'NONE',  ( 0.000000000000000000, -30.00000000000000000, 0.000000000000000000 ) ) ;
#25959 = CARTESIAN_POINT ( 'NONE',  ( 37.83989825151499531, 491.6297408768496098, 12.44743998625077630 ) ) ;
#25960 = ORIENTED_EDGE ( 'NONE', *, *, #68960, .F. ) ;
#25961 = MECHANICAL_DESIGN_GEOMETRIC_PRESENTATION_REPRESENTATION (  '', ( #91365 ), #8736 ) ;
#25962 = CARTESIAN_POINT ( 'NONE',  ( -30.81781730487858084, -29.88286713088693958, -38.15156302677360145 ) ) ;
#25963 = CARTESIAN_POINT ( 'NONE',  ( -19.50000000000047606, 49.99999999999996447, 59.82664205501238541 ) ) ;
#25964 = CARTESIAN_POINT ( 'NONE',  ( 26.11923076923076792, 1.411358822780289120E-15, 0.000000000000000000 ) ) ;
#25965 = SURFACE_STYLE_FILL_AREA ( #521 ) ;
#25967 = CARTESIAN_POINT ( 'NONE',  ( 12.60774193670373755, -34.58958930473867355, -32.31369604931713013 ) ) ;
#25966 = LINE ( 'NONE', #24869, #94899 ) ;
#25968 = ORIENTED_EDGE ( 'NONE', *, *, #28672, .T. ) ;
#25969 = LINE ( 'NONE', #1067, #1338 ) ;
#25970 = EDGE_LOOP ( 'NONE', ( #47562, #13565, #77232, #85430 ) ) ;
#25971 = AXIS2_PLACEMENT_3D ( 'NONE', #27006, #53375, #61481 ) ;
#25972 = CARTESIAN_POINT ( 'NONE',  ( 14.54015256618498775, 9.738273119607207207, -5.000000000000000000 ) ) ;
#25973 = DIRECTION ( 'NONE',  ( 0.000000000000000000, 0.000000000000000000, -1.000000000000000000 ) ) ;
#25974 = CARTESIAN_POINT ( 'NONE',  ( -33.96054341680977728, 40.58705955278919930, -60.99169518065951934 ) ) ;
#25975 = CARTESIAN_POINT ( 'NONE',  ( -97.59218698678627391, -60.00000000000000711, 66.40864316552561775 ) ) ;
#25976 = DIRECTION ( 'NONE',  ( 0.000000000000000000, 0.000000000000000000, 1.000000000000000000 ) ) ;
#25977 = CARTESIAN_POINT ( 'NONE',  ( 17.33349330513380693, 1.593028355512270962E-15, 0.000000000000000000 ) ) ;
#25978 = CARTESIAN_POINT ( 'NONE',  ( 34.06332199976886699, 330.0526646846329299, -3.810096259360388427 ) ) ;
#25979 = CARTESIAN_POINT ( 'NONE',  ( -3.857142857142847880, -48.79941684889506348, 103.1763305333244176 ) ) ;
#25981 = CARTESIAN_POINT ( 'NONE',  ( -6.991644891724774880, 41.20407541762637749, -58.47941460531158953 ) ) ;
#25980 = CARTESIAN_POINT ( 'NONE',  ( 0.000000000000000000, -3.000000000000002665, -75.00000000000001421 ) ) ;
#25982 = ADVANCED_FACE ( 'NONE', ( #17189 ), #89995, .T. ) ;
#25983 = CARTESIAN_POINT ( 'NONE',  ( -85.06961102174302880, -25.47176778552115195, 167.4802045267348092 ) ) ;
#25984 = ORIENTED_EDGE ( 'NONE', *, *, #59518, .T. ) ;
#25985 = CARTESIAN_POINT ( 'NONE',  ( 6.195804100829465533, 41.59435685053998810, -70.65487364791137281 ) ) ;
#25986 = EDGE_LOOP ( 'NONE', ( #98822, #79790, #5848, #23926 ) ) ;
#25987 = EDGE_LOOP ( 'NONE', ( #46808, #11864, #83005, #58454 ) ) ;
#25988 = CARTESIAN_POINT ( 'NONE',  ( 0.000000000000000000, 0.000000000000000000, 5.000000000000002665 ) ) ;
#25989 =( BOUNDED_SURFACE ( )  B_SPLINE_SURFACE ( 3, 2, ( 
 ( #64192, #55519, #88460 ),
 ( #14535, #47444, #982 ),
 ( #57652, #42014, #84075 ),
 ( #17236, #17759, #42543 ) ),
 .UNSPECIFIED., .F., .F., .F. ) 
 B_SPLINE_SURFACE_WITH_KNOTS ( ( 4, 4 ),
 ( 3, 3 ),
 ( 4.336808689942017736E-19, 0.001384307398009136702 ),
 ( 0.000000000000000000, 1.000000000000000000 ),
 .UNSPECIFIED. ) 
 GEOMETRIC_REPRESENTATION_ITEM ( )  RATIONAL_B_SPLINE_SURFACE ( (
 ( 1.000000000000000000, 0.7976994903569329942, 1.000000000000000000),
 ( 1.000000000000000000, 0.8073889694077948098, 1.000000000000000000),
 ( 1.000000000000000000, 0.8171087964275586257, 1.000000000000000000),
 ( 1.000000000000000000, 0.8266506655095640088, 1.000000000000000000) ) ) 
 REPRESENTATION_ITEM ( '' )  SURFACE ( )  );
#25990 = ADVANCED_FACE ( 'NONE', ( #33921 ), #32267, .T. ) ;
#25991 = ORIENTED_EDGE ( 'NONE', *, *, #66239, .T. ) ;
#25992 = AXIS2_PLACEMENT_3D ( 'NONE', #37289, #56052, #96556 ) ;
#25993 = CARTESIAN_POINT ( 'NONE',  ( -18.15175992912209324, 304.6383698585960929, 8.891572390514982160 ) ) ;
#25994 = FILL_AREA_STYLE ('',( #2176 ) ) ;
#25995 = CARTESIAN_POINT ( 'NONE',  ( -6.831979103402613163, -3.295157223185851691, -6.443785395948810724 ) ) ;
#25996 = CARTESIAN_POINT ( 'NONE',  ( -3.787333677597864323, 16.53967541042004186, 5.888147140825949144 ) ) ;
#25997 = CARTESIAN_POINT ( 'NONE',  ( 0.000000000000000000, 0.000000000000000000, -13.00000000000000000 ) ) ;
#25998 = CARTESIAN_POINT ( 'NONE',  ( 0.000000000000000000, 0.000000000000000000, 0.000000000000000000 ) ) ;
#25999 = CARTESIAN_POINT ( 'NONE',  ( -5.000000000000000888, -15.25486520280274050, 12.58693527119031330 ) ) ;
#26000 = CARTESIAN_POINT ( 'NONE',  ( 98.01458704197314376, -60.00000000000006395, 53.57113828723962001 ) ) ;
#26001 = CARTESIAN_POINT ( 'NONE',  ( -114.0746799351349665, -60.00000000000000000, 159.9915189542998633 ) ) ;
#26002 = CARTESIAN_POINT ( 'NONE',  ( -61.12306988036042554, -29.06572220310668442, 70.22504446809620049 ) ) ;
#26003 = EDGE_LOOP ( 'NONE', ( #32900, #78242, #29815, #4895, #65812 ) ) ;
#26004 =( NAMED_UNIT ( * ) PLANE_ANGLE_UNIT ( ) SI_UNIT ( $, .RADIAN. ) );
#26005 = CARTESIAN_POINT ( 'NONE',  ( 11.22784523005032042, -60.00000000003856826, -44.73795172861001390 ) ) ;
#26006 = ORIENTED_EDGE ( 'NONE', *, *, #81851, .F. ) ;
#26007 = CARTESIAN_POINT ( 'NONE',  ( 4.963618185166544627, -18.58607934322651190, 26.97811559224125944 ) ) ;
#26008 = CARTESIAN_POINT ( 'NONE',  ( -102.1368288975054384, -37.82054834480975103, 158.6782685907600410 ) ) ;
#26009 = CARTESIAN_POINT ( 'NONE',  ( 2.977408999572652260, -12.31250000204838635, 7.188101187500000044 ) ) ;
#26010 = FACE_OUTER_BOUND ( 'NONE', #65858, .T. ) ;
#26011 = FACE_OUTER_BOUND ( 'NONE', #41969, .T. ) ;
#26012 = ORIENTED_EDGE ( 'NONE', *, *, #42280, .F. ) ;
#26013 = CARTESIAN_POINT ( 'NONE',  ( -46.00000000000002132, 487.9826193845792659, -0.2183537434872499794 ) ) ;
#26014 = EDGE_CURVE ( 'NONE', #44978, #31177, #104536, .T. ) ;
#26015 = CARTESIAN_POINT ( 'NONE',  ( -68.31247128209859909, -59.99999999999997868, 132.4338893582065566 ) ) ;
#26016 = CARTESIAN_POINT ( 'NONE',  ( -3.405129524038740474, -1.148734789949058976, 104.5473292663561864 ) ) ;
#26017 = CARTESIAN_POINT ( 'NONE',  ( -7.188101187500002709, -23.18750000204838813, 2.977408999572648707 ) ) ;
#26018 = AXIS2_PLACEMENT_3D ( 'NONE', #104383, #45120, #70446 ) ;
#26019 = FACE_BOUND ( 'NONE', #25853, .T. ) ;
#26020 = ORIENTED_EDGE ( 'NONE', *, *, #17013, .T. ) ;
#26021 = DIRECTION ( 'NONE',  ( 0.000000000000000000, 1.000000000000000000, 0.000000000000000000 ) ) ;
#26022 = CARTESIAN_POINT ( 'NONE',  ( 2.220638482690572957, -0.000000000000000000, 16.90642566760537591 ) ) ;
#26023 = DIRECTION ( 'NONE',  ( 0.000000000000000000, -1.000000000000000000, 0.000000000000000000 ) ) ;
#26024 = AXIS2_PLACEMENT_3D ( 'NONE', #94740, #86653, #12723 ) ;
#26025 = CARTESIAN_POINT ( 'NONE',  ( 32.85889741710023060, 464.9534104978457094, 11.16060310718602544 ) ) ;
#26026 = CARTESIAN_POINT ( 'NONE',  ( -9.721254568807728091, 44.08029630702152701, -13.03955032007097969 ) ) ;
#26027 = DIRECTION ( 'NONE',  ( 0.9396926207859142011, 1.150791560227857419E-16, -0.3420201433256527812 ) ) ;
#26028 = CARTESIAN_POINT ( 'NONE',  ( 86.66370790318070760, -60.00000000000002842, -0.08902744567370259043 ) ) ;
#26029 = CARTESIAN_POINT ( 'NONE',  ( -31.27606781357311760, -32.54866752878100300, 32.34274477842507167 ) ) ;
#26030 = FILL_AREA_STYLE_COLOUR ( '', #49025 ) ;
#26031 = CARTESIAN_POINT ( 'NONE',  ( 43.92012437998704399, -39.52645832331002396, 42.42191456129378224 ) ) ;
#26032 = DIRECTION ( 'NONE',  ( -1.000000000000000000, -1.224606353822377258E-16, -0.000000000000000000 ) ) ;
#26033 = CIRCLE ( 'NONE', #1858, 4.981862520314373377 ) ;
#26034 = ORIENTED_EDGE ( 'NONE', *, *, #75060, .T. ) ;
#26035 = DIRECTION ( 'NONE',  ( 0.000000000000000000, 0.000000000000000000, 1.000000000000000000 ) ) ;
#26036 = CIRCLE ( 'NONE', #101746, 1.000000000000000444 ) ;
#26037 = CARTESIAN_POINT ( 'NONE',  ( -78.40755826573125375, -38.62304279762774684, 189.4248641629946803 ) ) ;
#26038 = ORIENTED_EDGE ( 'NONE', *, *, #39443, .T. ) ;
#26040 = SURFACE_STYLE_USAGE ( .BOTH. , #83155 ) ;
#26039 = DIRECTION ( 'NONE',  ( 0.000000000000000000, 0.000000000000000000, -1.000000000000000000 ) ) ;
#26041 = CARTESIAN_POINT ( 'NONE',  ( 33.22078196456656940, -59.99999999999998579, 38.21881171944680489 ) ) ;
#26042 = CARTESIAN_POINT ( 'NONE',  ( -49.02741474918240527, 7.901513937033902479, -16.35941288907603308 ) ) ;
#26043 = CARTESIAN_POINT ( 'NONE',  ( -7.398423365523743911, 41.20504426844082246, -59.67381271312094526 ) ) ;
#26044 = CARTESIAN_POINT ( 'NONE',  ( 6.231493956936422940, 4.173545622688802581, -5.000000000000000000 ) ) ;
#26045 = CARTESIAN_POINT ( 'NONE',  ( 0.05613245601036522675, 1.278525034529249149, -6.499999999999999112 ) ) ;
#26046 = CARTESIAN_POINT ( 'NONE',  ( 5.000000000000000000, -34.80405935700601816, 1.298618523705024952 ) ) ;
#26047 = CARTESIAN_POINT ( 'NONE',  ( 17.64329382111521127, 45.32481993297742662, 6.176472982800854439 ) ) ;
#26048 = CARTESIAN_POINT ( 'NONE',  ( 106.3730004120468635, -60.00000000000000000, 118.7265111617542743 ) ) ;
#26049 = CARTESIAN_POINT ( 'NONE',  ( -6.312904226987146927, -49.68714783853175732, 39.49778964097281175 ) ) ;
#26050 = EDGE_CURVE ( 'NONE', #53736, #68599, #105639, .T. ) ;
#26051 = ORIENTED_EDGE ( 'NONE', *, *, #48889, .F. ) ;
#26052 = EDGE_CURVE ( 'NONE', #64557, #72570, #82216, .T. ) ;
#26053 = CIRCLE ( 'NONE', #100054, 5.000000000000000888 ) ;
#26054 = CARTESIAN_POINT ( 'NONE',  ( -98.04222423866050917, -30.00000000000004619, 190.4877416275006397 ) ) ;
#26055 = ORIENTED_EDGE ( 'NONE', *, *, #64959, .T. ) ;
#26056 = FACE_OUTER_BOUND ( 'NONE', #76411, .T. ) ;
#26057 = CARTESIAN_POINT ( 'NONE',  ( 87.62222222222222001, -4.171999999999998820, 0.000000000000000000 ) ) ;
#26058 = CARTESIAN_POINT ( 'NONE',  ( 27.74070829223574464, 311.1873351945520199, 11.69411441391677009 ) ) ;
#26059 = CARTESIAN_POINT ( 'NONE',  ( 7.040774347399620936, 41.35742771039598153, -58.68913404742972517 ) ) ;
#26060 = CARTESIAN_POINT ( 'NONE',  ( -7.188101187500002709, -21.68750000204838813, 2.977408999572648707 ) ) ;
#26061 = CIRCLE ( 'NONE', #17399, 3.309500000000001663 ) ;
#26063 = EDGE_CURVE ( 'NONE', #42431, #15319, #42551, .T. ) ;
#26062 = DIRECTION ( 'NONE',  ( -1.000000000000000000, -1.224606353822377258E-16, -0.000000000000000000 ) ) ;
#26064 = AXIS2_PLACEMENT_3D ( 'NONE', #6336, #39278, #72156 ) ;
#26065 = DIRECTION ( 'NONE',  ( -0.000000000000000000, -1.000000000000000000, -0.000000000000000000 ) ) ;
#26066 = ORIENTED_EDGE ( 'NONE', *, *, #67922, .T. ) ;
#26067 = CARTESIAN_POINT ( 'NONE',  ( 82.60475124576561257, -36.02199222531928058, 160.6691209302269669 ) ) ;
#26068 = CARTESIAN_POINT ( 'NONE',  ( -4.284822031654962338, -1.092833614412279220, 104.4267991316945086 ) ) ;
#26069 =( LENGTH_UNIT ( ) NAMED_UNIT ( * ) SI_UNIT ( .MILLI., .METRE. ) );
#26070 = ORIENTED_EDGE ( 'NONE', *, *, #65638, .F. ) ;
#26071 = CARTESIAN_POINT ( 'NONE',  ( -53.87663890650263454, 50.00000000000000711, -33.03186720634269591 ) ) ;
#26072 = CARTESIAN_POINT ( 'NONE',  ( -0.9426293753149518340, 17.83864352553418442, -49.67541775974505924 ) ) ;
#26073 = CARTESIAN_POINT ( 'NONE',  ( -5.082755093536326818, -9.218750002048382797, 5.082755093536325042 ) ) ;
#26074 = CARTESIAN_POINT ( 'NONE',  ( -23.55598625820995196, 303.7182208366987197, 10.12520193139073577 ) ) ;
#26075 = CARTESIAN_POINT ( 'NONE',  ( 0.000000000000000000, 0.000000000000000000, 1.734723475976807094E-15 ) ) ;
#26076 = ORIENTED_EDGE ( 'NONE', *, *, #35018, .F. ) ;
#26077 = CONICAL_SURFACE ( 'NONE', #74197, 3.309500000000001663, 0.9599310885968770357 ) ;
#26078 =( LENGTH_UNIT ( ) NAMED_UNIT ( * ) SI_UNIT ( .MILLI., .METRE. ) );
#26079 = CARTESIAN_POINT ( 'NONE',  ( -6.500000000000000000, -3.155218591052693977, -0.5622968210053880256 ) ) ;
#26080 = CARTESIAN_POINT ( 'NONE',  ( 87.15839251447800962, -53.73024192609155847, 193.0048309959825872 ) ) ;
#26081 = CARTESIAN_POINT ( 'NONE',  ( -1.250000000000000888, 7.938566201357359020, -7.198902722707429369 ) ) ;
#26082 = ADVANCED_FACE ( 'NONE', ( #81883 ), #56549, .T. ) ;
#26083 = CARTESIAN_POINT ( 'NONE',  ( 5.082755093536324154, -31.34375000204838457, 5.082755093536326818 ) ) ;
#26084 = FACE_BOUND ( 'NONE', #92941, .T. ) ;
#26085 = DIRECTION ( 'NONE',  ( -0.000000000000000000, -1.000000000000000000, -0.000000000000000000 ) ) ;
#26086 = EDGE_CURVE ( 'NONE', #88866, #3905, #59826, .T. ) ;
#26087 = CARTESIAN_POINT ( 'NONE',  ( -7.922281120364393914, -4.573931137438282057, -8.047472243342934206 ) ) ;
#26088 = ITEM_DEFINED_TRANSFORMATION ( 'NONE', 'NONE', #69652,  #10728 ) ;
#26089 = ORIENTED_EDGE ( 'NONE', *, *, #426, .F. ) ;
#26090 =( GEOMETRIC_REPRESENTATION_CONTEXT ( 3 ) GLOBAL_UNCERTAINTY_ASSIGNED_CONTEXT ( ( #13487 ) ) GLOBAL_UNIT_ASSIGNED_CONTEXT ( ( #1886, #84954, #2956 ) ) REPRESENTATION_CONTEXT ( 'NONE', 'WORKASPACE' ) );
#26091 = AXIS2_PLACEMENT_3D ( 'NONE', #65803, #84112, #34536 ) ;
#26092 = CARTESIAN_POINT ( 'NONE',  ( 0.08434562425236380445, 44.08548369317411897, 16.25000000000002842 ) ) ;
#26093 = AXIS2_PLACEMENT_3D ( 'NONE', #70970, #105459, #96328 ) ;
#26094 = CARTESIAN_POINT ( 'NONE',  ( -9.999565592957996074, 7.500620397551100993, 0.000000000000000000 ) ) ;
#26095 = EDGE_CURVE ( 'NONE', #54801, #61302, #52875, .T. ) ;
#26096 = CARTESIAN_POINT ( 'NONE',  ( -18.99999999999999645, 4.000000000000000000, -2.500000000000000000 ) ) ;
#26097 = ORIENTED_EDGE ( 'NONE', *, *, #50408, .T. ) ;
#26098 =( GEOMETRIC_REPRESENTATION_CONTEXT ( 3 ) GLOBAL_UNCERTAINTY_ASSIGNED_CONTEXT ( ( #10047 ) ) GLOBAL_UNIT_ASSIGNED_CONTEXT ( ( #87876, #22637, #62540 ) ) REPRESENTATION_CONTEXT ( 'NONE', 'WORKASPACE' ) );
#26099 = DIRECTION ( 'NONE',  ( 0.000000000000000000, 0.000000000000000000, 1.000000000000000000 ) ) ;
#26100 = CARTESIAN_POINT ( 'NONE',  ( -42.79891897445037330, 462.9518546950670270, 4.196605471987052027 ) ) ;
#26101 = CARTESIAN_POINT ( 'NONE',  ( 111.7135535141261187, -57.67100837368887767, 192.2061815498727526 ) ) ;
#26102 = TOROIDAL_SURFACE ( 'NONE', #67413, 64.50000000000000000, 0.5000000000000000000 ) ;
#26104 = CARTESIAN_POINT ( 'NONE',  ( 33.00000000000000000, 435.0774731480752280, 11.67986145722081304 ) ) ;
#26103 = AXIS2_PLACEMENT_3D ( 'NONE', #8500, #26865, #43541 ) ;
#26105 = CARTESIAN_POINT ( 'NONE',  ( -9.647409248820050465, 51.27677058736198745, -3.402434490781860443 ) ) ;
#26106 = CARTESIAN_POINT ( 'NONE',  ( 0.000000000000000000, 0.000000000000000000, -25.03750572909317285 ) ) ;
#26107 = CARTESIAN_POINT ( 'NONE',  ( 16.64348903516496492, 43.47556584774762456, -6.657797401562562278 ) ) ;
#26108 = CARTESIAN_POINT ( 'NONE',  ( -76.72214885510777549, -60.00000000000001421, 189.6187291083674040 ) ) ;
#26109 = DIRECTION ( 'NONE',  ( -1.000000000000000000, 0.000000000000000000, 0.000000000000000000 ) ) ;
#26110 = FACE_OUTER_BOUND ( 'NONE', #67934, .T. ) ;
#26111 = CARTESIAN_POINT ( 'NONE',  ( 7.592810154713590230E-15, 48.00000000000000000, -62.00000000000000000 ) ) ;
#26112 = B_SPLINE_CURVE_WITH_KNOTS ( 'NONE', 3,
 ( #83008, #19393, #42540, #52225, #36103, #68973 ),
 .UNSPECIFIED., .F., .F.,
 ( 4, 2, 4 ),
 ( -5.145455527293658110E-06, 0.0004153350442917327912, 0.0008358155441107592218 ),
 .UNSPECIFIED. ) ;
#26113 = CARTESIAN_POINT ( 'NONE',  ( -84.13144306823785712, -50.17137820680997606, 187.2782904672004634 ) ) ;
#26114 = VERTEX_POINT ( 'NONE', #32318 ) ;
#26115 = DIRECTION ( 'NONE',  ( 0.000000000000000000, 0.000000000000000000, 1.000000000000000000 ) ) ;
#26116 = EDGE_LOOP ( 'NONE', ( #31281, #73149, #51684, #31159 ) ) ;
#26117 = CARTESIAN_POINT ( 'NONE',  ( -6.943482370013978944, -10.52848370260726085, 3.973876482044364611 ) ) ;
#26118 = ADVANCED_FACE ( 'NONE', ( #24234 ), #60837, .F. ) ;
#26119 = CARTESIAN_POINT ( 'NONE',  ( 1.000000000000000000, -56.57158839599533451, 6.200363299250661875 ) ) ;
#26120 = CARTESIAN_POINT ( 'NONE',  ( -87.03651754438010357, -60.20087593430655204, -7.185994694023575491 ) ) ;
#26121 = MECHANICAL_DESIGN_GEOMETRIC_PRESENTATION_REPRESENTATION (  '', ( #96680 ), #15751 ) ;
#26122 = CARTESIAN_POINT ( 'NONE',  ( -6.547363650393914547, -12.76646305665534342, -7.895817423510182564 ) ) ;
#26123 = CARTESIAN_POINT ( 'NONE',  ( -4.201140726046737939, 12.27787011423575692, -5.000000000000000000 ) ) ;
#26124 = CONICAL_SURFACE ( 'NONE', #86395, 3.309500000000007880, 0.9599310885968770357 ) ;
#26125 = DIRECTION ( 'NONE',  ( 0.000000000000000000, 1.000000000000000000, 0.000000000000000000 ) ) ;
#26126 = CARTESIAN_POINT ( 'NONE',  ( 27.72723468844076322, 36.41215165560291922, -9.903269780309406300 ) ) ;
#26127 = ADVANCED_FACE ( 'NONE', ( #11183 ), #21954, .T. ) ;
#26128 = CARTESIAN_POINT ( 'NONE',  ( -22.57731121199999080, 28.20557510165627235, 30.87924556879399063 ) ) ;
#26129 = CARTESIAN_POINT ( 'NONE',  ( 49.67137106584178241, -60.00000000000004263, 77.31490210218785819 ) ) ;
#26130 = CARTESIAN_POINT ( 'NONE',  ( -35.05271644150329280, 437.8393516193276582, 4.418594605291610300 ) ) ;
#26131 = CARTESIAN_POINT ( 'NONE',  ( -67.59740049799954420, -60.00000000000004263, -35.88590100950167994 ) ) ;
#26132 = CARTESIAN_POINT ( 'NONE',  ( -69.72170801787599714, -56.86188030024484874, 111.2991454040818695 ) ) ;
#26133 = ORIENTED_EDGE ( 'NONE', *, *, #100184, .T. ) ;
#26134 = CARTESIAN_POINT ( 'NONE',  ( 77.72372478688149045, -60.00000000000015632, 197.5639835283903381 ) ) ;
#26135 = CARTESIAN_POINT ( 'NONE',  ( 110.0995903249117589, -57.67119305192648682, 129.6557836479702246 ) ) ;
#26136 = ORIENTED_EDGE ( 'NONE', *, *, #82201, .F. ) ;
#26137 = CARTESIAN_POINT ( 'NONE',  ( 15.68577251487070612, -4.397129302180654342, 14.34458040922159583 ) ) ;
#26138 = DIRECTION ( 'NONE',  ( -1.000000000000000000, -1.224606353822377258E-16, -0.000000000000000000 ) ) ;
#26139 = ORIENTED_EDGE ( 'NONE', *, *, #63229, .T. ) ;
#26140 = LINE ( 'NONE', #33143, #63089 ) ;
#26141 = CARTESIAN_POINT ( 'NONE',  ( 47.78396355473342538, 15.50490861890768635, -16.83695313132077231 ) ) ;
#26142 = DIRECTION ( 'NONE',  ( 0.000000000000000000, 0.000000000000000000, -1.000000000000000000 ) ) ;
#26143 = CARTESIAN_POINT ( 'NONE',  ( 7.188101187500000044, -14.65625000204838457, 0.000000000000000000 ) ) ;
#26144 = CARTESIAN_POINT ( 'NONE',  ( -3.313708498984760276, -18.21875000409676915, -8.000000000000000000 ) ) ;
#26145 = CARTESIAN_POINT ( 'NONE',  ( 22.67073868809948323, -4.285714285714295357, -11.17734400176825815 ) ) ;
#26146 = LINE ( 'NONE', #39242, #30516 ) ;
#26147 = LINE ( 'NONE', #1799, #36566 ) ;
#26148 = CARTESIAN_POINT ( 'NONE',  ( 0.000000000000000000, 0.000000000000000000, 0.000000000000000000 ) ) ;
#26149 =( NAMED_UNIT ( * ) SI_UNIT ( $, .STERADIAN. ) SOLID_ANGLE_UNIT ( ) );
#26150 = UNCERTAINTY_MEASURE_WITH_UNIT (LENGTH_MEASURE( 1.000000000000000082E-05 ), #82847, 'distance_accuracy_value', 'NONE');
#26151 = VERTEX_POINT ( 'NONE', #52185 ) ;
#26152 = CARTESIAN_POINT ( 'NONE',  ( -6.809786362084849998, 41.36669071755328986, -70.61902766660038822 ) ) ;
#26154 = CARTESIAN_POINT ( 'NONE',  ( 33.42066694708537256, -49.89779052485263122, 36.47770383487736012 ) ) ;
#26153 = CARTESIAN_POINT ( 'NONE',  ( -3.396360046677566746, -49.15315706213335289, 103.9790200242205032 ) ) ;
#26155 = CARTESIAN_POINT ( 'NONE',  ( 31.84958088623538686, 317.5633087689430454, -5.928141683191124223 ) ) ;
#26156 = ORIENTED_EDGE ( 'NONE', *, *, #50265, .T. ) ;
#26157 = CARTESIAN_POINT ( 'NONE',  ( -1.116779127739723210, 14.48579825753870765, 51.07894496868025414 ) ) ;
#26158 = ORIENTED_EDGE ( 'NONE', *, *, #46849, .F. ) ;
#26160 = FILL_AREA_STYLE_COLOUR ( '', #33733 ) ;
#26159 = CARTESIAN_POINT ( 'NONE',  ( 0.08285530294364830406, 1.570896314703518870, 8.000000000000000000 ) ) ;
#26161 = DIRECTION ( 'NONE',  ( 1.000000000000000000, -0.000000000000000000, -0.000000000000000000 ) ) ;
#26162 = DIRECTION ( 'NONE',  ( 0.000000000000000000, 0.000000000000000000, 1.000000000000000000 ) ) ;
#26163 = CARTESIAN_POINT ( 'NONE',  ( 0.3346317158865195207, 46.19713137549851467, 16.29267624532406344 ) ) ;
#26164 = CARTESIAN_POINT ( 'NONE',  ( 0.9532286629884955120, 13.93731468125776374, -51.31239236590303676 ) ) ;
#26165 = ORIENTED_EDGE ( 'NONE', *, *, #48532, .T. ) ;
#26166 = CARTESIAN_POINT ( 'NONE',  ( 92.55080760481821756, -59.99999999999997868, -10.81156607774824607 ) ) ;
#26167 = CARTESIAN_POINT ( 'NONE',  ( 32.95589646111110937, 464.8957215206408478, 10.75300444715717951 ) ) ;
#26169 = CARTESIAN_POINT ( 'NONE',  ( 29.99999999999995381, 464.1568293259584834, 11.21040210117823399 ) ) ;
#26168 = CONICAL_SURFACE ( 'NONE', #84636, 4.000000000000001776, 0.9599310885968808105 ) ;
#26170 = AXIS2_PLACEMENT_3D ( 'NONE', #56635, #33458, #73886 ) ;
#26171 = DIRECTION ( 'NONE',  ( 0.000000000000000000, -1.000000000000000000, 0.000000000000000000 ) ) ;
#26172 = EDGE_LOOP ( 'NONE', ( #39564, #71684, #92179, #19403 ) ) ;
#26173 = ADVANCED_FACE ( 'NONE', ( #60317 ), #6359, .T. ) ;
#26174 = CARTESIAN_POINT ( 'NONE',  ( 65.03872891708842019, -1.232595164407830946E-29, 4.000000000000007105 ) ) ;
#26175 = ORIENTED_EDGE ( 'NONE', *, *, #85732, .T. ) ;
#26176 = EDGE_LOOP ( 'NONE', ( #8053, #26807, #93005, #77891 ) ) ;
#26177 = CARTESIAN_POINT ( 'NONE',  ( 3.313708498984761608, -10.71874999999999289, -8.000000000000000000 ) ) ;
#26178 = CARTESIAN_POINT ( 'NONE',  ( 6.692588830498431562, -7.935834885954435869, 0.04058884017440032160 ) ) ;
#26179 = CARTESIAN_POINT ( 'NONE',  ( -15.54267344201861434, 34.77189900418887447, -23.41194221326999525 ) ) ;
#26180 = DIRECTION ( 'NONE',  ( -1.000000000000000000, 0.000000000000000000, 0.000000000000000000 ) ) ;
#26181 = CARTESIAN_POINT ( 'NONE',  ( 85.00363781311220635, -60.19116803139766603, -16.05942585105188058 ) ) ;
#26182 = CARTESIAN_POINT ( 'NONE',  ( -35.91510745124932669, 303.8491723658412411, 0.06940248214010066863 ) ) ;
#26183 = DIRECTION ( 'NONE',  ( 0.000000000000000000, -1.000000000000000000, 0.000000000000000000 ) ) ;
#26185 = EDGE_CURVE ( 'NONE', #21601, #75683, #54625, .T. ) ;
#26184 = SURFACE_STYLE_USAGE ( .BOTH. , #24047 ) ;
#26186 = VERTEX_POINT ( 'NONE', #93193 ) ;
#26187 = CARTESIAN_POINT ( 'NONE',  ( -6.499999999999999112, 1.416734669067071017, -5.722373386996367550 ) ) ;
#26188 = CIRCLE ( 'NONE', #86441, 5.000000000000002665 ) ;
#26189 = VERTEX_POINT ( 'NONE', #59775 ) ;
#26190 = DIRECTION ( 'NONE',  ( 0.000000000000000000, -1.000000000000000000, 0.000000000000000000 ) ) ;
#26191 = CARTESIAN_POINT ( 'NONE',  ( 3.567967761885403544, -49.07022467159661971, 103.4762329555118612 ) ) ;
#26193 = VERTEX_POINT ( 'NONE', #92116 ) ;
#26192 = CARTESIAN_POINT ( 'NONE',  ( 18.58349330513380693, 4.898587196589411843E-16, -4.000000000000001776 ) ) ;
#26194 = CARTESIAN_POINT ( 'NONE',  ( 71.71719020375222442, -29.06458548707639622, 101.3022678019235343 ) ) ;
#26195 = EDGE_LOOP ( 'NONE', ( #50583, #102655, #53196, #51507, #88858 ) ) ;
#26196 = CARTESIAN_POINT ( 'NONE',  ( 0.000000000000000000, 0.000000000000000000, 4.000000000000000000 ) ) ;
#26197 = CARTESIAN_POINT ( 'NONE',  ( 4.401442555609581635E-16, -24.78125000204838813, -7.188101187500000044 ) ) ;
#26198 = CARTESIAN_POINT ( 'NONE',  ( -113.3548229410037465, -57.67117998536030399, 185.4730977758015911 ) ) ;
#26199 = EDGE_CURVE ( 'NONE', #70423, #63451, #1498, .T. ) ;
#26200 = ORIENTED_EDGE ( 'NONE', *, *, #99487, .F. ) ;
#26201 = CIRCLE ( 'NONE', #50243, 2.000000000000000000 ) ;
#26202 = DIRECTION ( 'NONE',  ( -1.000000000000000000, 0.000000000000000000, 0.000000000000000000 ) ) ;
#26203 = CARTESIAN_POINT ( 'NONE',  ( 102.7192639426134662, -37.84832478631605568, 177.0129730847589258 ) ) ;
#26204 = CARTESIAN_POINT ( 'NONE',  ( -36.37766630548127722, 28.20754914235178390, -11.81157041065297975 ) ) ;
#26205 = AXIS2_PLACEMENT_3D ( 'NONE', #100597, #9445, #1889 ) ;
#26206 = CARTESIAN_POINT ( 'NONE',  ( 30.00000000000000000, 450.0000000000002274, 13.20242257375370976 ) ) ;
#26207 = ADVANCED_FACE ( 'NONE', ( #18810 ), #30063, .T. ) ;
#26208 = CARTESIAN_POINT ( 'NONE',  ( -3.313708498984760720, -21.21875000409676915, -8.000000000000000000 ) ) ;
#26209 = DIRECTION ( 'NONE',  ( 1.000000000000000000, 0.000000000000000000, 0.000000000000000000 ) ) ;
#26210 = DIRECTION ( 'NONE',  ( 0.000000000000000000, -1.000000000000000000, 0.000000000000000000 ) ) ;
#26211 = CARTESIAN_POINT ( 'NONE',  ( 70.41111111111112564, 6.915964383211875250E-15, 0.000000000000000000 ) ) ;
#26212 = DIRECTION ( 'NONE',  ( -1.000000000000000000, -0.000000000000000000, -0.000000000000000000 ) ) ;
#26213 = CARTESIAN_POINT ( 'NONE',  ( -1.469576158976823947E-15, -20.37499999999999289, 8.000000000000000000 ) ) ;
#26214 = DIRECTION ( 'NONE',  ( 0.000000000000000000, -0.4497171033863425760, -0.8931710513232039572 ) ) ;
#26215 = CARTESIAN_POINT ( 'NONE',  ( -3.836411046842014727, 15.00000000000001066, -9.999999999999959144 ) ) ;
#26216 = VERTEX_POINT ( 'NONE', #21451 ) ;
#26217 = SURFACE_SIDE_STYLE ('',( #99507 ) ) ;
#26218 =( NAMED_UNIT ( * ) SI_UNIT ( $, .STERADIAN. ) SOLID_ANGLE_UNIT ( ) );
#26219 = CARTESIAN_POINT ( 'NONE',  ( 0.000000000000000000, 0.000000000000000000, 35.82893434829263413 ) ) ;
#26220 = CARTESIAN_POINT ( 'NONE',  ( -87.76554063038440745, -29.99999999999999645, 186.1736720200109971 ) ) ;
#26221 = EDGE_CURVE ( 'NONE', #56846, #51415, #38177, .T. ) ;
#26222 = ORIENTED_EDGE ( 'NONE', *, *, #54776, .F. ) ;
#26223 = LINE ( 'NONE', #74176, #11714 ) ;
#26224 = CARTESIAN_POINT ( 'NONE',  ( 71.71515109230394103, -57.67815897944166181, 169.1494729058397581 ) ) ;
#26226 = CARTESIAN_POINT ( 'NONE',  ( -8.559508646656370345, 53.96349637827587031, 1.531152949374564365 ) ) ;
#26225 =( LENGTH_UNIT ( ) NAMED_UNIT ( * ) SI_UNIT ( .MILLI., .METRE. ) );
#26227 = CARTESIAN_POINT ( 'NONE',  ( 46.76197682092300312, -34.80551308950123968, -36.64518833549670518 ) ) ;
#26228 = CARTESIAN_POINT ( 'NONE',  ( 5.416666666666666963, -4.378239541354686182, -5.848636054922042860 ) ) ;
#26229 = DIRECTION ( 'NONE',  ( 0.000000000000000000, -1.000000000000000000, 0.000000000000000000 ) ) ;
#26230 = CARTESIAN_POINT ( 'NONE',  ( -33.53236062124648953, -60.00000000000000711, 45.21991715472178441 ) ) ;
#26231 = CARTESIAN_POINT ( 'NONE',  ( -32.15310320217076878, 439.7024266304582625, 23.94087012106557211 ) ) ;
#26232 = CARTESIAN_POINT ( 'NONE',  ( 37.22806219797154625, 463.3233819687148980, 20.09366234602714840 ) ) ;
#26233 = CARTESIAN_POINT ( 'NONE',  ( -84.25800729984597126, -61.06716200360207125, 192.6535660339058040 ) ) ;
#26234 = AXIS2_PLACEMENT_3D ( 'NONE', #91302, #25531, #43792 ) ;
#26235 = ORIENTED_EDGE ( 'NONE', *, *, #49341, .F. ) ;
#26236 = CARTESIAN_POINT ( 'NONE',  ( 30.71756172601006085, 13.08262462249239100, 41.56006324341294800 ) ) ;
#26237 = CARTESIAN_POINT ( 'NONE',  ( -8.282562182867314604, -53.40262204257363976, 32.78376551419927409 ) ) ;
#26238 = CARTESIAN_POINT ( 'NONE',  ( 0.000000000000000000, 0.000000000000000000, 0.000000000000000000 ) ) ;
#26239 = VECTOR ( 'NONE', #10357, 1000.000000000000000 ) ;
#26240 = CARTESIAN_POINT ( 'NONE',  ( -41.57853049034962112, 486.1006523484328454, 12.35204812598594160 ) ) ;
#26242 = CARTESIAN_POINT ( 'NONE',  ( 3.096124615231415245, -69.43176308602586744, 13.34236499254138408 ) ) ;
#26241 = CARTESIAN_POINT ( 'NONE',  ( -36.66795030846187586, 306.3035926564865008, 4.617914666504396415 ) ) ;
#26243 = EDGE_CURVE ( 'NONE', #35975, #86295, #78064, .T. ) ;
#26244 = ORIENTED_EDGE ( 'NONE', *, *, #7689, .F. ) ;
#26245 = CARTESIAN_POINT ( 'NONE',  ( -7.149690282015371601, -5.000000000000036415, -15.41216073230092753 ) ) ;
#26246 = CARTESIAN_POINT ( 'NONE',  ( -29.85247340496026780, 12.86254483752416711, -39.61457847635377050 ) ) ;
#26247 = CARTESIAN_POINT ( 'NONE',  ( 33.41308119780744335, 300.5641305218781554, -0.7154550005598049323 ) ) ;
#26248 = CYLINDRICAL_SURFACE ( 'NONE', #89828, 4.000000000000001776 ) ;
#26249 = EDGE_CURVE ( 'NONE', #48477, #54135, #25346, .T. ) ;
#26250 = CIRCLE ( 'NONE', #39985, 2.000000000000000000 ) ;
#26251 = FILL_AREA_STYLE_COLOUR ( '', #68516 ) ;
#26252 = CARTESIAN_POINT ( 'NONE',  ( 46.00000000000000000, 500.0000000000002274, 0.000000000000000000 ) ) ;
#26253 = CARTESIAN_POINT ( 'NONE',  ( 109.4365241820779460, -29.99999999999997158, 178.4894931318444264 ) ) ;
#26254 = CARTESIAN_POINT ( 'NONE',  ( -81.37979335976676509, -32.56286079620799967, 146.9012815414374415 ) ) ;
#26255 = EDGE_LOOP ( 'NONE', ( #19404, #5386, #69988 ) ) ;
#26256 = CARTESIAN_POINT ( 'NONE',  ( 102.0666666666666629, -4.171999999999998820, 0.000000000000000000 ) ) ;
#26257 = CARTESIAN_POINT ( 'NONE',  ( -9.999952458099501840, 253.9998811452386462, 0.2653554233229243331 ) ) ;
#26258 = CARTESIAN_POINT ( 'NONE',  ( -8.000000000000001776, -20.84375000409677270, 3.313708498984759387 ) ) ;
#26259 = CARTESIAN_POINT ( 'NONE',  ( -15.99999999999999645, 2.437231117875781727, -5.694551215225702734 ) ) ;
#26260 = CARTESIAN_POINT ( 'NONE',  ( 37.61995183727506031, 438.1738172413044481, 4.432413526166450346 ) ) ;
#26261 = DIRECTION ( 'NONE',  ( -1.000000000000000000, -1.224606353822377258E-16, -0.000000000000000000 ) ) ;
#26262 = VERTEX_POINT ( 'NONE', #105000 ) ;
#26263 = EDGE_CURVE ( 'NONE', #81794, #99203, #85617, .T. ) ;
#26264 = CARTESIAN_POINT ( 'NONE',  ( -20.39914337211097006, 304.8937497850257614, 9.945937256050433106 ) ) ;
#26265 = ORIENTED_EDGE ( 'NONE', *, *, #73138, .F. ) ;
#26266 = CARTESIAN_POINT ( 'NONE',  ( 32.94021323899734455, 485.0599191339525191, 5.361609822540892800 ) ) ;
#26267 = DIRECTION ( 'NONE',  ( 0.000000000000000000, 0.000000000000000000, 1.000000000000000000 ) ) ;
#26268 = CARTESIAN_POINT ( 'NONE',  ( 32.10528697966010014, 486.1671898930082421, 5.449875171705066634 ) ) ;
#26269 = CARTESIAN_POINT ( 'NONE',  ( -5.363597346089342466, 41.33266196706077267, -58.39526881795508473 ) ) ;
#26270 = CARTESIAN_POINT ( 'NONE',  ( 5.962730926219388827, -13.90752838006108227, 13.89020537730394622 ) ) ;
#26271 = CARTESIAN_POINT ( 'NONE',  ( 44.31720021651388919, 435.2315751315647958, 12.07978424043336929 ) ) ;
#26272 = ORIENTED_EDGE ( 'NONE', *, *, #93262, .T. ) ;
#26273 = CARTESIAN_POINT ( 'NONE',  ( 112.0843263065733453, -59.99999999999998579, 166.2625348020058311 ) ) ;
#26274 = AXIS2_PLACEMENT_3D ( 'NONE', #75041, #71, #97727 ) ;
#26276 = CARTESIAN_POINT ( 'NONE',  ( 25.24426991834572576, -49.91242165019021826, 33.57203989678414757 ) ) ;
#26275 = CARTESIAN_POINT ( 'NONE',  ( -91.59718878904411099, -29.99999999999996803, 199.7679234505767738 ) ) ;
#26278 = CARTESIAN_POINT ( 'NONE',  ( 1.714505518806292863E-15, 61.50000000000000000, -6.999999999999992895 ) ) ;
#26277 = PRODUCT_DEFINITION_CONTEXT ( 'detailed design', #83806, 'design' ) ;
#26279 = DIRECTION ( 'NONE',  ( 0.000000000000000000, 0.000000000000000000, 1.000000000000000000 ) ) ;
#26280 = CARTESIAN_POINT ( 'NONE',  ( -42.37195134635844340, -46.43793568724321119, 42.48696600435207671 ) ) ;
#26281 =( GEOMETRIC_REPRESENTATION_CONTEXT ( 3 ) GLOBAL_UNCERTAINTY_ASSIGNED_CONTEXT ( ( #56931 ) ) GLOBAL_UNIT_ASSIGNED_CONTEXT ( ( #49252, #47663, #16362 ) ) REPRESENTATION_CONTEXT ( 'NONE', 'WORKASPACE' ) );
#26282 = CARTESIAN_POINT ( 'NONE',  ( -9.182549847561064738, 53.50073754291216943, -3.877052053296246914 ) ) ;
#26283 = UNCERTAINTY_MEASURE_WITH_UNIT (LENGTH_MEASURE( 1.000000000000000082E-05 ), #61897, 'distance_accuracy_value', 'NONE');
#26284 = VERTEX_POINT ( 'NONE', #94261 ) ;
#26285 = CARTESIAN_POINT ( 'NONE',  ( 0.000000000000000000, 0.000000000000000000, 0.000000000000000000 ) ) ;
#26286 = CARTESIAN_POINT ( 'NONE',  ( 10.00000000000000000, 15.00000000000000000, 10.00000000000000000 ) ) ;
#26287 = CARTESIAN_POINT ( 'NONE',  ( 40.77380256327629837, 468.8478597483947965, 21.13608272249925690 ) ) ;
#26288 = CIRCLE ( 'NONE', #53791, 9.999999999999998224 ) ;
#26289 = DIRECTION ( 'NONE',  ( 0.000000000000000000, 0.000000000000000000, 1.000000000000000000 ) ) ;
#26290 = LINE ( 'NONE', #89910, #34476 ) ;
#26291 = DIRECTION ( 'NONE',  ( 0.000000000000000000, 0.000000000000000000, -1.000000000000000000 ) ) ;
#26292 = ORIENTED_EDGE ( 'NONE', *, *, #89928, .T. ) ;
#26293 = CARTESIAN_POINT ( 'NONE',  ( -47.61850715973584869, -38.32480789866512083, 63.16917730038245082 ) ) ;
#26294 = VERTEX_POINT ( 'NONE', #20424 ) ;
#26295 = CARTESIAN_POINT ( 'NONE',  ( 76.05159319993262557, -29.99999999993064037, 166.0196408361732381 ) ) ;
#26296 = CARTESIAN_POINT ( 'NONE',  ( 19.42585305423203224, 41.87255863741783912, -80.48841060219729115 ) ) ;
#26297 = DIRECTION ( 'NONE',  ( -1.000000000000000000, -1.224606353822377258E-16, -0.000000000000000000 ) ) ;
#26298 = FACE_OUTER_BOUND ( 'NONE', #37129, .T. ) ;
#26299 = CARTESIAN_POINT ( 'NONE',  ( 80.81161881489168763, -30.00000000000000355, 8.164499038400824915 ) ) ;
#26300 =( BOUNDED_SURFACE ( )  B_SPLINE_SURFACE ( 3, 2, ( 
 ( #65041, #41296, #55854 ),
 ( #89331, #82281, #65577 ),
 ( #14351, #6260, #97939 ),
 ( #22505, #90383, #15961 ) ),
 .UNSPECIFIED., .F., .F., .F. ) 
 B_SPLINE_SURFACE_WITH_KNOTS ( ( 4, 4 ),
 ( 3, 3 ),
 ( 0.01611645847898578870, 0.01831749139115683780 ),
 ( 0.000000000000000000, 0.8386188628085423646 ),
 .UNSPECIFIED. ) 
 GEOMETRIC_REPRESENTATION_ITEM ( )  RATIONAL_B_SPLINE_SURFACE ( (
 ( 1.000000000000000000, 0.7543742219143267924, 0.9207212652179949108),
 ( 1.000000000000000000, 0.7738259253571172502, 0.9269995412618118324),
 ( 1.000000000000000000, 0.7927721361627113605, 0.9331146633523637046),
 ( 1.000000000000000000, 0.8105494169260334392, 0.9388524989238771212) ) ) 
 REPRESENTATION_ITEM ( '' )  SURFACE ( )  );
#26301 =( LENGTH_UNIT ( ) NAMED_UNIT ( * ) SI_UNIT ( .MILLI., .METRE. ) );
#26302 = EDGE_LOOP ( 'NONE', ( #92538, #73179, #29945, #11326 ) ) ;
#26303 = ADVANCED_FACE ( 'NONE', ( #78585 ), #39118, .T. ) ;
#26304 = VERTEX_POINT ( 'NONE', #37116 ) ;
#26305 = ORIENTED_EDGE ( 'NONE', *, *, #9063, .F. ) ;
#26306 = CARTESIAN_POINT ( 'NONE',  ( -47.90305809253368352, 10.05329658600980380, -16.85535821593460781 ) ) ;
#26307 =( LENGTH_UNIT ( ) NAMED_UNIT ( * ) SI_UNIT ( .MILLI., .METRE. ) );
#26308 = DIRECTION ( 'NONE',  ( 0.000000000000000000, -1.000000000000000000, 0.000000000000000000 ) ) ;
#26309 = CARTESIAN_POINT ( 'NONE',  ( 5.999787407977320797, -13.99968111184449171, 0.2740427891042958031 ) ) ;
#26310 = EDGE_CURVE ( 'NONE', #37464, #5588, #1178, .T. ) ;
#26311 = CARTESIAN_POINT ( 'NONE',  ( -32.19533475021953706, 392.4752074454114563, 25.42422936412204493 ) ) ;
#26313 = ADVANCED_FACE ( 'NONE', ( #87230 ), #13312, .F. ) ;
#26312 =( NAMED_UNIT ( * ) PLANE_ANGLE_UNIT ( ) SI_UNIT ( $, .RADIAN. ) );
#26314 = ORIENTED_EDGE ( 'NONE', *, *, #2319, .F. ) ;
#26315 = CARTESIAN_POINT ( 'NONE',  ( -1.308996937483428491, 49.99999999999999289, -95.00000000000001421 ) ) ;
#26316 = ORIENTED_EDGE ( 'NONE', *, *, #65872, .F. ) ;
#26317 = FILL_AREA_STYLE_COLOUR ( '', #65661 ) ;
#26318 = CARTESIAN_POINT ( 'NONE',  ( 71.34172708741220958, -38.32795092330694331, 142.0021045512803539 ) ) ;
#26319 = CARTESIAN_POINT ( 'NONE',  ( 6.162888688655344005, -3.752776749732561257, 6.500000000000000000 ) ) ;
#26320 = CARTESIAN_POINT ( 'NONE',  ( 26.96170002121218801, 306.9387515484356186, 10.87917313509033335 ) ) ;
#26321 = EDGE_CURVE ( 'NONE', #87331, #28004, #11317, .T. ) ;
#26322 = CARTESIAN_POINT ( 'NONE',  ( -5.192560085536403136, 247.3569455736875682, 3.013051918867572176 ) ) ;
#26323 = CONICAL_SURFACE ( 'NONE', #86579, 5.000000000000000000, 0.9599310885968913576 ) ;
#26324 = ORIENTED_EDGE ( 'NONE', *, *, #42428, .T. ) ;
#26325 = CARTESIAN_POINT ( 'NONE',  ( 11.28351131189991641, -9.073918974790325720, -12.46553453015538793 ) ) ;
#26326 = CARTESIAN_POINT ( 'NONE',  ( 24.30812977188561419, 295.4061218410959100, 2.054700292315147170 ) ) ;
#26327 = DIRECTION ( 'NONE',  ( 0.000000000000000000, -0.5000000000000009992, -0.8660254037844380415 ) ) ;
#26328 = ADVANCED_FACE ( 'NONE', ( #49396, #65063 ), #41846, .F. ) ;
#26329 = CARTESIAN_POINT ( 'NONE',  ( 14.83949740352631252, 1.410031051010677716, -2.190466161075831142 ) ) ;
#26330 = VERTEX_POINT ( 'NONE', #56419 ) ;
#26332 = CARTESIAN_POINT ( 'NONE',  ( -24.62889686368193765, 295.5521682776166585, 2.087298195416544377 ) ) ;
#26331 =( NAMED_UNIT ( * ) PLANE_ANGLE_UNIT ( ) SI_UNIT ( $, .RADIAN. ) );
#26333 = FACE_OUTER_BOUND ( 'NONE', #45742, .T. ) ;
#26334 = CARTESIAN_POINT ( 'NONE',  ( 0.000000000000000000, 0.000000000000000000, -7.259124522925831435 ) ) ;
#26335 = CARTESIAN_POINT ( 'NONE',  ( -32.83703342409244641, 465.7129651006319477, 11.08653443108803138 ) ) ;
#26336 = AXIS2_PLACEMENT_3D ( 'NONE', #45375, #78256, #100405 ) ;
#26337 = ADVANCED_FACE ( 'NONE', ( #48334 ), #3070, .T. ) ;
#26338 = CARTESIAN_POINT ( 'NONE',  ( -6.928203230275509661, 104.7311667549100491, -4.000000000000001776 ) ) ;
#26339 = ORIENTED_EDGE ( 'NONE', *, *, #102337, .F. ) ;
#26340 = FACE_OUTER_BOUND ( 'NONE', #94558, .T. ) ;
#26341 = CARTESIAN_POINT ( 'NONE',  ( 86.12920843257361980, -28.31461485542720879, 182.7851167764210913 ) ) ;
#26342 = SURFACE_STYLE_FILL_AREA ( #92080 ) ;
#26343 = CARTESIAN_POINT ( 'NONE',  ( -8.002549191641280757, 102.8991202088222252, 2.540710531356172437E-12 ) ) ;
#26344 = VERTEX_POINT ( 'NONE', #34861 ) ;
#26345 = CARTESIAN_POINT ( 'NONE',  ( 91.71403545851765671, -57.66150985471095680, -19.81184364356237637 ) ) ;
#26346 = DIRECTION ( 'NONE',  ( 0.000000000000000000, 1.000000000000000000, 0.000000000000000000 ) ) ;
#26347 = DIRECTION ( 'NONE',  ( -1.000000000000000000, -1.224606353822377258E-16, -0.000000000000000000 ) ) ;
#26348 = DIRECTION ( 'NONE',  ( -1.000000000000000000, -0.000000000000000000, -0.000000000000000000 ) ) ;
#26349 = STYLED_ITEM ( 'NONE', ( #99095 ), #96183 ) ;
#26350 = CARTESIAN_POINT ( 'NONE',  ( -97.22778952995973611, -30.00000000000000355, 132.2006373510576509 ) ) ;
#26351 = PRESENTATION_LAYER_ASSIGNMENT (  '', '', ( #53857 ) ) ;
#26352 = AXIS2_PLACEMENT_3D ( 'NONE', #41256, #74143, #98941 ) ;
#26353 = CARTESIAN_POINT ( 'NONE',  ( -8.000000000000000000, -29.96764154942184888, -1.065389812439802020 ) ) ;
#26354 = CARTESIAN_POINT ( 'NONE',  ( 0.000000000000000000, -50.00000000000000000, 112.0000000000000000 ) ) ;
#26356 = DIRECTION ( 'NONE',  ( -1.000000000000000000, -0.000000000000000000, -0.000000000000000000 ) ) ;
#26355 = CARTESIAN_POINT ( 'NONE',  ( -9.843039827103263306, 246.4091649749165924, -1.781495459429543793 ) ) ;
#26357 = FACE_OUTER_BOUND ( 'NONE', #15133, .T. ) ;
#26358 = LINE ( 'NONE', #34442, #56638 ) ;
#26359 = CARTESIAN_POINT ( 'NONE',  ( 5.382057749264594904, -82.00173201596055605, -2.659775980967107767 ) ) ;
#26360 = CARTESIAN_POINT ( 'NONE',  ( 43.10000000000000142, -3.309499999999999886, 4.475777889183790779E-16 ) ) ;
#26361 = CARTESIAN_POINT ( 'NONE',  ( 0.000000000000000000, 4.898587196589413815E-16, -4.000000000000000888 ) ) ;
#26362 = AXIS2_PLACEMENT_3D ( 'NONE', #38493, #21787, #71354 ) ;
#26363 = CARTESIAN_POINT ( 'NONE',  ( 12.43157790776222704, -16.68004855619690119, -34.60072825135022612 ) ) ;
#26364 = CARTESIAN_POINT ( 'NONE',  ( -25.70623218437548374, -29.04638407032486924, 30.12123181827645979 ) ) ;
#26365 = ORIENTED_EDGE ( 'NONE', *, *, #27257, .T. ) ;
#26366 = CARTESIAN_POINT ( 'NONE',  ( 6.239948093758000525, 10.55525250974069174, 3.176436098724912505 ) ) ;
#26367 = CARTESIAN_POINT ( 'NONE',  ( 1.793818517922412203, 21.43745688976599695, 6.770759481125232071 ) ) ;
#26368 = CARTESIAN_POINT ( 'NONE',  ( -60.87314043734040325, -29.35674091808159147, -24.66679337420148244 ) ) ;
#26370 = CARTESIAN_POINT ( 'NONE',  ( 28.17977184163764193, 1.482358050883964840E-15, 0.000000000000000000 ) ) ;
#26369 = CARTESIAN_POINT ( 'NONE',  ( 72.11682663846713126, 6.975173280561618775E-15, 0.000000000000000000 ) ) ;
#26371 = EDGE_CURVE ( 'NONE', #71961, #44907, #97748, .T. ) ;
#26372 = ORIENTED_EDGE ( 'NONE', *, *, #103652, .F. ) ;
#26373 = DIRECTION ( 'NONE',  ( 0.000000000000000000, 1.000000000000000000, 0.000000000000000000 ) ) ;
#26374 = ORIENTED_EDGE ( 'NONE', *, *, #99001, .F. ) ;
#26375 = FACE_OUTER_BOUND ( 'NONE', #31516, .T. ) ;
#26376 = ADVANCED_FACE ( 'NONE', ( #67208 ), #56387, .T. ) ;
#26377 = EDGE_CURVE ( 'NONE', #44516, #13812, #35828, .T. ) ;
#26378 = DIRECTION ( 'NONE',  ( 0.000000000000000000, -1.000000000000000000, 0.000000000000000000 ) ) ;
#26379 = CARTESIAN_POINT ( 'NONE',  ( -81.74325047390442478, -60.00000000000000711, -26.86817790202253065 ) ) ;
#26380 = VERTEX_POINT ( 'NONE', #10540 ) ;
#26381 = CARTESIAN_POINT ( 'NONE',  ( -7.895830884676383832, 294.7033644922051963, -6.143025603150206848 ) ) ;
#26382 = CARTESIAN_POINT ( 'NONE',  ( 100.5709118951127152, -52.75385023292707842, 193.7746871183922792 ) ) ;
#26383 = AXIS2_PLACEMENT_3D ( 'NONE', #98115, #24264, #31806 ) ;
#26385 = CARTESIAN_POINT ( 'NONE',  ( -3.991107381396968634, -1.050392363564321307, 104.5611067885113386 ) ) ;
#26384 = CARTESIAN_POINT ( 'NONE',  ( 3.887627447353766641, 294.8076638163112762, -9.231226148363823825 ) ) ;
#26386 = VERTEX_POINT ( 'NONE', #19757 ) ;
#26387 = EDGE_CURVE ( 'NONE', #57728, #9383, #6427, .T. ) ;
#26388 = ORIENTED_EDGE ( 'NONE', *, *, #9741, .T. ) ;
#26389 = ORIENTED_EDGE ( 'NONE', *, *, #71650, .F. ) ;
#26390 = CARTESIAN_POINT ( 'NONE',  ( 31.59989307617499321, 345.3384981963453129, 19.62160995718464207 ) ) ;
#26391 = DIRECTION ( 'NONE',  ( 0.000000000000000000, -1.000000000000000000, 0.000000000000000000 ) ) ;
#26392 = CARTESIAN_POINT ( 'NONE',  ( 15.55855383130857383, 46.20420475984591491, 4.781350493801785007 ) ) ;
#26393 = ORIENTED_EDGE ( 'NONE', *, *, #94216, .F. ) ;
#26394 = CARTESIAN_POINT ( 'NONE',  ( 0.05613245601076726626, 1.278525034532176141, -6.499999999999999112 ) ) ;
#26395 = CARTESIAN_POINT ( 'NONE',  ( 6.562934840145639548, 4.277581483015136854, 6.282640795011892543 ) ) ;
#26396 = CARTESIAN_POINT ( 'NONE',  ( 0.4964154566687637438, -4.996589667937443302, -7.345652830558661250 ) ) ;
#26397 = CARTESIAN_POINT ( 'NONE',  ( -73.03813016181682372, -57.65004463643786892, 181.4998991682408302 ) ) ;
#26398 = CARTESIAN_POINT ( 'NONE',  ( -43.99225961071505253, 464.6045839418125638, 10.45666854317281036 ) ) ;
#26399 = CARTESIAN_POINT ( 'NONE',  ( 0.000000000000000000, 56.87938524157181774, 0.000000000000000000 ) ) ;
#26400 = CARTESIAN_POINT ( 'NONE',  ( 38.81358894280276672, 485.1131561813238591, -4.191378885298274959 ) ) ;
#26401 = VECTOR ( 'NONE', #27222, 1000.000000000000227 ) ;
#26402 = CARTESIAN_POINT ( 'NONE',  ( -90.15663891815873399, -29.99999999999996447, 30.33658191415442573 ) ) ;
#26403 = DIRECTION ( 'NONE',  ( 0.000000000000000000, -1.000000000000000000, 0.000000000000000000 ) ) ;
#26404 = CARTESIAN_POINT ( 'NONE',  ( -51.23517434054790698, -42.97794402298157479, 54.10049340080158231 ) ) ;
#26405 = CARTESIAN_POINT ( 'NONE',  ( 105.5353273971932140, 1.030564683017419500E-14, 0.000000000000000000 ) ) ;
#26406 = ORIENTED_EDGE ( 'NONE', *, *, #104489, .T. ) ;
#26407 = CYLINDRICAL_SURFACE ( 'NONE', #18505, 4.000000000000000000 ) ;
#26408 = CARTESIAN_POINT ( 'NONE',  ( -14.29190075645216851, 12.99999999999999289, 10.00000000000000178 ) ) ;
#26409 = CARTESIAN_POINT ( 'NONE',  ( 10.79499483409554550, -1.039388583189924775, 20.32137925714343751 ) ) ;
#26410 = ORIENTED_EDGE ( 'NONE', *, *, #72078, .T. ) ;
#26411 = CARTESIAN_POINT ( 'NONE',  ( 6.000208918519489565, 245.9996866221002279, -0.2646532170642357795 ) ) ;
#26412 = CARTESIAN_POINT ( 'NONE',  ( 76.52617406485063611, -38.41457857166980006, 181.9190546311624814 ) ) ;
#26413 = CARTESIAN_POINT ( 'NONE',  ( 32.88333705524082973, 439.7317646416722141, 24.13381181826093069 ) ) ;
#26414 = CARTESIAN_POINT ( 'NONE',  ( -5.930615719913575390, 51.27008138075110111, -8.357849859401051518 ) ) ;
#26415 = FACE_OUTER_BOUND ( 'NONE', #10705, .T. ) ;
#26416 = CARTESIAN_POINT ( 'NONE',  ( -11.85444436786843525, 42.00000000000000000, -90.56128410203886858 ) ) ;
#26417 = CARTESIAN_POINT ( 'NONE',  ( 93.74430992741119439, -30.00000000000001066, 191.2477460422086892 ) ) ;
#26418 = CONICAL_SURFACE ( 'NONE', #84965, 3.309500000000001663, 0.9599310885968770357 ) ;
#26419 = CARTESIAN_POINT ( 'NONE',  ( -11.36440988823891018, 43.57563821449488017, -13.50564546251721509 ) ) ;
#26420 = SURFACE_STYLE_FILL_AREA ( #45107 ) ;
#26421 = CARTESIAN_POINT ( 'NONE',  ( -32.93513049338658760, 465.6726574193328361, 10.66039033145138326 ) ) ;
#26422 = ADVANCED_FACE ( 'NONE', ( #51532 ), #54699, .T. ) ;
#26423 = ORIENTED_EDGE ( 'NONE', *, *, #62642, .T. ) ;
#26424 = EDGE_LOOP ( 'NONE', ( #92241, #83269, #21277, #62668, #55551, #58225, #103599, #89473, #88990, #40187 ) ) ;
#26425 = CARTESIAN_POINT ( 'NONE',  ( 51.21436344590323131, -22.18943343881225871, 46.87532722179359013 ) ) ;
#26426 = CARTESIAN_POINT ( 'NONE',  ( -46.00000000000000000, 437.9690125970932399, 14.09127711025738883 ) ) ;
#26427 = CARTESIAN_POINT ( 'NONE',  ( 58.92761780597729881, -4.000000000000000000, 0.000000000000000000 ) ) ;
#26428 = ADVANCED_FACE ( 'NONE', ( #101154 ), #16859, .T. ) ;
#26429 = ORIENTED_EDGE ( 'NONE', *, *, #21027, .F. ) ;
#26430 = CARTESIAN_POINT ( 'NONE',  ( -87.92473828310710360, -38.36961232417662160, -19.67705683220690105 ) ) ;
#26431 = ORIENTED_EDGE ( 'NONE', *, *, #49212, .F. ) ;
#26432 = FILL_AREA_STYLE ('',( #74388 ) ) ;
#26433 = CARTESIAN_POINT ( 'NONE',  ( 110.2521165255493969, -38.35601262087017460, 184.3169374418023665 ) ) ;
#26434 = CARTESIAN_POINT ( 'NONE',  ( 13.43131796715543125, 24.48388052888637745, 2.370280691517476779 ) ) ;
#26435 = CARTESIAN_POINT ( 'NONE',  ( 90.66858095960151331, -52.71678089307656023, 67.18335908107627574 ) ) ;
#26436 = CARTESIAN_POINT ( 'NONE',  ( 35.45036406932566564, 436.3203772529585649, 5.179456583034234285 ) ) ;
#26437 = CARTESIAN_POINT ( 'NONE',  ( -23.41949505512490504, 304.4436526223547048, -9.872909214488972296 ) ) ;
#26438 = DIRECTION ( 'NONE',  ( -1.000000000000000000, -1.224606353822377258E-16, -0.000000000000000000 ) ) ;
#26439 = DIRECTION ( 'NONE',  ( 0.000000000000000000, 0.000000000000000000, -1.000000000000000000 ) ) ;
#26440 = CYLINDRICAL_SURFACE ( 'NONE', #66423, 4.000000000000000000 ) ;
#26441 = ORIENTED_EDGE ( 'NONE', *, *, #66882, .T. ) ;
#26442 = CARTESIAN_POINT ( 'NONE',  ( 60.76565412937480204, -22.11966791577999913, 66.05797801596867203 ) ) ;
#26443 = CARTESIAN_POINT ( 'NONE',  ( 0.6418249586330869727, 37.14405262803889940, 27.42421770560467209 ) ) ;
#26444 = DIRECTION ( 'NONE',  ( 1.000000000000000000, 1.224606353822377258E-16, 0.000000000000000000 ) ) ;
#26445 = EDGE_LOOP ( 'NONE', ( #5907, #88414, #14815, #11005 ) ) ;
#26446 = CARTESIAN_POINT ( 'NONE',  ( -33.88237199998296489, 485.0486819176492759, 1.241522336454282227 ) ) ;
#26447 = CARTESIAN_POINT ( 'NONE',  ( -42.19277509307554652, 346.1477229841391363, 13.95430603839016648 ) ) ;
#26448 = CARTESIAN_POINT ( 'NONE',  ( -38.81968145246697333, 25.17318795309900281, -12.34933546114397984 ) ) ;
#26449 = DIRECTION ( 'NONE',  ( -1.000000000000000000, -1.224606353822377258E-16, -0.000000000000000000 ) ) ;
#26450 = CARTESIAN_POINT ( 'NONE',  ( -3.313708498984765161, -29.46874999999999645, 7.999999999999998224 ) ) ;
#26451 = CARTESIAN_POINT ( 'NONE',  ( -43.60180431260018707, -27.81332246800423036, 38.60050550264399050 ) ) ;
#26452 = EDGE_CURVE ( 'NONE', #38217, #104028, #32343, .T. ) ;
#26453 = CARTESIAN_POINT ( 'NONE',  ( 16.02298420952691771, 43.96085526717300951, -4.310639523075502133 ) ) ;
#26454 = AXIS2_PLACEMENT_3D ( 'NONE', #61489, #19997, #85765 ) ;
#26455 = EDGE_LOOP ( 'NONE', ( #35125, #38183, #72142, #74344 ) ) ;
#26456 = CARTESIAN_POINT ( 'NONE',  ( 84.74406210802428063, -35.85138381605241875, 179.5088509989636805 ) ) ;
#26457 = EDGE_CURVE ( 'NONE', #25084, #105946, #13361, .T. ) ;
#26458 = CARTESIAN_POINT ( 'NONE',  ( -39.28083343692465945, 437.8791283697678409, 22.93287928653034058 ) ) ;
#26459 = ORIENTED_EDGE ( 'NONE', *, *, #82052, .T. ) ;
#26460 = VECTOR ( 'NONE', #60968, 1000.000000000000000 ) ;
#26461 = CARTESIAN_POINT ( 'NONE',  ( 14.11595029532510104, 2.410436752314617959, -5.024000119269091513 ) ) ;
#26462 = DIRECTION ( 'NONE',  ( -1.000000000000000000, -1.224606353822377258E-16, -0.000000000000000000 ) ) ;
#26463 = CARTESIAN_POINT ( 'NONE',  ( 32.20627895475151092, 464.6794106235104209, 10.68705400064636812 ) ) ;
#26464 = CARTESIAN_POINT ( 'NONE',  ( -23.31310657521862240, -27.07274008780074936, -38.41778960086845984 ) ) ;
#26465 = CARTESIAN_POINT ( 'NONE',  ( -9.480263010783763988, -0.4492663453375149163, 19.86871132324680289 ) ) ;
#26466 = SURFACE_STYLE_FILL_AREA ( #25947 ) ;
#26467 = CARTESIAN_POINT ( 'NONE',  ( 47.51011502736643166, -59.99999999999999289, 65.91768184338560843 ) ) ;
#26468 = MECHANICAL_DESIGN_GEOMETRIC_PRESENTATION_REPRESENTATION (  '', ( #79771 ), #93578 ) ;
#26469 = CARTESIAN_POINT ( 'NONE',  ( 7.150931910075644105, 106.7862579852226332, -3.588457848165351738 ) ) ;
#26470 = CARTESIAN_POINT ( 'NONE',  ( 19.24333786597378193, -16.79214355476590015, 31.49079971865065986 ) ) ;
#26472 = CARTESIAN_POINT ( 'NONE',  ( -14.52296734940917311, 21.59519996265376562, -5.118403002213263164 ) ) ;
#26471 = CARTESIAN_POINT ( 'NONE',  ( -39.40204838967584777, -37.44295604146311263, 49.05621705154725021 ) ) ;
#26473 = CARTESIAN_POINT ( 'NONE',  ( -9.948513602187995630, 88.86977943343859465, 1.045942665286138107 ) ) ;
#26474 = CARTESIAN_POINT ( 'NONE',  ( -1.320432766682874540E-15, -10.53125000204838457, 7.188101187500000044 ) ) ;
#26475 = CARTESIAN_POINT ( 'NONE',  ( 22.08400538955477899, 294.9973745800270990, -1.969057594002644906 ) ) ;
#26476 = CARTESIAN_POINT ( 'NONE',  ( -7.264118654998711122, 4.945491722146218017, -7.907633014911222169 ) ) ;
#26477 = ORIENTED_EDGE ( 'NONE', *, *, #38374, .F. ) ;
#26478 = CARTESIAN_POINT ( 'NONE',  ( -13.63130828375568981, 294.5445729804733901, -10.06530370901874072 ) ) ;
#26479 = CARTESIAN_POINT ( 'NONE',  ( -17.49999999999721823, 50.01864923522455086, 61.58301093894252176 ) ) ;
#26480 =( GEOMETRIC_REPRESENTATION_CONTEXT ( 3 ) GLOBAL_UNCERTAINTY_ASSIGNED_CONTEXT ( ( #8461 ) ) GLOBAL_UNIT_ASSIGNED_CONTEXT ( ( #21937, #86146, #69937 ) ) REPRESENTATION_CONTEXT ( 'NONE', 'WORKASPACE' ) );
#26481 = CARTESIAN_POINT ( 'NONE',  ( 0.4973051450695264442, -3.866309095700703136, 8.000000000000000000 ) ) ;
#26482 = DIRECTION ( 'NONE',  ( 0.000000000000000000, -1.000000000000000000, 0.000000000000000000 ) ) ;
#26483 = CIRCLE ( 'NONE', #31630, 4.000000000000001776 ) ;
#26485 = CARTESIAN_POINT ( 'NONE',  ( 25.58909025738432774, -47.40908607597074820, -33.48593688835422455 ) ) ;
#26484 = CARTESIAN_POINT ( 'NONE',  ( 4.885277709441186111, 53.57062629529884390, 8.466573372809225617 ) ) ;
#26486 = EDGE_CURVE ( 'NONE', #12685, #79036, #77413, .T. ) ;
#26487 = PRESENTATION_LAYER_ASSIGNMENT (  '', '', ( #62657 ) ) ;
#26488 = VERTEX_POINT ( 'NONE', #50986 ) ;
#26489 = VECTOR ( 'NONE', #15412, 1000.000000000000000 ) ;
#26490 = CARTESIAN_POINT ( 'NONE',  ( 28.28105526222837085, 36.39302830438535352, 8.375257444619659708 ) ) ;
#26491 = FACE_OUTER_BOUND ( 'NONE', #55277, .T. ) ;
#26492 = CIRCLE ( 'NONE', #84811, 5.000000000000002665 ) ;
#26493 = ORIENTED_EDGE ( 'NONE', *, *, #61984, .F. ) ;
#26494 = EDGE_CURVE ( 'NONE', #17325, #31918, #66745, .T. ) ;
#26495 = CARTESIAN_POINT ( 'NONE',  ( 14.85284876471456350, 5.000000000000002665, 0.000000000000000000 ) ) ;
#26496 = ADVANCED_FACE ( 'NONE', ( #66661 ), #41056, .T. ) ;
#26497 = CARTESIAN_POINT ( 'NONE',  ( 30.64348173561366195, 7.829960647508035443, -41.65811975367154218 ) ) ;
#26498 = DIRECTION ( 'NONE',  ( 0.000000000000000000, 1.000000000000000000, -0.000000000000000000 ) ) ;
#26499 = CARTESIAN_POINT ( 'NONE',  ( -105.4858918486370385, -60.00000000000000711, 113.2841891985042366 ) ) ;
#26500 = DIRECTION ( 'NONE',  ( -1.000000000000000000, -1.224606353822377258E-16, -0.000000000000000000 ) ) ;
#26501 = CARTESIAN_POINT ( 'NONE',  ( 7.264118654998712010, -4.945491722146226898, -7.907633014911222169 ) ) ;
#26502 = CARTESIAN_POINT ( 'NONE',  ( 31.14694070047868735, 432.3293837220155069, 24.29762062537629319 ) ) ;
#26503 = CARTESIAN_POINT ( 'NONE',  ( 39.32386068305349625, 460.7288320239697441, 2.118193558184886083 ) ) ;
#26505 = CARTESIAN_POINT ( 'NONE',  ( 5.749654562269868196E-15, 24.35682532067546902, 46.94949242731048145 ) ) ;
#26504 = CARTESIAN_POINT ( 'NONE',  ( 6.145467200820246667, -3.000000000000002665, -92.99666842291070168 ) ) ;
#26506 = CARTESIAN_POINT ( 'NONE',  ( -82.51321957585668088, -46.47945556470999406, 176.1511104553312350 ) ) ;
#26507 = ORIENTED_EDGE ( 'NONE', *, *, #58122, .F. ) ;
#26508 = CARTESIAN_POINT ( 'NONE',  ( 6.701893401236465486, 41.44328394225253476, -70.59544911815949320 ) ) ;
#26509 = EDGE_CURVE ( 'NONE', #45637, #84193, #16933, .T. ) ;
#26510 = ORIENTED_EDGE ( 'NONE', *, *, #5663, .F. ) ;
#26511 = VERTEX_POINT ( 'NONE', #6159 ) ;
#26512 = CARTESIAN_POINT ( 'NONE',  ( 43.88846153846154152, 1.411358822780289120E-15, 0.000000000000000000 ) ) ;
#26513 = DIRECTION ( 'NONE',  ( -0.000000000000000000, -1.000000000000000000, -0.000000000000000000 ) ) ;
#26514 = ORIENTED_EDGE ( 'NONE', *, *, #1587, .T. ) ;
#26515 = CIRCLE ( 'NONE', #47174, 4.000000000000007105 ) ;
#26516 = CARTESIAN_POINT ( 'NONE',  ( -19.02089907821467918, 303.6992913295931658, 9.904582106010233034 ) ) ;
#26517 = DIRECTION ( 'NONE',  ( 0.000000000000000000, 1.000000000000000000, 0.000000000000000000 ) ) ;
#26518 = DIRECTION ( 'NONE',  ( 0.000000000000000000, 0.000000000000000000, 1.000000000000000000 ) ) ;
#26519 = CARTESIAN_POINT ( 'NONE',  ( -6.928203230275506108, -64.73116675491002070, -4.000000000000001776 ) ) ;
#26520 = CARTESIAN_POINT ( 'NONE',  ( 9.491091496279695579E-16, 54.30758622938872549, 7.749999999999999112 ) ) ;
#26521 = DIRECTION ( 'NONE',  ( -1.000000000000000000, -1.224606353822377258E-16, -0.000000000000000000 ) ) ;
#26522 = CARTESIAN_POINT ( 'NONE',  ( 16.33361799548379523, 3.851859888774471706E-31, 5.000000000000001776 ) ) ;
#26523 = CARTESIAN_POINT ( 'NONE',  ( 86.74683449613482367, -14.21045842199431242, 20.02856677177719646 ) ) ;
#26524 = CARTESIAN_POINT ( 'NONE',  ( -101.1248876217780719, -29.99999999999996803, 198.7487848662925387 ) ) ;
#26525 = CARTESIAN_POINT ( 'NONE',  ( -57.05921168992595227, -46.44064480593611677, 67.94562297101694526 ) ) ;
#26526 = ORIENTED_EDGE ( 'NONE', *, *, #38528, .T. ) ;
#26527 = CARTESIAN_POINT ( 'NONE',  ( 6.086031112480590366, 15.01982037264469838, 3.462237351910362193 ) ) ;
#26528 = CARTESIAN_POINT ( 'NONE',  ( 39.12642507647372270, -59.99999999997108802, -42.14755403963000191 ) ) ;
#26529 = VERTEX_POINT ( 'NONE', #105402 ) ;
#26530 = CARTESIAN_POINT ( 'NONE',  ( 6.121031749467999106, -42.95355877999562466, 31.03873517957318739 ) ) ;
#26531 = CARTESIAN_POINT ( 'NONE',  ( -105.2354536759059869, -52.71042663006205231, 175.0634013992600160 ) ) ;
#26532 = FILL_AREA_STYLE ('',( #68559 ) ) ;
#26533 =( NAMED_UNIT ( * ) PLANE_ANGLE_UNIT ( ) SI_UNIT ( $, .RADIAN. ) );
#26534 = CARTESIAN_POINT ( 'NONE',  ( 4.021832409241297590, -29.99999999999998224, 5.962323058997216485 ) ) ;
#26535 = VERTEX_POINT ( 'NONE', #104879 ) ;
#26536 = TOROIDAL_SURFACE ( 'NONE', #98767, 11.00000000000000533, 4.000000000000000000 ) ;
#26537 = CARTESIAN_POINT ( 'NONE',  ( -59.79892528436459997, -60.00000000000002842, 99.75862326221643173 ) ) ;
#26538 = CARTESIAN_POINT ( 'NONE',  ( -3.707709148203271354, -1.099523832062968998, 104.5934084724869564 ) ) ;
#26539 = CARTESIAN_POINT ( 'NONE',  ( 7.188101187499999156, -21.12500000204838813, 2.977408999572654924 ) ) ;
#26540 = CARTESIAN_POINT ( 'NONE',  ( -1.250441718889297782, 36.68885173498831165, -28.65503145627670989 ) ) ;
#26541 = LINE ( 'NONE', #49703, #27174 ) ;
#26542 = CIRCLE ( 'NONE', #67618, 10.00000000000000178 ) ;
#26543 = CARTESIAN_POINT ( 'NONE',  ( -0.5402994271758849720, 21.82491192351207587, -6.984019969325498955 ) ) ;
#26544 = CARTESIAN_POINT ( 'NONE',  ( -11.57838703060089358, -4.921403515191947520, -12.56403927680040589 ) ) ;
#26545 = DIRECTION ( 'NONE',  ( 0.000000000000000000, 1.000000000000000000, 0.000000000000000000 ) ) ;
#26546 = CARTESIAN_POINT ( 'NONE',  ( 8.659875471883962561, -13.99571786196214340, 15.99679319869066418 ) ) ;
#26547 = CARTESIAN_POINT ( 'NONE',  ( -7.500000000016720847, 43.33959969848450555, -60.00534814812790785 ) ) ;
#26548 = UNCERTAINTY_MEASURE_WITH_UNIT (LENGTH_MEASURE( 1.000000000000000082E-05 ), #51975, 'distance_accuracy_value', 'NONE');
#26549 = CARTESIAN_POINT ( 'NONE',  ( -30.91330409187026262, -49.90965397396043102, 35.32750583910272013 ) ) ;
#26550 = CARTESIAN_POINT ( 'NONE',  ( 98.59800593614012598, 1.016364837396684119E-14, 0.000000000000000000 ) ) ;
#26551 = B_SPLINE_CURVE_WITH_KNOTS ( 'NONE', 3,
 ( #81399, #73308, #15615, #90041, #56599, #31827 ),
 .UNSPECIFIED., .F., .F.,
 ( 4, 2, 4 ),
 ( 0.003981881017442843659, 0.005970145066490154147, 0.007958409115537464634 ),
 .UNSPECIFIED. ) ;
#26552 = CARTESIAN_POINT ( 'NONE',  ( 42.51421430475448915, -22.24489720477335908, 36.74246443512219429 ) ) ;
#26553 = CARTESIAN_POINT ( 'NONE',  ( 7.999999999999998224, -14.09374999999999112, 3.313708498984766049 ) ) ;
#26554 = ORIENTED_EDGE ( 'NONE', *, *, #18071, .T. ) ;
#26555 = CARTESIAN_POINT ( 'NONE',  ( -43.03265099499957813, 484.2747968070553384, -0.8099405866661226749 ) ) ;
#26556 = EDGE_CURVE ( 'NONE', #92815, #104203, #56401, .T. ) ;
#26557 = CARTESIAN_POINT ( 'NONE',  ( -77.93035626155285911, -38.56579719186625255, 187.9925447483828123 ) ) ;
#26558 = ORIENTED_EDGE ( 'NONE', *, *, #4748, .F. ) ;
#26559 = CARTESIAN_POINT ( 'NONE',  ( 0.000000000000000000, 4.898587196589412829E-16, -4.000000000000000000 ) ) ;
#26560 = CARTESIAN_POINT ( 'NONE',  ( 39.55075348946911618, -60.00000000000002132, 42.69056844256114402 ) ) ;
#26561 = DIRECTION ( 'NONE',  ( -1.000000000000000000, -1.224606353822377258E-16, -0.000000000000000000 ) ) ;
#26562 = CARTESIAN_POINT ( 'NONE',  ( -6.828042834505470893, 41.63841151066672808, -58.95291702778771281 ) ) ;
#26563 = CARTESIAN_POINT ( 'NONE',  ( 4.678819457397437986, 8.078722181090837395, -5.000000000000000000 ) ) ;
#26564 = CARTESIAN_POINT ( 'NONE',  ( 0.2595206531158502639, 2.531175536751796962, -6.499999999999999112 ) ) ;
#26565 = CARTESIAN_POINT ( 'NONE',  ( 11.36650669486618881, 1.474610560812782335E-15, 0.000000000000000000 ) ) ;
#26566 = DIRECTION ( 'NONE',  ( -1.000000000000000000, -0.000000000000000000, -0.000000000000000000 ) ) ;
#26567 = B_SPLINE_CURVE_WITH_KNOTS ( 'NONE', 3,
 ( #25729, #19769, #83911, #42385, #77423, #100624 ),
 .UNSPECIFIED., .F., .F.,
 ( 4, 2, 4 ),
 ( 0.000000000000000000, 0.001995463903526791850, 0.003990927807053583701 ),
 .UNSPECIFIED. ) ;
#26568 = CARTESIAN_POINT ( 'NONE',  ( 109.1439378327955723, -60.00000000000000711, 136.9933165474393491 ) ) ;
#26569 = CARTESIAN_POINT ( 'NONE',  ( -1.997303689625640200E-15, 5.309483803148800973, 3.803704290982250491 ) ) ;
#26570 = CIRCLE ( 'NONE', #38549, 0.5000000000000004441 ) ;
#26571 = AXIS2_PLACEMENT_3D ( 'NONE', #63023, #39287, #63564 ) ;
#26572 = CARTESIAN_POINT ( 'NONE',  ( -45.71963733757689852, -30.00000000000002842, 56.30991746768105344 ) ) ;
#26573 = EDGE_CURVE ( 'NONE', #96657, #68930, #104604, .T. ) ;
#26574 = ORIENTED_EDGE ( 'NONE', *, *, #45255, .T. ) ;
#26575 = CARTESIAN_POINT ( 'NONE',  ( 2.519529083135078729, -49.57861714554732657, 103.1541576364171817 ) ) ;
#26576 = COLOUR_RGB ( '', 0.31764706, 0.68627451, 0.89019608) ;
#26577 = COLOUR_RGB ( '', 0.66274510, 0.83137255, 0.94901961) ;
#26578 = CARTESIAN_POINT ( 'NONE',  ( -81.51781765243289612, -30.00000000000003908, -9.022581224190874494 ) ) ;
#26579 = VERTEX_POINT ( 'NONE', #75677 ) ;
#26580 = CARTESIAN_POINT ( 'NONE',  ( 26.11201203623409484, 37.18374287936713785, -8.043240354485387655 ) ) ;
#26581 = FACE_OUTER_BOUND ( 'NONE', #69273, .T. ) ;
#26582 = DIRECTION ( 'NONE',  ( 0.000000000000000000, -1.000000000000000000, 0.000000000000000000 ) ) ;
#26583 = FACE_OUTER_BOUND ( 'NONE', #35118, .T. ) ;
#26584 = CARTESIAN_POINT ( 'NONE',  ( 5.082755093536325930, -17.84375000204838457, -5.082755093536325042 ) ) ;
#26585 =( LENGTH_UNIT ( ) NAMED_UNIT ( * ) SI_UNIT ( .MILLI., .METRE. ) );
#26586 = DIRECTION ( 'NONE',  ( -1.000000000000000000, -1.224606353822377258E-16, -0.000000000000000000 ) ) ;
#26587 = EDGE_CURVE ( 'NONE', #98662, #42319, #58107, .T. ) ;
#26589 = ORIENTED_EDGE ( 'NONE', *, *, #103541, .F. ) ;
#26588 = DIRECTION ( 'NONE',  ( 0.000000000000000000, 1.000000000000000000, 0.000000000000000000 ) ) ;
#26590 = CARTESIAN_POINT ( 'NONE',  ( 80.25229455199325912, -53.38333115846620558, 165.9811891832442825 ) ) ;
#26591 = EDGE_CURVE ( 'NONE', #52946, #82359, #71893, .T. ) ;
#26592 = CARTESIAN_POINT ( 'NONE',  ( 101.2019940638598854, 1.030564683017419500E-14, 0.000000000000000000 ) ) ;
#26593 = ORIENTED_EDGE ( 'NONE', *, *, #64836, .T. ) ;
#26594 = CARTESIAN_POINT ( 'NONE',  ( -32.94021323899823983, 485.0599191339509844, 5.361609822537348080 ) ) ;
#26595 = CYLINDRICAL_SURFACE ( 'NONE', #57596, 4.250000000000000000 ) ;
#26596 = DIRECTION ( 'NONE',  ( 0.000000000000000000, 0.000000000000000000, -1.000000000000000000 ) ) ;
#26597 = CARTESIAN_POINT ( 'NONE',  ( 0.000000000000000000, 0.000000000000000000, -9.975036109638290682 ) ) ;
#26598 = DIRECTION ( 'NONE',  ( 0.000000000000000000, 0.000000000000000000, -1.000000000000000000 ) ) ;
#26599 = CARTESIAN_POINT ( 'NONE',  ( -33.51634086989047745, 434.0198194387172634, 13.77974706611873223 ) ) ;
#26600 = ORIENTED_EDGE ( 'NONE', *, *, #3275, .T. ) ;
#26601 = CIRCLE ( 'NONE', #2440, 4.000000000000001776 ) ;
#26602 = DIRECTION ( 'NONE',  ( -1.000000000000000000, -0.000000000000000000, -0.000000000000000000 ) ) ;
#26603 = CARTESIAN_POINT ( 'NONE',  ( 87.32513032536655828, -39.06015956257186161, 189.6234660408021000 ) ) ;
#26604 = CARTESIAN_POINT ( 'NONE',  ( 0.1683254529209002592, 35.08181111624585924, -27.25000000000000711 ) ) ;
#26605 = VECTOR ( 'NONE', #33318, 1000.000000000000227 ) ;
#26606 = CARTESIAN_POINT ( 'NONE',  ( -2.977408999572654480, -24.12500000204838457, 7.188101187499999156 ) ) ;
#26607 = DIRECTION ( 'NONE',  ( 0.000000000000000000, -1.000000000000000000, 0.000000000000000000 ) ) ;
#26608 = AXIS2_PLACEMENT_3D ( 'NONE', #48051, #72856, #31906 ) ;
#26609 = CARTESIAN_POINT ( 'NONE',  ( 17.81438722625302518, 6.123233995736772199E-16, -5.000000000000001776 ) ) ;
#26610 = CARTESIAN_POINT ( 'NONE',  ( 41.68941770529601598, 436.0776509569181485, 20.67692828010792994 ) ) ;
#26611 = MECHANICAL_DESIGN_GEOMETRIC_PRESENTATION_REPRESENTATION (  '', ( #48951 ), #86872 ) ;
#26612 = VERTEX_POINT ( 'NONE', #35255 ) ;
#26613 = CARTESIAN_POINT ( 'NONE',  ( 43.63899620156487202, 434.3182181978403946, 14.37213632273145336 ) ) ;
#26614 = LINE ( 'NONE', #91840, #66764 ) ;
#26615 = CARTESIAN_POINT ( 'NONE',  ( -9.943426268670526369, 7.591391548649984777, 0.000000000000000000 ) ) ;
#26616 =( BOUNDED_SURFACE ( )  B_SPLINE_SURFACE ( 3, 2, ( 
 ( #39240, #47300, #71055 ),
 ( #80196, #104479, #64567 ),
 ( #6300, #105023, #31164 ),
 ( #47820, #72641, #30092 ),
 ( #31681, #62975, #48359 ),
 ( #23595, #89376, #81251 ) ),
 .UNSPECIFIED., .F., .F., .F. ) 
 B_SPLINE_SURFACE_WITH_KNOTS ( ( 4, 2, 4 ),
 ( 3, 3 ),
 ( 0.03206831234578191858, 0.03607477026923514019, 0.04008122819268836873 ),
 ( 0.000000000000000000, 1.000000000000000000 ),
 .UNSPECIFIED. ) 
 GEOMETRIC_REPRESENTATION_ITEM ( )  RATIONAL_B_SPLINE_SURFACE ( (
 ( 1.000000000000000000, 0.8047780936700358323, 1.000000000000000000),
 ( 1.000000000000000000, 0.8123790890099117368, 1.000000000000000000),
 ( 1.000000000000000000, 0.8190678900508682192, 1.000000000000000000),
 ( 1.000000000000000000, 0.8192345188317075033, 1.000000000000000000),
 ( 1.000000000000000000, 0.8126126219723355248, 1.000000000000000000),
 ( 1.000000000000000000, 0.8047712657247791945, 1.000000000000000000) ) ) 
 REPRESENTATION_ITEM ( '' )  SURFACE ( )  );
#26617 = FACE_OUTER_BOUND ( 'NONE', #102214, .T. ) ;
#26618 = VERTEX_POINT ( 'NONE', #61520 ) ;
#26619 = CARTESIAN_POINT ( 'NONE',  ( -30.00000000000000000, 464.1958267128339344, 14.61098489593202920 ) ) ;
#26620 = CARTESIAN_POINT ( 'NONE',  ( -7.500000000000004441, 44.25000000000000711, -71.71180648257555390 ) ) ;
#26621 = ORIENTED_EDGE ( 'NONE', *, *, #75483, .F. ) ;
#26622 = CARTESIAN_POINT ( 'NONE',  ( 33.74590849135869064, 434.0087241940787521, 12.79517754095366477 ) ) ;
#26623 = CARTESIAN_POINT ( 'NONE',  ( -0.6190732552358791940, 13.31368202499944253, -49.41014691098467893 ) ) ;
#26624 = DIRECTION ( 'NONE',  ( -0.8191520442889975717, 0.000000000000000000, -0.5735764363510378328 ) ) ;
#26625 = LINE ( 'NONE', #59497, #18577 ) ;
#26626 = CARTESIAN_POINT ( 'NONE',  ( -92.00444157296256265, -60.00000000000001421, 202.3484270727608134 ) ) ;
#26627 = CARTESIAN_POINT ( 'NONE',  ( 10.12089751115670566, 43.29055768924980185, -15.40779740156171052 ) ) ;
#26628 = CARTESIAN_POINT ( 'NONE',  ( 97.73333333333333428, 4.172000000000019249, 0.000000000000000000 ) ) ;
#26629 = DIRECTION ( 'NONE',  ( -0.000000000000000000, 1.000000000000000000, -0.000000000000000000 ) ) ;
#26630 = CARTESIAN_POINT ( 'NONE',  ( -83.21273294567592416, -57.32323371491776243, 189.0402996391318879 ) ) ;
#26631 = EDGE_CURVE ( 'NONE', #77823, #39684, #39187, .T. ) ;
#26632 = MECHANICAL_DESIGN_GEOMETRIC_PRESENTATION_REPRESENTATION (  '', ( #55826 ), #76553 ) ;
#26633 = EDGE_LOOP ( 'NONE', ( #100676, #79635, #31894, #17939 ) ) ;
#26634 = DIRECTION ( 'NONE',  ( 0.5735764363510557073, -0.8191520442889850262, 1.003171929053516612E-16 ) ) ;
#26635 = EDGE_CURVE ( 'NONE', #64161, #90150, #74367, .T. ) ;
#26636 = CARTESIAN_POINT ( 'NONE',  ( 3.626288723285810534, -1.044241108143921126, 104.3502830461760880 ) ) ;
#26637 =( GEOMETRIC_REPRESENTATION_CONTEXT ( 3 ) GLOBAL_UNCERTAINTY_ASSIGNED_CONTEXT ( ( #24141 ) ) GLOBAL_UNIT_ASSIGNED_CONTEXT ( ( #56916, #49358, #106538 ) ) REPRESENTATION_CONTEXT ( 'NONE', 'WORKASPACE' ) );
#26638 = CARTESIAN_POINT ( 'NONE',  ( -85.12517225352462447, -52.70214463376765934, 4.505281520561013942 ) ) ;
#26639 = CARTESIAN_POINT ( 'NONE',  ( -16.48453010140518060, 43.81223275022514940, 4.157797401561229123 ) ) ;
#26640 = CARTESIAN_POINT ( 'NONE',  ( -1.469576158976823947E-15, -19.06250000409677270, 8.000000000000000000 ) ) ;
#26641 = FACE_OUTER_BOUND ( 'NONE', #100656, .T. ) ;
#26642 = CARTESIAN_POINT ( 'NONE',  ( -22.37422507490808954, 28.20471669103546475, 31.02961587878847638 ) ) ;
#26643 = CARTESIAN_POINT ( 'NONE',  ( 59.93162491489189847, -30.00000000000002842, 91.51739161628221098 ) ) ;
#26644 = CARTESIAN_POINT ( 'NONE',  ( -75.59778980771257295, -60.00000000000000711, -32.85486631586996253 ) ) ;
#26645 = CARTESIAN_POINT ( 'NONE',  ( -72.11871523709537257, -53.38464545085997059, 118.2014658002872665 ) ) ;
#26646 = ORIENTED_EDGE ( 'NONE', *, *, #99351, .T. ) ;
#26647 = CARTESIAN_POINT ( 'NONE',  ( 72.31505286502601848, -14.21045842199433373, 125.5027806063605595 ) ) ;
#26648 =( NAMED_UNIT ( * ) SI_UNIT ( $, .STERADIAN. ) SOLID_ANGLE_UNIT ( ) );
#26649 = CARTESIAN_POINT ( 'NONE',  ( 18.22952343553518162, -60.00000000000000000, 42.38361649051553570 ) ) ;
#26650 = EDGE_LOOP ( 'NONE', ( #42081, #30079, #103166, #27982 ) ) ;
#26651 = CARTESIAN_POINT ( 'NONE',  ( 9.865311185090694934, -11.68002284843480787, 9.419147808596591176 ) ) ;
#26652 = EDGE_CURVE ( 'NONE', #67620, #27128, #69253, .T. ) ;
#26653 = CARTESIAN_POINT ( 'NONE',  ( 7.188101187499999156, -24.12500000204838813, 2.977408999572654924 ) ) ;
#26654 = CARTESIAN_POINT ( 'NONE',  ( -4.472135954999580498, -9.729227799326372050, 4.000000000000000000 ) ) ;
#26655 = ORIENTED_EDGE ( 'NONE', *, *, #63996, .T. ) ;
#26656 = CARTESIAN_POINT ( 'NONE',  ( 0.000000000000000000, 300.0000000000000568, 0.000000000000000000 ) ) ;
#26657 = DIRECTION ( 'NONE',  ( 0.000000000000000000, 0.000000000000000000, -1.000000000000000000 ) ) ;
#26658 = CARTESIAN_POINT ( 'NONE',  ( 47.24423074384412757, 16.91655035847116650, -16.58644287016981522 ) ) ;
#26659 = CARTESIAN_POINT ( 'NONE',  ( 26.01965034449775516, 305.5777608012918449, -9.622097568370508114 ) ) ;
#26660 = CARTESIAN_POINT ( 'NONE',  ( -5.082755093536325042, -14.09375000204838457, -5.082755093536325930 ) ) ;
#26661 = CARTESIAN_POINT ( 'NONE',  ( -8.000000000000001776, -17.84375000409676915, 3.313708498984759387 ) ) ;
#26662 = CARTESIAN_POINT ( 'NONE',  ( 0.000000000000000000, 0.000000000000000000, 0.000000000000000000 ) ) ;
#26663 =( NAMED_UNIT ( * ) SI_UNIT ( $, .STERADIAN. ) SOLID_ANGLE_UNIT ( ) );
#26664 = CARTESIAN_POINT ( 'NONE',  ( -1.308996937480700895, 49.99999999999999289, -75.00000000000001421 ) ) ;
#26665 = CARTESIAN_POINT ( 'NONE',  ( 70.41111111111112564, 6.915964383211875250E-15, 0.000000000000000000 ) ) ;
#26666 = VECTOR ( 'NONE', #25225, 999.9999999999998863 ) ;
#26667 = ORIENTED_EDGE ( 'NONE', *, *, #71874, .F. ) ;
#26668 = CARTESIAN_POINT ( 'NONE',  ( -7.126323198032135764, 41.48433374936583107, -70.04207028682751002 ) ) ;
#26670 = CARTESIAN_POINT ( 'NONE',  ( 32.66538190274433617, -53.37042454289756677, 36.73435524595355162 ) ) ;
#26669 =( LENGTH_UNIT ( ) NAMED_UNIT ( * ) SI_UNIT ( .MILLI., .METRE. ) );
#26671 = CARTESIAN_POINT ( 'NONE',  ( 35.53638905438354101, 390.1040284153648940, 6.613863457673663682 ) ) ;
#26672 = EDGE_LOOP ( 'NONE', ( #16760, #28835, #84390, #16937, #103359 ) ) ;
#26673 = SURFACE_STYLE_USAGE ( .BOTH. , #6313 ) ;
#26674 = EDGE_CURVE ( 'NONE', #62090, #70831, #24369, .T. ) ;
#26675 = UNCERTAINTY_MEASURE_WITH_UNIT (LENGTH_MEASURE( 1.000000000000000082E-05 ), #58357, 'distance_accuracy_value', 'NONE');
#26676 = AXIS2_PLACEMENT_3D ( 'NONE', #35128, #76076, #57753 ) ;
#26677 = VERTEX_POINT ( 'NONE', #9334 ) ;
#26679 = DIRECTION ( 'NONE',  ( 0.000000000000000000, 0.000000000000000000, -1.000000000000000000 ) ) ;
#26678 = CARTESIAN_POINT ( 'NONE',  ( 0.000000000000000000, -46.00000000000000000, 112.0000000000000000 ) ) ;
#26680 = CARTESIAN_POINT ( 'NONE',  ( 11.08349330513380515, 4.898587196589411843E-16, -4.000000000000001776 ) ) ;
#26681 = CARTESIAN_POINT ( 'NONE',  ( -34.02541642150921319, 436.1155524591087556, 7.421587081314565459 ) ) ;
#26682 = AXIS2_PLACEMENT_3D ( 'NONE', #17491, #19651, #9900 ) ;
#26683 = CIRCLE ( 'NONE', #73109, 5.000000000000002665 ) ;
#26684 = CARTESIAN_POINT ( 'NONE',  ( 0.000000000000000000, -1.023477375540016387, 0.000000000000000000 ) ) ;
#26685 = PRESENTATION_LAYER_ASSIGNMENT (  '', '', ( #73110 ) ) ;
#26686 = CARTESIAN_POINT ( 'NONE',  ( 83.86866073052654258, -5.000000000000000888, 6.123233995736779101E-16 ) ) ;
#26687 = CARTESIAN_POINT ( 'NONE',  ( -37.07355662510683914, 464.0045528213379384, 19.58584291728184823 ) ) ;
#26688 = ORIENTED_EDGE ( 'NONE', *, *, #84570, .T. ) ;
#26689 = CARTESIAN_POINT ( 'NONE',  ( 81.12704008932206534, -60.00000000000000711, -27.25892719060451341 ) ) ;
#26690 = LINE ( 'NONE', #85979, #82595 ) ;
#26691 = AXIS2_PLACEMENT_3D ( 'NONE', #52909, #68578, #85831 ) ;
#26692 = DIRECTION ( 'NONE',  ( 0.000000000000000000, -1.000000000000000000, 0.000000000000000000 ) ) ;
#26693 =( GEOMETRIC_REPRESENTATION_CONTEXT ( 3 ) GLOBAL_UNCERTAINTY_ASSIGNED_CONTEXT ( ( #104097 ) ) GLOBAL_UNIT_ASSIGNED_CONTEXT ( ( #60796, #85605, #4144 ) ) REPRESENTATION_CONTEXT ( 'NONE', 'WORKASPACE' ) );
#26694 = CARTESIAN_POINT ( 'NONE',  ( -46.77678417914653153, 18.74709138458503332, -15.58010501040351592 ) ) ;
#26695 = EDGE_CURVE ( 'NONE', #61495, #39668, #42624, .T. ) ;
#26696 = VERTEX_POINT ( 'NONE', #99954 ) ;
#26697 = EDGE_CURVE ( 'NONE', #40330, #66259, #28909, .T. ) ;
#26698 = CARTESIAN_POINT ( 'NONE',  ( -36.81701302529270237, 27.89050725896737859, 13.21903061592501061 ) ) ;
#26699 = ORIENTED_EDGE ( 'NONE', *, *, #82452, .F. ) ;
#26700 = ORIENTED_EDGE ( 'NONE', *, *, #94079, .F. ) ;
#26701 = CARTESIAN_POINT ( 'NONE',  ( 7.002641335706727865, 83.94912737319167206, 3.868676264653293728 ) ) ;
#26702 = CARTESIAN_POINT ( 'NONE',  ( 51.01037695545453232, 500.0000000000002274, 0.000000000000000000 ) ) ;
#26703 = CARTESIAN_POINT ( 'NONE',  ( -16.75187969033554936, 34.99134772383131065, -21.80698433968595751 ) ) ;
#26704 = CARTESIAN_POINT ( 'NONE',  ( 30.11650669486618881, 1.474610560812782335E-15, 0.000000000000000000 ) ) ;
#26705 = CARTESIAN_POINT ( 'NONE',  ( 82.73735319387645859, -37.80016373507481120, -11.88716716749071800 ) ) ;
#26706 = CARTESIAN_POINT ( 'NONE',  ( -40.15721392778465315, 315.4447579100735197, 2.968104171095417243 ) ) ;
#26707 = CARTESIAN_POINT ( 'NONE',  ( -18.67438172734769353, 303.6203036519360694, -10.04920665861971507 ) ) ;
#26708 = CARTESIAN_POINT ( 'NONE',  ( -17.39223945882862665, 34.17273883436914872, 24.13379576214062538 ) ) ;
#26709 = ORIENTED_EDGE ( 'NONE', *, *, #45674, .T. ) ;
#26710 = CARTESIAN_POINT ( 'NONE',  ( 33.74271564777244237, 484.1802673187708592, 2.058285076122321922 ) ) ;
#26711 = VERTEX_POINT ( 'NONE', #30210 ) ;
#26712 = CARTESIAN_POINT ( 'NONE',  ( 9.500904806078523279, 51.30114290918681519, -3.607704468417440857 ) ) ;
#26713 = DIRECTION ( 'NONE',  ( 0.000000000000000000, 0.000000000000000000, 1.000000000000000000 ) ) ;
#26715 = ORIENTED_EDGE ( 'NONE', *, *, #42462, .F. ) ;
#26714 = CARTESIAN_POINT ( 'NONE',  ( -42.19179521602280403, 485.4956273777414708, -3.824025998168937512 ) ) ;
#26716 = CARTESIAN_POINT ( 'NONE',  ( 76.26163437509697474, -25.60425469984666691, 115.8635891106310680 ) ) ;
#26717 = ADVANCED_FACE ( 'NONE', ( #64168 ), #104598, .T. ) ;
#26718 = ORIENTED_EDGE ( 'NONE', *, *, #103403, .T. ) ;
#26719 = CARTESIAN_POINT ( 'NONE',  ( 0.7777777777777733492, -50.00000000000000711, 40.97837836547554957 ) ) ;
#26720 = DIRECTION ( 'NONE',  ( 0.000000000000000000, 0.5000000000000009992, 0.8660254037844381525 ) ) ;
#26721 = CARTESIAN_POINT ( 'NONE',  ( -2.977408999572650039, -26.18750000204838457, -7.188101187500000933 ) ) ;
#26722 = AXIS2_PLACEMENT_3D ( 'NONE', #62520, #45793, #52817 ) ;
#26723 = CARTESIAN_POINT ( 'NONE',  ( -95.04855897266367037, -57.67186573470212352, 33.03592761066350647 ) ) ;
#26724 = ADVANCED_FACE ( 'NONE', ( #63095 ), #14509, .F. ) ;
#26725 = AXIS2_PLACEMENT_3D ( 'NONE', #101149, #35391, #75262 ) ;
#26726 = VERTEX_POINT ( 'NONE', #22120 ) ;
#26727 = DIRECTION ( 'NONE',  ( 0.000000000000000000, 0.000000000000000000, -1.000000000000000000 ) ) ;
#26728 = CARTESIAN_POINT ( 'NONE',  ( 105.0593050701437079, -52.71712251083815204, 179.5715820065424850 ) ) ;
#26729 = CARTESIAN_POINT ( 'NONE',  ( 0.000000000000000000, 0.000000000000000000, 0.000000000000000000 ) ) ;
#26730 = CARTESIAN_POINT ( 'NONE',  ( 4.250000000000000000, 0.000000000000000000, -3.764187203485586330 ) ) ;
#26731 = CARTESIAN_POINT ( 'NONE',  ( 8.000000000000000000, -26.09375000409677270, -3.313708498984761608 ) ) ;
#26732 = EDGE_CURVE ( 'NONE', #70311, #80736, #85773, .T. ) ;
#26733 = CYLINDRICAL_SURFACE ( 'NONE', #10636, 7.499999999992679633 ) ;
#26734 = DIRECTION ( 'NONE',  ( 0.000000000000000000, 0.000000000000000000, 1.000000000000000000 ) ) ;
#26735 =( NAMED_UNIT ( * ) SI_UNIT ( $, .STERADIAN. ) SOLID_ANGLE_UNIT ( ) );
#26736 = CARTESIAN_POINT ( 'NONE',  ( 9.646083234704169840, 33.01290609023479306, -2.643797197754292228 ) ) ;
#26737 = DIRECTION ( 'NONE',  ( 0.000000000000000000, 1.000000000000000000, 0.000000000000000000 ) ) ;
#26738 = DIRECTION ( 'NONE',  ( 0.000000000000000000, 0.000000000000000000, 1.000000000000000000 ) ) ;
#26739 = CARTESIAN_POINT ( 'NONE',  ( 31.80704930621342541, 485.2748291366697231, 5.788617803630847547 ) ) ;
#26740 = ORIENTED_EDGE ( 'NONE', *, *, #32190, .F. ) ;
#26741 = DIRECTION ( 'NONE',  ( 0.000000000000000000, -1.000000000000000000, 0.000000000000000000 ) ) ;
#26742 = DIRECTION ( 'NONE',  ( -1.000000000000000000, -1.224606353822377258E-16, -0.000000000000000000 ) ) ;
#26743 = CARTESIAN_POINT ( 'NONE',  ( 1.231392085578007389, 11.27926140874486727, 50.25247630643868746 ) ) ;
#26744 = CARTESIAN_POINT ( 'NONE',  ( -86.31276977314503540, -29.99999999999999645, 180.5061992413450298 ) ) ;
#26745 = ORIENTED_EDGE ( 'NONE', *, *, #92950, .T. ) ;
#26746 = CARTESIAN_POINT ( 'NONE',  ( 33.52307692307692122, 4.172000000000003261, 0.000000000000000000 ) ) ;
#26747 = CARTESIAN_POINT ( 'NONE',  ( 71.49549276749331739, -57.67960528813748056, 166.9847680060588857 ) ) ;
#26748 = AXIS2_PLACEMENT_3D ( 'NONE', #53198, #54225, #20354 ) ;
#26750 = DIRECTION ( 'NONE',  ( 0.000000000000000000, -1.000000000000000000, 0.000000000000000000 ) ) ;
#26749 = CARTESIAN_POINT ( 'NONE',  ( -15.29454505947251164, 3.501281615896531640, -3.973654925239204605 ) ) ;
#26751 = CARTESIAN_POINT ( 'NONE',  ( 34.56201351537013267, -31.18758961746727465, -37.90746136657972443 ) ) ;
#26752 = CARTESIAN_POINT ( 'NONE',  ( -15.66336674554169406, 21.48481245971760956, -5.205033774386319756 ) ) ;
#26753 = AXIS2_PLACEMENT_3D ( 'NONE', #26111, #11449, #9855 ) ;
#26754 = CARTESIAN_POINT ( 'NONE',  ( -40.04008949875484547, 489.2273486934108178, 11.31296313617192517 ) ) ;
#26755 = CARTESIAN_POINT ( 'NONE',  ( -40.00918711724499843, -59.99999999999998579, 52.09662703808838558 ) ) ;
#26756 = AXIS2_PLACEMENT_3D ( 'NONE', #71898, #7913, #15483 ) ;
#26757 = SURFACE_STYLE_USAGE ( .BOTH. , #67713 ) ;
#26758 = B_SPLINE_CURVE_WITH_KNOTS ( 'NONE', 3,
 ( #66449, #99327, #32520, #33052, #81536, #50263 ),
 .UNSPECIFIED., .F., .F.,
 ( 4, 2, 4 ),
 ( 1.226634733346699349E-18, 0.002016319290324606727, 0.004032638580649211719 ),
 .UNSPECIFIED. ) ;
#26759 = CIRCLE ( 'NONE', #40494, 4.000000000000000888 ) ;
#26760 = CARTESIAN_POINT ( 'NONE',  ( -85.44437512040904892, -61.07326030157955188, 193.8761068449719573 ) ) ;
#26761 = ORIENTED_EDGE ( 'NONE', *, *, #12607, .F. ) ;
#26762 = DIRECTION ( 'NONE',  ( -1.000000000000000000, -1.224606353822377258E-16, -0.000000000000000000 ) ) ;
#26763 = CARTESIAN_POINT ( 'NONE',  ( -5.033944729454126410, -32.51260769746507151, 29.29872852438901631 ) ) ;
#26764 = DIRECTION ( 'NONE',  ( 0.000000000000000000, 0.000000000000000000, 1.000000000000000000 ) ) ;
#26765 = CARTESIAN_POINT ( 'NONE',  ( -1.083333333333332593, -6.880090707843076636, -5.848636054922048189 ) ) ;
#26767 = CARTESIAN_POINT ( 'NONE',  ( 3.583116682864208258, -68.97239290731430117, 13.45661401736036211 ) ) ;
#26766 = CARTESIAN_POINT ( 'NONE',  ( -42.77939692685449558, 390.9255358409083669, 19.61564233301173843 ) ) ;
#26768 = ADVANCED_FACE ( 'NONE', ( #6961 ), #19056, .T. ) ;
#26769 = VERTEX_POINT ( 'NONE', #53921 ) ;
#26770 =( LENGTH_UNIT ( ) NAMED_UNIT ( * ) SI_UNIT ( .MILLI., .METRE. ) );
#26771 = CARTESIAN_POINT ( 'NONE',  ( 0.08416673536544136414, 28.20649408426940141, 38.24999999999999289 ) ) ;
#26772 = CARTESIAN_POINT ( 'NONE',  ( -30.82780738024908729, 10.08347807711980515, -40.33814864068006756 ) ) ;
#26773 = CARTESIAN_POINT ( 'NONE',  ( 25.45638573206032618, 295.6828782483409555, -9.821760129149877727 ) ) ;
#26774 = EDGE_CURVE ( 'NONE', #99463, #72747, #9983, .T. ) ;
#26775 = CARTESIAN_POINT ( 'NONE',  ( 45.31383884518383098, 362.9196860876334085, 5.161789940898600548 ) ) ;
#26776 =( BOUNDED_SURFACE ( )  B_SPLINE_SURFACE ( 3, 2, ( 
 ( #104262, #30408, #12069 ),
 ( #22325, #46046, #69791 ),
 ( #45527, #20762, #53598 ),
 ( #78930, #88099, #20226 ) ),
 .UNSPECIFIED., .F., .F., .F. ) 
 B_SPLINE_SURFACE_WITH_KNOTS ( ( 4, 4 ),
 ( 3, 3 ),
 ( 0.05778559309751216816, 0.08382991918232818307 ),
 ( 0.3700819400308131280, 1.000000000000000000 ),
 .UNSPECIFIED. ) 
 GEOMETRIC_REPRESENTATION_ITEM ( )  RATIONAL_B_SPLINE_SURFACE ( (
 ( 0.8634409734957675386, 0.8155016339180689577, 1.000000000000000000),
 ( 0.8634412033712403067, 0.8155019444918201188, 1.000000000000000000),
 ( 0.8634411474490393257, 0.8155018689380103547, 1.000000000000000000),
 ( 0.8634409197777686007, 0.8155015613422507137, 1.000000000000000000) ) ) 
 REPRESENTATION_ITEM ( '' )  SURFACE ( )  );
#26777 = SURFACE_SIDE_STYLE ('',( #100614 ) ) ;
#26778 = CARTESIAN_POINT ( 'NONE',  ( 31.08349330513380337, 4.898587196589405926E-16, -4.000000000000001776 ) ) ;
#26779 = CARTESIAN_POINT ( 'NONE',  ( 108.0662294780436383, -29.99999999999999645, 149.4678247624379708 ) ) ;
#26780 = CARTESIAN_POINT ( 'NONE',  ( -82.46821273478651904, -25.62404814617509530, 146.0476204998806793 ) ) ;
#26781 = ORIENTED_EDGE ( 'NONE', *, *, #69849, .T. ) ;
#26782 = LINE ( 'NONE', #93071, #89472 ) ;
#26783 = CARTESIAN_POINT ( 'NONE',  ( 6.000469943554648466, 254.0007049167048478, 0.2622423038614427604 ) ) ;
#26784 = CARTESIAN_POINT ( 'NONE',  ( 39.13906141225513835, -57.69405802890273094, 54.30799458850530215 ) ) ;
#26785 = CARTESIAN_POINT ( 'NONE',  ( 0.000000000000000000, 0.000000000000000000, -6.800000000000000711 ) ) ;
#26786 =( BOUNDED_SURFACE ( )  B_SPLINE_SURFACE ( 3, 2, ( 
 ( #40548, #17358, #83134 ),
 ( #73432, #65361, #80993 ),
 ( #9231, #64312, #97184 ),
 ( #23328, #41084, #56169 ),
 ( #89110, #15206, #59952 ),
 ( #11348, #20048, #60485 ),
 ( #68015, #42674, #93365 ),
 ( #76097, #19517, #68567 ),
 ( #52352, #69096, #26538 ),
 ( #2198, #44280, #75573 ),
 ( #2737, #26016, #50742 ),
 ( #100901, #27069, #101969 ) ),
 .UNSPECIFIED., .F., .F., .F. ) 
 B_SPLINE_SURFACE_WITH_KNOTS ( ( 4, 2, 2, 2, 2, 4 ),
 ( 3, 3 ),
 ( 6.260183343931302602E-16, 0.0007735885786028768403, 0.001547177157205127662, 0.001933971446506253019, 0.002320765735807378376, 0.003094354314409629089 ),
 ( 0.000000000000000000, 1.000000000000000000 ),
 .UNSPECIFIED. ) 
 GEOMETRIC_REPRESENTATION_ITEM ( )  RATIONAL_B_SPLINE_SURFACE ( (
 ( 1.000000000000000000, 0.9603284238771461201, 1.000000000000000000),
 ( 1.000000000000000000, 0.9628724889915971641, 1.000000000000000000),
 ( 1.000000000000000000, 0.9663306537745371960, 1.000000000000000000),
 ( 1.000000000000000000, 0.9744563874113795210, 1.000000000000000000),
 ( 1.000000000000000000, 0.9789903143387164164, 1.000000000000000000),
 ( 1.000000000000000000, 0.9855527733005580160, 1.000000000000000000),
 ( 1.000000000000000000, 0.9877025284828774288, 1.000000000000000000),
 ( 1.000000000000000000, 0.9916277982505475874, 1.000000000000000000),
 ( 1.000000000000000000, 0.9934221110298016022, 1.000000000000000000),
 ( 1.000000000000000000, 0.9980179737616281521, 1.000000000000000000),
 ( 1.000000000000000000, 1.000016370385754083, 1.000000000000000000),
 ( 1.000000000000000000, 1.000000000000000000, 1.000000000000000000) ) ) 
 REPRESENTATION_ITEM ( '' )  SURFACE ( )  );
#26787 = CARTESIAN_POINT ( 'NONE',  ( 4.678819457397437986, 8.078722181090837395, -5.000000000000000000 ) ) ;
#26788 = VERTEX_POINT ( 'NONE', #31283 ) ;
#26789 = UNCERTAINTY_MEASURE_WITH_UNIT (LENGTH_MEASURE( 1.000000000000000082E-05 ), #72703, 'distance_accuracy_value', 'NONE');
#26790 = FACE_BOUND ( 'NONE', #12184, .T. ) ;
#26791 = ORIENTED_EDGE ( 'NONE', *, *, #46196, .F. ) ;
#26792 = DIRECTION ( 'NONE',  ( -1.000000000000000000, -0.000000000000000000, -0.000000000000000000 ) ) ;
#26793 = PLANE ( 'NONE',  #48037 ) ;
#26794 = CARTESIAN_POINT ( 'NONE',  ( 37.62251730745840916, 437.3427388312647395, 4.535622330043188377 ) ) ;
#26795 = CARTESIAN_POINT ( 'NONE',  ( -58.76133767616301640, 50.00000000000000000, 23.44026136864787446 ) ) ;
#26796 = CARTESIAN_POINT ( 'NONE',  ( 6.038222094115994310, -12.57840291894174989, 12.65816746961330885 ) ) ;
#26797 = FACE_OUTER_BOUND ( 'NONE', #72133, .T. ) ;
#26798 = ORIENTED_EDGE ( 'NONE', *, *, #8144, .T. ) ;
#26799 = CARTESIAN_POINT ( 'NONE',  ( 109.9245725901865853, -60.00000000000000000, 191.4319832265045704 ) ) ;
#26801 = CARTESIAN_POINT ( 'NONE',  ( 18.86798682596964838, -32.51239220599620694, 29.71099402561047498 ) ) ;
#26800 = CARTESIAN_POINT ( 'NONE',  ( -85.76719879059909601, -14.21045842199445630, 195.9089143291284074 ) ) ;
#26802 = CARTESIAN_POINT ( 'NONE',  ( 37.66154869537736261, 377.9587457276326177, 5.098102565965574762 ) ) ;
#26803 = CARTESIAN_POINT ( 'NONE',  ( -40.63004339231220996, -25.69609495895222651, 36.04365259879974559 ) ) ;
#26804 = EDGE_CURVE ( 'NONE', #34768, #13191, #5060, .T. ) ;
#26805 = CARTESIAN_POINT ( 'NONE',  ( -37.29474511894800770, 18.64284798593206105, -9.274907802262537970 ) ) ;
#26806 = UNCERTAINTY_MEASURE_WITH_UNIT (LENGTH_MEASURE( 1.000000000000000082E-05 ), #28727, 'distance_accuracy_value', 'NONE');
#26807 = ORIENTED_EDGE ( 'NONE', *, *, #90182, .T. ) ;
#26808 = CARTESIAN_POINT ( 'NONE',  ( -1.650803255657556479, -4.285714285714296246, 25.22241582816892702 ) ) ;
#26809 = DIRECTION ( 'NONE',  ( 1.871721906610600077E-16, 0.000000000000000000, -1.000000000000000000 ) ) ;
#26810 = CARTESIAN_POINT ( 'NONE',  ( 6.840078058529589278, -12.20617675668042601, 8.820020145246234122 ) ) ;
#26811 = SURFACE_STYLE_USAGE ( .BOTH. , #35430 ) ;
#26812 = CARTESIAN_POINT ( 'NONE',  ( 5.819846122303830249, 6.321060697774965931, 2.051601713726983078 ) ) ;
#26813 = CARTESIAN_POINT ( 'NONE',  ( -34.90665437305706575, 461.8152559346092971, 3.957791774131551144 ) ) ;
#26814 = VERTEX_POINT ( 'NONE', #73279 ) ;
#26815 = CARTESIAN_POINT ( 'NONE',  ( -16.42611686831678242, 36.46285186709818760, -24.26654634025086210 ) ) ;
#26816 = ORIENTED_EDGE ( 'NONE', *, *, #24544, .F. ) ;
#26817 = VECTOR ( 'NONE', #54009, 1000.000000000000000 ) ;
#26818 = CARTESIAN_POINT ( 'NONE',  ( 57.01429441072921378, -30.00000000006595968, 82.99024849085006394 ) ) ;
#26819 = CARTESIAN_POINT ( 'NONE',  ( 29.92008363729422982, 41.07848214471710691, -66.38191137410871079 ) ) ;
#26820 = UNCERTAINTY_MEASURE_WITH_UNIT (LENGTH_MEASURE( 1.000000000000000082E-05 ), #90012, 'distance_accuracy_value', 'NONE');
#26821 = CARTESIAN_POINT ( 'NONE',  ( 24.46199350025671038, 25.40999692020810130, -31.75662788421451665 ) ) ;
#26822 = CARTESIAN_POINT ( 'NONE',  ( 83.30424347533678997, -30.00000000000000711, 45.32559808931431178 ) ) ;
#26823 = CARTESIAN_POINT ( 'NONE',  ( -32.10816233020364052, 435.9969136641942100, 24.01734164033964092 ) ) ;
#26824 = EDGE_CURVE ( 'NONE', #10145, #44815, #104765, .T. ) ;
#26825 = EDGE_LOOP ( 'NONE', ( #56411, #93207, #24562, #24289, #13592, #2861, #103757, #51228 ) ) ;
#26826 = AXIS2_PLACEMENT_3D ( 'NONE', #85716, #67400, #51721 ) ;
#26827 = B_SPLINE_CURVE_WITH_KNOTS ( 'NONE', 3,
 ( #12639, #38035, #87622, #63882 ),
 .UNSPECIFIED., .F., .F.,
 ( 4, 4 ),
 ( 6.938893903907228378E-18, 0.0004064560158441167894 ),
 .UNSPECIFIED. ) ;
#26828 = ORIENTED_EDGE ( 'NONE', *, *, #97761, .T. ) ;
#26829 = ORIENTED_EDGE ( 'NONE', *, *, #30294, .F. ) ;
#26831 = ORIENTED_EDGE ( 'NONE', *, *, #71252, .F. ) ;
#26830 = CARTESIAN_POINT ( 'NONE',  ( -48.02835407290533709, 9.771516447483559631, -16.85535821593460426 ) ) ;
#26832 = CARTESIAN_POINT ( 'NONE',  ( 32.87547266101556431, 465.6993878536748070, 10.91512469976365551 ) ) ;
#26833 = CARTESIAN_POINT ( 'NONE',  ( -36.56938426534607345, 26.05443706425352346, -11.43459265307532746 ) ) ;
#26834 = VECTOR ( 'NONE', #84481, 1000.000000000000000 ) ;
#26835 = CARTESIAN_POINT ( 'NONE',  ( 5.981118819178458779, -13.97183456180058947, 0.5452870891823661248 ) ) ;
#26836 = CARTESIAN_POINT ( 'NONE',  ( -32.10523269976815897, 436.9427959952963647, 23.91264094315748068 ) ) ;
#26837 = DIRECTION ( 'NONE',  ( 0.000000000000000000, 0.000000000000000000, 1.000000000000000000 ) ) ;
#26838 = EDGE_LOOP ( 'NONE', ( #33974, #56124, #38211, #100969, #87317 ) ) ;
#26839 = CARTESIAN_POINT ( 'NONE',  ( 10.48543666094595217, 50.00000000000000000, -78.95657223723276275 ) ) ;
#26840 = EDGE_LOOP ( 'NONE', ( #76072, #2314, #95349, #11733 ) ) ;
#26841 = CARTESIAN_POINT ( 'NONE',  ( 32.88333705524178896, 439.7317646416724415, 24.13381181826117228 ) ) ;
#26842 = CARTESIAN_POINT ( 'NONE',  ( 74.51953474006475631, -38.33012379840763373, 164.9748051664451793 ) ) ;
#26843 = CARTESIAN_POINT ( 'NONE',  ( 5.975663821522140928, 7.000939006314000679, -0.8740179403733884245 ) ) ;
#26844 = VECTOR ( 'NONE', #78319, 1000.000000000000000 ) ;
#26845 = AXIS2_PLACEMENT_3D ( 'NONE', #10447, #57930, #68164 ) ;
#26846 = CARTESIAN_POINT ( 'NONE',  ( 30.76197147106075747, 299.0183610105614775, 10.86750422692454343 ) ) ;
#26847 = AXIS2_PLACEMENT_3D ( 'NONE', #36075, #99151, #2052 ) ;
#26848 = CARTESIAN_POINT ( 'NONE',  ( -4.472135954999578722, 249.9999999999999432, 4.000000000000002665 ) ) ;
#26849 = CIRCLE ( 'NONE', #45595, 3.309500000000001663 ) ;
#26850 = ORIENTED_EDGE ( 'NONE', *, *, #97959, .T. ) ;
#26851 = CIRCLE ( 'NONE', #45746, 60.00000000000000000 ) ;
#26852 = CARTESIAN_POINT ( 'NONE',  ( 17.26536970378601765, 45.41327343741739497, -6.504208684746127567 ) ) ;
#26853 = CARTESIAN_POINT ( 'NONE',  ( 0.000000000000000000, 0.000000000000000000, 0.000000000000000000 ) ) ;
#26854 = CARTESIAN_POINT ( 'NONE',  ( -16.75187969033532553, 37.11970326878314808, 21.80698433968612093 ) ) ;
#26855 = ADVANCED_FACE ( 'NONE', ( #58724 ), #17206, .F. ) ;
#26856 = CARTESIAN_POINT ( 'NONE',  ( 14.99524476912893434, 1.250852691627993396, -0.4434096852967474578 ) ) ;
#26857 = ORIENTED_EDGE ( 'NONE', *, *, #102723, .F. ) ;
#26859 = DIRECTION ( 'NONE',  ( 0.000000000000000000, 0.5000000000000018874, 0.8660254037844374864 ) ) ;
#26858 = SURFACE_STYLE_USAGE ( .BOTH. , #83980 ) ;
#26860 = CARTESIAN_POINT ( 'NONE',  ( 1.000000000000000222, -5.000000000000000000, -14.14213562373095101 ) ) ;
#26861 = CARTESIAN_POINT ( 'NONE',  ( 5.656854249492380582, -10.81249999999999289, -5.656854249492379694 ) ) ;
#26862 = CYLINDRICAL_SURFACE ( 'NONE', #93422, 13.27631144943088515 ) ;
#26863 = EDGE_CURVE ( 'NONE', #58211, #84262, #11739, .T. ) ;
#26864 = CARTESIAN_POINT ( 'NONE',  ( -7.150931910075641440, 103.2137420147773526, -3.588457848165358843 ) ) ;
#26865 = DIRECTION ( 'NONE',  ( -0.000000000000000000, 1.000000000000000000, 0.000000000000000000 ) ) ;
#26866 = CARTESIAN_POINT ( 'NONE',  ( 84.31560656641553919, -57.43926515212457673, 191.1735246261523855 ) ) ;
#26867 = CARTESIAN_POINT ( 'NONE',  ( -7.856156674185535316, 67.82625813595271325, 0.000000000000000000 ) ) ;
#26868 = ORIENTED_EDGE ( 'NONE', *, *, #104609, .F. ) ;
#26869 = CARTESIAN_POINT ( 'NONE',  ( -6.270061300899935297, 4.268872906156492952, -6.443866470201758290 ) ) ;
#26870 = EDGE_CURVE ( 'NONE', #21594, #76213, #23715, .T. ) ;
#26871 = DIRECTION ( 'NONE',  ( -1.000000000000000000, -0.000000000000000000, -0.000000000000000000 ) ) ;
#26872 = CARTESIAN_POINT ( 'NONE',  ( -10.00000000000000355, 105.0000000000000000, 0.000000000000000000 ) ) ;
#26873 = CARTESIAN_POINT ( 'NONE',  ( -1.469576158976823947E-15, -18.87499999999999289, 8.000000000000000000 ) ) ;
#26874 = CARTESIAN_POINT ( 'NONE',  ( -93.92629083922592770, -29.99999999999999645, 111.5267929669124101 ) ) ;
#26875 = CARTESIAN_POINT ( 'NONE',  ( 3.400000000000000355, 0.000000000000000000, -1.581124522925831499 ) ) ;
#26876 = CARTESIAN_POINT ( 'NONE',  ( 10.11650669486618881, 4.898587196589411843E-16, -4.000000000000000888 ) ) ;
#26877 = DIRECTION ( 'NONE',  ( 0.000000000000000000, 1.000000000000000000, 0.000000000000000000 ) ) ;
#26879 = FACE_OUTER_BOUND ( 'NONE', #73309, .T. ) ;
#26878 = CARTESIAN_POINT ( 'NONE',  ( -7.914973979435151463, -3.817460047930454348, -7.907502498112421563 ) ) ;
#26880 = CARTESIAN_POINT ( 'NONE',  ( 0.000000000000000000, 32.68727484027578356, 0.000000000000000000 ) ) ;
#26881 = CARTESIAN_POINT ( 'NONE',  ( -28.73416115563823681, -29.92329866866804977, 30.94992384361019688 ) ) ;
#26882 = CARTESIAN_POINT ( 'NONE',  ( 37.83989825151499531, 491.6297408768496098, 12.44743998625077630 ) ) ;
#26883 = CARTESIAN_POINT ( 'NONE',  ( 0.000000000000000000, -5.000000000000000000, 10.00000000000000000 ) ) ;
#26884 = DIRECTION ( 'NONE',  ( -1.000000000000000000, -0.000000000000000000, -0.000000000000000000 ) ) ;
#26885 = CARTESIAN_POINT ( 'NONE',  ( 40.90099630364926497, -25.13177883036392757, -30.10567145231062369 ) ) ;
#26886 = COLOUR_RGB ( '', 0.40784314, 0.44705882, 0.49803922) ;
#26887 = CARTESIAN_POINT ( 'NONE',  ( -23.35130136342643326, -29.03948800314977063, 29.66951933061897151 ) ) ;
#26888 = ORIENTED_EDGE ( 'NONE', *, *, #39369, .T. ) ;
#26889 = CARTESIAN_POINT ( 'NONE',  ( 6.242019780568028864, 10.53669266913567348, -3.192545347364960762 ) ) ;
#26890 = CARTESIAN_POINT ( 'NONE',  ( -9.918010731619574472, 108.7915168484322521, -1.300854425901575073 ) ) ;
#26891 = CARTESIAN_POINT ( 'NONE',  ( -19.99473970835801140, -32.51530817802121476, 29.81274010585231338 ) ) ;
#26892 = CARTESIAN_POINT ( 'NONE',  ( -71.80342408229677176, -30.00000000000000000, -19.71767938363507966 ) ) ;
#26894 = DIRECTION ( 'NONE',  ( -1.000000000000000000, -0.000000000000000000, -0.000000000000000000 ) ) ;
#26893 = CARTESIAN_POINT ( 'NONE',  ( 43.52560603733946465, 486.7876375777498197, 7.034422870327473376 ) ) ;
#26895 = EDGE_CURVE ( 'NONE', #48149, #103416, #77212, .T. ) ;
#26896 = VERTEX_POINT ( 'NONE', #25312 ) ;
#26897 = CARTESIAN_POINT ( 'NONE',  ( -36.47337843289997039, 437.5890141897104400, 4.249048303382426894 ) ) ;
#26898 = VERTEX_POINT ( 'NONE', #8020 ) ;
#26899 = EDGE_CURVE ( 'NONE', #93985, #596, #34131, .T. ) ;
#26900 = PRESENTATION_LAYER_ASSIGNMENT (  '', '', ( #56087 ) ) ;
#26901 = CARTESIAN_POINT ( 'NONE',  ( -8.000000000000000000, -24.03125000409677270, -3.313708498984762496 ) ) ;
#26902 = ORIENTED_EDGE ( 'NONE', *, *, #12769, .F. ) ;
#26903 = AXIS2_PLACEMENT_3D ( 'NONE', #69766, #61697, #80484 ) ;
#26904 = CARTESIAN_POINT ( 'NONE',  ( 15.47206823513687368, 2.694788529765176133, -1.611870258425112334 ) ) ;
#26905 = CIRCLE ( 'NONE', #38960, 4.000000000000000888 ) ;
#26906 = CARTESIAN_POINT ( 'NONE',  ( 100.8650305359696517, -52.74513607102953472, 193.5094557858945450 ) ) ;
#26907 = AXIS2_PLACEMENT_3D ( 'NONE', #80575, #22394, #79525 ) ;
#26909 = CARTESIAN_POINT ( 'NONE',  ( 11.36650669486618881, -3.851859888774471706E-31, 4.000000000000000888 ) ) ;
#26908 = CARTESIAN_POINT ( 'NONE',  ( 5.121377489766137714, -19.23622649283650077, 27.08678039004259830 ) ) ;
#26910 = VERTEX_POINT ( 'NONE', #41990 ) ;
#26911 = ORIENTED_EDGE ( 'NONE', *, *, #35079, .F. ) ;
#26912 = VECTOR ( 'NONE', #2145, 1000.000000000000000 ) ;
#26913 = ORIENTED_EDGE ( 'NONE', *, *, #38775, .F. ) ;
#26915 =( BOUNDED_CURVE ( )  B_SPLINE_CURVE ( 2, ( #96480, #7971, #81323 ),
 .UNSPECIFIED., .F., .F. ) 
 B_SPLINE_CURVE_WITH_KNOTS ( ( 3, 3 ),
 ( 0.000000000000000000, 1.000000000000000000 ),
 .UNSPECIFIED. ) 
 CURVE ( )  GEOMETRIC_REPRESENTATION_ITEM ( )  RATIONAL_B_SPLINE_CURVE ( ( 1.000000000000000000, 1.857142857142858317, 1.000000000000000000 ) ) 
 REPRESENTATION_ITEM ( '' )  );
#26914 = CARTESIAN_POINT ( 'NONE',  ( 27.18297321513363940, 309.6406833422096270, 11.30666984776100925 ) ) ;
#26916 = CARTESIAN_POINT ( 'NONE',  ( -39.33042632267828509, 460.7392826591625408, 2.124562382289973961 ) ) ;
#26917 = DIRECTION ( 'NONE',  ( 0.5735764363510440500, 0.8191520442889932418, 0.000000000000000000 ) ) ;
#26918 = EDGE_LOOP ( 'NONE', ( #13985, #53453, #8213, #42713 ) ) ;
#26919 = ADVANCED_FACE ( 'NONE', ( #41459 ), #62494, .F. ) ;
#26920 = DIRECTION ( 'NONE',  ( -1.000000000000000000, 0.000000000000000000, 0.000000000000000000 ) ) ;
#26921 = PRESENTATION_STYLE_ASSIGNMENT (( #35539 ) ) ;
#26922 = CARTESIAN_POINT ( 'NONE',  ( 31.47314211086991165, 438.9571839453554389, 23.21193214522953951 ) ) ;
#26923 = CARTESIAN_POINT ( 'NONE',  ( -92.22404989346505033, -59.99999999999755573, -19.73939852595544764 ) ) ;
#26924 = CARTESIAN_POINT ( 'NONE',  ( 0.000000000000000000, -54.00000000000000711, 45.00000000000000000 ) ) ;
#26925 = CONICAL_SURFACE ( 'NONE', #104410, 4.172000000000001485, 0.9599310885968750373 ) ;
#26926 = CARTESIAN_POINT ( 'NONE',  ( -22.42417502586373246, 305.3961751430792333, 10.05444931189341773 ) ) ;
#26927 = CARTESIAN_POINT ( 'NONE',  ( -6.729774149518023663, 41.69338218132584473, -58.98699202062753244 ) ) ;
#26928 = CARTESIAN_POINT ( 'NONE',  ( -77.20948002450832348, -29.99999999999995737, -26.53460153345886496 ) ) ;
#26929 = CARTESIAN_POINT ( 'NONE',  ( -43.53206229128350202, 464.6078677241816877, 9.489307009109641200 ) ) ;
#26930 = CARTESIAN_POINT ( 'NONE',  ( -51.29768049186471046, -18.72484688875610459, 45.83708237476789549 ) ) ;
#26931 = ORIENTED_EDGE ( 'NONE', *, *, #39644, .T. ) ;
#26932 = CARTESIAN_POINT ( 'NONE',  ( -4.472135954999578722, 249.9999999999999432, -4.000000000000002665 ) ) ;
#26933 = ORIENTED_EDGE ( 'NONE', *, *, #65772, .F. ) ;
#26934 = CARTESIAN_POINT ( 'NONE',  ( 4.898587196589412829E-16, -13.62499999999999112, -8.000000000000000000 ) ) ;
#26935 = CARTESIAN_POINT ( 'NONE',  ( -9.041223236741398495, 295.5670253727008685, -10.03755077321278222 ) ) ;
#26936 = CARTESIAN_POINT ( 'NONE',  ( 11.91633406602797685, -2.062723235127855492, 20.64923308538431712 ) ) ;
#26937 = VERTEX_POINT ( 'NONE', #49547 ) ;
#26938 = CARTESIAN_POINT ( 'NONE',  ( 5.094000037296067873, 247.5536587622877107, -3.174960020027676411 ) ) ;
#26939 = CARTESIAN_POINT ( 'NONE',  ( 81.18586761171566479, -38.84088417715932451, 194.8800132995233412 ) ) ;
#26940 = CARTESIAN_POINT ( 'NONE',  ( 3.384215095276664531, -49.13301901873818878, 104.0501775326194576 ) ) ;
#26941 = CYLINDRICAL_SURFACE ( 'NONE', #90978, 4.000000000000000888 ) ;
#26942 = AXIS2_PLACEMENT_3D ( 'NONE', #21225, #54054, #37937 ) ;
#26943 = LINE ( 'NONE', #75446, #1454 ) ;
#26944 = CARTESIAN_POINT ( 'NONE',  ( 87.05705487234845918, -30.00000000000000355, 183.9282422150870104 ) ) ;
#26945 = DIRECTION ( 'NONE',  ( 0.000000000000000000, 0.000000000000000000, 1.000000000000000000 ) ) ;
#26946 = DIRECTION ( 'NONE',  ( -1.000000000000000000, -0.000000000000000000, -0.000000000000000000 ) ) ;
#26947 = ORIENTED_EDGE ( 'NONE', *, *, #65905, .T. ) ;
#26948 = ORIENTED_EDGE ( 'NONE', *, *, #14262, .T. ) ;
#26949 = CARTESIAN_POINT ( 'NONE',  ( 52.29916411013782351, -25.64426098774818286, 49.83386183445969664 ) ) ;
#26950 = CARTESIAN_POINT ( 'NONE',  ( -45.99999999997621103, 435.9911642595333774, 13.93550065361152690 ) ) ;
#26951 = CARTESIAN_POINT ( 'NONE',  ( -7.500000000000007994, 40.00000000000000000, -72.67206406577980715 ) ) ;
#26952 = ORIENTED_EDGE ( 'NONE', *, *, #38703, .T. ) ;
#26953 = CARTESIAN_POINT ( 'NONE',  ( -85.51831432850400461, -38.36002604018491979, -22.36822977887920771 ) ) ;
#26954 = ORIENTED_EDGE ( 'NONE', *, *, #26086, .F. ) ;
#26955 = CARTESIAN_POINT ( 'NONE',  ( 107.7883601516577698, -38.35935003634334350, 193.3568233556534324 ) ) ;
#26956 = CARTESIAN_POINT ( 'NONE',  ( 13.08520229868874729, 23.85374324172591898, -4.084787787685606020 ) ) ;
#26957 = CARTESIAN_POINT ( 'NONE',  ( 85.97056482012806100, -45.28272053107379236, 43.44903282293562796 ) ) ;
#26958 = CARTESIAN_POINT ( 'NONE',  ( -1.220619361806398961, 45.62969810379784974, -17.81327476936460030 ) ) ;
#26959 = CARTESIAN_POINT ( 'NONE',  ( -9.999999999999994671, -3.000000000000003109, -83.69100306100425257 ) ) ;
#26960 = CARTESIAN_POINT ( 'NONE',  ( 4.312270534946733846, -9.512596744310483743, -11.64851190995536712 ) ) ;
#26961 = DIRECTION ( 'NONE',  ( 0.000000000000000000, 0.000000000000000000, 1.000000000000000000 ) ) ;
#26962 = COLOUR_RGB ( '', 0.40784314, 0.44705882, 0.49803922) ;
#26963 = DIRECTION ( 'NONE',  ( -1.000000000000000000, -0.000000000000000000, -0.000000000000000000 ) ) ;
#26964 = CARTESIAN_POINT ( 'NONE',  ( 7.955546711082998712, 53.39389859135090433, 2.456618345357718155E-12 ) ) ;
#26965 = VERTEX_POINT ( 'NONE', #48478 ) ;
#26966 = DIRECTION ( 'NONE',  ( 0.5735764363510466035, -0.8191520442889914655, 1.003171929053524500E-16 ) ) ;
#26967 = EDGE_CURVE ( 'NONE', #31421, #81027, #16927, .T. ) ;
#26968 = AXIS2_PLACEMENT_3D ( 'NONE', #19330, #51626, #100705 ) ;
#26969 = FACE_OUTER_BOUND ( 'NONE', #82225, .T. ) ;
#26970 = ORIENTED_EDGE ( 'NONE', *, *, #42584, .F. ) ;
#26971 = CARTESIAN_POINT ( 'NONE',  ( -5.122788966609808092, 53.50683659463715713, 8.531152949374556371 ) ) ;
#26972 = CARTESIAN_POINT ( 'NONE',  ( -40.93023141354418470, 381.5373706023750628, 26.74524372019637752 ) ) ;
#26973 = CARTESIAN_POINT ( 'NONE',  ( -18.99999999999999645, 4.000000000000000888, -1.500000000000000000 ) ) ;
#26974 = DIRECTION ( 'NONE',  ( 0.000000000000000000, -1.000000000000000000, 0.000000000000000000 ) ) ;
#26975 = CARTESIAN_POINT ( 'NONE',  ( -8.000000000000000000, -28.34374999999999289, -3.313708498984762496 ) ) ;
#26976 = AXIS2_PLACEMENT_3D ( 'NONE', #75077, #82660, #50801 ) ;
#26977 = CARTESIAN_POINT ( 'NONE',  ( 48.13867764410746020, -29.30200429754887992, 43.72835771138513650 ) ) ;
#26978 = ADVANCED_FACE ( 'NONE', ( #57100 ), #4833, .T. ) ;
#26979 = CIRCLE ( 'NONE', #9673, 2.000000000000000000 ) ;
#26980 = VECTOR ( 'NONE', #89666, 1000.000000000000000 ) ;
#26981 = AXIS2_PLACEMENT_3D ( 'NONE', #40180, #81161, #14300 ) ;
#26982 = AXIS2_PLACEMENT_3D ( 'NONE', #65707, #82948, #16081 ) ;
#26983 = CARTESIAN_POINT ( 'NONE',  ( 59.41111111111111143, 6.915964383211875250E-15, 0.000000000000000000 ) ) ;
#26984 = CIRCLE ( 'NONE', #82049, 3.309500000000001663 ) ;
#26985 = EDGE_LOOP ( 'NONE', ( #75991, #36864, #85301, #75184, #4530 ) ) ;
#26986 = CARTESIAN_POINT ( 'NONE',  ( 82.60104337135625485, -57.21257082304840935, 187.3407815826748788 ) ) ;
#26987 = DIRECTION ( 'NONE',  ( -1.000000000000000000, -0.000000000000000000, -0.000000000000000000 ) ) ;
#26988 = CARTESIAN_POINT ( 'NONE',  ( -87.14767027655014431, -37.99999999998310329, 189.0874028505847662 ) ) ;
#26989 = ORIENTED_EDGE ( 'NONE', *, *, #91496, .T. ) ;
#26990 = CARTESIAN_POINT ( 'NONE',  ( -97.17100149276052434, -37.82057918150324838, 120.9264675858186848 ) ) ;
#26991 = EDGE_CURVE ( 'NONE', #53736, #53725, #72049, .T. ) ;
#26992 = DIRECTION ( 'NONE',  ( 0.000000000000000000, -1.000000000000000000, 0.000000000000000000 ) ) ;
#26993 = CARTESIAN_POINT ( 'NONE',  ( -12.12626197893092339, -3.000000000000002665, -94.24800833403701006 ) ) ;
#26994 = CARTESIAN_POINT ( 'NONE',  ( 3.292161566725979593, 304.8518027751346722, 8.936999415071538166 ) ) ;
#26995 = CONICAL_SURFACE ( 'NONE', #66606, 4.000000000000001776, 0.9599310885968774798 ) ;
#26996 = CARTESIAN_POINT ( 'NONE',  ( -26.07542528179775587, -28.11225759749947883, -38.33793174107837132 ) ) ;
#26997 = CARTESIAN_POINT ( 'NONE',  ( 47.40123518113406220, -60.00000000000001421, 65.67392086698521325 ) ) ;
#26998 = CARTESIAN_POINT ( 'NONE',  ( 21.50348335299959857, -26.68737644460689751, 37.20438602441733167 ) ) ;
#26999 = CARTESIAN_POINT ( 'NONE',  ( 101.2019940638598854, 5.000000000000021316, 0.000000000000000000 ) ) ;
#27000 =( NAMED_UNIT ( * ) PLANE_ANGLE_UNIT ( ) SI_UNIT ( $, .RADIAN. ) );
#27002 = CARTESIAN_POINT ( 'NONE',  ( -11.42275469891026241, 20.37773691717305269, -8.181910656862440234 ) ) ;
#27001 = CARTESIAN_POINT ( 'NONE',  ( -30.23468791487915297, -32.60645102688423691, 40.71049962837252423 ) ) ;
#27003 = CARTESIAN_POINT ( 'NONE',  ( 7.088826403996534076, 296.1964324881835751, -10.02186216631562843 ) ) ;
#27004 = CARTESIAN_POINT ( 'NONE',  ( 33.08751701378358945, 301.6823158026044780, 11.49690784967660662 ) ) ;
#27005 = DIRECTION ( 'NONE',  ( 0.000000000000000000, -1.000000000000000000, 0.000000000000000000 ) ) ;
#27006 = CARTESIAN_POINT ( 'NONE',  ( 0.000000000000000000, -1.200000000000000030E-05, 17.50000000000000000 ) ) ;
#27007 = ORIENTED_EDGE ( 'NONE', *, *, #28315, .T. ) ;
#27008 = CARTESIAN_POINT ( 'NONE',  ( 0.000000000000000000, 0.000000000000000000, -9.975036109638290682 ) ) ;
#27009 = AXIS2_PLACEMENT_3D ( 'NONE', #91491, #25733, #50467 ) ;
#27010 = CARTESIAN_POINT ( 'NONE',  ( -17.49999999999995381, 51.39211690089769746, 62.71362001260538932 ) ) ;
#27011 = UNCERTAINTY_MEASURE_WITH_UNIT (LENGTH_MEASURE( 1.000000000000000082E-05 ), #16054, 'distance_accuracy_value', 'NONE');
#27012 = CARTESIAN_POINT ( 'NONE',  ( 59.89460441624491693, 6.975173280561618775E-15, 0.000000000000000000 ) ) ;
#27013 = AXIS2_PLACEMENT_3D ( 'NONE', #74498, #40544, #65358 ) ;
#27014 = DIRECTION ( 'NONE',  ( 0.000000000000000000, 0.000000000000000000, 1.000000000000000000 ) ) ;
#27016 = CARTESIAN_POINT ( 'NONE',  ( 40.42072553015707115, -21.77015276485149187, -27.31244395070953956 ) ) ;
#27015 = CARTESIAN_POINT ( 'NONE',  ( 9.176645556628276523, 250.5273903240672837, 3.973966573947710135 ) ) ;
#27017 = EDGE_CURVE ( 'NONE', #44463, #86259, #65206, .T. ) ;
#27018 = ORIENTED_EDGE ( 'NONE', *, *, #89607, .F. ) ;
#27019 = CARTESIAN_POINT ( 'NONE',  ( 27.42610126120553460, 36.50006826818918171, 10.02586106038927305 ) ) ;
#27020 = FACE_OUTER_BOUND ( 'NONE', #83424, .T. ) ;
#27021 = EDGE_LOOP ( 'NONE', ( #20004, #90289, #53712, #36832 ) ) ;
#27022 = ADVANCED_FACE ( 'NONE', ( #61388 ), #1334, .T. ) ;
#27023 = DIRECTION ( 'NONE',  ( 0.000000000000000000, -2.311253228826400140E-16, 1.000000000000000000 ) ) ;
#27024 = EDGE_CURVE ( 'NONE', #61594, #55094, #56479, .T. ) ;
#27025 = CARTESIAN_POINT ( 'NONE',  ( -6.738100187484505454, 41.71798639774085160, -59.05424569925489209 ) ) ;
#27026 = DIRECTION ( 'NONE',  ( -1.000000000000000000, -0.000000000000000000, -0.000000000000000000 ) ) ;
#27027 = CARTESIAN_POINT ( 'NONE',  ( -92.14138347090150205, -59.99999999999999289, 3.768088791749690802 ) ) ;
#27028 = CARTESIAN_POINT ( 'NONE',  ( -5.656854249492381470, -25.06249999999999289, 5.656854249492379694 ) ) ;
#27029 = CARTESIAN_POINT ( 'NONE',  ( 6.562874270078295602, 3.301808241302743863, 6.845811579416823278 ) ) ;
#27030 = CARTESIAN_POINT ( 'NONE',  ( 31.19652432992544888, 378.3327707670021027, 24.28948218791313707 ) ) ;
#27031 = CARTESIAN_POINT ( 'NONE',  ( 41.50820411079202188, 461.5963371455320612, 2.703439750996334823 ) ) ;
#27032 = CARTESIAN_POINT ( 'NONE',  ( -34.50213009991706059, 434.5101795678424992, 9.485856115010102840 ) ) ;
#27033 = CARTESIAN_POINT ( 'NONE',  ( -82.99743053524834124, -42.97928617255369943, 175.1928188408835751 ) ) ;
#27034 = AXIS2_PLACEMENT_3D ( 'NONE', #78013, #102825, #62378 ) ;
#27035 = ORIENTED_EDGE ( 'NONE', *, *, #80092, .F. ) ;
#27036 = SURFACE_STYLE_USAGE ( .BOTH. , #9726 ) ;
#27037 = ORIENTED_EDGE ( 'NONE', *, *, #64124, .F. ) ;
#27038 = ORIENTED_EDGE ( 'NONE', *, *, #65516, .F. ) ;
#27039 = CARTESIAN_POINT ( 'NONE',  ( 71.63333333333333997, 6.915964383211875250E-15, 0.000000000000000000 ) ) ;
#27040 = FACE_OUTER_BOUND ( 'NONE', #68109, .T. ) ;
#27041 = CYLINDRICAL_SURFACE ( 'NONE', #88775, 1.250000000000001110 ) ;
#27042 = ORIENTED_EDGE ( 'NONE', *, *, #89592, .F. ) ;
#27043 = EDGE_CURVE ( 'NONE', #77685, #60237, #25511, .T. ) ;
#27044 = CARTESIAN_POINT ( 'NONE',  ( -4.250000000000000000, 5.204748896376250699E-16, -9.449444346342716017 ) ) ;
#27045 = DIRECTION ( 'NONE',  ( 0.000000000000000000, 0.000000000000000000, 1.000000000000000000 ) ) ;
#27046 = CARTESIAN_POINT ( 'NONE',  ( 7.151597709147947235, -11.78929265052215847, 3.587174531012139678 ) ) ;
#27047 = CARTESIAN_POINT ( 'NONE',  ( -37.85084083633361729, 438.0234350436313093, 4.171260309356228824 ) ) ;
#27048 = VECTOR ( 'NONE', #70100, 1000.000000000000341 ) ;
#27049 = DIRECTION ( 'NONE',  ( 1.000000000000000000, 1.224606353822377258E-16, 0.000000000000000000 ) ) ;
#27050 = SURFACE_STYLE_FILL_AREA ( #100357 ) ;
#27051 = VECTOR ( 'NONE', #84971, 1000.000000000000000 ) ;
#27052 = CARTESIAN_POINT ( 'NONE',  ( -5.000000000000000000, -14.90044762032552228, 12.47949281813645861 ) ) ;
#27053 = CARTESIAN_POINT ( 'NONE',  ( 104.6755681235317326, -59.99999999999997158, 94.38101796850538960 ) ) ;
#27054 = EDGE_CURVE ( 'NONE', #17355, #57657, #39270, .T. ) ;
#27055 = CARTESIAN_POINT ( 'NONE',  ( -83.90898588706018302, -30.00000000000009592, 196.6629347554013520 ) ) ;
#27056 = CARTESIAN_POINT ( 'NONE',  ( -60.51311341646994890, -39.49057771885277646, 73.58478999695718414 ) ) ;
#27057 = ORIENTED_EDGE ( 'NONE', *, *, #11033, .T. ) ;
#27058 = PRESENTATION_STYLE_ASSIGNMENT (( #68007 ) ) ;
#27059 = ORIENTED_EDGE ( 'NONE', *, *, #75224, .F. ) ;
#27060 = VECTOR ( 'NONE', #94866, 1000.000000000000000 ) ;
#27061 = CARTESIAN_POINT ( 'NONE',  ( -105.1848697628562661, -52.71040872453725967, 177.3350388984402173 ) ) ;
#27062 = SURFACE_STYLE_FILL_AREA ( #26532 ) ;
#27063 = ADVANCED_FACE ( 'NONE', ( #28505 ), #93744, .T. ) ;
#27064 = CARTESIAN_POINT ( 'NONE',  ( 57.70539558375507738, 6.856755485862130937E-15, 0.000000000000000000 ) ) ;
#27065 = CARTESIAN_POINT ( 'NONE',  ( 14.90155535905845952, 42.58002643001236720, -90.01374837836192455 ) ) ;
#27066 = ORIENTED_EDGE ( 'NONE', *, *, #59356, .T. ) ;
#27067 =( NAMED_UNIT ( * ) SI_UNIT ( $, .STERADIAN. ) SOLID_ANGLE_UNIT ( ) );
#27068 = CARTESIAN_POINT ( 'NONE',  ( -78.46824605727127278, -60.00000000000002132, 193.7232304666046900 ) ) ;
#27069 = CARTESIAN_POINT ( 'NONE',  ( -3.352941176470594975, -1.200583151104953616, 104.5794940929807524 ) ) ;
#27070 = CARTESIAN_POINT ( 'NONE',  ( 5.082755093536324154, -21.21875000204838813, 5.082755093536326818 ) ) ;
#27071 = CARTESIAN_POINT ( 'NONE',  ( -1.102002922838543730, 36.52516746709567030, -29.11124182180218511 ) ) ;
#27072 = AXIS2_PLACEMENT_3D ( 'NONE', #1759, #27696, #42228 ) ;
#27073 = DIRECTION ( 'NONE',  ( -0.000000000000000000, 1.000000000000000000, -0.000000000000000000 ) ) ;
#27074 = CARTESIAN_POINT ( 'NONE',  ( 8.099999999999999645, 4.898587196589412829E-16, -4.000000000000000000 ) ) ;
#27075 = CARTESIAN_POINT ( 'NONE',  ( -31.21759734847655210, 387.2566916973277671, 24.99345285570965913 ) ) ;
#27076 = LINE ( 'NONE', #67501, #74450 ) ;
#27077 = CARTESIAN_POINT ( 'NONE',  ( 5.332775234344524939, -8.148154046107340065, 13.71400129111602517 ) ) ;
#27078 = CARTESIAN_POINT ( 'NONE',  ( -5.656854249492379694, -15.12500000409677092, -5.656854249492380582 ) ) ;
#27079 = CARTESIAN_POINT ( 'NONE',  ( 12.13034742782427955, 41.99999999999999289, -93.82352941176471006 ) ) ;
#27080 = CARTESIAN_POINT ( 'NONE',  ( -29.45685281427571311, -32.53887230772507877, 31.71332361860625682 ) ) ;
#27081 = DIRECTION ( 'NONE',  ( 0.000000000000000000, 0.7310552682428690385, 0.6823182503600110360 ) ) ;
#27082 = CARTESIAN_POINT ( 'NONE',  ( 43.41165897559503861, -18.78955090332965483, 36.60811760637851364 ) ) ;
#27083 = DIRECTION ( 'NONE',  ( -1.000000000000000000, -1.224606353822377258E-16, -0.000000000000000000 ) ) ;
#27084 = CARTESIAN_POINT ( 'NONE',  ( -7.800703710507058908, 88.58595692657945619, 1.791736796405269505 ) ) ;
#27085 = CARTESIAN_POINT ( 'NONE',  ( -85.94205773066651943, -38.64533204748195061, 199.0279254153126374 ) ) ;
#27086 = EDGE_LOOP ( 'NONE', ( #47654, #60528, #65878, #27892 ) ) ;
#27088 = CARTESIAN_POINT ( 'NONE',  ( 40.93292669599463096, 378.0706848361106722, 26.55786848468904537 ) ) ;
#27087 = CARTESIAN_POINT ( 'NONE',  ( 84.15948067047270342, -38.35796929636687480, -23.57197301947594781 ) ) ;
#27089 = CARTESIAN_POINT ( 'NONE',  ( -8.786988139152953468E-15, 18.64300841652315910, 38.36521369532682257 ) ) ;
#27090 = CARTESIAN_POINT ( 'NONE',  ( -19.08873399782305569, 49.65827795561243363, 61.75875619398528471 ) ) ;
#27091 = CARTESIAN_POINT ( 'NONE',  ( -7.500000000000007105, 39.99999999999562306, -59.88032989330454825 ) ) ;
#27092 = CARTESIAN_POINT ( 'NONE',  ( 34.90201944348623897, 461.8185193995851137, 3.961962287866056087 ) ) ;
#27093 = DIRECTION ( 'NONE',  ( -1.000000000000000000, -1.224606353822377258E-16, -0.000000000000000000 ) ) ;
#27094 = DIRECTION ( 'NONE',  ( -1.000000000000000000, -1.224606353822377258E-16, -0.000000000000000000 ) ) ;
#27095 = CARTESIAN_POINT ( 'NONE',  ( 4.999999999999993783, -4.000000000000003553, 102.2532056551910387 ) ) ;
#27096 = CARTESIAN_POINT ( 'NONE',  ( 112.1460658327969497, -60.00000000000000711, 168.0038417747363440 ) ) ;
#27097 = DIRECTION ( 'NONE',  ( 1.000000000000000000, 1.224606353822377258E-16, 0.000000000000000000 ) ) ;
#27098 = CARTESIAN_POINT ( 'NONE',  ( 18.86650669486618881, 1.474610560812782335E-15, 0.000000000000000000 ) ) ;
#27099 = EDGE_LOOP ( 'NONE', ( #91132, #39116, #19288, #10208, #85389 ) ) ;
#27100 = SURFACE_STYLE_FILL_AREA ( #2773 ) ;
#27101 = ADVANCED_FACE ( 'NONE', ( #92670 ), #101311, .T. ) ;
#27102 = CARTESIAN_POINT ( 'NONE',  ( -85.26005096827651641, -30.00000000000000711, 59.54443886065791247 ) ) ;
#27103 = ORIENTED_EDGE ( 'NONE', *, *, #60617, .T. ) ;
#27104 = LINE ( 'NONE', #92853, #92383 ) ;
#27105 = CARTESIAN_POINT ( 'NONE',  ( -16.75187969033554936, -1.200000000000000030E-05, -21.80698433968595751 ) ) ;
#27106 =( NAMED_UNIT ( * ) PLANE_ANGLE_UNIT ( ) SI_UNIT ( $, .RADIAN. ) );
#27107 = CARTESIAN_POINT ( 'NONE',  ( 90.51111111111110574, 1.023464760207051730E-14, 0.000000000000000000 ) ) ;
#27108 = CARTESIAN_POINT ( 'NONE',  ( -1.320432766682874540E-15, -16.90625000204838813, 7.188101187500000044 ) ) ;
#27109 = CARTESIAN_POINT ( 'NONE',  ( -3.140974613990812792, -5.000000000000002665, -96.68767211932356531 ) ) ;
#27110 = EDGE_CURVE ( 'NONE', #67362, #24694, #32420, .T. ) ;
#27111 = ADVANCED_FACE ( 'NONE', ( #69473 ), #78082, .T. ) ;
#27112 = DIRECTION ( 'NONE',  ( -1.000000000000000000, -1.224606353822377258E-16, -0.000000000000000000 ) ) ;
#27113 = AXIS2_PLACEMENT_3D ( 'NONE', #42484, #92097, #66227 ) ;
#27114 = ORIENTED_EDGE ( 'NONE', *, *, #31364, .F. ) ;
#27115 = CARTESIAN_POINT ( 'NONE',  ( 83.26238809008557951, -32.54124788460179474, 161.2361585245887170 ) ) ;
#27116 = ADVANCED_FACE ( 'NONE', ( #68413, #76478 ), #75955, .T. ) ;
#27117 = CARTESIAN_POINT ( 'NONE',  ( -3.857142857142855874, -1.200583151104943180, 103.1763305333244318 ) ) ;
#27118 = VECTOR ( 'NONE', #40340, 1000.000000000000114 ) ;
#27119 = CARTESIAN_POINT ( 'NONE',  ( 6.837824896291513355, -3.947820044545448326, -6.564402953523719830 ) ) ;
#27120 = ORIENTED_EDGE ( 'NONE', *, *, #2172, .T. ) ;
#27121 = DIRECTION ( 'NONE',  ( 0.000000000000000000, 0.000000000000000000, 1.000000000000000000 ) ) ;
#27122 = EDGE_CURVE ( 'NONE', #49696, #70900, #34501, .T. ) ;
#27123 = CARTESIAN_POINT ( 'NONE',  ( -4.413590570192279294, -9.188952443232103917, 5.751919616880372566 ) ) ;
#27124 = DIRECTION ( 'NONE',  ( -1.000000000000000000, -1.224606353822377258E-16, -0.000000000000000000 ) ) ;
#27125 = CARTESIAN_POINT ( 'NONE',  ( -4.813668318631113330, 251.7951322982669353, 3.583991016754759062 ) ) ;
#27126 = CARTESIAN_POINT ( 'NONE',  ( -8.000000000000000000, 9.797174393178825657E-16, -25.03750572909317285 ) ) ;
#27127 = FILL_AREA_STYLE_COLOUR ( '', #43445 ) ;
#27128 = VERTEX_POINT ( 'NONE', #100227 ) ;
#27129 = VECTOR ( 'NONE', #62039, 1000.000000000000000 ) ;
#27130 = CIRCLE ( 'NONE', #9823, 4.250000000000000000 ) ;
#27131 = DIRECTION ( 'NONE',  ( 0.000000000000000000, 0.000000000000000000, 1.000000000000000000 ) ) ;
#27132 = CARTESIAN_POINT ( 'NONE',  ( 8.913811505010652780, 18.64284798592881032, 37.38269509653739675 ) ) ;
#27133 = DIRECTION ( 'NONE',  ( 0.000000000000000000, 0.000000000000000000, -1.000000000000000000 ) ) ;
#27134 = CARTESIAN_POINT ( 'NONE',  ( 5.799999999999999822, 0.000000000000000000, 0.000000000000000000 ) ) ;
#27135 = CARTESIAN_POINT ( 'NONE',  ( 7.188101187500000044, -23.65625000204838457, 0.000000000000000000 ) ) ;
#27136 = CONICAL_SURFACE ( 'NONE', #40873, 5.000000000000010658, 0.9599310885968697082 ) ;
#27137 = VECTOR ( 'NONE', #103783, 999.9999999999998863 ) ;
#27138 = CARTESIAN_POINT ( 'NONE',  ( -1.152188841818234133E-13, -1.200000000000000030E-05, -49.25000000000000000 ) ) ;
#27139 = CARTESIAN_POINT ( 'NONE',  ( -14.44768974034976061, 5.957293599826361863, 7.129930386714873336 ) ) ;
#27140 = DIRECTION ( 'NONE',  ( 0.000000000000000000, -1.000000000000000000, 0.000000000000000000 ) ) ;
#27141 = CONTEXT_DEPENDENT_SHAPE_REPRESENTATION ( #27325, #37222 ) ;
#27142 = EDGE_LOOP ( 'NONE', ( #77355, #98300, #83131, #20855, #97682 ) ) ;
#27143 = CARTESIAN_POINT ( 'NONE',  ( -37.50059943756144776, 490.7879993827797307, 12.38039871356719246 ) ) ;
#27144 = VECTOR ( 'NONE', #85786, 1000.000000000000000 ) ;
#27145 = PRESENTATION_STYLE_ASSIGNMENT (( #35224 ) ) ;
#27146 = CARTESIAN_POINT ( 'NONE',  ( -6.019032792335750948, 4.468176404425925341, -5.000000000000000000 ) ) ;
#27147 = TOROIDAL_SURFACE ( 'NONE', #58124, 12.00000000000001066, 3.000000000000000000 ) ;
#27148 = CYLINDRICAL_SURFACE ( 'NONE', #61895, 5.000000000000002665 ) ;
#27149 = ORIENTED_EDGE ( 'NONE', *, *, #594, .F. ) ;
#27150 = CARTESIAN_POINT ( 'NONE',  ( -7.349939847252962011, 52.09173981223236183, -3.136341692644931456 ) ) ;
#27151 = CARTESIAN_POINT ( 'NONE',  ( -8.904581707875109942, 49.99999999999999289, -97.29851715192089046 ) ) ;
#27152 = ADVANCED_FACE ( 'NONE', ( #92133 ), #2055, .F. ) ;
#27153 = CARTESIAN_POINT ( 'NONE',  ( 33.17685491218571769, 435.0131028569089722, 15.11923937554624153 ) ) ;
#27154 = CARTESIAN_POINT ( 'NONE',  ( -5.656854249492381470, -22.25000000409676915, 5.656854249492379694 ) ) ;
#27155 = CIRCLE ( 'NONE', #61559, 5.000000000000010658 ) ;
#27156 = CARTESIAN_POINT ( 'NONE',  ( 16.10302234481879680, 5.501632350609837019, -4.770674012950182785 ) ) ;
#27157 = CARTESIAN_POINT ( 'NONE',  ( 36.31982962151198535, 26.03215893330996522, 12.39505216599222770 ) ) ;
#27158 = CARTESIAN_POINT ( 'NONE',  ( -82.77836920865000536, -60.00000000000002132, 198.6656318658897078 ) ) ;
#27159 = CARTESIAN_POINT ( 'NONE',  ( 9.953339094172397594, 44.05804770646479085, -12.94124162574283510 ) ) ;
#27160 = FACE_OUTER_BOUND ( 'NONE', #78305, .T. ) ;
#27161 = CIRCLE ( 'NONE', #85653, 1.000000000000008660 ) ;
#27162 = CARTESIAN_POINT ( 'NONE',  ( -83.76789176632343015, -50.14492659078340608, 186.2261076651866460 ) ) ;
#27163 = CARTESIAN_POINT ( 'NONE',  ( -4.036264873047459290, 54.13888204563361484, -7.153725211838067644 ) ) ;
#27164 = MECHANICAL_DESIGN_GEOMETRIC_PRESENTATION_REPRESENTATION (  '', ( #21992 ), #73960 ) ;
#27165 = ORIENTED_EDGE ( 'NONE', *, *, #16738, .F. ) ;
#27166 = EDGE_CURVE ( 'NONE', #3430, #21504, #13433, .T. ) ;
#27167 = CARTESIAN_POINT ( 'NONE',  ( 3.558939058151947776, -1.060970281106177859, 104.4181685828942108 ) ) ;
#27168 = CARTESIAN_POINT ( 'NONE',  ( -84.99953569365740691, -52.70058240222559931, 7.104635508431614177 ) ) ;
#27169 = CARTESIAN_POINT ( 'NONE',  ( -4.839353126352284207, 7.222265015501570851, -5.000000000000000000 ) ) ;
#27170 = CARTESIAN_POINT ( 'NONE',  ( 20.64244187944548159, 302.8988018313013413, 9.946989373691105030 ) ) ;
#27171 = DIRECTION ( 'NONE',  ( -1.000000000000000000, -0.000000000000000000, -0.000000000000000000 ) ) ;
#27172 = CARTESIAN_POINT ( 'NONE',  ( -11.85444436786843525, 42.00000000000000000, -90.56128410203886858 ) ) ;
#27174 = VECTOR ( 'NONE', #51286, 1000.000000000000000 ) ;
#27173 = CARTESIAN_POINT ( 'NONE',  ( -9.993576133260312108E-16, 61.49999999999999289, 8.160374191332742555 ) ) ;
#27175 = CARTESIAN_POINT ( 'NONE',  ( 76.24208907273079205, -14.21045842199436571, 145.5826741442930086 ) ) ;
#27176 = CARTESIAN_POINT ( 'NONE',  ( -91.01451176774321539, -60.00000000000003553, -21.65129702257078392 ) ) ;
#27177 = CARTESIAN_POINT ( 'NONE',  ( -73.71532386833389694, -32.54439743916745442, 110.4898480562198415 ) ) ;
#27178 = VERTEX_POINT ( 'NONE', #10154 ) ;
#27179 = CARTESIAN_POINT ( 'NONE',  ( 71.62958147348905413, -29.99999999999999645, 135.6714503744467493 ) ) ;
#27180 = ORIENTED_EDGE ( 'NONE', *, *, #71883, .F. ) ;
#27181 = CARTESIAN_POINT ( 'NONE',  ( 29.86891141250063697, -59.99999999999378275, 45.62306988735215185 ) ) ;
#27182 = ORIENTED_EDGE ( 'NONE', *, *, #2521, .F. ) ;
#27183 = LINE ( 'NONE', #60599, #102640 ) ;
#27184 = CARTESIAN_POINT ( 'NONE',  ( -2.977408999572654480, -27.50000000204838457, 7.188101187499999156 ) ) ;
#27185 = EDGE_CURVE ( 'NONE', #95900, #23394, #80572, .T. ) ;
#27186 = CARTESIAN_POINT ( 'NONE',  ( -5.981691436642410764, -6.027309008058858275, -0.5384679144502708681 ) ) ;
#27187 = ORIENTED_EDGE ( 'NONE', *, *, #43815, .T. ) ;
#27188 = TOROIDAL_SURFACE ( 'NONE', #47840, 6.999999999999999112, 0.5000000000000000000 ) ;
#27189 = ORIENTED_EDGE ( 'NONE', *, *, #11769, .T. ) ;
#27190 = CARTESIAN_POINT ( 'NONE',  ( 5.000000000000000000, 6.123233995736766282E-16, -8.553285714285713937 ) ) ;
#27191 = SURFACE_STYLE_USAGE ( .BOTH. , #35271 ) ;
#27192 = CARTESIAN_POINT ( 'NONE',  ( -28.59280391696366053, -60.00000000000000711, 44.96178721945644696 ) ) ;
#27193 = CARTESIAN_POINT ( 'NONE',  ( 33.26095177349862553, 318.5585020271619783, -6.438101968021065602 ) ) ;
#27194 = CARTESIAN_POINT ( 'NONE',  ( -7.188101187500001821, -15.50000000204838635, -2.977408999572651371 ) ) ;
#27195 = DIRECTION ( 'NONE',  ( 0.000000000000000000, -1.000000000000000000, 0.000000000000000000 ) ) ;
#27196 = LINE ( 'NONE', #19112, #80774 ) ;
#27197 =( NAMED_UNIT ( * ) SI_UNIT ( $, .STERADIAN. ) SOLID_ANGLE_UNIT ( ) );
#27198 = CARTESIAN_POINT ( 'NONE',  ( -5.036189802311375807, 50.00000000000001421, -93.73786388411662074 ) ) ;
#27199 = CARTESIAN_POINT ( 'NONE',  ( -12.49999999999999289, -3.155919820767365547, -14.15697966438807498 ) ) ;
#27200 = CARTESIAN_POINT ( 'NONE',  ( 40.60010613376692845, 436.1985323639532339, 6.054933560615542554 ) ) ;
#27201 = UNCERTAINTY_MEASURE_WITH_UNIT (LENGTH_MEASURE( 1.000000000000000082E-05 ), #35919, 'distance_accuracy_value', 'NONE');
#27202 = VERTEX_POINT ( 'NONE', #59795 ) ;
#27203 = CARTESIAN_POINT ( 'NONE',  ( 5.603804764709383157, -2.702239074867123669, 103.9691152301460875 ) ) ;
#27204 = PRESENTATION_LAYER_ASSIGNMENT (  '', '', ( #73641 ) ) ;
#27205 = VECTOR ( 'NONE', #35004, 1000.000000000000000 ) ;
#27207 = CARTESIAN_POINT ( 'NONE',  ( 32.06800782219411872, -36.02032094391599770, 33.29063352059957026 ) ) ;
#27206 = CARTESIAN_POINT ( 'NONE',  ( -3.423905177083530038, -49.17202489992615000, 103.8439100969724507 ) ) ;
#27208 = CARTESIAN_POINT ( 'NONE',  ( -2.910977163136218682, -8.673617379884035472E-16, 22.23822744035697241 ) ) ;
#27209 = VERTEX_POINT ( 'NONE', #51672 ) ;
#27210 = DIRECTION ( 'NONE',  ( 0.000000000000000000, 0.000000000000000000, 1.000000000000000000 ) ) ;
#27211 = PRODUCT_DEFINITION ( 'UNKNOWN', '', #88740, #92021 ) ;
#27212 = ORIENTED_EDGE ( 'NONE', *, *, #5860, .F. ) ;
#27214 = DIRECTION ( 'NONE',  ( 1.000000000000000000, 1.224606353822377258E-16, 0.000000000000000000 ) ) ;
#27213 = CARTESIAN_POINT ( 'NONE',  ( 26.84999999999999787, 1.533819458162526451E-15, 0.000000000000000000 ) ) ;
#27215 = STYLED_ITEM ( 'NONE', ( #71547 ), #59293 ) ;
#27216 = CARTESIAN_POINT ( 'NONE',  ( 13.48376080047430392, 302.5481724856162487, -10.06453332316872284 ) ) ;
#27217 = CARTESIAN_POINT ( 'NONE',  ( 52.81650669486619165, 6.856755485862130937E-15, 0.000000000000000000 ) ) ;
#27218 = CIRCLE ( 'NONE', #16866, 4.000000000000000888 ) ;
#27219 = CIRCLE ( 'NONE', #30674, 4.000000000000000888 ) ;
#27220 = CARTESIAN_POINT ( 'NONE',  ( 6.249999999999998224, 0.000000000000000000, 0.000000000000000000 ) ) ;
#27221 = CYLINDRICAL_SURFACE ( 'NONE', #72388, 4.000000000000000000 ) ;
#27222 = DIRECTION ( 'NONE',  ( 0.5735764363510491570, -0.8191520442889895781, 1.003171929053522035E-16 ) ) ;
#27223 = VERTEX_POINT ( 'NONE', #10675 ) ;
#27224 = CARTESIAN_POINT ( 'NONE',  ( 92.49443939637855294, -60.00000000000000711, -11.29237403364020409 ) ) ;
#27225 =( NAMED_UNIT ( * ) SI_UNIT ( $, .STERADIAN. ) SOLID_ANGLE_UNIT ( ) );
#27226 = CARTESIAN_POINT ( 'NONE',  ( 38.51282804765381940, 490.3045649923045062, 12.08595093631995532 ) ) ;
#27227 =( BOUNDED_SURFACE ( )  B_SPLINE_SURFACE ( 3, 2, ( 
 ( #87045, #5050, #46562 ),
 ( #13114, #20217, #69267 ),
 ( #29880, #53594, #54624 ),
 ( #13650, #86525, #102140 ),
 ( #104257, #45522, #77344 ),
 ( #21790, #79456, #85437 ),
 ( #70844, #62760, #77877 ),
 ( #3455, #94055, #3989 ),
 ( #28294, #36917, #93536 ),
 ( #5567, #85990, #87565 ),
 ( #61169, #38494, #37983 ),
 ( #11519, #71357, #19682 ),
 ( #12062, #46040, #52521 ),
 ( #4511, #44449, #103736 ),
 ( #44992, #102679, #28840 ),
 ( #78395, #61718, #37449 ),
 ( #20756, #12587, #70318 ),
 ( #103213, #29358, #95133 ),
 ( #21267, #39013, #90206 ),
 ( #106366, #55683, #23373 ) ),
 .UNSPECIFIED., .F., .F., .F. ) 
 B_SPLINE_SURFACE_WITH_KNOTS ( ( 4, 2, 2, 2, 2, 2, 2, 2, 2, 4 ),
 ( 3, 3 ),
 ( -1.480586486746204855E-15, 0.001208125624079908192, 0.002416251248161296970, 0.003624376872242685531, 0.004832502496324074526, 0.005436565308364768589, 0.006040628120405463521, 0.007248753744486852515, 0.008456879368568242378, 0.009665004992649630505 ),
 ( 0.000000000000000000, 1.000000000000000000 ),
 .UNSPECIFIED. ) 
 GEOMETRIC_REPRESENTATION_ITEM ( )  RATIONAL_B_SPLINE_SURFACE ( (
 ( 1.000000000000000000, 0.8291561975891529324, 1.000000000000000000),
 ( 1.000000000000000000, 0.8411444448780550642, 1.000000000000000000),
 ( 1.000000000000000000, 0.8513107778598306696, 1.000000000000000000),
 ( 1.000000000000000000, 0.8686991428046330066, 1.000000000000000000),
 ( 1.000000000000000000, 0.8759367825450403711, 1.000000000000000000),
 ( 1.000000000000000000, 0.8878384569990958042, 1.000000000000000000),
 ( 1.000000000000000000, 0.8925163270236815549, 1.000000000000000000),
 ( 1.000000000000000000, 0.8988019894163230550, 1.000000000000000000),
 ( 1.000000000000000000, 0.9004488336117625336, 1.000000000000000000),
 ( 1.000000000000000000, 0.9004787869545872736, 1.000000000000000000),
 ( 1.000000000000000000, 0.9000741598243027219, 1.000000000000000000),
 ( 1.000000000000000000, 0.8984769429442116540, 1.000000000000000000),
 ( 1.000000000000000000, 0.8972871579692190958, 1.000000000000000000),
 ( 1.000000000000000000, 0.8926126616867483543, 1.000000000000000000),
 ( 1.000000000000000000, 0.8880148073973201939, 1.000000000000000000),
 ( 1.000000000000000000, 0.8760712452964969366, 1.000000000000000000),
 ( 1.000000000000000000, 0.8688049777774786708, 1.000000000000000000),
 ( 1.000000000000000000, 0.8513604698956054317, 1.000000000000000000),
 ( 1.000000000000000000, 0.8411660073558567818, 1.000000000000000000),
 ( 1.000000000000000000, 0.8291561975888496194, 1.000000000000000000) ) ) 
 REPRESENTATION_ITEM ( '' )  SURFACE ( )  );
#27228 = MECHANICAL_DESIGN_GEOMETRIC_PRESENTATION_REPRESENTATION (  '', ( #82294 ), #87478 ) ;
#27229 = FACE_OUTER_BOUND ( 'NONE', #6394, .T. ) ;
#27230 = ORIENTED_EDGE ( 'NONE', *, *, #10407, .T. ) ;
#27231 = AXIS2_PLACEMENT_3D ( 'NONE', #40497, #98195, #64776 ) ;
#27232 = CARTESIAN_POINT ( 'NONE',  ( -103.3985022873205111, -30.00000000000063238, 197.1317429111190904 ) ) ;
#27233 = ORIENTED_EDGE ( 'NONE', *, *, #10371, .F. ) ;
#27234 = ORIENTED_EDGE ( 'NONE', *, *, #66520, .T. ) ;
#27235 = CARTESIAN_POINT ( 'NONE',  ( 7.800703710507058908, 81.41404307342060065, 1.791736796405269061 ) ) ;
#27236 = FILL_AREA_STYLE ('',( #42841 ) ) ;
#27237 = CARTESIAN_POINT ( 'NONE',  ( -16.12443969100768371, 34.43093541110913236, -24.15018447417424241 ) ) ;
#27238 = DIRECTION ( 'NONE',  ( -1.000000000000000000, -1.224606353822377258E-16, -0.000000000000000000 ) ) ;
#27239 = CARTESIAN_POINT ( 'NONE',  ( 83.25497522988638366, -37.81035774849722486, -7.772203072343009111 ) ) ;
#27240 = CARTESIAN_POINT ( 'NONE',  ( -36.72214694598457640, 305.2241286510804912, 0.4044219380610372672 ) ) ;
#27241 = FACE_BOUND ( 'NONE', #88310, .T. ) ;
#27242 = CARTESIAN_POINT ( 'NONE',  ( -17.57685455970505473, 45.00000000000000711, 63.18451563121624304 ) ) ;
#27243 = SURFACE_STYLE_USAGE ( .BOTH. , #103218 ) ;
#27244 = EDGE_LOOP ( 'NONE', ( #99171, #63795, #100668, #97545, #49668 ) ) ;
#27245 = CARTESIAN_POINT ( 'NONE',  ( 6.500000000000000888, 0.000000000000000000, 1.734723475976807094E-15 ) ) ;
#27246 = EDGE_CURVE ( 'NONE', #83606, #77985, #28999, .T. ) ;
#27247 = ORIENTED_EDGE ( 'NONE', *, *, #47748, .F. ) ;
#27248 = CIRCLE ( 'NONE', #77162, 13.50000000000000000 ) ;
#27249 = SURFACE_SIDE_STYLE ('',( #68746 ) ) ;
#27250 = CARTESIAN_POINT ( 'NONE',  ( 0.000000000000000000, 0.000000000000000000, 0.000000000000000000 ) ) ;
#27252 = ORIENTED_EDGE ( 'NONE', *, *, #68744, .F. ) ;
#27251 = CARTESIAN_POINT ( 'NONE',  ( 5.402795611188940583, 41.73472188612398526, -58.79867419242892623 ) ) ;
#27253 = CARTESIAN_POINT ( 'NONE',  ( 72.38549888608767446, -49.90611211077317222, 116.9150284757207174 ) ) ;
#27254 = VERTEX_POINT ( 'NONE', #52204 ) ;
#27255 = CARTESIAN_POINT ( 'NONE',  ( 4.867809078344842888, -47.05361238721339134, 42.73860010202603377 ) ) ;
#27256 = CARTESIAN_POINT ( 'NONE',  ( 6.837824896291513355, -3.947820044545448326, -6.564402953523719830 ) ) ;
#27257 = EDGE_CURVE ( 'NONE', #76134, #80842, #73728, .T. ) ;
#27258 = CARTESIAN_POINT ( 'NONE',  ( -2.977408999572650039, -27.68750000204838457, -7.188101187500000933 ) ) ;
#27259 =( BOUNDED_SURFACE ( )  B_SPLINE_SURFACE ( 3, 2, ( 
 ( #1078, #34054, #25979 ),
 ( #58840, #91733, #69589 ),
 ( #53909, #101935, #13971 ),
 ( #54962, #102479, #86841 ) ),
 .UNSPECIFIED., .F., .F., .F. ) 
 B_SPLINE_SURFACE_WITH_KNOTS ( ( 4, 4 ),
 ( 3, 3 ),
 ( 1.084202172485504434E-18, 0.0009823161607563541970 ),
 ( 0.000000000000000000, 1.000000000000000000 ),
 .UNSPECIFIED. ) 
 GEOMETRIC_REPRESENTATION_ITEM ( )  RATIONAL_B_SPLINE_SURFACE ( (
 ( 1.000000000000000000, 0.9359444767143320076, 1.000000000000000000),
 ( 1.000000000000000000, 0.9457608441872440430, 1.000000000000000000),
 ( 1.000000000000000000, 0.9551386542018457382, 1.000000000000000000),
 ( 1.000000000000000000, 0.9603284238771502279, 1.000000000000000000) ) ) 
 REPRESENTATION_ITEM ( '' )  SURFACE ( )  );
#27260 = ADVANCED_FACE ( 'NONE', ( #21471 ), #77611, .T. ) ;
#27261 = CARTESIAN_POINT ( 'NONE',  ( -100.9355741078537676, -57.67123050614609525, 74.71304529006944506 ) ) ;
#27262 = ORIENTED_EDGE ( 'NONE', *, *, #20920, .T. ) ;
#27263 = CARTESIAN_POINT ( 'NONE',  ( 32.09911992168216699, 438.9232547152094526, 23.66653216045977359 ) ) ;
#27264 = COLOUR_RGB ( '', 0.72549020, 0.75294118, 0.79215686) ;
#27265 = CARTESIAN_POINT ( 'NONE',  ( 104.0818543291210858, -52.71697307696259571, 186.3349087221899367 ) ) ;
#27266 = VECTOR ( 'NONE', #75861, 999.9999999999998863 ) ;
#27267 = CARTESIAN_POINT ( 'NONE',  ( -9.333555687487613994, 83.21897303391028800, 3.591168747312688314 ) ) ;
#27268 = CARTESIAN_POINT ( 'NONE',  ( 48.91297851734898927, 13.22767571191357838, -16.49376885358496736 ) ) ;
#27269 = CARTESIAN_POINT ( 'NONE',  ( 5.656854249492378806, -20.37500000409677270, 5.656854249492381470 ) ) ;
#27270 = CARTESIAN_POINT ( 'NONE',  ( -12.37144696128342147, -4.000000000000003553, 20.44658103856077602 ) ) ;
#27271 = DIRECTION ( 'NONE',  ( 0.5735764363510462704, 0.8191520442889915765, 0.000000000000000000 ) ) ;
#27272 = MECHANICAL_DESIGN_GEOMETRIC_PRESENTATION_REPRESENTATION (  '', ( #28986 ), #6567 ) ;
#27273 = PRESENTATION_STYLE_ASSIGNMENT (( #59609 ) ) ;
#27275 = AXIS2_PLACEMENT_3D ( 'NONE', #94502, #37346, #70208 ) ;
#27274 = B_SPLINE_CURVE_WITH_KNOTS ( 'NONE', 3,
 ( #50148, #68478, #34006, #1580, #66877, #99765, #50652, #27522, #59862, #76542, #9676, #99218, #25934, #67933, #26453, #34541, #58793, #83568 ),
 .UNSPECIFIED., .F., .F.,
 ( 4, 2, 2, 2, 2, 2, 2, 2, 4 ),
 ( 0.007186523243523818515, 0.007691201619852154787, 0.008195879996180491928, 0.008700558372508828200, 0.009205236748837164473, 0.009709915125165500746, 0.01021459350149383702, 0.01071927187782217329, 0.01122395025415050956 ),
 .UNSPECIFIED. ) ;
#27276 = SURFACE_STYLE_FILL_AREA ( #100574 ) ;
#27277 = CARTESIAN_POINT ( 'NONE',  ( 97.47675437802963927, -60.00000000000000000, 196.6138812136176739 ) ) ;
#27278 = DIRECTION ( 'NONE',  ( 0.000000000000000000, 0.000000000000000000, 1.000000000000000000 ) ) ;
#27279 = CARTESIAN_POINT ( 'NONE',  ( 2.625273426274975730, -29.99999999999998934, -7.180406059207282254 ) ) ;
#27280 = ORIENTED_EDGE ( 'NONE', *, *, #57168, .T. ) ;
#27281 = CARTESIAN_POINT ( 'NONE',  ( 43.62838954006723213, 434.9736691849515751, 14.34345830637718322 ) ) ;
#27282 = CARTESIAN_POINT ( 'NONE',  ( 11.99733130325763319, -4.773999631975849312, -12.57663782514914530 ) ) ;
#27283 = CARTESIAN_POINT ( 'NONE',  ( 0.1555636098919296328, 13.68574936779574891, 49.25766232864418726 ) ) ;
#27284 = CARTESIAN_POINT ( 'NONE',  ( -90.30437240975373925, -30.00000000000000000, 190.0991083897584417 ) ) ;
#27285 = ORIENTED_EDGE ( 'NONE', *, *, #54593, .F. ) ;
#27286 = FACE_OUTER_BOUND ( 'NONE', #22459, .T. ) ;
#27287 = VECTOR ( 'NONE', #67871, 1000.000000000000000 ) ;
#27288 = CARTESIAN_POINT ( 'NONE',  ( 85.39600985831239655, -57.56620033426278127, 202.4570461212290695 ) ) ;
#27290 = DIRECTION ( 'NONE',  ( -1.000000000000000000, -1.224606353822377258E-16, -0.000000000000000000 ) ) ;
#27289 = CARTESIAN_POINT ( 'NONE',  ( -14.97535898699339185, 1.269652431127602732, 0.8876819510843543259 ) ) ;
#27291 = ADVANCED_FACE ( 'NONE', ( #5782 ), #69996, .F. ) ;
#27292 = CARTESIAN_POINT ( 'NONE',  ( 72.70106880652396342, -38.32395693884171095, -30.14377858825407230 ) ) ;
#27293 = DIRECTION ( 'NONE',  ( 0.000000000000000000, 0.000000000000000000, -1.000000000000000000 ) ) ;
#27294 = CARTESIAN_POINT ( 'NONE',  ( -32.45631383308813867, -60.00000000000000711, 44.46787372447708009 ) ) ;
#27295 = VECTOR ( 'NONE', #13665, 1000.000000000000000 ) ;
#27296 = B_SPLINE_CURVE_WITH_KNOTS ( 'NONE', 3,
 ( #99112, #27422, #68915, #2552, #61351, #52699, #85625, #53768, #35498, #44095, #93173, #20932 ),
 .UNSPECIFIED., .F., .F.,
 ( 4, 2, 2, 2, 2, 4 ),
 ( 0.000000000000000000, 0.1248429703045113720, 0.2498676475284268006, 0.4999170019762576023, 0.7499663564240884872, 1.000000000000000000 ),
 .UNSPECIFIED. ) ;
#27297 = CARTESIAN_POINT ( 'NONE',  ( -31.61648724296877688, 439.7300051528717972, 23.66942472547106391 ) ) ;
#27298 = CARTESIAN_POINT ( 'NONE',  ( 64.91565662647984425, 48.00000000000000000, 6.815324757469506167 ) ) ;
#27299 = CARTESIAN_POINT ( 'NONE',  ( -86.71180320006325815, -28.07811669808429755, 185.8229765233257922 ) ) ;
#27300 = ORIENTED_EDGE ( 'NONE', *, *, #25650, .T. ) ;
#27301 = CARTESIAN_POINT ( 'NONE',  ( 30.90097930193326192, 13.60840423680625300, 41.14831600716837556 ) ) ;
#27302 = CARTESIAN_POINT ( 'NONE',  ( -2.040435125742793954, -53.40256923005231471, 32.78745887589579411 ) ) ;
#27303 = DIRECTION ( 'NONE',  ( -1.000000000000000000, 0.000000000000000000, 0.000000000000000000 ) ) ;
#27304 = DIRECTION ( 'NONE',  ( 0.000000000000000000, -1.000000000000000000, 0.000000000000000000 ) ) ;
#27307 = EDGE_CURVE ( 'NONE', #85998, #42587, #86730, .T. ) ;
#27306 = CARTESIAN_POINT ( 'NONE',  ( 7.347880794884118356E-15, 0.000000000000000000, -60.00000000000000000 ) ) ;
#27305 = CARTESIAN_POINT ( 'NONE',  ( -38.24569826024678321, 310.6312515531008671, 5.698628603124755720 ) ) ;
#27308 = VERTEX_POINT ( 'NONE', #29572 ) ;
#27309 = CARTESIAN_POINT ( 'NONE',  ( 43.86650669486618881, -3.851859888774471706E-31, 4.000000000000000888 ) ) ;
#27310 = CARTESIAN_POINT ( 'NONE',  ( 38.42890617179530466, 491.4184709533606110, 12.30537189783381358 ) ) ;
#27311 = CIRCLE ( 'NONE', #6528, 3.309500000000007880 ) ;
#27312 = CARTESIAN_POINT ( 'NONE',  ( -4.644767399454820200, -5.000000000000039968, -15.65217902603417066 ) ) ;
#27313 = DIRECTION ( 'NONE',  ( 1.000000000000000000, -0.000000000000000000, -0.000000000000000000 ) ) ;
#27314 = CARTESIAN_POINT ( 'NONE',  ( 17.51243376013908559, 50.00000000000000711, 63.32942081862142913 ) ) ;
#27315 = CARTESIAN_POINT ( 'NONE',  ( 23.95564068939877345, 305.6666757346319514, -9.824255363916352124 ) ) ;
#27316 = PRESENTATION_STYLE_ASSIGNMENT (( #50458 ) ) ;
#27317 = CARTESIAN_POINT ( 'NONE',  ( 0.000000000000000000, 80.00000000000000000, -66.00000000000000000 ) ) ;
#27318 = AXIS2_PLACEMENT_3D ( 'NONE', #70954, #29990, #52631 ) ;
#27319 = CARTESIAN_POINT ( 'NONE',  ( 102.0720237449618679, -14.21045842199434439, 125.2221798637976349 ) ) ;
#27320 = CARTESIAN_POINT ( 'NONE',  ( -78.40731456737989902, -56.84664622636871201, 154.9013258714905987 ) ) ;
#27321 = ORIENTED_EDGE ( 'NONE', *, *, #39572, .F. ) ;
#27322 = CARTESIAN_POINT ( 'NONE',  ( 0.000000000000000000, 0.000000000000000000, 0.000000000000000000 ) ) ;
#27323 = CARTESIAN_POINT ( 'NONE',  ( 5.384233811324318886, 253.0021709134476851, 2.655407383564598156 ) ) ;
#27324 = CARTESIAN_POINT ( 'NONE',  ( 11.32753640269611850, -57.67122862458237620, 41.63783267011080369 ) ) ;
#27325 =( REPRESENTATION_RELATIONSHIP ('NONE','NONE', #69581, #59830 ) REPRESENTATION_RELATIONSHIP_WITH_TRANSFORMATION ( #27680 )SHAPE_REPRESENTATION_RELATIONSHIP( ) );
#27326 = CARTESIAN_POINT ( 'NONE',  ( -7.270302578004622873, -3.659675574298181466, -18.03744543697015956 ) ) ;
#27328 = AXIS2_PLACEMENT_3D ( 'NONE', #39396, #72274, #56057 ) ;
#27327 = CARTESIAN_POINT ( 'NONE',  ( 43.51858057942322944, 326.4877523563876593, -2.294238957344378882 ) ) ;
#27329 = EDGE_CURVE ( 'NONE', #45219, #78511, #73798, .T. ) ;
#27330 = DIRECTION ( 'NONE',  ( -1.000000000000000000, -1.224606353822377258E-16, -0.000000000000000000 ) ) ;
#27331 = ORIENTED_EDGE ( 'NONE', *, *, #80971, .F. ) ;
#27332 = CARTESIAN_POINT ( 'NONE',  ( 0.000000000000000000, 304.8518027762758038, -10.00000000000000178 ) ) ;
#27333 = CARTESIAN_POINT ( 'NONE',  ( 31.75936052488420458, 439.7430734213018013, 23.78634771736264142 ) ) ;
#27334 = ORIENTED_EDGE ( 'NONE', *, *, #102416, .T. ) ;
#27335 = SURFACE_SIDE_STYLE ('',( #20317 ) ) ;
#27337 = ADVANCED_FACE ( 'NONE', ( #38192 ), #52079, .T. ) ;
#27336 = CARTESIAN_POINT ( 'NONE',  ( 3.316968746324327366, 15.92795519102023860, 9.435590127032936536 ) ) ;
#27338 = CARTESIAN_POINT ( 'NONE',  ( 6.764423792815447811, 41.48989066009205118, -70.49176070406230110 ) ) ;
#27339 = CARTESIAN_POINT ( 'NONE',  ( -65.26738680893376454, 49.99999999999999289, 0.8120011905356555593 ) ) ;
#27340 = CARTESIAN_POINT ( 'NONE',  ( 6.019773438520846121, -12.68390881199739439, 12.80591459027740520 ) ) ;
#27342 = CYLINDRICAL_SURFACE ( 'NONE', #23865, 1.250000000000001110 ) ;
#27341 = VECTOR ( 'NONE', #21572, 1000.000000000000000 ) ;
#27343 = VERTEX_POINT ( 'NONE', #100103 ) ;
#27344 = CARTESIAN_POINT ( 'NONE',  ( 0.000000000000000000, 4.898587196589413815E-16, -4.000000000000000888 ) ) ;
#27346 = CARTESIAN_POINT ( 'NONE',  ( 21.89153770144105948, -18.59655829513583214, 27.69837461209327145 ) ) ;
#27345 = CARTESIAN_POINT ( 'NONE',  ( -77.10962715007582347, -30.00000000000002842, 176.8398472105207020 ) ) ;
#27347 = CARTESIAN_POINT ( 'NONE',  ( 1.389906337552808880E-14, 14.17434517210798184, -56.74723269274520021 ) ) ;
#27348 = CARTESIAN_POINT ( 'NONE',  ( 37.34256500486003461, 354.2819331376351215, 1.821034110566981390 ) ) ;
#27349 = CARTESIAN_POINT ( 'NONE',  ( -34.28121086557304409, -32.56895737632404320, 33.60869056487658213 ) ) ;
#27350 = UNCERTAINTY_MEASURE_WITH_UNIT (LENGTH_MEASURE( 1.000000000000000082E-05 ), #52303, 'distance_accuracy_value', 'NONE');
#27351 = ORIENTED_EDGE ( 'NONE', *, *, #57675, .F. ) ;
#27352 = DIRECTION ( 'NONE',  ( -0.000000000000000000, 1.000000000000000000, 0.000000000000000000 ) ) ;
#27353 = DIRECTION ( 'NONE',  ( 0.5735764363510470476, -0.8191520442889911324, 1.003171929053524007E-16 ) ) ;
#27354 = CARTESIAN_POINT ( 'NONE',  ( -14.00172459590632457, -58.00011126645020454, 26.85642925593120722 ) ) ;
#27355 = VECTOR ( 'NONE', #95339, 1000.000000000000000 ) ;
#27356 = CARTESIAN_POINT ( 'NONE',  ( 7.414346147791993857, -62.35410842337736170, -3.010818766110530120 ) ) ;
#27357 = ORIENTED_EDGE ( 'NONE', *, *, #73329, .T. ) ;
#27358 = DIRECTION ( 'NONE',  ( -0.000000000000000000, -0.000000000000000000, -1.000000000000000000 ) ) ;
#27359 = ORIENTED_EDGE ( 'NONE', *, *, #46714, .T. ) ;
#27360 = CARTESIAN_POINT ( 'NONE',  ( 95.05407124332270996, -30.00000000000007461, 191.3402996794985427 ) ) ;
#27361 = CARTESIAN_POINT ( 'NONE',  ( 0.000000000000000000, 0.000000000000000000, 0.000000000000000000 ) ) ;
#27362 = EDGE_CURVE ( 'NONE', #3104, #60267, #91026, .T. ) ;
#27363 = CARTESIAN_POINT ( 'NONE',  ( -4.472135954999579610, -84.72922779932639514, 4.000000000000002665 ) ) ;
#27364 = CARTESIAN_POINT ( 'NONE',  ( 82.29247763371455449, -30.00000000000000000, 36.77940851373791276 ) ) ;
#27365 = CARTESIAN_POINT ( 'NONE',  ( -32.09911992168218831, 438.9232547152092252, 23.66653216045979491 ) ) ;
#27366 = ORIENTED_EDGE ( 'NONE', *, *, #104173, .F. ) ;
#27367 = ORIENTED_EDGE ( 'NONE', *, *, #18949, .T. ) ;
#27368 = ORIENTED_EDGE ( 'NONE', *, *, #74195, .F. ) ;
#27369 = MECHANICAL_DESIGN_GEOMETRIC_PRESENTATION_REPRESENTATION (  '', ( #42778 ), #35988 ) ;
#27370 = DIRECTION ( 'NONE',  ( 1.000000000000000000, -0.000000000000000000, -0.000000000000000000 ) ) ;
#27371 = CARTESIAN_POINT ( 'NONE',  ( -38.47428897412184767, 485.7788508071988645, -4.770630528146724281 ) ) ;
#27372 = DIRECTION ( 'NONE',  ( 1.000000000000000000, 0.000000000000000000, 0.000000000000000000 ) ) ;
#27373 = CIRCLE ( 'NONE', #63517, 1.000000000000000888 ) ;
#27374 = CARTESIAN_POINT ( 'NONE',  ( 5.383284837158156755, -13.00049343515777878, 2.657356347551693698 ) ) ;
#27376 = CIRCLE ( 'NONE', #54861, 4.999999999999999112 ) ;
#27375 = CARTESIAN_POINT ( 'NONE',  ( -31.44965265175576974, 392.5298586342441922, 24.22355757266445053 ) ) ;
#27377 = DIRECTION ( 'NONE',  ( 1.000000000000000000, -0.000000000000000000, -0.000000000000000000 ) ) ;
#27378 = ORIENTED_EDGE ( 'NONE', *, *, #24853, .F. ) ;
#27379 = CARTESIAN_POINT ( 'NONE',  ( -9.739726766105677669, 49.99999999999999289, -82.38252115500968387 ) ) ;
#27380 = VERTEX_POINT ( 'NONE', #45614 ) ;
#27381 = CARTESIAN_POINT ( 'NONE',  ( -4.567209634097050497, -64.06400213914488972, -3.891254717191805046 ) ) ;
#27382 = CARTESIAN_POINT ( 'NONE',  ( 77.51835495759516448, -38.51555964928014930, 186.5383354859341409 ) ) ;
#27383 = CARTESIAN_POINT ( 'NONE',  ( 14.34999999999999787, 1.533819458162526451E-15, 0.000000000000000000 ) ) ;
#27384 = CARTESIAN_POINT ( 'NONE',  ( 22.56285362583756893, 303.3507920709804466, 10.04438543891975577 ) ) ;
#27385 = AXIS2_PLACEMENT_3D ( 'NONE', #23145, #32297, #16618 ) ;
#27386 = CARTESIAN_POINT ( 'NONE',  ( -5.476751506168965555, 246.8364287713300484, -2.461144630687901902 ) ) ;
#27387 = ORIENTED_EDGE ( 'NONE', *, *, #54089, .F. ) ;
#27388 = CARTESIAN_POINT ( 'NONE',  ( -1.308996938995745207, -3.000000000000003553, -95.00000000000000000 ) ) ;
#27389 = CARTESIAN_POINT ( 'NONE',  ( 16.96468291457295052, 45.49948827470971224, -6.626685320826405601 ) ) ;
#27390 = CARTESIAN_POINT ( 'NONE',  ( 30.65126007668194319, 298.3960702967059433, 2.720726122834696170 ) ) ;
#27391 = EDGE_CURVE ( 'NONE', #74620, #5264, #21356, .T. ) ;
#27392 = DIRECTION ( 'NONE',  ( -1.000000000000000000, -0.000000000000000000, -0.000000000000000000 ) ) ;
#27393 = CARTESIAN_POINT ( 'NONE',  ( 15.45341029906007080, 2.829415941283409008, 2.060260514166198931 ) ) ;
#27394 = VERTEX_POINT ( 'NONE', #31042 ) ;
#27395 = AXIS2_PLACEMENT_3D ( 'NONE', #71809, #54551, #29808 ) ;
#27396 = CARTESIAN_POINT ( 'NONE',  ( 7.801642220026312025, -88.58796826149033166, 1.787233835843583751 ) ) ;
#27397 = CARTESIAN_POINT ( 'NONE',  ( -4.022544416453470717, -1.369395410676483849, 103.0357414394656246 ) ) ;
#27398 = CARTESIAN_POINT ( 'NONE',  ( 5.799999999999999822, 0.000000000000000000, 0.000000000000000000 ) ) ;
#27399 = PRESENTATION_LAYER_ASSIGNMENT (  '', '', ( #78996 ) ) ;
#27400 = DIRECTION ( 'NONE',  ( 0.000000000000000000, 1.000000000000000000, 0.000000000000000000 ) ) ;
#27401 = EDGE_CURVE ( 'NONE', #101774, #93942, #55261, .T. ) ;
#27402 = VECTOR ( 'NONE', #30929, 1000.000000000000227 ) ;
#27403 = CARTESIAN_POINT ( 'NONE',  ( -6.944371705245973914, 104.4610030857544984, -3.972324460300566074 ) ) ;
#27404 = CIRCLE ( 'NONE', #87642, 4.000000000000007105 ) ;
#27405 = CARTESIAN_POINT ( 'NONE',  ( 43.99399868442856842, 464.5851102539050999, 10.32278593046345705 ) ) ;
#27406 = CARTESIAN_POINT ( 'NONE',  ( 86.54311645508100526, -24.44606347078198283, 184.2149994208030535 ) ) ;
#27407 = CONICAL_SURFACE ( 'NONE', #1460, 10.39117206796836257, 1.221730476396047926 ) ;
#27408 = CARTESIAN_POINT ( 'NONE',  ( 17.86210361494363141, 36.33998000098823411, -23.65466217301442242 ) ) ;
#27409 = CARTESIAN_POINT ( 'NONE',  ( -8.623093486195200441, 129.1228760232908144, 4.999999999999366729 ) ) ;
#27410 = EDGE_LOOP ( 'NONE', ( #50378, #9846 ) ) ;
#27411 = SURFACE_SIDE_STYLE ('',( #27941 ) ) ;
#27412 = DIRECTION ( 'NONE',  ( -1.000000000000000000, -1.224606353822377258E-16, -0.000000000000000000 ) ) ;
#27413 = CARTESIAN_POINT ( 'NONE',  ( -81.90009874109570376, -30.00000000000000000, 32.92589465123853643 ) ) ;
#27414 = SURFACE_SIDE_STYLE ('',( #93167 ) ) ;
#27415 = CARTESIAN_POINT ( 'NONE',  ( 17.50000000000000711, -2.499999999999999556, 0.000000000000000000 ) ) ;
#27417 = CARTESIAN_POINT ( 'NONE',  ( 17.08544069068336668, 304.5690947107618740, -10.06009145438460983 ) ) ;
#27416 = CARTESIAN_POINT ( 'NONE',  ( -9.699016383038333800, 246.8236182855164600, 2.444973590251029893 ) ) ;
#27418 = EDGE_CURVE ( 'NONE', #45176, #54829, #82434, .T. ) ;
#27419 = CARTESIAN_POINT ( 'NONE',  ( 1.258203773053022889, -53.99999999999999289, 40.95164674802879290 ) ) ;
#27420 = CARTESIAN_POINT ( 'NONE',  ( -41.16595618007350055, -35.63923124053023628, 38.70344113984020140 ) ) ;
#27421 = CARTESIAN_POINT ( 'NONE',  ( 38.95242300084920117, 491.1731620564962668, 12.13306966136837062 ) ) ;
#27422 = CARTESIAN_POINT ( 'NONE',  ( 5.688070444776314183, -4.337726323045820287, -16.91120255682890061 ) ) ;
#27423 = DIRECTION ( 'NONE',  ( -1.000000000000000000, -1.224606353822377258E-16, -0.000000000000000000 ) ) ;
#27424 = CARTESIAN_POINT ( 'NONE',  ( 64.15845098142789027, -29.68239269618735321, -23.41016185180100351 ) ) ;
#27425 = EDGE_CURVE ( 'NONE', #95837, #85235, #87199, .T. ) ;
#27426 = CIRCLE ( 'NONE', #18876, 7.981862520314372489 ) ;
#27427 = CARTESIAN_POINT ( 'NONE',  ( -24.22841651280220887, -56.87824106493767573, 34.54384085670383797 ) ) ;
#27428 = EDGE_LOOP ( 'NONE', ( #42154, #51118, #79452, #47330, #27331, #27038 ) ) ;
#27429 = CARTESIAN_POINT ( 'NONE',  ( 6.969759372139044729, 9.053100120927640049, 0.6630323575263609159 ) ) ;
#27430 = FILL_AREA_STYLE ('',( #101279 ) ) ;
#27431 = CARTESIAN_POINT ( 'NONE',  ( -20.16347608971366867, -39.47721886123265733, 30.99930452457605767 ) ) ;
#27433 = EDGE_CURVE ( 'NONE', #98070, #15534, #46258, .T. ) ;
#27432 = CARTESIAN_POINT ( 'NONE',  ( 0.1682304686574977171, 36.30024107553214918, -29.74999999999999289 ) ) ;
#27434 = ORIENTED_EDGE ( 'NONE', *, *, #39263, .F. ) ;
#27435 = CARTESIAN_POINT ( 'NONE',  ( 0.000000000000000000, 0.000000000000000000, 0.000000000000000000 ) ) ;
#27436 = ORIENTED_EDGE ( 'NONE', *, *, #86024, .F. ) ;
#27437 = DIRECTION ( 'NONE',  ( -1.000000000000000000, -0.000000000000000000, -0.000000000000000000 ) ) ;
#27438 = DIRECTION ( 'NONE',  ( 0.000000000000000000, 1.000000000000000000, -3.755786496842903988E-16 ) ) ;
#27439 = CARTESIAN_POINT ( 'NONE',  ( 4.898587196589412829E-16, -24.31250000409677270, -8.000000000000000000 ) ) ;
#27440 = ORIENTED_EDGE ( 'NONE', *, *, #79054, .T. ) ;
#27441 = DIRECTION ( 'NONE',  ( 0.000000000000000000, 1.000000000000000000, -0.000000000000000000 ) ) ;
#27442 = CONICAL_SURFACE ( 'NONE', #15388, 3.309500000000001663, 0.9599310885968770357 ) ;
#27443 = CARTESIAN_POINT ( 'NONE',  ( 98.96726417907956375, -37.80060191501620181, 191.9129845458357408 ) ) ;
#27445 = CARTESIAN_POINT ( 'NONE',  ( -3.999995229665001428, -8.688226215992830959, 6.928205984420947594 ) ) ;
#27444 = CARTESIAN_POINT ( 'NONE',  ( 9.496329878501317268, 294.6569770103990891, -3.146524261899395825 ) ) ;
#27446 = EDGE_CURVE ( 'NONE', #82852, #63286, #13520, .T. ) ;
#27447 = ORIENTED_EDGE ( 'NONE', *, *, #80414, .F. ) ;
#27448 = ORIENTED_EDGE ( 'NONE', *, *, #25142, .F. ) ;
#27449 = EDGE_LOOP ( 'NONE', ( #64676, #83979, #61838, #87305, #975, #101894, #33292, #45036, #37605 ) ) ;
#27450 = CARTESIAN_POINT ( 'NONE',  ( 24.90254304838390453, 305.8449809694421333, 10.38262587369874268 ) ) ;
#27451 = EDGE_CURVE ( 'NONE', #44416, #32988, #53752, .T. ) ;
#27452 = CARTESIAN_POINT ( 'NONE',  ( -8.000000000000000000, -28.34374999999999289, -3.313708498984762496 ) ) ;
#27453 = DIRECTION ( 'NONE',  ( 1.000000000000000000, 0.000000000000000000, 0.000000000000000000 ) ) ;
#27454 = VERTEX_POINT ( 'NONE', #5664 ) ;
#27455 = DIRECTION ( 'NONE',  ( -0.000000000000000000, -0.000000000000000000, -1.000000000000000000 ) ) ;
#27456 = CARTESIAN_POINT ( 'NONE',  ( -6.821510609914083645, 41.53001914905370029, -70.37925568527511189 ) ) ;
#27457 = LINE ( 'NONE', #60857, #58258 ) ;
#27458 = CARTESIAN_POINT ( 'NONE',  ( -92.79822040692241103, -60.00000000000483169, -18.69254732702162514 ) ) ;
#27459 = DIRECTION ( 'NONE',  ( 0.6293714829493110008, -0.5427490687642032574, -0.5561609342679288970 ) ) ;
#27460 = CARTESIAN_POINT ( 'NONE',  ( -27.57151080649627417, 314.0751515626058676, 12.18133379269485239 ) ) ;
#27461 = CARTESIAN_POINT ( 'NONE',  ( 7.500000000000000888, 1.224646799147353256E-15, -5.000000000000000000 ) ) ;
#27462 = EDGE_CURVE ( 'NONE', #92577, #4111, #4080, .T. ) ;
#27463 = CARTESIAN_POINT ( 'NONE',  ( -84.17958645690445962, -14.21045842199424314, -18.06708323581670328 ) ) ;
#27464 = ADVANCED_FACE ( 'NONE', ( #69878 ), #78969, .T. ) ;
#27465 = CARTESIAN_POINT ( 'NONE',  ( -43.52581800834794024, 465.2717506914920023, 9.360548986731394905 ) ) ;
#27466 = AXIS2_PLACEMENT_3D ( 'NONE', #20658, #29264, #101517 ) ;
#27467 = CARTESIAN_POINT ( 'NONE',  ( -49.42298433514555001, -49.90609790616115049, 53.22976286859889683 ) ) ;
#27468 = EDGE_LOOP ( 'NONE', ( #80322, #35742, #91740, #32919 ) ) ;
#27469 = CARTESIAN_POINT ( 'NONE',  ( -52.56483885390523625, 48.00000000000000000, -38.23529411764706509 ) ) ;
#27470 = VERTEX_POINT ( 'NONE', #86083 ) ;
#27471 = CARTESIAN_POINT ( 'NONE',  ( -8.000000000000000000, -13.24999999999999467, -9.797174393178825657E-16 ) ) ;
#27472 = CARTESIAN_POINT ( 'NONE',  ( -9.609724578342728307, 294.6537309100401671, -2.768030809497829203 ) ) ;
#27473 = CONICAL_SURFACE ( 'NONE', #44618, 4.171999999999999709, 0.7853981633974708165 ) ;
#27474 = CARTESIAN_POINT ( 'NONE',  ( 13.86650669486618881, 1.474610560812782335E-15, 0.000000000000000000 ) ) ;
#27475 = ORIENTED_EDGE ( 'NONE', *, *, #9863, .F. ) ;
#27476 = CARTESIAN_POINT ( 'NONE',  ( 4.696906829037954978, 248.5600185251210519, -3.734050370377327344 ) ) ;
#27477 = B_SPLINE_CURVE_WITH_KNOTS ( 'NONE', 3,
 ( #64936, #39619, #15317, #49264, #106439, #15849 ),
 .UNSPECIFIED., .F., .F.,
 ( 4, 2, 4 ),
 ( 0.003990927807053584568, 0.005983070073873398773, 0.007975212340693213844 ),
 .UNSPECIFIED. ) ;
#27478 = CARTESIAN_POINT ( 'NONE',  ( 68.48188116143754200, -38.33341530762260163, 126.0809973183768307 ) ) ;
#27479 = DIRECTION ( 'NONE',  ( 0.000000000000000000, 0.000000000000000000, 1.000000000000000000 ) ) ;
#27480 = EDGE_CURVE ( 'NONE', #65902, #83087, #22838, .T. ) ;
#27481 = CARTESIAN_POINT ( 'NONE',  ( -1.885326977220364242, -7.100374495473466219, -13.29788260066169414 ) ) ;
#27482 = CARTESIAN_POINT ( 'NONE',  ( 23.57730434126663255, 18.64316884711714906, 30.67950393662606245 ) ) ;
#27483 = CARTESIAN_POINT ( 'NONE',  ( 85.96547421025208280, -30.00000000000000355, 178.3596608991437904 ) ) ;
#27484 = PRODUCT ( '15. Rubber Handle Cover', '15. Rubber Handle Cover', '', ( #76028 ) ) ;
#27485 = CARTESIAN_POINT ( 'NONE',  ( 43.37536761788344819, 434.6169042472851061, 10.05068736165323351 ) ) ;
#27486 = DIRECTION ( 'NONE',  ( 0.000000000000000000, 0.000000000000000000, -1.000000000000000000 ) ) ;
#27488 = B_SPLINE_CURVE_WITH_KNOTS ( 'NONE', 3,
 ( #15360, #39133, #48246, #62874, #87680, #30518 ),
 .UNSPECIFIED., .F., .F.,
 ( 4, 2, 4 ),
 ( 0.000000000000000000, 0.001720022418478405661, 0.003440044836956811323 ),
 .UNSPECIFIED. ) ;
#27487 = CIRCLE ( 'NONE', #43001, 10.00000000000000000 ) ;
#27489 = VERTEX_POINT ( 'NONE', #64960 ) ;
#27490 = VERTEX_POINT ( 'NONE', #8308 ) ;
#27491 = CARTESIAN_POINT ( 'NONE',  ( 51.33239210164947508, -39.50898634762949513, 53.05425396579943254 ) ) ;
#27492 = CARTESIAN_POINT ( 'NONE',  ( 6.578489868540880359, 41.30622290872879887, -58.38226432520261966 ) ) ;
#27493 = CARTESIAN_POINT ( 'NONE',  ( -5.500000000000006217, 42.00000000000000000, -58.69229087761261354 ) ) ;
#27494 = ORIENTED_EDGE ( 'NONE', *, *, #4331, .F. ) ;
#27495 = CARTESIAN_POINT ( 'NONE',  ( -90.54712574570254446, -38.40309215953966770, -14.40705472300955847 ) ) ;
#27496 = AXIS2_PLACEMENT_3D ( 'NONE', #56305, #9352, #31560 ) ;
#27497 = ORIENTED_EDGE ( 'NONE', *, *, #44560, .T. ) ;
#27498 = CARTESIAN_POINT ( 'NONE',  ( 16.14595037866761729, 6.775806037746459509, 6.185188124841393353 ) ) ;
#27499 = CARTESIAN_POINT ( 'NONE',  ( 110.3742243073734812, -38.35605051120794684, 158.9574927243544948 ) ) ;
#27500 = CARTESIAN_POINT ( 'NONE',  ( 10.03715787451029584, 14.00015749138419174, 10.50872311893226296 ) ) ;
#27501 = CARTESIAN_POINT ( 'NONE',  ( 83.05433171731620234, -37.85161955793942923, 27.04821047549421564 ) ) ;
#27502 = CARTESIAN_POINT ( 'NONE',  ( 0.000000000000000000, -99.99999999999997158, 6.000000000000000888 ) ) ;
#27503 = CARTESIAN_POINT ( 'NONE',  ( -26.27395767078098388, 305.7318160080068310, -9.587391517416717690 ) ) ;
#27504 = CARTESIAN_POINT ( 'NONE',  ( 4.293150003526390535, -12.96978500885370345, -9.455099716441868196 ) ) ;
#27505 = CARTESIAN_POINT ( 'NONE',  ( -23.97745264537545040, 25.74979706031962579, -30.95109073255507326 ) ) ;
#27506 = SURFACE_STYLE_FILL_AREA ( #68460 ) ;
#27507 = CARTESIAN_POINT ( 'NONE',  ( 8.642300018713374499, 129.6053270932821135, -6.133294652287071463E-13 ) ) ;
#27508 = ORIENTED_EDGE ( 'NONE', *, *, #84282, .T. ) ;
#27509 = ADVANCED_FACE ( 'NONE', ( #25059 ), #70361, .T. ) ;
#27510 = CARTESIAN_POINT ( 'NONE',  ( 0.7847972972063655961, 36.39241504557466556, 29.48654454112834244 ) ) ;
#27511 = LINE ( 'NONE', #20500, #99484 ) ;
#27512 = DIRECTION ( 'NONE',  ( -1.000000000000000000, -1.224606353822377258E-16, -0.000000000000000000 ) ) ;
#27513 = ORIENTED_EDGE ( 'NONE', *, *, #43704, .F. ) ;
#27514 = DIRECTION ( 'NONE',  ( -1.000000000000000000, -1.224606353822377258E-16, -0.000000000000000000 ) ) ;
#27515 = CARTESIAN_POINT ( 'NONE',  ( -30.71792534725271651, 320.3613057377743303, 14.24394111771609950 ) ) ;
#27516 = CARTESIAN_POINT ( 'NONE',  ( -3.672464763049774796E-06, -18.02989419364509516, 35.00496915990722613 ) ) ;
#27517 = CARTESIAN_POINT ( 'NONE',  ( 17.33349330513380337, 4.898587196589405926E-16, -4.000000000000001776 ) ) ;
#27518 = CARTESIAN_POINT ( 'NONE',  ( -8.000000000000001776, -20.65624999999998934, 3.313708498984758943 ) ) ;
#27519 = CARTESIAN_POINT ( 'NONE',  ( -48.22718221699823005, -29.29832994236101484, 43.93128805990089347 ) ) ;
#27520 = ADVANCED_FACE ( 'NONE', ( #32084 ), #14269, .F. ) ;
#27521 = CIRCLE ( 'NONE', #17097, 1.000000000000000888 ) ;
#27522 = CARTESIAN_POINT ( 'NONE',  ( 15.43434203115574377, 44.00353298636623123, -5.764138573818327949 ) ) ;
#27523 = ORIENTED_EDGE ( 'NONE', *, *, #14441, .F. ) ;
#27524 = CARTESIAN_POINT ( 'NONE',  ( 82.99625799389046676, -60.91576764804962352, 190.5939014586151643 ) ) ;
#27525 = CARTESIAN_POINT ( 'NONE',  ( -27.99999999999999645, 0.000000000000000000, 0.000000000000000000 ) ) ;
#27526 = CARTESIAN_POINT ( 'NONE',  ( -86.73809324249754127, -41.71369293968039926, 189.2643421761773936 ) ) ;
#27527 = VERTEX_POINT ( 'NONE', #66552 ) ;
#27528 = CARTESIAN_POINT ( 'NONE',  ( -94.35836587452192248, -45.26550033706196530, 96.73288487592235185 ) ) ;
#27529 = CARTESIAN_POINT ( 'NONE',  ( 34.42407431220851066, 0.000000000000000000, 5.000000000000002665 ) ) ;
#27530 = DIRECTION ( 'NONE',  ( -0.8660254037844371533, -0.5000000000000025535, 0.000000000000000000 ) ) ;
#27531 = DIRECTION ( 'NONE',  ( 0.000000000000000000, 0.000000000000000000, 1.000000000000000000 ) ) ;
#27532 = CARTESIAN_POINT ( 'NONE',  ( -27.71163250425533420, -28.72695625282879561, -38.27699728131180024 ) ) ;
#27533 = ADVANCED_FACE ( 'NONE', ( #66019, #98899 ), #31564, .F. ) ;
#27534 = SURFACE_STYLE_USAGE ( .BOTH. , #61470 ) ;
#27535 = CIRCLE ( 'NONE', #99857, 4.000000000000007105 ) ;
#27536 = CARTESIAN_POINT ( 'NONE',  ( 41.13664993942406767, -60.00000000000000000, 53.77317075040697603 ) ) ;
#27537 = CARTESIAN_POINT ( 'NONE',  ( 34.91252575250545931, -35.46210594863769217, 44.14912163742516071 ) ) ;
#27538 = DIRECTION ( 'NONE',  ( -1.000000000000000000, -0.000000000000000000, -0.000000000000000000 ) ) ;
#27539 = CARTESIAN_POINT ( 'NONE',  ( 17.70630566656853233, -16.17175919650291505, 31.52307540510448192 ) ) ;
#27541 = CARTESIAN_POINT ( 'NONE',  ( -10.81517053142260210, 16.02938924181589897, 9.536203003419373658 ) ) ;
#27540 = CARTESIAN_POINT ( 'NONE',  ( -2.499999999999996447, -10.61161683768976083, -19.67321569086711364 ) ) ;
#27542 = CARTESIAN_POINT ( 'NONE',  ( 1.487796992647206995, 297.5563421047799579, -10.00151720974370129 ) ) ;
#27543 = CARTESIAN_POINT ( 'NONE',  ( 42.09210974227526947, 317.4093497706929270, -4.557617623460385126 ) ) ;
#27544 = CARTESIAN_POINT ( 'NONE',  ( 39.24609676134105030, 311.8013972301173453, 2.046850167889632921 ) ) ;
#27545 = CARTESIAN_POINT ( 'NONE',  ( 0.000000000000000000, 4.898587196589413815E-16, -4.000000000000000888 ) ) ;
#27546 = AXIS2_PLACEMENT_3D ( 'NONE', #66417, #100905, #59956 ) ;
#27547 = EDGE_LOOP ( 'NONE', ( #95971, #75692, #46122, #29223 ) ) ;
#27548 = CARTESIAN_POINT ( 'NONE',  ( -43.85205561063334301, 464.7392644986606456, 11.03676161964631319 ) ) ;
#27549 = CARTESIAN_POINT ( 'NONE',  ( -1.758251042101240058, -60.00000000000000000, 39.63689313157515670 ) ) ;
#27550 = VERTEX_POINT ( 'NONE', #106467 ) ;
#27551 = DIRECTION ( 'NONE',  ( 0.4753313241819922541, 0.2469313775204109718, -0.8444436198155955697 ) ) ;
#27552 = CARTESIAN_POINT ( 'NONE',  ( 4.699999999999999289, 0.000000000000000000, 6.499999999999999112 ) ) ;
#27553 = LINE ( 'NONE', #99794, #26912 ) ;
#27554 =( BOUNDED_SURFACE ( )  B_SPLINE_SURFACE ( 3, 2, ( 
 ( #104492, #63528, #80211 ),
 ( #55399, #88330, #72131 ),
 ( #105040, #31181, #23074 ),
 ( #14942, #47836, #80743 ),
 ( #6858, #106616, #82346 ),
 ( #49973, #82881, #1406 ),
 ( #8979, #34372, #48897 ),
 ( #8454, #25759, #58617 ) ),
 .UNSPECIFIED., .F., .F., .T. ) 
 B_SPLINE_SURFACE_WITH_KNOTS ( ( 4, 2, 2, 4 ),
 ( 3, 3 ),
 ( 0.009824648773345148398, 0.02000824059645995093, 0.02510003650801735306, 0.03019183241957475519 ),
 ( 0.000000000000000000, 1.000000000000000000 ),
 .UNSPECIFIED. ) 
 GEOMETRIC_REPRESENTATION_ITEM ( )  RATIONAL_B_SPLINE_SURFACE ( (
 ( 1.000000000000000000, 0.7071067811865475727, 1.000000000000000000),
 ( 1.000000000000000000, 0.7071067811865475727, 1.000000000000000000),
 ( 1.000000000000000000, 0.7071080532101867711, 1.000000000000000000),
 ( 1.000000000000000000, 0.7071061931969254699, 1.000000000000000000),
 ( 1.000000000000000000, 0.7071074416173600552, 1.000000000000000000),
 ( 1.000000000000000000, 0.7071061821613239262, 1.000000000000000000),
 ( 1.000000000000000000, 0.7071482299271628635, 1.000000000000000000),
 ( 1.000000000000000000, 0.7071067811865643371, 1.000000000000000000) ) ) 
 REPRESENTATION_ITEM ( '' )  SURFACE ( )  );
#27555 = CIRCLE ( 'NONE', #44854, 12.50000000000000000 ) ;
#27558 = EDGE_CURVE ( 'NONE', #81048, #75857, #82736, .T. ) ;
#27557 = CARTESIAN_POINT ( 'NONE',  ( -6.444268991759913412, -60.22817020191458681, -36.83317943627129409 ) ) ;
#27556 = CARTESIAN_POINT ( 'NONE',  ( 9.333079356992124431, 251.7783308007486198, 3.592383266237774375 ) ) ;
#27559 = EDGE_LOOP ( 'NONE', ( #98012, #84254 ) ) ;
#27560 = CARTESIAN_POINT ( 'NONE',  ( 0.000000000000000000, -80.00000000000000000, 27.00000000000000000 ) ) ;
#27561 = DIRECTION ( 'NONE',  ( 0.000000000000000000, -1.000000000000000000, 0.000000000000000000 ) ) ;
#27562 = ORIENTED_EDGE ( 'NONE', *, *, #7614, .F. ) ;
#27563 = CARTESIAN_POINT ( 'NONE',  ( 0.000000000000000000, 79.50000000000000000, 0.000000000000000000 ) ) ;
#27564 = CARTESIAN_POINT ( 'NONE',  ( 0.000000000000000000, 0.000000000000000000, -13.00000000000000000 ) ) ;
#27565 = VECTOR ( 'NONE', #15358, 1000.000000000000000 ) ;
#27566 = PRESENTATION_STYLE_ASSIGNMENT (( #76055 ) ) ;
#27567 = CARTESIAN_POINT ( 'NONE',  ( -92.04245549561946405, -60.00000000000000000, 19.36274040525862006 ) ) ;
#27568 = CARTESIAN_POINT ( 'NONE',  ( 28.99999999999999645, 0.000000000000000000, 0.000000000000000000 ) ) ;
#27569 = SURFACE_STYLE_USAGE ( .BOTH. , #94935 ) ;
#27570 = PRESENTATION_STYLE_ASSIGNMENT (( #100340 ) ) ;
#27572 =( LENGTH_UNIT ( ) NAMED_UNIT ( * ) SI_UNIT ( .MILLI., .METRE. ) );
#27571 = CARTESIAN_POINT ( 'NONE',  ( 7.996668422911924701, -3.000000000000002665, -78.85453279918097280 ) ) ;
#27573 = VECTOR ( 'NONE', #7219, 1000.000000000000000 ) ;
#27574 = CARTESIAN_POINT ( 'NONE',  ( -85.62098330289637715, -21.92300381590476732, 167.5840582116480562 ) ) ;
#27575 = EDGE_LOOP ( 'NONE', ( #36638, #45448, #34595, #84513 ) ) ;
#27576 = DIRECTION ( 'NONE',  ( 0.2039034312721268727, 0.2189633091458398073, 0.9541899496239500955 ) ) ;
#27577 = EDGE_LOOP ( 'NONE', ( #25178, #18606, #39054, #97855, #73856, #105474, #61317 ) ) ;
#27578 = ORIENTED_EDGE ( 'NONE', *, *, #100772, .F. ) ;
#27579 = CARTESIAN_POINT ( 'NONE',  ( 0.000000000000000000, 0.000000000000000000, 0.000000000000000000 ) ) ;
#27580 = CARTESIAN_POINT ( 'NONE',  ( -14.24124568368173094, -4.332661967058738739, -11.33228852116109842 ) ) ;
#27581 = EDGE_CURVE ( 'NONE', #82621, #26618, #10067, .T. ) ;
#27582 = ORIENTED_EDGE ( 'NONE', *, *, #84280, .T. ) ;
#27583 = FILL_AREA_STYLE_COLOUR ( '', #39273 ) ;
#27584 = CARTESIAN_POINT ( 'NONE',  ( -88.38279035983548226, -57.66943555457145720, -24.13713039724196818 ) ) ;
#27585 = DIRECTION ( 'NONE',  ( 0.000000000000000000, 0.000000000000000000, 1.000000000000000000 ) ) ;
#27586 = CARTESIAN_POINT ( 'NONE',  ( -1.053783150697139126, 13.98491295135151447, 6.925164142196040373 ) ) ;
#27587 = CARTESIAN_POINT ( 'NONE',  ( -9.537927238823506570, 102.3537314288182074, -3.010735687602419386 ) ) ;
#27588 = DIRECTION ( 'NONE',  ( 0.000000000000000000, -1.000000000000000000, 0.000000000000000000 ) ) ;
#27589 = CARTESIAN_POINT ( 'NONE',  ( 1.464720647026959308E-15, 47.77514352166374323, 11.96035173608223090 ) ) ;
#27590 = CARTESIAN_POINT ( 'NONE',  ( 91.01367250360885919, -30.00000000000005684, 38.60059757395459457 ) ) ;
#27591 = EDGE_CURVE ( 'NONE', #39998, #5468, #37674, .T. ) ;
#27592 = CARTESIAN_POINT ( 'NONE',  ( -81.10703223160209063, -14.21045842199456288, 192.6080781080067652 ) ) ;
#27593 = CARTESIAN_POINT ( 'NONE',  ( -58.97854848860931298, -53.38957946420630662, 76.08090858395418365 ) ) ;
#27594 = EDGE_LOOP ( 'NONE', ( #67751, #17113, #90300, #38816, #74497 ) ) ;
#27595 = CARTESIAN_POINT ( 'NONE',  ( 6.481635180341071667, 16.00630266284368730, 2.650895967029502476 ) ) ;
#27596 = ORIENTED_EDGE ( 'NONE', *, *, #70152, .F. ) ;
#27597 = CARTESIAN_POINT ( 'NONE',  ( -106.4199118972464788, -60.15533903948110606, 177.4979064205827513 ) ) ;
#27598 =( LENGTH_UNIT ( ) NAMED_UNIT ( * ) SI_UNIT ( .MILLI., .METRE. ) );
#27599 = SURFACE_STYLE_USAGE ( .BOTH. , #69618 ) ;
#27600 = B_SPLINE_CURVE_WITH_KNOTS ( 'NONE', 3,
 ( #31199, #23096, #12313, #30120, #45239, #4233, #78119, #37168, #70029, #102931 ),
 .UNSPECIFIED., .F., .F.,
 ( 4, 2, 2, 2, 4 ),
 ( 0.000000000000000000, 0.001026607246098428655, 0.002053214492196857310, 0.003079821738295285966, 0.004106428984393714621 ),
 .UNSPECIFIED. ) ;
#27601 = SURFACE_SIDE_STYLE ('',( #91764 ) ) ;
#27602 = ORIENTED_EDGE ( 'NONE', *, *, #43391, .T. ) ;
#27603 = CARTESIAN_POINT ( 'NONE',  ( 7.758748231342716295, -5.000000000000001776, -73.00623724565090811 ) ) ;
#27604 = CARTESIAN_POINT ( 'NONE',  ( -10.51296777078104050, 50.00000000000000000, -92.64705882352942012 ) ) ;
#27605 = CARTESIAN_POINT ( 'NONE',  ( 5.082755093536325930, -11.84375000204838635, -5.082755093536325042 ) ) ;
#27606 = EDGE_CURVE ( 'NONE', #89753, #67545, #73028, .T. ) ;
#27607 = CARTESIAN_POINT ( 'NONE',  ( 30.00000000000000000, 0.000000000000000000, 15.00000000000000000 ) ) ;
#27608 = CARTESIAN_POINT ( 'NONE',  ( 30.11650669486618881, 4.000000000000003553, 4.898587196589414801E-16 ) ) ;
#27609 = CARTESIAN_POINT ( 'NONE',  ( 4.898587196589412829E-16, -10.62499999999999289, -8.000000000000000000 ) ) ;
#27610 = CARTESIAN_POINT ( 'NONE',  ( -22.91885868373643831, 305.6172567281201964, 10.10309701371861912 ) ) ;
#27611 = SURFACE_STYLE_FILL_AREA ( #84209 ) ;
#27612 = CARTESIAN_POINT ( 'NONE',  ( 6.407477497206921058, -15.51226555635960480, 14.54000465036871503 ) ) ;
#27613 = CARTESIAN_POINT ( 'NONE',  ( -31.71665931334666055, -53.38053263592674114, 36.28720432217011904 ) ) ;
#27614 = CONICAL_SURFACE ( 'NONE', #101641, 3.309500000000001663, 0.9599310885968770357 ) ;
#27615 = CARTESIAN_POINT ( 'NONE',  ( 33.00000000000000000, 485.0303364503728289, 0.9535057477322557151 ) ) ;
#27616 = UNCERTAINTY_MEASURE_WITH_UNIT (LENGTH_MEASURE( 1.000000000000000082E-05 ), #65958, 'distance_accuracy_value', 'NONE');
#27617 = CARTESIAN_POINT ( 'NONE',  ( 45.30861358563132057, -22.24403561376615812, 39.34052521140961289 ) ) ;
#27618 = CARTESIAN_POINT ( 'NONE',  ( -32.80261435968446904, 487.0248074981827244, 8.977354182202281763 ) ) ;
#27619 = CARTESIAN_POINT ( 'NONE',  ( 11.28790243858420084, 9.071383756617068528, -0.5355294694855753379 ) ) ;
#27620 = CARTESIAN_POINT ( 'NONE',  ( -97.97456883874956191, -38.48009392417085195, 200.9861677195517586 ) ) ;
#27621 = ORIENTED_EDGE ( 'NONE', *, *, #18093, .T. ) ;
#27623 = DIRECTION ( 'NONE',  ( 0.000000000000000000, 0.2013748291391406209, 0.9795142562460140701 ) ) ;
#27622 = CARTESIAN_POINT ( 'NONE',  ( -16.13488272710901583, 21.13099985707890127, -3.419103882786595605 ) ) ;
#27624 = CARTESIAN_POINT ( 'NONE',  ( 57.46228475329571239, -59.99999999999999289, 75.03564804614198636 ) ) ;
#27625 = CARTESIAN_POINT ( 'NONE',  ( -48.49185632690704750, 10.49696353563009055, -14.43858684427239325 ) ) ;
#27626 = CARTESIAN_POINT ( 'NONE',  ( -7.133125787874796231, 41.57692897371567398, -59.23559257119363508 ) ) ;
#27627 = CARTESIAN_POINT ( 'NONE',  ( 4.910934285265537547, 41.41789230214733664, -70.63711736860776114 ) ) ;
#27628 = DIRECTION ( 'NONE',  ( 0.000000000000000000, -1.000000000000000000, 0.000000000000000000 ) ) ;
#27629 = DIRECTION ( 'NONE',  ( -0.000000000000000000, -0.000000000000000000, -1.000000000000000000 ) ) ;
#27630 = CARTESIAN_POINT ( 'NONE',  ( 32.48439440699409886, 435.0131534033402545, 18.09282574846879044 ) ) ;
#27631 = CARTESIAN_POINT ( 'NONE',  ( 111.6052588162456516, -60.00000000000000711, 183.6789224556778208 ) ) ;
#27632 = CIRCLE ( 'NONE', #87870, 7.000000000000000000 ) ;
#27633 = CARTESIAN_POINT ( 'NONE',  ( 0.000000000000000000, 0.000000000000000000, -10.00000000000000000 ) ) ;
#27634 = CIRCLE ( 'NONE', #93112, 3.400000000000000355 ) ;
#27635 = ORIENTED_EDGE ( 'NONE', *, *, #48127, .T. ) ;
#27636 = EDGE_CURVE ( 'NONE', #33315, #53479, #47239, .T. ) ;
#27637 = CARTESIAN_POINT ( 'NONE',  ( 3.035724950089529361, -49.45330424012770720, 103.2067224559505974 ) ) ;
#27638 = CARTESIAN_POINT ( 'NONE',  ( -84.13737281345436259, -29.99999999999997158, 51.97699099161796710 ) ) ;
#27639 = VERTEX_POINT ( 'NONE', #68152 ) ;
#27640 = AXIS2_PLACEMENT_3D ( 'NONE', #22747, #30841, #70737 ) ;
#27642 = DIRECTION ( 'NONE',  ( -1.000000000000000000, -1.224606353822377258E-16, -0.000000000000000000 ) ) ;
#27641 = CARTESIAN_POINT ( 'NONE',  ( -86.79134504753260160, -38.60262278463063979, 199.4600156365133614 ) ) ;
#27643 = CARTESIAN_POINT ( 'NONE',  ( 46.00000000000000711, 437.8938411292168666, 13.38357595664191813 ) ) ;
#27644 = DIRECTION ( 'NONE',  ( 1.000000000000000000, 0.000000000000000000, -0.000000000000000000 ) ) ;
#27645 = CARTESIAN_POINT ( 'NONE',  ( 9.333079356992101339, 28.22166919925128425, 3.592383266237780592 ) ) ;
#27646 = CARTESIAN_POINT ( 'NONE',  ( 2.977408999572650927, -17.75000000204838457, -7.188101187500001821 ) ) ;
#27647 = CARTESIAN_POINT ( 'NONE',  ( 6.043427762771891310, -5.000000000000002665, -74.51456333905348117 ) ) ;
#27648 = EDGE_CURVE ( 'NONE', #7449, #42837, #36391, .T. ) ;
#27649 = ADVANCED_FACE ( 'NONE', ( #85404 ), #69689, .T. ) ;
#27650 = AXIS2_PLACEMENT_3D ( 'NONE', #52396, #26065, #60003 ) ;
#27651 = UNCERTAINTY_MEASURE_WITH_UNIT (LENGTH_MEASURE( 1.000000000000000082E-05 ), #95144, 'distance_accuracy_value', 'NONE');
#27652 = CARTESIAN_POINT ( 'NONE',  ( 102.6464385083043283, -5.000000000000000888, 6.123233995736779101E-16 ) ) ;
#27654 = ORIENTED_EDGE ( 'NONE', *, *, #13559, .F. ) ;
#27653 = CARTESIAN_POINT ( 'NONE',  ( -38.81331594050915612, 485.4121048083255232, -4.285540015901212030 ) ) ;
#27655 = CARTESIAN_POINT ( 'NONE',  ( 80.23453759376155858, -56.87460238040762306, 171.5698434726804464 ) ) ;
#27656 = AXIS2_PLACEMENT_3D ( 'NONE', #90812, #24515, #80571 ) ;
#27657 = CARTESIAN_POINT ( 'NONE',  ( -46.00000000000000000, 459.9277931459674278, 6.461582622316496938 ) ) ;
#27658 = FACE_BOUND ( 'NONE', #17099, .T. ) ;
#27659 = ORIENTED_EDGE ( 'NONE', *, *, #97404, .F. ) ;
#27660 = CARTESIAN_POINT ( 'NONE',  ( 57.70539558375507738, 4.898587196589294500E-16, -4.000000000000007105 ) ) ;
#27661 = FILL_AREA_STYLE ('',( #33596 ) ) ;
#27662 = CARTESIAN_POINT ( 'NONE',  ( 1.049032378833995693, 6.899894373156700844, -0.3607371497494533674 ) ) ;
#27663 = CARTESIAN_POINT ( 'NONE',  ( 20.00000000000000000, 12.99999999999999289, 0.000000000000000000 ) ) ;
#27664 = CARTESIAN_POINT ( 'NONE',  ( -42.61140200160144786, 465.9030374194822457, 13.21253569360411895 ) ) ;
#27665 = CARTESIAN_POINT ( 'NONE',  ( 8.413542354226143161, -1.106381881529997724, 15.48637553561542113 ) ) ;
#27666 = ADVANCED_FACE ( 'NONE', ( #101046 ), #67631, .T. ) ;
#27667 = ORIENTED_EDGE ( 'NONE', *, *, #30862, .T. ) ;
#27668 = UNCERTAINTY_MEASURE_WITH_UNIT (LENGTH_MEASURE( 1.000000000000000082E-05 ), #101104, 'distance_accuracy_value', 'NONE');
#27669 = DIRECTION ( 'NONE',  ( -1.000000000000000000, -1.224606353822377258E-16, -0.000000000000000000 ) ) ;
#27670 = AXIS2_PLACEMENT_3D ( 'NONE', #36170, #20537, #93304 ) ;
#27671 = CARTESIAN_POINT ( 'NONE',  ( -5.000000000000000888, -68.69775162920400646, 12.24814655256842855 ) ) ;
#27673 = EDGE_CURVE ( 'NONE', #17858, #37257, #80665, .T. ) ;
#27672 = CARTESIAN_POINT ( 'NONE',  ( 86.62318117064180001, -60.99931462043210928, 194.7255943711274426 ) ) ;
#27674 = CARTESIAN_POINT ( 'NONE',  ( 42.83167223033138526, 435.5834305853641695, 17.69761675603227857 ) ) ;
#27675 = CARTESIAN_POINT ( 'NONE',  ( -5.082755093536326818, -25.71875000204838813, 5.082755093536325042 ) ) ;
#27676 = CARTESIAN_POINT ( 'NONE',  ( -41.74378088170519874, 488.3362766135676338, 9.453202772108019403 ) ) ;
#27677 = LINE ( 'NONE', #12489, #10439 ) ;
#27678 = CARTESIAN_POINT ( 'NONE',  ( 41.91039677604278069, 435.8602217528023743, 20.32597409357570584 ) ) ;
#27679 = B_SPLINE_CURVE_WITH_KNOTS ( 'NONE', 3,
 ( #56416, #15440, #106031, #7342, #32176, #59643, #84443, #59110, #34327, #35933, #61238, #11057, #10009, #18673, #52057, #10536, #68259, #43453, #84972, #26772, #94122, #67203, #43980, #100079, #20288, #42374, #50983, #26246, #69332, #60715 ),
 .UNSPECIFIED., .F., .F.,
 ( 4, 2, 2, 2, 2, 2, 2, 2, 2, 2, 2, 2, 2, 2, 4 ),
 ( 0.01451434872829001493, 0.01497952839231827919, 0.01521211822433241566, 0.01544470805634655386, 0.01567729788836069033, 0.01590988772037483026, 0.01637506738440308585, 0.01684024704843134143, 0.01730542671245959702, 0.01823578604051610125, 0.01916614536857260548, 0.02009650469662910624, 0.02102686402468561047, 0.02149204368871385912, 0.02195722335274210429 ),
 .UNSPECIFIED. ) ;
#27680 = ITEM_DEFINED_TRANSFORMATION ( 'NONE', 'NONE', #36958,  #10728 ) ;
#27681 = VERTEX_POINT ( 'NONE', #50353 ) ;
#27682 = CARTESIAN_POINT ( 'NONE',  ( 23.86650669486618881, 1.474610560812782335E-15, 0.000000000000000000 ) ) ;
#27683 = DIRECTION ( 'NONE',  ( -0.5735764363510497121, 0.8191520442889892450, 1.003171929053521665E-16 ) ) ;
#27684 = CARTESIAN_POINT ( 'NONE',  ( -5.918835035098597430, 4.611273631704160714, -4.999999999999999112 ) ) ;
#27685 = AXIS2_PLACEMENT_3D ( 'NONE', #34103, #91778, #74509 ) ;
#27686 = VERTEX_POINT ( 'NONE', #19115 ) ;
#27687 = CARTESIAN_POINT ( 'NONE',  ( 5.656854249492378806, -17.18749999999999289, 5.656854249492381470 ) ) ;
#27688 = CARTESIAN_POINT ( 'NONE',  ( -34.49820706003161064, 464.8461132930464714, 18.22442427693934519 ) ) ;
#27689 = CARTESIAN_POINT ( 'NONE',  ( 32.70848551668328952, 434.6726260045710433, 17.17137052634237193 ) ) ;
#27690 = CARTESIAN_POINT ( 'NONE',  ( 68.45015997180047407, 6.975173280561618775E-15, 0.000000000000000000 ) ) ;
#27691 = CARTESIAN_POINT ( 'NONE',  ( 9.536842176398144133, 102.3576463011601021, 3.014135744008186180 ) ) ;
#27692 = UNCERTAINTY_MEASURE_WITH_UNIT (LENGTH_MEASURE( 1.000000000000000082E-05 ), #49666, 'distance_accuracy_value', 'NONE');
#27693 = CARTESIAN_POINT ( 'NONE',  ( -108.4242937615723719, -59.99999999999997868, 194.8630744897274667 ) ) ;
#27694 = SURFACE_SIDE_STYLE ('',( #11444 ) ) ;
#27695 = DIRECTION ( 'NONE',  ( 0.000000000000000000, 0.000000000000000000, 1.000000000000000000 ) ) ;
#27696 = DIRECTION ( 'NONE',  ( -1.000000000000000000, -1.224606353822377258E-16, -0.000000000000000000 ) ) ;
#27697 = B_SPLINE_CURVE_WITH_KNOTS ( 'NONE', 3,
 ( #48958, #89974, #16078, #64132, #97001, #89451 ),
 .UNSPECIFIED., .F., .F.,
 ( 4, 2, 4 ),
 ( 0.004444412883774330643, 0.006655097293744430265, 0.008865781703714530754 ),
 .UNSPECIFIED. ) ;
#27698 = LINE ( 'NONE', #99936, #23267 ) ;
#27699 = CARTESIAN_POINT ( 'NONE',  ( -85.41269523509512851, -32.17776350644170691, 180.5340902165694388 ) ) ;
#27700 = CARTESIAN_POINT ( 'NONE',  ( -5.126781800564398139, 54.24761383184393537, -6.031152949374157579 ) ) ;
#27701 = CIRCLE ( 'NONE', #24303, 3.309500000000001663 ) ;
#27702 = VECTOR ( 'NONE', #18190, 1000.000000000000000 ) ;
#27703 = EDGE_LOOP ( 'NONE', ( #58717, #22026, #85919 ) ) ;
#27704 = CARTESIAN_POINT ( 'NONE',  ( 3.313708498984743844, -26.28125000000000000, 8.000000000000017764 ) ) ;
#27705 = EDGE_CURVE ( 'NONE', #36676, #56041, #78294, .T. ) ;
#27706 = CARTESIAN_POINT ( 'NONE',  ( 3.883877898720808908, -1.065320993063007426, 104.5781496044265566 ) ) ;
#27707 = CARTESIAN_POINT ( 'NONE',  ( -86.78765346559656280, -60.15861341457728884, -1.594545952693453339 ) ) ;
#27708 = AXIS2_PLACEMENT_3D ( 'NONE', #72849, #37893, #30856 ) ;
#27709 = CARTESIAN_POINT ( 'NONE',  ( 0.000000000000000000, 55.00000000000000000, 0.000000000000000000 ) ) ;
#27710 = CARTESIAN_POINT ( 'NONE',  ( -2.861896996888536382, 85.75376362043782308, -5.000000000000000000 ) ) ;
#27711 = CARTESIAN_POINT ( 'NONE',  ( -10.89098046483293558, -11.19508265682690151, 9.990606830166543162 ) ) ;
#27712 = CARTESIAN_POINT ( 'NONE',  ( -5.990573850131388767, -14.42843120744228536, 14.14171987952404130 ) ) ;
#27713 =( NAMED_UNIT ( * ) PLANE_ANGLE_UNIT ( ) SI_UNIT ( $, .RADIAN. ) );
#27714 = ADVANCED_FACE ( 'NONE', ( #10951 ), #76588, .T. ) ;
#27715 = CARTESIAN_POINT ( 'NONE',  ( 76.30472591814422856, -30.00000000000007105, 168.5677193688796649 ) ) ;
#27716 = EDGE_CURVE ( 'NONE', #35657, #93202, #38668, .T. ) ;
#27717 = CIRCLE ( 'NONE', #50062, 5.000000000000001776 ) ;
#27718 = CARTESIAN_POINT ( 'NONE',  ( -94.38155987036965655, -60.00000000000007105, 5.296623108471039565 ) ) ;
#27719 = CARTESIAN_POINT ( 'NONE',  ( -67.30718710595479592, -39.48677006991138683, 93.17581753966889835 ) ) ;
#27720 = EDGE_LOOP ( 'NONE', ( #58692, #62237, #66477, #38086, #8595 ) ) ;
#27721 = CARTESIAN_POINT ( 'NONE',  ( 86.31905819422470927, -30.00000000000006750, 198.0863690661441296 ) ) ;
#27722 = CARTESIAN_POINT ( 'NONE',  ( 58.89338521243953295, 40.83722513022537015, -28.14236001438834478 ) ) ;
#27723 = ORIENTED_EDGE ( 'NONE', *, *, #66495, .T. ) ;
#27724 = CARTESIAN_POINT ( 'NONE',  ( 29.01678287318512162, -59.99999999999877787, 45.16868993385956799 ) ) ;
#27725 = ORIENTED_EDGE ( 'NONE', *, *, #5205, .T. ) ;
#27726 = CARTESIAN_POINT ( 'NONE',  ( 13.86010052718616947, -8.688880844539829340, 12.24034105654405913 ) ) ;
#27727 = CARTESIAN_POINT ( 'NONE',  ( -7.188101187500002709, -26.18750000204838457, 2.977408999572647819 ) ) ;
#27728 = EDGE_CURVE ( 'NONE', #83020, #75460, #54180, .T. ) ;
#27729 = CIRCLE ( 'NONE', #96519, 5.000000000000002665 ) ;
#27730 = CARTESIAN_POINT ( 'NONE',  ( -4.813668318631101783, -8.204867701733141061, 3.583991016754771497 ) ) ;
#27731 = VERTEX_POINT ( 'NONE', #77309 ) ;
#27732 = SURFACE_STYLE_USAGE ( .BOTH. , #84327 ) ;
#27733 = ORIENTED_EDGE ( 'NONE', *, *, #100030, .F. ) ;
#27734 = DIRECTION ( 'NONE',  ( -1.000000000000000000, -1.224606353822377258E-16, -0.000000000000000000 ) ) ;
#27735 = CARTESIAN_POINT ( 'NONE',  ( 20.77592568779148863, 5.000000000000002665, 0.000000000000000000 ) ) ;
#27736 = CARTESIAN_POINT ( 'NONE',  ( -43.97714636534035293, -60.00000000001949019, 63.83295154858610232 ) ) ;
#27737 = DIRECTION ( 'NONE',  ( -2.742080092235280244E-17, -0.000000000000000000, 1.000000000000000000 ) ) ;
#27738 = CARTESIAN_POINT ( 'NONE',  ( -2.977408999572654480, -30.50000000204838813, 7.188101187499999156 ) ) ;
#27739 = EDGE_CURVE ( 'NONE', #27639, #16669, #7679, .T. ) ;
#27740 = PLANE ( 'NONE',  #22560 ) ;
#27741 = CARTESIAN_POINT ( 'NONE',  ( 1.650803255657553592, -4.285714285714296246, -25.22241582816892347 ) ) ;
#27742 = CARTESIAN_POINT ( 'NONE',  ( 43.88846153846154152, -4.171999999999999709, 5.616230220889763424E-16 ) ) ;
#27743 = CARTESIAN_POINT ( 'NONE',  ( 3.140974613990258568, 50.00000000000000000, -96.68767211932436112 ) ) ;
#27744 = CARTESIAN_POINT ( 'NONE',  ( -5.656854249492379694, -14.93749999999999289, -5.656854249492380582 ) ) ;
#27745 =( NAMED_UNIT ( * ) SI_UNIT ( $, .STERADIAN. ) SOLID_ANGLE_UNIT ( ) );
#27746 = ORIENTED_EDGE ( 'NONE', *, *, #18767, .T. ) ;
#27748 = CARTESIAN_POINT ( 'NONE',  ( 32.80054068545892676, -49.89943310828323320, 36.16858534763461819 ) ) ;
#27747 = DIRECTION ( 'NONE',  ( 0.5735764363510470476, -0.8191520442889911324, 1.003171929053524007E-16 ) ) ;
#27749 = CIRCLE ( 'NONE', #79429, 4.250000000000000000 ) ;
#27750 = CARTESIAN_POINT ( 'NONE',  ( -15.50035291838204721, -4.285714285714287364, -20.16952962162827845 ) ) ;
#27751 = VERTEX_POINT ( 'NONE', #25609 ) ;
#27752 = CARTESIAN_POINT ( 'NONE',  ( -23.21751746555280249, 25.98869614573808207, -30.70617127781034839 ) ) ;
#27753 = CONICAL_SURFACE ( 'NONE', #87995, 5.000000000000000000, 0.9599310885968913576 ) ;
#27755 = CARTESIAN_POINT ( 'NONE',  ( -32.54922218626916930, 319.8023524069591303, -6.363686095274232457 ) ) ;
#27754 = CARTESIAN_POINT ( 'NONE',  ( -26.70997489550019210, 34.89067225687768570, -7.618312596025223371 ) ) ;
#27756 = FACE_OUTER_BOUND ( 'NONE', #83645, .T. ) ;
#27757 = CARTESIAN_POINT ( 'NONE',  ( -43.69141235711237670, 485.1129823701677992, 2.341835213801349624 ) ) ;
#27758 = DIRECTION ( 'NONE',  ( 0.000000000000000000, 1.000000000000000000, 0.000000000000000000 ) ) ;
#27759 = DIRECTION ( 'NONE',  ( -1.000000000000000000, -0.000000000000000000, -0.000000000000000000 ) ) ;
#27760 = CARTESIAN_POINT ( 'NONE',  ( -7.500000000000000888, 2.886751345948123326, -7.198902722707428481 ) ) ;
#27761 = ORIENTED_EDGE ( 'NONE', *, *, #95708, .T. ) ;
#27762 = CARTESIAN_POINT ( 'NONE',  ( 92.68349473529568172, -60.00000000000001421, -4.407455099632911377 ) ) ;
#27763 = DIRECTION ( 'NONE',  ( -0.5735764363510497121, 0.8191520442889892450, 1.003171929053521665E-16 ) ) ;
#27764 =( NAMED_UNIT ( * ) PLANE_ANGLE_UNIT ( ) SI_UNIT ( $, .RADIAN. ) );
#27765 = CARTESIAN_POINT ( 'NONE',  ( -36.73972469232126770, 391.2873159729405188, 5.934521470291739043 ) ) ;
#27766 = CARTESIAN_POINT ( 'NONE',  ( -5.582554154870011054, 41.37363122748190136, -70.85834493696303582 ) ) ;
#27767 = DIRECTION ( 'NONE',  ( 0.000000000000000000, -1.000000000000000000, 0.000000000000000000 ) ) ;
#27768 = ORIENTED_EDGE ( 'NONE', *, *, #65597, .F. ) ;
#27769 = CONICAL_SURFACE ( 'NONE', #67376, 4.000000000000007105, 0.9599310885968835860 ) ;
#27770 = CARTESIAN_POINT ( 'NONE',  ( -92.17868644654814148, -29.99999999997585931, 199.7068435760925809 ) ) ;
#27771 = VERTEX_POINT ( 'NONE', #5016 ) ;
#27772 = AXIS2_PLACEMENT_3D ( 'NONE', #12170, #94170, #70429 ) ;
#27773 = CARTESIAN_POINT ( 'NONE',  ( 3.313708498984800688, -11.28124999999998934, 7.999999999999960032 ) ) ;
#27774 = CARTESIAN_POINT ( 'NONE',  ( 5.601730134768060587, -12.35429686688395989, -12.97150009825808148 ) ) ;
#27775 = CYLINDRICAL_SURFACE ( 'NONE', #55671, 5.000000000000002665 ) ;
#27776 = FILL_AREA_STYLE ('',( #51459 ) ) ;
#27777 = CARTESIAN_POINT ( 'NONE',  ( 82.90625021741112732, -37.79796058491805866, -11.19383744670581571 ) ) ;
#27778 = CARTESIAN_POINT ( 'NONE',  ( -37.76134924625720402, 305.2126739483049960, -7.610856539317000014 ) ) ;
#27779 = CARTESIAN_POINT ( 'NONE',  ( -11.89662026262662842, 304.5916488899262617, -10.05529741525224452 ) ) ;
#27780 = CARTESIAN_POINT ( 'NONE',  ( -18.27524112071357720, 45.00000000000001421, 62.41775947855344242 ) ) ;
#27781 = CARTESIAN_POINT ( 'NONE',  ( 3.490407211888509836E-12, -4.332980043422162808, 17.83347932686506354 ) ) ;
#27782 = VERTEX_POINT ( 'NONE', #86493 ) ;
#27784 = EDGE_CURVE ( 'NONE', #20727, #2280, #59371, .T. ) ;
#27783 = CARTESIAN_POINT ( 'NONE',  ( -42.73089261237365832, 435.7309723475635792, 18.11242468272465089 ) ) ;
#27785 = ORIENTED_EDGE ( 'NONE', *, *, #90377, .F. ) ;
#27786 = DIRECTION ( 'NONE',  ( 1.000000000000000000, 0.000000000000000000, 0.000000000000000000 ) ) ;
#27788 = ORIENTED_EDGE ( 'NONE', *, *, #44999, .F. ) ;
#27787 = CARTESIAN_POINT ( 'NONE',  ( 5.000000000000000000, -60.71953810597794643, 12.61250543007074931 ) ) ;
#27789 = CARTESIAN_POINT ( 'NONE',  ( 76.14851803333424130, -56.84259894051964324, 140.2336560434112300 ) ) ;
#27790 = COLOUR_RGB ( '', 0.09019608, 0.27058824, 0.51372549) ;
#27791 = ORIENTED_EDGE ( 'NONE', *, *, #83537, .T. ) ;
#27792 = AXIS2_PLACEMENT_3D ( 'NONE', #70183, #21145, #62632 ) ;
#27793 = CARTESIAN_POINT ( 'NONE',  ( 3.914937639300730687, -48.74218602603162509, 43.65505948954400850 ) ) ;
#27794 = CARTESIAN_POINT ( 'NONE',  ( -30.00000000000000000, 500.0000000000002274, 12.00000000000000888 ) ) ;
#27795 = CARTESIAN_POINT ( 'NONE',  ( -1.320432766682874540E-15, -25.53125000204838813, 7.188101187500000044 ) ) ;
#27796 = CARTESIAN_POINT ( 'NONE',  ( -72.23603530542938245, -57.67079283669161782, 174.4370243615865661 ) ) ;
#27797 = ORIENTED_EDGE ( 'NONE', *, *, #71867, .F. ) ;
#27798 = AXIS2_PLACEMENT_3D ( 'NONE', #98716, #90648, #16754 ) ;
#27799 = CYLINDRICAL_SURFACE ( 'NONE', #23081, 8.000000000000000000 ) ;
#27800 = CARTESIAN_POINT ( 'NONE',  ( 105.2612990973347991, -52.71713998817723024, 170.4785330017703302 ) ) ;
#27801 = CARTESIAN_POINT ( 'NONE',  ( -36.31989234532075272, 28.16027530257773392, -12.39692247340019371 ) ) ;
#27802 = EDGE_CURVE ( 'NONE', #20962, #81388, #63259, .T. ) ;
#27803 = AXIS2_PLACEMENT_3D ( 'NONE', #29638, #46318, #86268 ) ;
#27804 = CARTESIAN_POINT ( 'NONE',  ( 0.8750000000000016653, -70.58759490697437400, 13.02737050516260098 ) ) ;
#27805 = CARTESIAN_POINT ( 'NONE',  ( -3.313708498984765161, -16.15625000409677270, 7.999999999999998224 ) ) ;
#27806 = CARTESIAN_POINT ( 'NONE',  ( -51.41203370401020578, -29.90211857482027114, 49.01905699928327209 ) ) ;
#27807 = CARTESIAN_POINT ( 'NONE',  ( 9.165151389911699198, 249.7328921871707905, -4.000000000000001776 ) ) ;
#27808 = CARTESIAN_POINT ( 'NONE',  ( 1.380949872273418154E-15, 45.89575828009193259, 11.27631144943088337 ) ) ;
#27809 = ADVANCED_FACE ( 'NONE', ( #37417 ), #62726, .F. ) ;
#27810 =( NAMED_UNIT ( * ) SI_UNIT ( $, .STERADIAN. ) SOLID_ANGLE_UNIT ( ) );
#27811 = DIRECTION ( 'NONE',  ( -1.000000000000000000, 0.000000000000000000, 0.000000000000000000 ) ) ;
#27812 = DIRECTION ( 'NONE',  ( 4.317635597591861497E-20, -0.9664921437969917761, -0.2566961939310660190 ) ) ;
#27813 = LINE ( 'NONE', #35356, #47035 ) ;
#27814 = ORIENTED_EDGE ( 'NONE', *, *, #27673, .F. ) ;
#27815 = CARTESIAN_POINT ( 'NONE',  ( -3.642721895236043395, -49.00544355537606833, 43.86825576446273089 ) ) ;
#27816 = CARTESIAN_POINT ( 'NONE',  ( 11.47222955920350707, -4.944097607773928260, -12.56918813344000263 ) ) ;
#27817 = CARTESIAN_POINT ( 'NONE',  ( 1.159636676343374750, 11.84329530645718265, 50.01746790140171584 ) ) ;
#27818 = CARTESIAN_POINT ( 'NONE',  ( -86.35638819720911386, -30.00000000000000355, 180.7480702730107112 ) ) ;
#27819 = EDGE_LOOP ( 'NONE', ( #49477, #99642, #105559, #7349 ) ) ;
#27820 = CARTESIAN_POINT ( 'NONE',  ( 7.500000000000001776, 0.000000000000000000, 0.000000000000000000 ) ) ;
#27821 = CARTESIAN_POINT ( 'NONE',  ( 77.35975252159606441, -57.51975665479443478, 195.6400774986267095 ) ) ;
#27822 = AXIS2_PLACEMENT_3D ( 'NONE', #69623, #5409, #14005 ) ;
#27823 = DIRECTION ( 'NONE',  ( 0.000000000000000000, 0.000000000000000000, 1.000000000000000000 ) ) ;
#27824 = CARTESIAN_POINT ( 'NONE',  ( 46.78448780204201540, -34.81110335320523319, -36.64205672983788276 ) ) ;
#27825 = AXIS2_PLACEMENT_3D ( 'NONE', #19301, #5703, #63966 ) ;
#27826 = CARTESIAN_POINT ( 'NONE',  ( 7.500000000000000000, -4.999999999999999112, -36.97043916959989929 ) ) ;
#27827 = CARTESIAN_POINT ( 'NONE',  ( 6.400000000000000355, 9.237604307034018802, 0.000000000000000000 ) ) ;
#27828 = PRODUCT_DEFINITION_SHAPE ( 'NONE', 'NONE',  #52852 ) ;
#27829 = CARTESIAN_POINT ( 'NONE',  ( -67.41425160460600807, -60.00000000000000711, 128.3978068706913973 ) ) ;
#27830 =( NAMED_UNIT ( * ) SI_UNIT ( $, .STERADIAN. ) SOLID_ANGLE_UNIT ( ) );
#27831 = CARTESIAN_POINT ( 'NONE',  ( 65.26738680890606759, 48.00000000000000000, 0.8120011905328435864 ) ) ;
#27832 = CARTESIAN_POINT ( 'NONE',  ( -86.49700811817415058, -46.49039750389685821, 190.2550539850416840 ) ) ;
#27833 = ORIENTED_EDGE ( 'NONE', *, *, #93832, .T. ) ;
#27834 = CARTESIAN_POINT ( 'NONE',  ( 34.10284876471455817, 1.482358050883964840E-15, 0.000000000000000000 ) ) ;
#27835 = CARTESIAN_POINT ( 'NONE',  ( -0.9911087893856018738, -25.54951634130952698, 28.14790268315395849 ) ) ;
#27836 = CARTESIAN_POINT ( 'NONE',  ( -6.678341091416172048, 41.85887519985161731, -59.41504748149177573 ) ) ;
#27837 = CARTESIAN_POINT ( 'NONE',  ( -3.249999999999999112, -5.629165124598882741, -5.592027715088716988 ) ) ;
#27838 = CARTESIAN_POINT ( 'NONE',  ( -32.96172342428652513, 300.4657064437288341, 3.200647364369005654 ) ) ;
#27839 = ORIENTED_EDGE ( 'NONE', *, *, #61779, .T. ) ;
#27840 = AXIS2_PLACEMENT_3D ( 'NONE', #86643, #14294, #12711 ) ;
#27841 = CARTESIAN_POINT ( 'NONE',  ( 24.33159596665262470, 34.19642918197134662, -12.16579798332631768 ) ) ;
#27842 = DIRECTION ( 'NONE',  ( 0.000000000000000000, 0.000000000000000000, 1.000000000000000000 ) ) ;
#27843 = CARTESIAN_POINT ( 'NONE',  ( 15.11650669486618881, 4.000000000000003553, 4.898587196589414801E-16 ) ) ;
#27844 = EDGE_CURVE ( 'NONE', #80842, #82136, #62841, .T. ) ;
#27845 = DIRECTION ( 'NONE',  ( 0.000000000000000000, 0.000000000000000000, -1.000000000000000000 ) ) ;
#27846 = CARTESIAN_POINT ( 'NONE',  ( 25.83562903227484497, 295.7929986566709886, -9.797862988238321691 ) ) ;
#27847 = CARTESIAN_POINT ( 'NONE',  ( 34.94338628507543376, 342.5355909536760350, -0.9693026116538068226 ) ) ;
#27848 = EDGE_CURVE ( 'NONE', #25681, #46054, #48568, .T. ) ;
#27849 = CARTESIAN_POINT ( 'NONE',  ( 53.78349330513380266, 6.975173280561618775E-15, 0.000000000000000000 ) ) ;
#27850 = CARTESIAN_POINT ( 'NONE',  ( 9.300970015859846285, 53.68222913732174817, -1.771665439178985446 ) ) ;
#27851 = EDGE_CURVE ( 'NONE', #93450, #62342, #45923, .T. ) ;
#27852 = CARTESIAN_POINT ( 'NONE',  ( 98.01458704197314376, -60.00000000000006395, 53.57113828723962001 ) ) ;
#27853 = CARTESIAN_POINT ( 'NONE',  ( -79.54470974501947467, -46.43897030528811598, 150.5969177418128595 ) ) ;
#27854 = ORIENTED_EDGE ( 'NONE', *, *, #95773, .T. ) ;
#27855 = CARTESIAN_POINT ( 'NONE',  ( 15.75384615384615294, 1.411358822780289120E-15, 0.000000000000000000 ) ) ;
#27856 = CARTESIAN_POINT ( 'NONE',  ( 0.000000000000000000, 0.000000000000000000, -1.875285714285714445 ) ) ;
#27857 = CARTESIAN_POINT ( 'NONE',  ( 56.31243090753932989, -57.67579812645779924, 95.28593385378083269 ) ) ;
#27858 = CARTESIAN_POINT ( 'NONE',  ( 0.000000000000000000, 27.68727484027578356, -33.82893434829263413 ) ) ;
#27859 = CARTESIAN_POINT ( 'NONE',  ( 41.99603398301461255, 317.0185905804366939, -4.657216470168420663 ) ) ;
#27860 = CARTESIAN_POINT ( 'NONE',  ( 34.74668892571865086, 477.5740991570432925, -0.3050944403155617657 ) ) ;
#27861 = ORIENTED_EDGE ( 'NONE', *, *, #48575, .T. ) ;
#27862 = B_SPLINE_CURVE_WITH_KNOTS ( 'NONE', 3,
 ( #62909, #95278, #87187, #37604, #86670, #69933, #11671, #21407, #93681, #44604, #70466, #3609, #61860, #13797, #79602, #36011, #102292, #54242, #20377, #12739, #79079, #13266, #28993, #45661 ),
 .UNSPECIFIED., .F., .F.,
 ( 4, 2, 2, 2, 2, 2, 2, 2, 2, 2, 2, 4 ),
 ( 0.007009756851916126852, 0.007512278926379567512, 0.008014801000843008172, 0.008517323075306448832, 0.008768584112538169162, 0.009019845149769889492, 0.009271106187001611557, 0.009522367224233333621, 0.01002488929869677428, 0.01027615033592849635, 0.01052741137316021841, 0.01102993344762366601 ),
 .UNSPECIFIED. ) ;
#27863 = DIRECTION ( 'NONE',  ( -1.000000000000000000, -0.000000000000000000, -0.000000000000000000 ) ) ;
#27864 = MECHANICAL_DESIGN_GEOMETRIC_PRESENTATION_REPRESENTATION (  '', ( #57119 ), #24373 ) ;
#27865 = AXIS2_PLACEMENT_3D ( 'NONE', #25806, #40864, #100165 ) ;
#27866 = CYLINDRICAL_SURFACE ( 'NONE', #101766, 5.000000000000000888 ) ;
#27867 = CARTESIAN_POINT ( 'NONE',  ( -5.082755093536326818, -30.21875000204838813, 5.082755093536325042 ) ) ;
#27868 = EDGE_CURVE ( 'NONE', #64268, #33845, #35296, .T. ) ;
#27869 = VERTEX_POINT ( 'NONE', #37950 ) ;
#27870 = PRESENTATION_STYLE_ASSIGNMENT (( #76887 ) ) ;
#27871 = CARTESIAN_POINT ( 'NONE',  ( -3.484792534604214342, 15.95825086476136967, 9.380155525692146057 ) ) ;
#27872 = CARTESIAN_POINT ( 'NONE',  ( 6.299403769935631558, 41.97741512816498499, -69.49222142767905552 ) ) ;
#27873 = CARTESIAN_POINT ( 'NONE',  ( -64.91565662645538737, 49.99999999999999289, 6.815324757469617190 ) ) ;
#27874 = CARTESIAN_POINT ( 'NONE',  ( 83.86866073052654258, 6.123233995736568081E-16, -5.000000000000011546 ) ) ;
#27875 = AXIS2_PLACEMENT_3D ( 'NONE', #93661, #34388, #1966 ) ;
#27876 = SURFACE_STYLE_USAGE ( .BOTH. , #1931 ) ;
#27877 = ORIENTED_EDGE ( 'NONE', *, *, #103459, .T. ) ;
#27878 = CARTESIAN_POINT ( 'NONE',  ( 92.74075353299672031, -60.00000000000002132, -7.839124456446247891 ) ) ;
#27879 = VECTOR ( 'NONE', #44670, 1000.000000000000000 ) ;
#27881 = CARTESIAN_POINT ( 'NONE',  ( 20.49951756439809358, -53.39523566873690186, 33.37178152886023952 ) ) ;
#27880 = CARTESIAN_POINT ( 'NONE',  ( -74.83603090277703984, -14.21045842199441012, 137.5224045200043577 ) ) ;
#27882 = CARTESIAN_POINT ( 'NONE',  ( 1.484151383916717602E-14, 4.501353321498349658, -60.59507871780017751 ) ) ;
#27883 = CARTESIAN_POINT ( 'NONE',  ( -37.51903186869294871, -49.89542786323897161, 39.00874087383915167 ) ) ;
#27884 = AXIS2_PLACEMENT_3D ( 'NONE', #99105, #911, #82939 ) ;
#27885 = UNCERTAINTY_MEASURE_WITH_UNIT (LENGTH_MEASURE( 1.000000000000000082E-05 ), #26307, 'distance_accuracy_value', 'NONE');
#27886 = EDGE_LOOP ( 'NONE', ( #22369, #37253 ) ) ;
#27887 = FILL_AREA_STYLE_COLOUR ( '', #13382 ) ;
#27888 = CARTESIAN_POINT ( 'NONE',  ( 43.58349330513380693, -7.703719777548943412E-31, 4.000000000000001776 ) ) ;
#27889 = LINE ( 'NONE', #84484, #81879 ) ;
#27890 = CARTESIAN_POINT ( 'NONE',  ( 7.343637806710344051, -62.55636878099384290, 3.177475076494676198 ) ) ;
#27891 = CARTESIAN_POINT ( 'NONE',  ( -16.05785784214753065, 4.775831776487158287, 3.710403933803144927 ) ) ;
#27892 = ORIENTED_EDGE ( 'NONE', *, *, #61995, .T. ) ;
#27893 = FACE_OUTER_BOUND ( 'NONE', #81232, .T. ) ;
#27894 = ORIENTED_EDGE ( 'NONE', *, *, #103917, .T. ) ;
#27895 = CARTESIAN_POINT ( 'NONE',  ( 92.20262301002225058, -29.99999999999975486, 190.9253757062230932 ) ) ;
#27896 = CARTESIAN_POINT ( 'NONE',  ( 33.09320956684935311, 40.69741856558304960, -62.14400065382765348 ) ) ;
#27897 = DIRECTION ( 'NONE',  ( -1.000000000000000000, -0.000000000000000000, -0.000000000000000000 ) ) ;
#27898 = CARTESIAN_POINT ( 'NONE',  ( 81.43962946624536414, -30.00000000000000355, -9.755616628628736464 ) ) ;
#27899 =( BOUNDED_SURFACE ( )  B_SPLINE_SURFACE ( 3, 2, ( 
 ( #31402, #13, #98213 ),
 ( #32981, #82568, #65852 ),
 ( #49116, #15700, #6540 ),
 ( #98730, #24886, #81477 ) ),
 .UNSPECIFIED., .F., .F., .F. ) 
 B_SPLINE_SURFACE_WITH_KNOTS ( ( 4, 4 ),
 ( 3, 3 ),
 ( 1.734723475976807094E-18, 0.0002932394964387638383 ),
 ( 0.000000000000000000, 1.000000000000000000 ),
 .UNSPECIFIED. ) 
 GEOMETRIC_REPRESENTATION_ITEM ( )  RATIONAL_B_SPLINE_SURFACE ( (
 ( 1.000000000000000000, 0.7912633096140038180, 1.000000000000000000),
 ( 1.000000000000000000, 0.7930984581161097946, 1.000000000000000000),
 ( 1.000000000000000000, 0.7948408637866294368, 1.000000000000000000),
 ( 1.000000000000000000, 0.7964893136847220889, 1.000000000000000000) ) ) 
 REPRESENTATION_ITEM ( '' )  SURFACE ( )  );
#27900 = CARTESIAN_POINT ( 'NONE',  ( -32.14349642894332248, 424.2545041670527439, 25.05049640504120845 ) ) ;
#27901 = ORIENTED_EDGE ( 'NONE', *, *, #5146, .T. ) ;
#27902 = AXIS2_PLACEMENT_3D ( 'NONE', #104732, #61108, #20156 ) ;
#27903 = VERTEX_POINT ( 'NONE', #38461 ) ;
#27904 = ORIENTED_EDGE ( 'NONE', *, *, #95483, .T. ) ;
#27905 = CARTESIAN_POINT ( 'NONE',  ( -32.70701262249002639, 465.7750753107770265, 13.84670167514589068 ) ) ;
#27906 = CARTESIAN_POINT ( 'NONE',  ( 37.61650669486618881, -3.851859888774471706E-31, 4.000000000000000888 ) ) ;
#27907 = VECTOR ( 'NONE', #71321, 1000.000000000000000 ) ;
#27908 = CARTESIAN_POINT ( 'NONE',  ( 41.61220833757316484, 437.6913339738342756, 21.78352536266461925 ) ) ;
#27909 = CARTESIAN_POINT ( 'NONE',  ( -17.85280542844888529, 43.24717813759219354, -5.051306223358245973 ) ) ;
#27910 = CARTESIAN_POINT ( 'NONE',  ( 6.123233995736761352E-16, 69.00000000000000000, 4.999999999999993783 ) ) ;
#27911 = CARTESIAN_POINT ( 'NONE',  ( 52.56483885390523625, 48.00000000000000000, -38.23529411764706509 ) ) ;
#27912 = EDGE_LOOP ( 'NONE', ( #79261, #105882, #35327, #58434 ) ) ;
#27914 = ADVANCED_FACE ( 'NONE', ( #30368 ), #36885, .F. ) ;
#27913 = CARTESIAN_POINT ( 'NONE',  ( 7.374560640984048732, 50.00000000000000000, -94.59600210749853488 ) ) ;
#27915 = AXIS2_PLACEMENT_3D ( 'NONE', #95421, #4822, #38279 ) ;
#27916 = ORIENTED_EDGE ( 'NONE', *, *, #81192, .T. ) ;
#27917 = CARTESIAN_POINT ( 'NONE',  ( -5.382954851612912428, -62.00012508510553744, -2.657971597726730639 ) ) ;
#27918 = CARTESIAN_POINT ( 'NONE',  ( 74.24252310225787710, -38.32799067271444926, 162.4645122954939609 ) ) ;
#27919 = DIRECTION ( 'NONE',  ( -1.000000000000000000, -1.224606353822377258E-16, -0.000000000000000000 ) ) ;
#27920 = CARTESIAN_POINT ( 'NONE',  ( 22.39204233095570729, 303.2998958009682724, 10.03333151357952424 ) ) ;
#27921 = DIRECTION ( 'NONE',  ( 0.000000000000000000, -1.000000000000000000, 0.000000000000000000 ) ) ;
#27922 = ORIENTED_EDGE ( 'NONE', *, *, #11565, .F. ) ;
#27923 = CARTESIAN_POINT ( 'NONE',  ( 1.163414459189985485E-15, 0.000000000000000000, -9.500000000000000000 ) ) ;
#27924 = CARTESIAN_POINT ( 'NONE',  ( 12.79230769230769305, 1.411358822780289120E-15, 0.000000000000000000 ) ) ;
#27925 = CARTESIAN_POINT ( 'NONE',  ( 38.82758694742345540, 312.8745823789997189, 6.266461510169453852 ) ) ;
#27926 = EDGE_CURVE ( 'NONE', #88535, #41081, #9997, .T. ) ;
#27927 = CARTESIAN_POINT ( 'NONE',  ( 0.000000000000000000, 0.000000000000000000, 0.000000000000000000 ) ) ;
#27928 = VERTEX_POINT ( 'NONE', #56724 ) ;
#27929 = SURFACE_SIDE_STYLE ('',( #75346 ) ) ;
#27930 = DIRECTION ( 'NONE',  ( -1.000000000000000000, -0.000000000000000000, -0.000000000000000000 ) ) ;
#27931 = PRESENTATION_STYLE_ASSIGNMENT (( #77500 ) ) ;
#27932 = FACE_OUTER_BOUND ( 'NONE', #86636, .T. ) ;
#27933 = CARTESIAN_POINT ( 'NONE',  ( -7.344361273354515163, 102.5543946941147766, -3.175733139645589009 ) ) ;
#27934 = CARTESIAN_POINT ( 'NONE',  ( 9.090909090909088164, 16.00000000000000000, 4.165977904505314910 ) ) ;
#27935 = CARTESIAN_POINT ( 'NONE',  ( 86.13876527465689037, -31.92079174777700956, 184.4232561367118137 ) ) ;
#27936 = EDGE_CURVE ( 'NONE', #54576, #79036, #45599, .T. ) ;
#27937 = DIRECTION ( 'NONE',  ( 0.000000000000000000, -1.000000000000000000, 0.000000000000000000 ) ) ;
#27938 = EDGE_CURVE ( 'NONE', #31781, #35660, #2532, .T. ) ;
#27939 = CARTESIAN_POINT ( 'NONE',  ( -3.204808325454104878, 114.6770343510770402, 5.000000000000000000 ) ) ;
#27940 = VERTEX_POINT ( 'NONE', #72390 ) ;
#27941 = SURFACE_STYLE_FILL_AREA ( #86155 ) ;
#27942 = CIRCLE ( 'NONE', #7235, 3.309500000000001663 ) ;
#27943 = FACE_OUTER_BOUND ( 'NONE', #78286, .T. ) ;
#27944 = DIRECTION ( 'NONE',  ( 0.5735764363510462704, 0.8191520442889915765, 0.000000000000000000 ) ) ;
#27945 = CARTESIAN_POINT ( 'NONE',  ( 5.000000000000000000, -14.89995766649703590, 12.47930207026080751 ) ) ;
#27946 = VECTOR ( 'NONE', #65807, 1000.000000000000000 ) ;
#27947 = ADVANCED_FACE ( 'NONE', ( #73974 ), #25338, .F. ) ;
#27948 = CARTESIAN_POINT ( 'NONE',  ( -86.44692486882411231, -29.99999999999999645, 67.03969724269380492 ) ) ;
#27949 = B_SPLINE_CURVE_WITH_KNOTS ( 'NONE', 3,
 ( #90479, #65136, #57028, #80242, #98554, #64101, #81827, #31731 ),
 .UNSPECIFIED., .F., .F.,
 ( 4, 2, 2, 4 ),
 ( 0.000000000000000000, 0.002068697987604109587, 0.003103046981406205364, 0.004137395975208301574 ),
 .UNSPECIFIED. ) ;
#27950 = DIRECTION ( 'NONE',  ( 0.000000000000000000, 0.000000000000000000, 1.000000000000000000 ) ) ;
#27951 = CIRCLE ( 'NONE', #48511, 15.14825148316532832 ) ;
#27952 = CARTESIAN_POINT ( 'NONE',  ( 27.54371250915762914, -57.67848980524139080, 44.08961535850244218 ) ) ;
#27953 = DIRECTION ( 'NONE',  ( 0.000000000000000000, 0.000000000000000000, -1.000000000000000000 ) ) ;
#27954 = CARTESIAN_POINT ( 'NONE',  ( 6.999999999999997335, -46.47786565829922978, 39.12435565298215323 ) ) ;
#27955 = CARTESIAN_POINT ( 'NONE',  ( 75.30000000000001137, 0.000000000000000000, 0.000000000000000000 ) ) ;
#27956 = CARTESIAN_POINT ( 'NONE',  ( 39.71213755904409481, 490.7526980994978203, 11.81179577511769097 ) ) ;
#27957 = CARTESIAN_POINT ( 'NONE',  ( 57.70539558375507738, -1.232595164407830946E-29, 4.000000000000007105 ) ) ;
#27958 = CARTESIAN_POINT ( 'NONE',  ( 44.47476154325583764, 485.8001484721103793, -0.4986663365551948224 ) ) ;
#27959 = CARTESIAN_POINT ( 'NONE',  ( 39.31680540536973467, -24.66152148494653673, -30.43544166128774009 ) ) ;
#27960 = CARTESIAN_POINT ( 'NONE',  ( -26.10329066505708440, -39.48148657949686680, 32.00599043094255336 ) ) ;
#27961 = ORIENTED_EDGE ( 'NONE', *, *, #35328, .F. ) ;
#27962 = CARTESIAN_POINT ( 'NONE',  ( 40.83002285427885880, 485.0211005501694785, -4.017563975491787787 ) ) ;
#27963 = CARTESIAN_POINT ( 'NONE',  ( 33.00000000000000000, 500.0000000000002274, 15.00000000000000711 ) ) ;
#27964 = CARTESIAN_POINT ( 'NONE',  ( -15.89867790359543065, -53.40221630055644653, 32.98641644927912608 ) ) ;
#27966 = CARTESIAN_POINT ( 'NONE',  ( -41.93285660804859560, 437.4666891908580624, 21.45432292391068430 ) ) ;
#27965 = CARTESIAN_POINT ( 'NONE',  ( -1.011535333131581726, 27.47315533557190648, 40.25229125636516159 ) ) ;
#27967 = ORIENTED_EDGE ( 'NONE', *, *, #94916, .T. ) ;
#27968 = CARTESIAN_POINT ( 'NONE',  ( 6.585530689845731089, -4.023059358968668953, -6.499999999999999112 ) ) ;
#27969 = ORIENTED_EDGE ( 'NONE', *, *, #27446, .F. ) ;
#27970 = DIRECTION ( 'NONE',  ( -0.000000000000000000, 1.000000000000000000, -0.000000000000000000 ) ) ;
#27971 = AXIS2_PLACEMENT_3D ( 'NONE', #38670, #86172, #5232 ) ;
#27972 = CARTESIAN_POINT ( 'NONE',  ( 15.31585736565561895, 3.092902776793541975, 3.111329462080190567 ) ) ;
#27973 = FACE_OUTER_BOUND ( 'NONE', #27449, .T. ) ;
#27974 = ORIENTED_EDGE ( 'NONE', *, *, #60385, .F. ) ;
#27975 = CYLINDRICAL_SURFACE ( 'NONE', #78151, 4.000000000000000000 ) ;
#27976 = CARTESIAN_POINT ( 'NONE',  ( 103.8597403422939180, -52.71705505079059861, 187.2922404200451183 ) ) ;
#27978 = CARTESIAN_POINT ( 'NONE',  ( -7.744329845603315832, -6.537117698465458204, -2.018701143083234673 ) ) ;
#27977 = CARTESIAN_POINT ( 'NONE',  ( -13.49999999999999822, 2.646256834279067771, -0.1392913482116606150 ) ) ;
#27979 = ORIENTED_EDGE ( 'NONE', *, *, #35238, .T. ) ;
#27980 = ORIENTED_EDGE ( 'NONE', *, *, #14904, .F. ) ;
#27981 = ADVANCED_FACE ( 'NONE', ( #52360 ), #584, .T. ) ;
#27982 = ORIENTED_EDGE ( 'NONE', *, *, #60950, .F. ) ;
#27983 = CARTESIAN_POINT ( 'NONE',  ( 22.54520074857146383, 305.4514246655992338, 9.066665743933437938 ) ) ;
#27984 = EDGE_CURVE ( 'NONE', #97763, #86992, #4244, .T. ) ;
#27985 = DIRECTION ( 'NONE',  ( 1.000000000000000000, 1.224606353822377258E-16, 0.000000000000000000 ) ) ;
#27986 = CARTESIAN_POINT ( 'NONE',  ( -14.95520043898949325, 4.194724623211063097, -5.164345506890816395 ) ) ;
#27987 = ORIENTED_EDGE ( 'NONE', *, *, #60565, .F. ) ;
#27988 = DIRECTION ( 'NONE',  ( 0.000000000000000000, -1.000000000000000000, 0.000000000000000000 ) ) ;
#27989 = CARTESIAN_POINT ( 'NONE',  ( -6.583551121182180665, 41.48989065997584191, -70.62107025447927811 ) ) ;
#27990 = CARTESIAN_POINT ( 'NONE',  ( 41.75331920095265303, 461.8277566036529720, 2.915730576367065119 ) ) ;
#27991 = CARTESIAN_POINT ( 'NONE',  ( -94.19891500039717869, -60.00000000000972022, 13.58511310247205728 ) ) ;
#27992 = CARTESIAN_POINT ( 'NONE',  ( 7.619753052866895970, -68.17451502807172403, -2.447276542590448134 ) ) ;
#27993 = FACE_OUTER_BOUND ( 'NONE', #28272, .T. ) ;
#27994 = CARTESIAN_POINT ( 'NONE',  ( -5.411616755802471701, 41.81753649772627313, -58.91471509483435653 ) ) ;
#27995 = EDGE_CURVE ( 'NONE', #54873, #96644, #62748, .T. ) ;
#27996 = CARTESIAN_POINT ( 'NONE',  ( -82.74168755217822024, -14.21045842199452203, -19.52755005266771349 ) ) ;
#27997 = CARTESIAN_POINT ( 'NONE',  ( -47.91943188888855332, -53.36384233853009107, 51.78005963556529423 ) ) ;
#27998 = ORIENTED_EDGE ( 'NONE', *, *, #38653, .T. ) ;
#27999 = DIRECTION ( 'NONE',  ( 0.000000000000000000, 0.000000000000000000, -1.000000000000000000 ) ) ;
#28000 = EDGE_LOOP ( 'NONE', ( #93657, #105134, #63752, #3155 ) ) ;
#28001 = CARTESIAN_POINT ( 'NONE',  ( 12.50000000000000178, -1.322514027130966552, -16.28752260425741483 ) ) ;
#28002 = CARTESIAN_POINT ( 'NONE',  ( -9.681569006903592012, 294.6516795043967250, -2.504656372063916780 ) ) ;
#28003 = DIRECTION ( 'NONE',  ( -1.000000000000000000, -1.224606353822377258E-16, -0.000000000000000000 ) ) ;
#28004 = VERTEX_POINT ( 'NONE', #85272 ) ;
#28005 = CARTESIAN_POINT ( 'NONE',  ( 0.000000000000000000, 0.000000000000000000, 4.000000000000000888 ) ) ;
#28006 = VERTEX_POINT ( 'NONE', #78754 ) ;
#28007 = CARTESIAN_POINT ( 'NONE',  ( 89.65068677404821074, -30.00000000002016165, 1.483486992794977866 ) ) ;
#28008 = CIRCLE ( 'NONE', #22839, 1.999999999999999556 ) ;
#28009 = CARTESIAN_POINT ( 'NONE',  ( 6.542885630808934927, 41.77241054322398384, -59.03854290128418825 ) ) ;
#28010 = CARTESIAN_POINT ( 'NONE',  ( -30.67950393659633335, 18.64316884710269662, -23.57730434127810426 ) ) ;
#28011 = CARTESIAN_POINT ( 'NONE',  ( 90.40025181191772674, -29.99999999999999289, 190.1625712390529088 ) ) ;
#28012 = AXIS2_PLACEMENT_3D ( 'NONE', #48683, #106388, #34684 ) ;
#28013 = DIRECTION ( 'NONE',  ( -1.734723475976807094E-16, -0.000000000000000000, -1.000000000000000000 ) ) ;
#28014 = DIRECTION ( 'NONE',  ( 0.5735764363510470476, -0.8191520442889911324, 1.003171929053524007E-16 ) ) ;
#28015 = VERTEX_POINT ( 'NONE', #29722 ) ;
#28016 = ORIENTED_EDGE ( 'NONE', *, *, #45590, .F. ) ;
#28017 = CARTESIAN_POINT ( 'NONE',  ( 53.60758669369196383, -46.43620476034607236, 60.07046025485742291 ) ) ;
#28018 = FACE_OUTER_BOUND ( 'NONE', #18424, .T. ) ;
#28019 = AXIS2_PLACEMENT_3D ( 'NONE', #41884, #8455, #26291 ) ;
#28020 = DIRECTION ( 'NONE',  ( -0.000000000000000000, -0.000000000000000000, 1.000000000000000000 ) ) ;
#28021 = ORIENTED_EDGE ( 'NONE', *, *, #74454, .F. ) ;
#28023 = EDGE_CURVE ( 'NONE', #21850, #99464, #71434, .T. ) ;
#28022 = CARTESIAN_POINT ( 'NONE',  ( -91.40442697271741679, -38.39518381489244803, -9.089042331466192337 ) ) ;
#28024 = VERTEX_POINT ( 'NONE', #78236 ) ;
#28025 = FACE_OUTER_BOUND ( 'NONE', #90621, .T. ) ;
#28026 = CARTESIAN_POINT ( 'NONE',  ( 107.0273482872364923, -38.36426640808143418, 194.8006998555924270 ) ) ;
#28027 = CARTESIAN_POINT ( 'NONE',  ( 10.94373115620249770, 16.64040335846121721, 9.320882347487696507 ) ) ;
#28028 = CARTESIAN_POINT ( 'NONE',  ( 83.68922614653902770, -45.28292466992145648, 14.69678876732623074 ) ) ;
#28029 = CARTESIAN_POINT ( 'NONE',  ( 40.35868996910548390, 344.7914381055520607, 21.62271489072101360 ) ) ;
#28030 = CARTESIAN_POINT ( 'NONE',  ( -26.87630176750905164, 307.4199632232798649, -9.428850274614722693 ) ) ;
#28031 = CARTESIAN_POINT ( 'NONE',  ( 4.698242434196062689, -14.20142765657284123, -8.220922734483856686 ) ) ;
#28032 = CARTESIAN_POINT ( 'NONE',  ( 5.821933341150374197, -1.421180797416045749, 6.500000000000000000 ) ) ;
#28033 = DIRECTION ( 'NONE',  ( 0.8257009859296333687, 0.000000000000000000, 0.5641080409237501092 ) ) ;
#28034 = CARTESIAN_POINT ( 'NONE',  ( 8.224467148743913825, 115.5412973725997716, 4.999999999998771649 ) ) ;
#28035 = ORIENTED_EDGE ( 'NONE', *, *, #9671, .F. ) ;
#28036 = ADVANCED_FACE ( 'NONE', ( #70683 ), #29213, .T. ) ;
#28037 = CARTESIAN_POINT ( 'NONE',  ( 1.011934152981637691, 36.47529646805227088, 29.25177536496077835 ) ) ;
#28038 = CARTESIAN_POINT ( 'NONE',  ( 7.404344845520721030, 40.29318110125479535, -70.39066561776979825 ) ) ;
#28039 = COLOUR_RGB ( '', 0.40784314, 0.44705882, 0.49803922) ;
#28040 = CARTESIAN_POINT ( 'NONE',  ( -32.88333705524179607, 439.7317646416723846, 24.13381181826116517 ) ) ;
#28041 = ORIENTED_EDGE ( 'NONE', *, *, #72474, .T. ) ;
#28042 = CARTESIAN_POINT ( 'NONE',  ( -26.73681790852576867, 307.3696589980178260, -8.440011308043008142 ) ) ;
#28043 = CARTESIAN_POINT ( 'NONE',  ( -29.29569811498970466, 313.0313481771436841, 12.40036593387712927 ) ) ;
#28044 = CARTESIAN_POINT ( 'NONE',  ( -4.000000000000000000, 0.000000000000000000, -6.838999999999999524 ) ) ;
#28045 = PRESENTATION_STYLE_ASSIGNMENT (( #38765 ) ) ;
#28046 = CARTESIAN_POINT ( 'NONE',  ( 7.999999999999998224, -23.09374999999999645, 3.313708498984766493 ) ) ;
#28047 = VECTOR ( 'NONE', #24945, 1000.000000000000000 ) ;
#28048 = CARTESIAN_POINT ( 'NONE',  ( 36.48461538461538822, 1.411358822780289120E-15, 0.000000000000000000 ) ) ;
#28049 = ORIENTED_EDGE ( 'NONE', *, *, #16114, .T. ) ;
#28050 = CARTESIAN_POINT ( 'NONE',  ( 84.63799656866569876, -42.96597369867873795, 184.5360133087482382 ) ) ;
#28051 = FACE_OUTER_BOUND ( 'NONE', #27099, .T. ) ;
#28052 = EDGE_CURVE ( 'NONE', #97405, #1352, #4848, .T. ) ;
#28053 = CARTESIAN_POINT ( 'NONE',  ( -16.32418145836352963, 45.71594865110102290, 6.626690021756176385 ) ) ;
#28054 = ORIENTED_EDGE ( 'NONE', *, *, #60865, .T. ) ;
#28055 = CARTESIAN_POINT ( 'NONE',  ( -86.61035443086036878, -45.26537160163291418, 48.35290667932413555 ) ) ;
#28056 = DIRECTION ( 'NONE',  ( 0.000000000000000000, -1.000000000000000000, 0.000000000000000000 ) ) ;
#28057 = CARTESIAN_POINT ( 'NONE',  ( -14.61924042696810488, -4.999999999997926103, -89.34162378225578038 ) ) ;
#28058 = CARTESIAN_POINT ( 'NONE',  ( 16.45451579217936811, 304.5657612144941027, 8.876165602381572484 ) ) ;
#28059 = CARTESIAN_POINT ( 'NONE',  ( -4.536700128592405790, -21.59318128966070205, -38.54827054018984711 ) ) ;
#28060 = EDGE_CURVE ( 'NONE', #64539, #77725, #71364, .T. ) ;
#28061 = SHAPE_REPRESENTATION_RELATIONSHIP ( 'NONE' , 'NONE' ,  #74292, #67921 ) ;
#28062 = CARTESIAN_POINT ( 'NONE',  ( 31.63672064570198472, -60.00000000000000711, 43.92342796496127022 ) ) ;
#28063 = CARTESIAN_POINT ( 'NONE',  ( 27.17445174878161396, -30.53057906289133072, 39.14485286163986899 ) ) ;
#28064 = CARTESIAN_POINT ( 'NONE',  ( 45.13615050346792401, -28.34248706039453580, 40.22011616339790407 ) ) ;
#28066 = CARTESIAN_POINT ( 'NONE',  ( -10.71251212345380566, 12.35323841155236479, 9.997968061205504853 ) ) ;
#28065 = CARTESIAN_POINT ( 'NONE',  ( 33.26922818042641694, 435.1894657785401819, 10.58222864814420383 ) ) ;
#28067 = CARTESIAN_POINT ( 'NONE',  ( 0.3768998597285306840, 294.9778291297479882, -9.999929723870947029 ) ) ;
#28068 = CARTESIAN_POINT ( 'NONE',  ( 2.977408999572650927, -9.875000002048386349, -7.188101187500001821 ) ) ;
#28069 = EDGE_CURVE ( 'NONE', #87999, #69327, #52420, .T. ) ;
#28070 = CARTESIAN_POINT ( 'NONE',  ( 33.20657005241940851, 300.3266200210385932, -0.7716179031724232917 ) ) ;
#28071 = CARTESIAN_POINT ( 'NONE',  ( -12.13034742782427955, -79.93083296558610584, -93.82352941176471006 ) ) ;
#28072 = CIRCLE ( 'NONE', #40115, 3.309500000000001663 ) ;
#28073 = VERTEX_POINT ( 'NONE', #33832 ) ;
#28074 = DIRECTION ( 'NONE',  ( 0.000000000000000000, 1.000000000000000000, -0.000000000000000000 ) ) ;
#28075 = SURFACE_SIDE_STYLE ('',( #11295 ) ) ;
#28076 = EDGE_LOOP ( 'NONE', ( #82666, #7623, #28216, #71205, #94406 ) ) ;
#28077 = CARTESIAN_POINT ( 'NONE',  ( -7.416346432021269308, -0.5927586397820543418, 15.44415232864270671 ) ) ;
#28078 = CARTESIAN_POINT ( 'NONE',  ( 46.00000000000000000, 488.3725375423206287, 3.127739281036224117 ) ) ;
#28079 = FACE_OUTER_BOUND ( 'NONE', #10869, .T. ) ;
#28081 = CARTESIAN_POINT ( 'NONE',  ( -12.93448875801435172, -60.22812974450989998, -36.57614896566138896 ) ) ;
#28080 = CARTESIAN_POINT ( 'NONE',  ( 9.380894568449093640, 252.0113063311093526, -3.467341429141170384 ) ) ;
#28082 = ORIENTED_EDGE ( 'NONE', *, *, #89521, .F. ) ;
#28083 = DIRECTION ( 'NONE',  ( -1.000000000000000000, -0.000000000000000000, -0.000000000000000000 ) ) ;
#28084 = CARTESIAN_POINT ( 'NONE',  ( 58.18888888888888999, 3.309500000000014541, 0.000000000000000000 ) ) ;
#28086 = VERTEX_POINT ( 'NONE', #74775 ) ;
#28085 = VECTOR ( 'NONE', #61568, 1000.000000000000227 ) ;
#28087 = FACE_OUTER_BOUND ( 'NONE', #46013, .T. ) ;
#28088 = CARTESIAN_POINT ( 'NONE',  ( 71.14984002819953446, 4.898587196589294500E-16, -4.000000000000007105 ) ) ;
#28089 =( NAMED_UNIT ( * ) SI_UNIT ( $, .STERADIAN. ) SOLID_ANGLE_UNIT ( ) );
#28090 = CARTESIAN_POINT ( 'NONE',  ( -91.98126730952112950, -59.99999999999999289, 6.611212861507896221 ) ) ;
#28091 = ORIENTED_EDGE ( 'NONE', *, *, #69975, .F. ) ;
#28092 = DIRECTION ( 'NONE',  ( 0.000000000000000000, 0.000000000000000000, -1.000000000000000000 ) ) ;
#28093 = DIRECTION ( 'NONE',  ( -1.000000000000000000, -1.224606353822377258E-16, -0.000000000000000000 ) ) ;
#28094 =( NAMED_UNIT ( * ) PLANE_ANGLE_UNIT ( ) SI_UNIT ( $, .RADIAN. ) );
#28095 = CARTESIAN_POINT ( 'NONE',  ( -9.989690267985800176, 26.02555583405089479, -0.5238310916885813295 ) ) ;
#28097 = DIRECTION ( 'NONE',  ( -0.9081249930074554166, 0.3474488548219246686, 0.2336413712469223303 ) ) ;
#28096 = CARTESIAN_POINT ( 'NONE',  ( -6.145467200824362486, -3.000000000000002665, -77.00333157709341947 ) ) ;
#28098 = CARTESIAN_POINT ( 'NONE',  ( -84.78135591110488178, -25.52853119631381418, 164.4154881268317752 ) ) ;
#28099 = ORIENTED_EDGE ( 'NONE', *, *, #37039, .F. ) ;
#28100 = CARTESIAN_POINT ( 'NONE',  ( -5.483224646687553161, 0.000000000000000000, -16.14659623657211540 ) ) ;
#28101 = EDGE_LOOP ( 'NONE', ( #87265, #60040, #63094, #29305, #43251 ) ) ;
#28102 = ORIENTED_EDGE ( 'NONE', *, *, #93067, .T. ) ;
#28103 = EDGE_CURVE ( 'NONE', #13515, #61663, #66208, .T. ) ;
#28104 =( LENGTH_UNIT ( ) NAMED_UNIT ( * ) SI_UNIT ( .MILLI., .METRE. ) );
#28105 = DIRECTION ( 'NONE',  ( 0.000000000000000000, 0.000000000000000000, -1.000000000000000000 ) ) ;
#28106 = ORIENTED_EDGE ( 'NONE', *, *, #61270, .T. ) ;
#28107 = CARTESIAN_POINT ( 'NONE',  ( 33.21102376836596193, 438.9613914113129454, 23.92328486949907784 ) ) ;
#28108 = CARTESIAN_POINT ( 'NONE',  ( -81.27538057784241232, -57.67119034933180188, -29.50368748078413361 ) ) ;
#28109 = LINE ( 'NONE', #85246, #71440 ) ;
#28110 = CARTESIAN_POINT ( 'NONE',  ( 17.33349330513380337, 1.593028355512270567E-15, 0.000000000000000000 ) ) ;
#28111 = AXIS2_PLACEMENT_3D ( 'NONE', #53208, #38121, #54772 ) ;
#28112 = CARTESIAN_POINT ( 'NONE',  ( -9.176803346051512378, 104.4705284420256106, 3.973598758023531019 ) ) ;
#28113 = DIRECTION ( 'NONE',  ( 0.000000000000000000, 0.000000000000000000, 1.000000000000000000 ) ) ;
#28114 = CARTESIAN_POINT ( 'NONE',  ( 4.165977904505312246, 16.00000000000000000, -9.090909090909088164 ) ) ;
#28115 = EDGE_CURVE ( 'NONE', #18709, #16503, #73020, .T. ) ;
#28116 = CARTESIAN_POINT ( 'NONE',  ( 104.6654747121523030, -30.00000000000000000, 124.7724495044359116 ) ) ;
#28117 = CARTESIAN_POINT ( 'NONE',  ( -78.42690035548760363, -14.21045842199427156, 178.5095186877798028 ) ) ;
#28118 = CARTESIAN_POINT ( 'NONE',  ( -55.57844914912075041, -32.55979464754466335, 58.72184905296868607 ) ) ;
#28119 = ORIENTED_EDGE ( 'NONE', *, *, #88580, .F. ) ;
#28120 = FILL_AREA_STYLE_COLOUR ( '', #81592 ) ;
#28121 = ORIENTED_EDGE ( 'NONE', *, *, #82894, .F. ) ;
#28122 = CARTESIAN_POINT ( 'NONE',  ( -105.9261641753950727, -60.15502446452519081, 182.9949040398753368 ) ) ;
#28123 = FACE_OUTER_BOUND ( 'NONE', #69453, .T. ) ;
#28124 = CARTESIAN_POINT ( 'NONE',  ( 8.000000000000000000, -18.68750000409676915, 0.000000000000000000 ) ) ;
#28125 = PRESENTATION_STYLE_ASSIGNMENT (( #19514 ) ) ;
#28126 = ORIENTED_EDGE ( 'NONE', *, *, #24617, .T. ) ;
#28127 = CARTESIAN_POINT ( 'NONE',  ( 6.827804075700396602, -4.999999999999998224, -71.19745154229144646 ) ) ;
#28128 = CARTESIAN_POINT ( 'NONE',  ( -21.83613416818080921, -59.99999999999997868, 40.48705974210427172 ) ) ;
#28129 = CARTESIAN_POINT ( 'NONE',  ( -0.9999999999999943379, 0.000000000000000000, 101.0455488498966758 ) ) ;
#28130 = CARTESIAN_POINT ( 'NONE',  ( 2.977408999572651815, -16.81250000204838457, 7.188101187500000933 ) ) ;
#28131 = CARTESIAN_POINT ( 'NONE',  ( 73.33904886068935980, 4.000000000000013323, 0.000000000000000000 ) ) ;
#28132 = LINE ( 'NONE', #37819, #106418 ) ;
#28133 = LINE ( 'NONE', #71196, #91193 ) ;
#28134 = CARTESIAN_POINT ( 'NONE',  ( -11.57268198878043286, -4.922585413835529167, -12.56430962643118399 ) ) ;
#28135 = CARTESIAN_POINT ( 'NONE',  ( -6.500000000000007105, 3.752776749732553707, -6.177802698399951886 ) ) ;
#28136 = CARTESIAN_POINT ( 'NONE',  ( -8.343637927466835080, 120.5097608953729775, 1.301042606982606110E-15 ) ) ;
#28137 = CARTESIAN_POINT ( 'NONE',  ( -15.89400772911371540, 45.88919441563189849, -6.421120341668841824 ) ) ;
#28138 = EDGE_CURVE ( 'NONE', #22950, #91205, #67887, .T. ) ;
#28139 = CARTESIAN_POINT ( 'NONE',  ( 36.87655955837855259, 438.2068510013161813, 3.933030107424693167 ) ) ;
#28140 = CARTESIAN_POINT ( 'NONE',  ( -30.44433818822805549, -53.38490099487817986, 35.76380123852791826 ) ) ;
#28141 = DIRECTION ( 'NONE',  ( -1.000000000000000000, -1.224606353822377258E-16, -0.000000000000000000 ) ) ;
#28142 = CARTESIAN_POINT ( 'NONE',  ( 48.60192115950092528, -46.43965766730325129, 50.71851945537365935 ) ) ;
#28143 = CARTESIAN_POINT ( 'NONE',  ( -27.10511071441333542, 36.88665068479732412, -7.556984339679825524 ) ) ;
#28144 = DIRECTION ( 'NONE',  ( 0.000000000000000000, 0.000000000000000000, 1.000000000000000000 ) ) ;
#28146 = ADVANCED_FACE ( 'NONE', ( #64709 ), #79820, .T. ) ;
#28145 = CARTESIAN_POINT ( 'NONE',  ( -101.6512650445923498, -38.44858725811527478, 199.8639472654733424 ) ) ;
#28147 = ORIENTED_EDGE ( 'NONE', *, *, #91657, .T. ) ;
#28149 = CARTESIAN_POINT ( 'NONE',  ( -28.35801031271196138, 36.30512300106359191, 8.950586257191373463 ) ) ;
#28148 = CARTESIAN_POINT ( 'NONE',  ( 0.000000000000000000, 0.000000000000000000, -13.00000000000000000 ) ) ;
#28150 = CARTESIAN_POINT ( 'NONE',  ( 14.77355847997981364, 5.782273590395790919, -6.926453096434407541 ) ) ;
#28151 = CARTESIAN_POINT ( 'NONE',  ( -19.27294821357206089, 49.83929858697661786, 61.40513943499198035 ) ) ;
#28152 =( NAMED_UNIT ( * ) SI_UNIT ( $, .STERADIAN. ) SOLID_ANGLE_UNIT ( ) );
#28153 = CYLINDRICAL_SURFACE ( 'NONE', #106338, 1.250000000000001110 ) ;
#28154 = CARTESIAN_POINT ( 'NONE',  ( -33.16955188770710095, 434.2034342956006299, 15.24725034886469466 ) ) ;
#28155 = CARTESIAN_POINT ( 'NONE',  ( 42.54181027558946226, 465.0722614357431439, 13.76085909084874892 ) ) ;
#28156 = CARTESIAN_POINT ( 'NONE',  ( 31.53897358591923350, 437.3651574122892498, 21.86285002934833699 ) ) ;
#28157 = CARTESIAN_POINT ( 'NONE',  ( 112.1206467272125451, -60.00000000000000711, 177.5187025037823219 ) ) ;
#28158 = EDGE_CURVE ( 'NONE', #103960, #59016, #74817, .T. ) ;
#28159 = CONICAL_SURFACE ( 'NONE', #96951, 4.000000000000007105, 0.9599310885968835860 ) ;
#28160 = CARTESIAN_POINT ( 'NONE',  ( -7.343637806710342275, -67.44363121900617841, 3.177475076494675310 ) ) ;
#28161 = ORIENTED_EDGE ( 'NONE', *, *, #4688, .T. ) ;
#28162 = EDGE_CURVE ( 'NONE', #28989, #32993, #55856, .T. ) ;
#28163 = FILL_AREA_STYLE_COLOUR ( '', #25202 ) ;
#28164 = CARTESIAN_POINT ( 'NONE',  ( -100.9645298483791578, -29.99999999999999289, 165.4281941735794987 ) ) ;
#28165 = VERTEX_POINT ( 'NONE', #64196 ) ;
#28167 = CARTESIAN_POINT ( 'NONE',  ( 5.294000222838083580, 18.59362110858084804, -37.95364038139827301 ) ) ;
#28166 = CARTESIAN_POINT ( 'NONE',  ( -90.66027514559715428, -38.50790017717925195, 200.7323953230764459 ) ) ;
#28168 = CARTESIAN_POINT ( 'NONE',  ( 12.45023096947980967, -3.972485752774072676, -13.21587846007173361 ) ) ;
#28169 = CARTESIAN_POINT ( 'NONE',  ( 5.691929483231186637, -5.629165124598852543, 3.250000000000002220 ) ) ;
#28170 = CARTESIAN_POINT ( 'NONE',  ( -3.140956913508186954, -4.999999999999999112, -16.11495416415134940 ) ) ;
#28171 = PRESENTATION_LAYER_ASSIGNMENT (  '', '', ( #12631 ) ) ;
#28172 = CARTESIAN_POINT ( 'NONE',  ( 4.401442555609581635E-16, -13.15625000204838280, -7.188101187500000044 ) ) ;
#28173 = SURFACE_SIDE_STYLE ('',( #53475 ) ) ;
#28174 = DIRECTION ( 'NONE',  ( -1.000000000000000000, -1.224606353822377258E-16, -0.000000000000000000 ) ) ;
#28176 = ORIENTED_EDGE ( 'NONE', *, *, #17746, .T. ) ;
#28175 = CARTESIAN_POINT ( 'NONE',  ( -33.22740183690338256, 464.7219767745360173, 9.606361102862551959 ) ) ;
#28177 = CARTESIAN_POINT ( 'NONE',  ( 82.60770557527793301, -42.97231573429220219, 171.7383286845875148 ) ) ;
#28178 = DIRECTION ( 'NONE',  ( -1.000000000000000000, -1.224606353822377258E-16, -0.000000000000000000 ) ) ;
#28179 = DIRECTION ( 'NONE',  ( -1.000000000000000000, -0.000000000000000000, -0.000000000000000000 ) ) ;
#28180 = ORIENTED_EDGE ( 'NONE', *, *, #66628, .F. ) ;
#28181 = DIRECTION ( 'NONE',  ( 0.000000000000000000, 1.000000000000000000, 0.000000000000000000 ) ) ;
#28182 = CIRCLE ( 'NONE', #88426, 7.000000000000000000 ) ;
#28183 = FACE_OUTER_BOUND ( 'NONE', #22800, .T. ) ;
#28184 = CARTESIAN_POINT ( 'NONE',  ( 20.00000000000000000, 12.99999999999999289, 4.000000000000000000 ) ) ;
#28185 =( NAMED_UNIT ( * ) PLANE_ANGLE_UNIT ( ) SI_UNIT ( $, .RADIAN. ) );
#28186 = FACE_OUTER_BOUND ( 'NONE', #2540, .T. ) ;
#28187 =( BOUNDED_CURVE ( )  B_SPLINE_CURVE ( 2, ( #67145, #49881, #75212 ),
 .UNSPECIFIED., .F., .T. ) 
 B_SPLINE_CURVE_WITH_KNOTS ( ( 3, 3 ),
 ( 0.000000000000000000, 1.000000000000000000 ),
 .UNSPECIFIED. ) 
 CURVE ( )  GEOMETRIC_REPRESENTATION_ITEM ( )  RATIONAL_B_SPLINE_CURVE ( ( 1.000000000000000000, 1.857142857142858317, 1.000000000000000000 ) ) 
 REPRESENTATION_ITEM ( '' )  );
#28189 = CARTESIAN_POINT ( 'NONE',  ( 0.6187927933819248327, 18.48342808587748820, 49.40998285506532994 ) ) ;
#28188 = CIRCLE ( 'NONE', #59187, 5.000000000000002665 ) ;
#28190 = CARTESIAN_POINT ( 'NONE',  ( 58.18888888888888999, -3.309500000000000774, 0.000000000000000000 ) ) ;
#28191 = ADVANCED_FACE ( 'NONE', ( #97065 ), #97579, .F. ) ;
#28192 = ORIENTED_EDGE ( 'NONE', *, *, #78967, .F. ) ;
#28193 = COLOUR_RGB ( '', 0.66274510, 0.83137255, 0.94901961) ;
#28194 = VECTOR ( 'NONE', #9978, 1000.000000000000000 ) ;
#28195 = VECTOR ( 'NONE', #3191, 1000.000000000000000 ) ;
#28196 = CARTESIAN_POINT ( 'NONE',  ( -2.360737205864155364, 300.9840656762371509, 9.719989882648539137 ) ) ;
#28197 = LINE ( 'NONE', #21171, #46182 ) ;
#28198 = DIRECTION ( 'NONE',  ( -0.5735764363510497121, 0.8191520442889892450, 1.003171929053521665E-16 ) ) ;
#28199 = EDGE_CURVE ( 'NONE', #49452, #62342, #56198, .T. ) ;
#28201 = CYLINDRICAL_SURFACE ( 'NONE', #37859, 5.000000000000002665 ) ;
#28200 = CARTESIAN_POINT ( 'NONE',  ( 34.10284876471455817, -5.000000000000000000, 6.123233995736768255E-16 ) ) ;
#28202 = CARTESIAN_POINT ( 'NONE',  ( -2.977408999572650039, -27.68750000204838813, -7.188101187500001821 ) ) ;
#28203 = CARTESIAN_POINT ( 'NONE',  ( 16.39985520464312785, 294.5680733035314915, -10.06030923778802411 ) ) ;
#28204 = CARTESIAN_POINT ( 'NONE',  ( -34.92499999999994742, 0.000000000000000000, 0.000000000000000000 ) ) ;
#28205 = CARTESIAN_POINT ( 'NONE',  ( -7.500000000000000000, -4.330127018922201643, -7.422398894150036064 ) ) ;
#28206 = ITEM_DEFINED_TRANSFORMATION ( 'NONE', 'NONE', #11110,  #10728 ) ;
#28207 = ORIENTED_EDGE ( 'NONE', *, *, #11033, .F. ) ;
#28208 = EDGE_CURVE ( 'NONE', #17199, #28900, #66544, .T. ) ;
#28209 = DIRECTION ( 'NONE',  ( 0.000000000000000000, -1.000000000000000000, 0.000000000000000000 ) ) ;
#28210 = CARTESIAN_POINT ( 'NONE',  ( 3.643324519380566085E-15, 34.17188553058033307, 29.75000000000000355 ) ) ;
#28211 = CARTESIAN_POINT ( 'NONE',  ( -2.989615061350497260, 50.26451032649107020, -4.999999999999999112 ) ) ;
#28212 = DIRECTION ( 'NONE',  ( 0.000000000000000000, 0.000000000000000000, 1.000000000000000000 ) ) ;
#28213 = ORIENTED_EDGE ( 'NONE', *, *, #72104, .T. ) ;
#28214 = FACE_BOUND ( 'NONE', #55252, .T. ) ;
#28215 = CARTESIAN_POINT ( 'NONE',  ( -10.74465425724631373, 49.99999999999999289, -95.72854256506849424 ) ) ;
#28216 = ORIENTED_EDGE ( 'NONE', *, *, #102114, .T. ) ;
#28217 = CARTESIAN_POINT ( 'NONE',  ( 32.52812566731132904, 435.6745906244506159, 17.82476273229491426 ) ) ;
#28218 = DIRECTION ( 'NONE',  ( 0.000000000000000000, -1.000000000000000000, 0.000000000000000000 ) ) ;
#28219 = CARTESIAN_POINT ( 'NONE',  ( 9.698972129396508990, 101.8237028725806113, -2.445345647270323663 ) ) ;
#28220 = CARTESIAN_POINT ( 'NONE',  ( -111.9121283550977637, -60.00000000000000000, 180.8211707975872287 ) ) ;
#28221 = CARTESIAN_POINT ( 'NONE',  ( 19.35735956073687802, 49.90708382027017365, 61.17470024478517132 ) ) ;
#28222 = CARTESIAN_POINT ( 'NONE',  ( 43.94716957229235987, 463.1429429498418813, 4.278538522906490726 ) ) ;
#28223 = CARTESIAN_POINT ( 'NONE',  ( -84.56571597818337693, -39.40317381275280439, 181.6710895502921232 ) ) ;
#28224 = CIRCLE ( 'NONE', #71291, 0.9999999999999966693 ) ;
#28225 = CARTESIAN_POINT ( 'NONE',  ( -4.959717421002378224, 53.54742482023647909, -8.497505399302097473 ) ) ;
#28226 =( GEOMETRIC_REPRESENTATION_CONTEXT ( 3 ) GLOBAL_UNCERTAINTY_ASSIGNED_CONTEXT ( ( #27692 ) ) GLOBAL_UNIT_ASSIGNED_CONTEXT ( ( #49666, #6545, #105259 ) ) REPRESENTATION_CONTEXT ( 'NONE', 'WORKASPACE' ) );
#28227 = ORIENTED_EDGE ( 'NONE', *, *, #88787, .F. ) ;
#28228 = CARTESIAN_POINT ( 'NONE',  ( -10.11986806485388080, 46.15873290010527086, -12.90779740156157374 ) ) ;
#28229 = EDGE_CURVE ( 'NONE', #35708, #89211, #102737, .T. ) ;
#28230 = CARTESIAN_POINT ( 'NONE',  ( 3.707709148203173655, -1.099523832062987871, 104.5934084724869564 ) ) ;
#28231 = CARTESIAN_POINT ( 'NONE',  ( -85.28888020613797494, -52.70782351190823078, 1.970730064499419676 ) ) ;
#28233 = B_SPLINE_CURVE_WITH_KNOTS ( 'NONE', 3,
 ( #101787, #27419, #44092, #94240, #100718, #35495, #43556, #43027, #92630, #36040, #3095, #69959, #102319, #51091, #77522, #76437, #60298, #2017, #28470, #68912, #27954, #18787 ),
 .UNSPECIFIED., .F., .F.,
 ( 4, 2, 2, 2, 2, 2, 2, 2, 2, 2, 4 ),
 ( 0.000000000000000000, 0.001418111674391761513, 0.002127167511587641727, 0.002836223348783521725, 0.003545279185979403024, 0.004254335023175285189, 0.005672446697567033909, 0.007090558371958782628, 0.008508670046350530480, 0.009926781720742280934, 0.01134489339513402965 ),
 .UNSPECIFIED. ) ;
#28232 = CARTESIAN_POINT ( 'NONE',  ( -32.12146351642663689, 487.8665243855083986, 8.631703203532680391 ) ) ;
#28234 = CARTESIAN_POINT ( 'NONE',  ( 8.986743721355239245, 136.5670193725957233, -5.000000000000612843 ) ) ;
#28235 = CARTESIAN_POINT ( 'NONE',  ( -5.979482036612522755, -14.26481676427878398, 14.07238976267243835 ) ) ;
#28236 = CARTESIAN_POINT ( 'NONE',  ( 11.85444436786839084, 42.00000000000000000, -90.56128410203886858 ) ) ;
#28237 = ADVANCED_FACE ( 'NONE', ( #53770 ), #45690, .T. ) ;
#28238 = CARTESIAN_POINT ( 'NONE',  ( 64.81979848413079992, -29.99999999999996803, 107.4021778588664375 ) ) ;
#28239 =( NAMED_UNIT ( * ) PLANE_ANGLE_UNIT ( ) SI_UNIT ( $, .RADIAN. ) );
#28240 = CARTESIAN_POINT ( 'NONE',  ( -94.98233504546384154, -60.00000000000004263, -11.07720828487985720 ) ) ;
#28241 = CARTESIAN_POINT ( 'NONE',  ( -76.26205980810522078, -25.60539408125360339, 115.8660843457751213 ) ) ;
#28242 = ORIENTED_EDGE ( 'NONE', *, *, #3704, .T. ) ;
#28243 = CARTESIAN_POINT ( 'NONE',  ( 100.5651899622199039, -60.00000000000009948, 204.3456409986242477 ) ) ;
#28244 = CARTESIAN_POINT ( 'NONE',  ( 28.77239501610283412, 40.83805528215972203, 58.36093113040321612 ) ) ;
#28245 = CARTESIAN_POINT ( 'NONE',  ( 27.95186532817653458, -57.67113474561467257, -43.11548192448071148 ) ) ;
#28246 = ORIENTED_EDGE ( 'NONE', *, *, #70013, .F. ) ;
#28247 = DIRECTION ( 'NONE',  ( -0.000000000000000000, -1.000000000000000000, -0.000000000000000000 ) ) ;
#28248 = CARTESIAN_POINT ( 'NONE',  ( 7.188101187500000933, -28.43750000204839523, -2.977408999572650483 ) ) ;
#28249 = CARTESIAN_POINT ( 'NONE',  ( -5.383284837158154978, -6.999506564842242540, 2.657356347551693254 ) ) ;
#28250 = EDGE_LOOP ( 'NONE', ( #12076, #3690 ) ) ;
#28251 = CARTESIAN_POINT ( 'NONE',  ( 38.54515645702225868, 1.482358050883964840E-15, 0.000000000000000000 ) ) ;
#28252 = ORIENTED_EDGE ( 'NONE', *, *, #104265, .F. ) ;
#28253 = CARTESIAN_POINT ( 'NONE',  ( -3.750000000000007105, 6.495190528383286477, 1.734723475976807094E-15 ) ) ;
#28254 = CARTESIAN_POINT ( 'NONE',  ( 46.78576055570671599, 18.82161635153732959, -15.45372055756656948 ) ) ;
#28255 = CARTESIAN_POINT ( 'NONE',  ( -92.16331255555544999, -59.99999999999997158, 22.02966310501888003 ) ) ;
#28256 = FACE_BOUND ( 'NONE', #27559, .T. ) ;
#28257 = CARTESIAN_POINT ( 'NONE',  ( 7.188101187500001821, -10.06250000204838280, -2.977408999572650483 ) ) ;
#28258 = CARTESIAN_POINT ( 'NONE',  ( -48.69302668856963123, 13.59112006856911670, 16.66703530934380240 ) ) ;
#28259 = VECTOR ( 'NONE', #13265, 1000.000000000000000 ) ;
#28260 = FACE_OUTER_BOUND ( 'NONE', #32200, .T. ) ;
#28261 = FILL_AREA_STYLE ('',( #36363 ) ) ;
#28262 = CARTESIAN_POINT ( 'NONE',  ( 1.570796324980112679, 50.00000000000000000, -97.00000000000000000 ) ) ;
#28263 = DIRECTION ( 'NONE',  ( 0.000000000000000000, 1.000000000000000000, 0.000000000000000000 ) ) ;
#28264 = CARTESIAN_POINT ( 'NONE',  ( 42.11386565848213337, 436.0925768526452089, 7.550517934394086694 ) ) ;
#28265 = EDGE_CURVE ( 'NONE', #75460, #77482, #71018, .T. ) ;
#28266 = AXIS2_PLACEMENT_3D ( 'NONE', #90612, #15650, #16183 ) ;
#28267 = VERTEX_POINT ( 'NONE', #13831 ) ;
#28268 = CARTESIAN_POINT ( 'NONE',  ( 4.526657684027824757, -2.093347780961849036, 103.5746540667394555 ) ) ;
#28269 = AXIS2_PLACEMENT_3D ( 'NONE', #36802, #94488, #20643 ) ;
#28270 = CARTESIAN_POINT ( 'NONE',  ( 32.30020061510025897, -18.68143019929715365, 30.13538509804329735 ) ) ;
#28271 =( NAMED_UNIT ( * ) SI_UNIT ( $, .STERADIAN. ) SOLID_ANGLE_UNIT ( ) );
#28272 = EDGE_LOOP ( 'NONE', ( #12106, #1135, #104252, #78407 ) ) ;
#28274 = CARTESIAN_POINT ( 'NONE',  ( -35.66932529116966322, 438.9565575286536045, 4.011496722538590909 ) ) ;
#28273 = CARTESIAN_POINT ( 'NONE',  ( -26.49239580055373366, 34.70527438946334797, -9.907946246971482296 ) ) ;
#28275 = CARTESIAN_POINT ( 'NONE',  ( -1.727368016638141196E-09, 38.95322581935191408, 63.66965480466879512 ) ) ;
#28276 = CARTESIAN_POINT ( 'NONE',  ( -19.24689719943499355, 294.6758623120367133, -10.03739701883414526 ) ) ;
#28277 = CARTESIAN_POINT ( 'NONE',  ( -7.500000000000000000, -3.000000000000000000, -20.99851272547259384 ) ) ;
#28278 = FACE_OUTER_BOUND ( 'NONE', #94851, .T. ) ;
#28279 = CARTESIAN_POINT ( 'NONE',  ( 4.681380154937392568, -50.73787295680594411, 103.7259032015043090 ) ) ;
#28280 = EDGE_LOOP ( 'NONE', ( #83904, #81409, #3547, #32017 ) ) ;
#28281 = CARTESIAN_POINT ( 'NONE',  ( 92.68696368336701141, -60.00000000000000711, -4.489033240709536798 ) ) ;
#28282 = CARTESIAN_POINT ( 'NONE',  ( -11.04468709431030149, 45.87751353276775035, -13.15154111190464548 ) ) ;
#28283 = SURFACE_STYLE_USAGE ( .BOTH. , #43894 ) ;
#28284 = CARTESIAN_POINT ( 'NONE',  ( -36.62762355347277321, 370.6867356965224189, 4.048972153900439963 ) ) ;
#28285 = CARTESIAN_POINT ( 'NONE',  ( -6.561889531081967597, 40.92548620270399340, -71.07459846643517665 ) ) ;
#28286 = DIRECTION ( 'NONE',  ( 0.000000000000000000, 0.000000000000000000, -1.000000000000000000 ) ) ;
#28287 = ORIENTED_EDGE ( 'NONE', *, *, #38414, .F. ) ;
#28288 = MECHANICAL_DESIGN_GEOMETRIC_PRESENTATION_REPRESENTATION (  '', ( #23114 ), #31656 ) ;
#28289 = CARTESIAN_POINT ( 'NONE',  ( -103.6855961668380388, -29.99999999989386978, 118.5309966294316126 ) ) ;
#28290 = EDGE_LOOP ( 'NONE', ( #91961, #102693, #58325, #102240, #30202 ) ) ;
#28291 =( NAMED_UNIT ( * ) SI_UNIT ( $, .STERADIAN. ) SOLID_ANGLE_UNIT ( ) );
#28292 = CARTESIAN_POINT ( 'NONE',  ( 66.26095113931063452, 6.856755485862130937E-15, 0.000000000000000000 ) ) ;
#28293 = DIRECTION ( 'NONE',  ( -0.7071067811865530128, 0.000000000000000000, 0.7071067811865421326 ) ) ;
#28294 = CARTESIAN_POINT ( 'NONE',  ( 14.89085744133905109, 23.12183015427916999, -0.5456866263682997875 ) ) ;
#28295 = CARTESIAN_POINT ( 'NONE',  ( 84.14220056850236062, -52.73722939407674204, -14.99994838795616658 ) ) ;
#28296 = CARTESIAN_POINT ( 'NONE',  ( 7.188101187500001821, -31.43750000204839168, -2.977408999572650483 ) ) ;
#28297 = CARTESIAN_POINT ( 'NONE',  ( -17.49999999999997513, 45.00000000000000711, 64.09953197936602010 ) ) ;
#28298 = CARTESIAN_POINT ( 'NONE',  ( 9.058657501722350958, 46.09928351899775123, -13.86902144048109697 ) ) ;
#28299 = ORIENTED_EDGE ( 'NONE', *, *, #22367, .F. ) ;
#28300 = DIRECTION ( 'NONE',  ( 1.000000000000000000, 0.000000000000000000, -1.224646799147353207E-16 ) ) ;
#28301 = ORIENTED_EDGE ( 'NONE', *, *, #40516, .T. ) ;
#28302 = CARTESIAN_POINT ( 'NONE',  ( 49.13349184603276854, 7.785586125543622948, -16.19411946323722873 ) ) ;
#28303 = CIRCLE ( 'NONE', #19767, 3.309500000000001663 ) ;
#28305 = ORIENTED_EDGE ( 'NONE', *, *, #89175, .T. ) ;
#28304 = FACE_OUTER_BOUND ( 'NONE', #74034, .T. ) ;
#28306 = CARTESIAN_POINT ( 'NONE',  ( 80.38791889184808781, -29.09062692944559458, 137.3129237731349974 ) ) ;
#28307 = EDGE_LOOP ( 'NONE', ( #77831, #18050, #42200, #50820 ) ) ;
#28308 = CARTESIAN_POINT ( 'NONE',  ( 2.268390192474211364, -49.89683323521570202, 40.92072922013065295 ) ) ;
#28309 = CARTESIAN_POINT ( 'NONE',  ( -7.188101187500000044, -21.40625000204838457, -8.802885111219163269E-16 ) ) ;
#28310 = CARTESIAN_POINT ( 'NONE',  ( -92.76516906498835624, -57.61752273625296539, 204.4213914816233739 ) ) ;
#28311 = EDGE_CURVE ( 'NONE', #50990, #80843, #23970, .T. ) ;
#28312 = ORIENTED_EDGE ( 'NONE', *, *, #42087, .T. ) ;
#28313 = CARTESIAN_POINT ( 'NONE',  ( 4.678819457397437986, 8.078722181090837395, 5.000000000000000000 ) ) ;
#28314 = DIRECTION ( 'NONE',  ( 0.000000000000000000, 0.000000000000000000, 1.000000000000000000 ) ) ;
#28315 = EDGE_CURVE ( 'NONE', #44644, #100880, #75149, .T. ) ;
#28316 = DIRECTION ( 'NONE',  ( -1.000000000000000000, -1.224606353822377258E-16, -0.000000000000000000 ) ) ;
#28317 = CARTESIAN_POINT ( 'NONE',  ( 8.000000000000000000, -17.09375000409676915, -3.313708498984761608 ) ) ;
#28318 = CARTESIAN_POINT ( 'NONE',  ( -49.54284130610121650, -29.59840805727827018, 45.89079715898707690 ) ) ;
#28319 = CARTESIAN_POINT ( 'NONE',  ( -2.499999999999911182, -27.33278205846447406, -31.42875897075158420 ) ) ;
#28320 = CARTESIAN_POINT ( 'NONE',  ( -45.99999999995579003, 486.5369520445917146, 4.408549137160468590 ) ) ;
#28321 = CARTESIAN_POINT ( 'NONE',  ( -37.85084083633360308, 438.0234350436312525, 4.171260309356210172 ) ) ;
#28322 = DIRECTION ( 'NONE',  ( -1.000000000000000000, -1.224606353822377258E-16, -0.000000000000000000 ) ) ;
#28324 = AXIS2_PLACEMENT_3D ( 'NONE', #62006, #45277, #71642 ) ;
#28323 = SHAPE_DEFINITION_REPRESENTATION ( #76852, #66748 ) ;
#28325 = CARTESIAN_POINT ( 'NONE',  ( 31.46253585067004721, -4.999999999999990230, 0.000000000000000000 ) ) ;
#28326 = ORIENTED_EDGE ( 'NONE', *, *, #32198, .F. ) ;
#28327 = CARTESIAN_POINT ( 'NONE',  ( -4.009756559019359123, -48.64709516568132130, 43.57946810439663210 ) ) ;
#28328 = EDGE_CURVE ( 'NONE', #48464, #91003, #39001, .T. ) ;
#28329 = CARTESIAN_POINT ( 'NONE',  ( 0.000000000000000000, -100.0000000000000000, -10.00000000000001954 ) ) ;
#28330 = CARTESIAN_POINT ( 'NONE',  ( 0.000000000000000000, -30.00000000000000000, 0.000000000000000000 ) ) ;
#28331 = CARTESIAN_POINT ( 'NONE',  ( -50.11359024763238068, -27.54911214440137357, -27.96617461654303227 ) ) ;
#28332 = CARTESIAN_POINT ( 'NONE',  ( -84.86247741117115595, -30.00000000000000355, 169.0207004501273786 ) ) ;
#28333 = AXIS2_PLACEMENT_3D ( 'NONE', #78958, #102712, #77375 ) ;
#28334 = B_SPLINE_CURVE_WITH_KNOTS ( 'NONE', 3,
 ( #27615, #11907, #3834, #1683 ),
 .UNSPECIFIED., .F., .F.,
 ( 4, 4 ),
 ( 2.122407100861210359E-17, 0.0007940539003705733134 ),
 .UNSPECIFIED. ) ;
#28335 = ORIENTED_EDGE ( 'NONE', *, *, #73401, .F. ) ;
#28336 = CARTESIAN_POINT ( 'NONE',  ( 1.284594766674681532, -49.99999999999997868, 44.94053020278990118 ) ) ;
#28337 = CARTESIAN_POINT ( 'NONE',  ( 75.27064724514200122, -57.56701362099152419, 191.4025409768277370 ) ) ;
#28338 = CARTESIAN_POINT ( 'NONE',  ( 9.739726766683151737, 48.00000000000000711, -87.61747884359282068 ) ) ;
#28339 = CARTESIAN_POINT ( 'NONE',  ( 28.36231118427504327, -28.96865690853695341, -38.25004534194034989 ) ) ;
#28340 = SURFACE_STYLE_USAGE ( .BOTH. , #94662 ) ;
#28341 = CARTESIAN_POINT ( 'NONE',  ( 2.617478843592800697, -3.000000000000003109, -75.26027323331686603 ) ) ;
#28342 = CARTESIAN_POINT ( 'NONE',  ( -72.02742768976531806, -59.99999999999998579, 154.4823517272751303 ) ) ;
#28343 = CARTESIAN_POINT ( 'NONE',  ( -1.098735407080559279, 7.248058225761153217, -6.326622577871103381 ) ) ;
#28344 =( NAMED_UNIT ( * ) SI_UNIT ( $, .STERADIAN. ) SOLID_ANGLE_UNIT ( ) );
#28345 = CARTESIAN_POINT ( 'NONE',  ( -86.12932764275537068, -28.31670544872752160, 182.7863807612648941 ) ) ;
#28346 = ORIENTED_EDGE ( 'NONE', *, *, #59568, .T. ) ;
#28347 = CARTESIAN_POINT ( 'NONE',  ( -41.50820411079205741, 461.5963371455321749, 2.703439750996430302 ) ) ;
#28348 = CARTESIAN_POINT ( 'NONE',  ( -2.014047270709469650, -39.47599645772569232, 30.46658341959906480 ) ) ;
#28349 = CARTESIAN_POINT ( 'NONE',  ( -6.780293022259969327, 41.80198833643462564, -59.33023405483342572 ) ) ;
#28350 = B_SPLINE_SURFACE_WITH_KNOTS ( 'NONE', 1, 3, ( 
 ( #58430, #16364, #65459, #99387, #73525, #105898, #48719, #98351, #8803, #15837, #16915, #7734, #91339, #24506, #32049, #7209, #97812, #57340, #89208, #82697, #90261, #40118, #33116, #74593, #82156, #670, #81096, #41711 ),
 ( #15307, #33634, #66515, #17453, #97281, #81607, #8269, #50319, #41182, #83225, #74060, #72993, #65983, #64926, #9319, #42230, #105387, #31527, #64408, #23433, #23977, #56818, #89742, #77270, #42768, #85914, #69193, #34182 ) ),
 .UNSPECIFIED., .F., .F., .F.,
 ( 2, 2 ),
 ( 4, 2, 2, 2, 2, 2, 2, 2, 2, 2, 2, 2, 2, 4 ),
 ( 0.000000000000000000, 1.000000000000000000 ),
 ( 0.08901491201581737678, 0.1032490540155679704, 0.1174831960153185778, 0.1317173380150691853, 0.1459514800148197788, 0.1744197640143299588, 0.2028880480138401388, 0.2598246160128514504, 0.3167611840118632616, 0.4306343200098861623, 0.5445074560079088410, 0.6583805920059359051, 0.7722537280039543095, 1.000000000000000000 ),
 .UNSPECIFIED. ) ;
#28351 = DIRECTION ( 'NONE',  ( -1.000000000000000000, 0.000000000000000000, 0.000000000000000000 ) ) ;
#28352 = ORIENTED_EDGE ( 'NONE', *, *, #97106, .T. ) ;
#28353 = ADVANCED_FACE ( 'NONE', ( #37101, #79633 ), #87216, .F. ) ;
#28356 = CARTESIAN_POINT ( 'NONE',  ( 29.87930712590254245, 10.71892156097790583, -14.93965356295128011 ) ) ;
#28355 = PRESENTATION_LAYER_ASSIGNMENT (  '', '', ( #30043 ) ) ;
#28354 = B_SPLINE_CURVE_WITH_KNOTS ( 'NONE', 3,
 ( #12434, #101465, #35161, #18992, #52912 ),
 .UNSPECIFIED., .F., .F.,
 ( 4, 1, 4 ),
 ( 0.000000000000000000, 0.003752776749732567464, 0.007505553499465134927 ),
 .UNSPECIFIED. ) ;
#28357 = B_SPLINE_CURVE_WITH_KNOTS ( 'NONE', 3,
 ( #1173, #19576, #3345, #100966, #18483, #27125, #17944, #58931, #83710, #60537, #60014, #51346, #92871, #2800, #42735, #52405, #19039, #84794, #51876, #85325, #43793, #35747, #68630, #11411, #99348, #25532, #91303, #17413, #50286, #83188, #11949, #4401, #86931, #63181, #14066, #55055 ),
 .UNSPECIFIED., .F., .F.,
 ( 4, 2, 2, 2, 2, 2, 2, 2, 2, 2, 2, 2, 2, 2, 2, 2, 2, 4 ),
 ( 0.01291936762762760545, 0.01372441420841340361, 0.01452946078919920177, 0.01533450736998499993, 0.01613955395077079635, 0.01694460053155659451, 0.01774964711234239267, 0.01855469369312819083, 0.01935974027391398899, 0.02016478685469979062, 0.02096983343548558879, 0.02177488001627139041, 0.02257992659705718858, 0.02338497317784298674, 0.02419001975862878837, 0.02459254304902168745, 0.02499506633941458306, 0.02580011292020054428 ),
 .UNSPECIFIED. ) ;
#28358 = DIRECTION ( 'NONE',  ( -1.000000000000000000, -1.224606353822377258E-16, -0.000000000000000000 ) ) ;
#28359 = FACE_OUTER_BOUND ( 'NONE', #51537, .T. ) ;
#28360 = FACE_OUTER_BOUND ( 'NONE', #57493, .T. ) ;
#28361 = ORIENTED_EDGE ( 'NONE', *, *, #95771, .T. ) ;
#28362 = CARTESIAN_POINT ( 'NONE',  ( 17.61979786233769829, 50.00000000000000711, 62.60467660056798422 ) ) ;
#28363 = CARTESIAN_POINT ( 'NONE',  ( 33.63427961064055438, 325.9154870834976236, -4.827994974213513757 ) ) ;
#28364 = ADVANCED_FACE ( 'NONE', ( #37638 ), #71680, .T. ) ;
#28365 = EDGE_CURVE ( 'NONE', #95805, #103579, #67218, .T. ) ;
#28366 = CARTESIAN_POINT ( 'NONE',  ( 9.668542035780198773, 53.51952571152754246, -2.198707408830915533 ) ) ;
#28367 = CARTESIAN_POINT ( 'NONE',  ( 91.97789438503755832, -14.21045842199438880, 64.70176211216229945 ) ) ;
#28368 = CARTESIAN_POINT ( 'NONE',  ( -82.38381349158181877, -29.09245844371520917, 149.5394180625729916 ) ) ;
#28369 = PRESENTATION_LAYER_ASSIGNMENT (  '', '', ( #48943 ) ) ;
#28370 = ORIENTED_EDGE ( 'NONE', *, *, #49995, .F. ) ;
#28371 = CARTESIAN_POINT ( 'NONE',  ( 42.18756898894579876, 484.4522853017719513, -2.425645685620453129 ) ) ;
#28372 = CARTESIAN_POINT ( 'NONE',  ( 5.909259836070535954, 253.8627720424205734, -1.072443315311453649 ) ) ;
#28373 = CARTESIAN_POINT ( 'NONE',  ( 33.02302426302988181, -57.69141391618915549, 47.29285870251012369 ) ) ;
#28374 = AXIS2_PLACEMENT_3D ( 'NONE', #88585, #98778, #16822 ) ;
#28375 = AXIS2_PLACEMENT_3D ( 'NONE', #59905, #33494, #44239 ) ;
#28376 = CARTESIAN_POINT ( 'NONE',  ( 43.55162665249213205, 368.5793226304579093, 13.69405092322887540 ) ) ;
#28377 = CARTESIAN_POINT ( 'NONE',  ( 34.76127829571465355, 469.3283515771897783, 1.881857718270027346 ) ) ;
#28378 = VERTEX_POINT ( 'NONE', #33261 ) ;
#28379 = PRESENTATION_LAYER_ASSIGNMENT (  '', '', ( #55860 ) ) ;
#28380 = CARTESIAN_POINT ( 'NONE',  ( 4.658253368731117838, 53.64149773577107538, -8.371863789803988709 ) ) ;
#28381 = DIRECTION ( 'NONE',  ( 1.000000000000000000, 1.224606353822377258E-16, 0.000000000000000000 ) ) ;
#28382 = CARTESIAN_POINT ( 'NONE',  ( -5.082755093536326818, -25.71875000204838813, 5.082755093536325042 ) ) ;
#28383 = ORIENTED_EDGE ( 'NONE', *, *, #45470, .F. ) ;
#28384 = PRESENTATION_STYLE_ASSIGNMENT (( #75827 ) ) ;
#28385 = EDGE_CURVE ( 'NONE', #85998, #82432, #45922, .T. ) ;
#28386 = CARTESIAN_POINT ( 'NONE',  ( -1.749942564367552134, 15.56091200510339512, 9.852211596319792264 ) ) ;
#28387 = LINE ( 'NONE', #19778, #62267 ) ;
#28388 = CARTESIAN_POINT ( 'NONE',  ( -51.78317192863611496, 49.99999999999999289, 39.73656039226784742 ) ) ;
#28389 = CARTESIAN_POINT ( 'NONE',  ( 12.50000000000000000, -2.999999999999996891, -14.34180675897363955 ) ) ;
#28390 = EDGE_CURVE ( 'NONE', #78191, #26284, #106166, .T. ) ;
#28391 = CARTESIAN_POINT ( 'NONE',  ( 16.75187969033571989, -1.200000000000000030E-05, 21.80698433968582961 ) ) ;
#28392 = ORIENTED_EDGE ( 'NONE', *, *, #77768, .F. ) ;
#28393 = CARTESIAN_POINT ( 'NONE',  ( 92.42253650716426705, -60.00000000000000000, -12.04573449290273501 ) ) ;
#28395 = CARTESIAN_POINT ( 'NONE',  ( 18.79022120343070057, -29.03183620043990487, 29.12074868831081886 ) ) ;
#28394 = CARTESIAN_POINT ( 'NONE',  ( -39.73689531673777964, -14.21045842199425735, 43.02931800076370195 ) ) ;
#28396 = CARTESIAN_POINT ( 'NONE',  ( 122.4708123290697444, 1.499999999999992450, -61.23540616453485086 ) ) ;
#28397 = EDGE_CURVE ( 'NONE', #98690, #32616, #21492, .T. ) ;
#28398 = CARTESIAN_POINT ( 'NONE',  ( -35.62035736894353732, -56.82933308392254190, 39.01374127240671896 ) ) ;
#28399 = ORIENTED_EDGE ( 'NONE', *, *, #97680, .T. ) ;
#28400 =( NAMED_UNIT ( * ) PLANE_ANGLE_UNIT ( ) SI_UNIT ( $, .RADIAN. ) );
#28401 = SURFACE_STYLE_USAGE ( .BOTH. , #13226 ) ;
#28402 = CARTESIAN_POINT ( 'NONE',  ( -43.58517788116170522, 464.0093709437825851, 6.089361716058439455 ) ) ;
#28403 = EDGE_CURVE ( 'NONE', #105826, #102392, #74123, .T. ) ;
#28404 = CARTESIAN_POINT ( 'NONE',  ( 0.000000000000000000, 300.0000000000000000, 9.936999415352289589 ) ) ;
#28405 = ORIENTED_EDGE ( 'NONE', *, *, #64836, .F. ) ;
#28406 = CARTESIAN_POINT ( 'NONE',  ( -50.50675741891196679, -38.33489965697940249, 69.68679463715933764 ) ) ;
#28407 = CARTESIAN_POINT ( 'NONE',  ( 14.83349330513380693, 1.593028355512270962E-15, 0.000000000000000000 ) ) ;
#28408 = CARTESIAN_POINT ( 'NONE',  ( 100.8461010101613056, -30.00000000000000711, 163.5864315675907790 ) ) ;
#28409 = CARTESIAN_POINT ( 'NONE',  ( 33.08652920850916956, 40.69826037889563253, -62.15288412041942934 ) ) ;
#28410 = DIRECTION ( 'NONE',  ( -1.000000000000000000, -1.224606353822377258E-16, -0.000000000000000000 ) ) ;
#28411 = CARTESIAN_POINT ( 'NONE',  ( 81.22126038271350978, -30.00000000000000000, 0.6198818140041580937 ) ) ;
#28412 = AXIS2_PLACEMENT_3D ( 'NONE', #59068, #19183, #26210 ) ;
#28413 = DIRECTION ( 'NONE',  ( 1.000000000000000000, 0.000000000000000000, -1.160749806054361473E-16 ) ) ;
#28414 = ORIENTED_EDGE ( 'NONE', *, *, #4528, .F. ) ;
#28415 = AXIS2_PLACEMENT_3D ( 'NONE', #76833, #34827, #19715 ) ;
#28416 = ORIENTED_EDGE ( 'NONE', *, *, #20157, .T. ) ;
#28417 = ORIENTED_EDGE ( 'NONE', *, *, #53965, .F. ) ;
#28418 = DIRECTION ( 'NONE',  ( -0.5735764363510494901, -0.8191520442889894671, 0.000000000000000000 ) ) ;
#28419 = CARTESIAN_POINT ( 'NONE',  ( 23.58349330513380337, 4.000000000000003553, 0.000000000000000000 ) ) ;
#28420 = CARTESIAN_POINT ( 'NONE',  ( -5.290067270632216712, -1.200000000000000030E-05, 6.031152949374556371 ) ) ;
#28421 = CARTESIAN_POINT ( 'NONE',  ( -43.61936128191153017, 427.3462587541194466, 15.28103652271592416 ) ) ;
#28422 = CARTESIAN_POINT ( 'NONE',  ( -31.31579387245123058, 439.0805111990142109, 22.75910752502478118 ) ) ;
#28423 = CARTESIAN_POINT ( 'NONE',  ( -7.344505440741524893, -87.44618927298701294, -3.175463080953003558 ) ) ;
#28424 = ORIENTED_EDGE ( 'NONE', *, *, #72187, .F. ) ;
#28425 = CARTESIAN_POINT ( 'NONE',  ( 1.224646799147352073E-15, 49.99999999999999289, -75.00000000000001421 ) ) ;
#28426 = ORIENTED_EDGE ( 'NONE', *, *, #33349, .F. ) ;
#28427 = CARTESIAN_POINT ( 'NONE',  ( 30.00000000000000000, 0.000000000000000000, 0.000000000000000000 ) ) ;
#28428 = CARTESIAN_POINT ( 'NONE',  ( 0.000000000000000000, 0.000000000000000000, 8.000000000000000000 ) ) ;
#28429 = CARTESIAN_POINT ( 'NONE',  ( -42.19179521602254823, 485.4956273777415277, -3.824025998169165330 ) ) ;
#28430 = CARTESIAN_POINT ( 'NONE',  ( 22.37268651138633402, 303.2941807803410370, 10.03209224172512748 ) ) ;
#28431 = CARTESIAN_POINT ( 'NONE',  ( -5.190609988845228173, 247.3607771325640385, -3.016375611400006651 ) ) ;
#28432 = CARTESIAN_POINT ( 'NONE',  ( 60.62648580738628112, -49.91109213625085772, 78.91779010420800944 ) ) ;
#28433 = EDGE_LOOP ( 'NONE', ( #63270, #527, #90316, #75731, #55245, #91788 ) ) ;
#28434 = CARTESIAN_POINT ( 'NONE',  ( 28.52985215182756917, 11.34625443571974657, -41.35275482200174224 ) ) ;
#28435 = CARTESIAN_POINT ( 'NONE',  ( 34.35000000000000142, 3.309500000000003439, 0.000000000000000000 ) ) ;
#28436 = CARTESIAN_POINT ( 'NONE',  ( -6.481635180341071667, 9.993697337156294935, -2.650895967029505140 ) ) ;
#28437 = CARTESIAN_POINT ( 'NONE',  ( 26.36650669486618881, 0.000000000000000000, 4.000000000000000888 ) ) ;
#28438 = EDGE_CURVE ( 'NONE', #61663, #15295, #13172, .T. ) ;
#28439 = CONICAL_SURFACE ( 'NONE', #85214, 0.6840402866513453084, 1.221730476396026610 ) ;
#28440 = EDGE_LOOP ( 'NONE', ( #63581, #4830 ) ) ;
#28442 = CARTESIAN_POINT ( 'NONE',  ( 30.00000000000000000, 461.8665070935973063, 11.40527499426175062 ) ) ;
#28441 =( NAMED_UNIT ( * ) SI_UNIT ( $, .STERADIAN. ) SOLID_ANGLE_UNIT ( ) );
#28443 = FILL_AREA_STYLE_COLOUR ( '', #39972 ) ;
#28444 = CARTESIAN_POINT ( 'NONE',  ( 98.59800593614012598, -2.002967142162725287E-29, 5.000000000000011546 ) ) ;
#28445 = ADVANCED_FACE ( 'NONE', ( #83913 ), #73686, .T. ) ;
#28446 = CARTESIAN_POINT ( 'NONE',  ( -7.897196874019794421, 101.2087279583219299, -1.302055520192093141 ) ) ;
#28448 = EDGE_CURVE ( 'NONE', #63004, #80882, #104417, .T. ) ;
#28447 = B_SPLINE_CURVE_WITH_KNOTS ( 'NONE', 3,
 ( #102956, #86261, #70589, #20503, #62504, #77618, #103479, #12860, #93801, #3194, #29119, #43646, #19958, #28042, #68470, #45260, #3735, #4259, #2646, #86789, #36664, #53341, #85174, #101360, #37188, #60391, #70050, #21020, #19430, #95391, #51730, #52800, #44730, #84647, #76535, #35593, #44190, #47359, #23644, #55437, #63030, #64622, #56500, #71628, #31221, #15520, #89429, #72173, #88891, #38761 ),
 .UNSPECIFIED., .F., .F.,
 ( 4, 2, 2, 2, 2, 2, 2, 2, 2, 2, 2, 2, 2, 2, 2, 2, 2, 2, 2, 2, 2, 2, 2, 2, 4 ),
 ( -6.000000000098130878E-08, 0.0005605446129132989497, 0.001121149225826598844, 0.002242358451653208608, 0.004484776903306437676, 0.005605986129133047439, 0.006727195354959656336, 0.007848404580786266099, 0.008969613806612876730, 0.01121203225826622636, 0.01233324148409289597, 0.01345445070991956732, 0.01569686916157306267, 0.01793928761322655802, 0.02242412451653353830, 0.02690896141984051512, 0.03587863522645447917, 0.05381798283968223379, 0.06278765664629612497, 0.07175733045291000922, 0.08072700425952387959, 0.08969667806613777772, 0.1076360256793653380, 0.1255753732925929123, 0.1435147209058204865 ),
 .UNSPECIFIED. ) ;
#28449 = PRESENTATION_LAYER_ASSIGNMENT (  '', '', ( #105917 ) ) ;
#28450 = FACE_OUTER_BOUND ( 'NONE', #77419, .T. ) ;
#28451 = DIRECTION ( 'NONE',  ( 0.000000000000000000, 1.000000000000000000, 0.000000000000000000 ) ) ;
#28452 = AXIS2_PLACEMENT_3D ( 'NONE', #94675, #86053, #3522 ) ;
#28453 = CARTESIAN_POINT ( 'NONE',  ( 86.38981295467488053, -17.31679843281874653, 180.1952732809204463 ) ) ;
#28454 = STYLED_ITEM ( 'NONE', ( #55382 ), #41599 ) ;
#28455 = DIRECTION ( 'NONE',  ( 0.000000000000000000, 0.000000000000000000, -1.000000000000000000 ) ) ;
#28456 = CARTESIAN_POINT ( 'NONE',  ( -7.989648714920444483, 50.29308867528581573, 0.000000000000000000 ) ) ;
#28457 = ORIENTED_EDGE ( 'NONE', *, *, #36837, .F. ) ;
#28458 = CONICAL_SURFACE ( 'NONE', #83528, 13.50000000000000178, 1.047197551196596077 ) ;
#28459 =( NAMED_UNIT ( * ) SI_UNIT ( $, .STERADIAN. ) SOLID_ANGLE_UNIT ( ) );
#28460 = LINE ( 'NONE', #29015, #72826 ) ;
#28461 = CARTESIAN_POINT ( 'NONE',  ( -46.00000000000000000, 450.0000000000002274, 13.20242257375370976 ) ) ;
#28462 = EDGE_CURVE ( 'NONE', #61410, #78701, #47031, .T. ) ;
#28463 = DIRECTION ( 'NONE',  ( -1.000000000000000000, -0.000000000000000000, -0.000000000000000000 ) ) ;
#28464 = EDGE_CURVE ( 'NONE', #45005, #51662, #101033, .T. ) ;
#28465 = CARTESIAN_POINT ( 'NONE',  ( -86.45353334008343893, -30.00000000000000000, 67.08143912832863975 ) ) ;
#28466 = CARTESIAN_POINT ( 'NONE',  ( 55.74444444444444713, 3.309500000000014541, 4.052968581778174646E-16 ) ) ;
#28467 = CARTESIAN_POINT ( 'NONE',  ( 24.14728948785597851, -57.67409579684246523, 42.95855127128432116 ) ) ;
#28469 = CARTESIAN_POINT ( 'NONE',  ( 16.96954359408614366, 304.5683848806726814, 9.876757081930351845 ) ) ;
#28468 = CARTESIAN_POINT ( 'NONE',  ( 35.15995658827085890, 490.3459154101568629, 12.17011141540134211 ) ) ;
#28470 = CARTESIAN_POINT ( 'NONE',  ( 6.836057901778168855, -47.88509835587553454, 39.21777279280524908 ) ) ;
#28471 = CARTESIAN_POINT ( 'NONE',  ( 41.85000000000000142, -3.309499999999999886, 0.000000000000000000 ) ) ;
#28472 = CARTESIAN_POINT ( 'NONE',  ( -17.97976569284698911, 49.99999999999999289, 61.91457000261350885 ) ) ;
#28473 = FACE_OUTER_BOUND ( 'NONE', #78034, .T. ) ;
#28474 = CARTESIAN_POINT ( 'NONE',  ( 0.000000000000000000, 0.000000000000000000, 4.000000000000000888 ) ) ;
#28475 = CARTESIAN_POINT ( 'NONE',  ( 39.55779653878227009, -24.73393910763277503, -30.38590686191570356 ) ) ;
#28476 = CARTESIAN_POINT ( 'NONE',  ( -25.24413934897445344, -49.91765848946642592, 33.57297437054807432 ) ) ;
#28477 = ORIENTED_EDGE ( 'NONE', *, *, #43950, .F. ) ;
#28478 = CARTESIAN_POINT ( 'NONE',  ( 40.49428179616492685, 485.6422782434408418, -4.370491944107985915 ) ) ;
#28479 = CARTESIAN_POINT ( 'NONE',  ( -10.00005432054556742, 109.0001358013791304, 0.2621623937322789533 ) ) ;
#28480 = CARTESIAN_POINT ( 'NONE',  ( -19.17790022078855827, -46.43920341883650593, 32.07300667617749923 ) ) ;
#28481 =( BOUNDED_SURFACE ( )  B_SPLINE_SURFACE ( 3, 2, ( 
 ( #98688, #90623, #49618 ),
 ( #56094, #82527, #42059 ),
 ( #41529, #74419, #494 ),
 ( #1035, #66881, #66337 ) ),
 .UNSPECIFIED., .F., .F., .T. ) 
 B_SPLINE_SURFACE_WITH_KNOTS ( ( 4, 4 ),
 ( 3, 3 ),
 ( 3.903127820947815962E-16, 0.0002239690292486364140 ),
 ( 0.000000000000000000, 1.000000000000000000 ),
 .UNSPECIFIED. ) 
 GEOMETRIC_REPRESENTATION_ITEM ( )  RATIONAL_B_SPLINE_SURFACE ( (
 ( 1.000000000000000000, 0.8238944711859870207, 1.000000000000000000),
 ( 1.000000000000000000, 0.8250855524373764682, 1.000000000000000000),
 ( 1.000000000000000000, 0.8262263977136614646, 1.000000000000000000),
 ( 1.000000000000000000, 0.8273155905872641158, 1.000000000000000000) ) ) 
 REPRESENTATION_ITEM ( '' )  SURFACE ( )  );
#28482 = CIRCLE ( 'NONE', #73146, 4.000000000000007105 ) ;
#28483 = CARTESIAN_POINT ( 'NONE',  ( 40.75856060348023391, 485.0489837854431698, -4.073182915998790676 ) ) ;
#28484 = ORIENTED_EDGE ( 'NONE', *, *, #33260, .F. ) ;
#28485 = VERTEX_POINT ( 'NONE', #295 ) ;
#28486 = VERTEX_POINT ( 'NONE', #100091 ) ;
#28487 = ADVANCED_FACE ( 'NONE', ( #100626 ), #84545, .F. ) ;
#28488 = CARTESIAN_POINT ( 'NONE',  ( -43.63933387927399821, 486.5321090506437827, 6.480556376458819656 ) ) ;
#28489 = ORIENTED_EDGE ( 'NONE', *, *, #6415, .T. ) ;
#28490 = CARTESIAN_POINT ( 'NONE',  ( 29.34999999999999787, 3.309500000000003439, 0.000000000000000000 ) ) ;
#28491 = CARTESIAN_POINT ( 'NONE',  ( 21.84999999999999787, 1.533819458162526451E-15, 0.000000000000000000 ) ) ;
#28492 = CARTESIAN_POINT ( 'NONE',  ( 103.2090184944486282, -60.16447056206801847, 192.4869700436993583 ) ) ;
#28494 = CARTESIAN_POINT ( 'NONE',  ( 0.000000000000000000, 0.000000000000000000, -9.974599999999998801 ) ) ;
#28493 = CARTESIAN_POINT ( 'NONE',  ( -13.49999999999999822, 0.6589394956329776010, 1.021521734388685814E-15 ) ) ;
#28495 = ORIENTED_EDGE ( 'NONE', *, *, #86457, .F. ) ;
#28496 = AXIS2_PLACEMENT_3D ( 'NONE', #39711, #14875, #97383 ) ;
#28497 = ORIENTED_EDGE ( 'NONE', *, *, #7614, .T. ) ;
#28498 = ORIENTED_EDGE ( 'NONE', *, *, #6384, .F. ) ;
#28499 = CARTESIAN_POINT ( 'NONE',  ( 23.26573150479070762, 305.7875708879445824, 9.141252083811004070 ) ) ;
#28500 = ADVANCED_FACE ( 'NONE', ( #37537 ), #57905, .T. ) ;
#28501 = DIRECTION ( 'NONE',  ( 0.000000000000000000, 0.000000000000000000, -1.000000000000000000 ) ) ;
#28502 = DIRECTION ( 'NONE',  ( -0.9508028509851106369, 0.1865215626109575919, -0.2473532802284052201 ) ) ;
#28503 = ORIENTED_EDGE ( 'NONE', *, *, #88138, .F. ) ;
#28504 =( GEOMETRIC_REPRESENTATION_CONTEXT ( 3 ) GLOBAL_UNCERTAINTY_ASSIGNED_CONTEXT ( ( #77428 ) ) GLOBAL_UNIT_ASSIGNED_CONTEXT ( ( #89013, #55550, #54487 ) ) REPRESENTATION_CONTEXT ( 'NONE', 'WORKASPACE' ) );
#28505 = FACE_OUTER_BOUND ( 'NONE', #52864, .T. ) ;
#28506 = CARTESIAN_POINT ( 'NONE',  ( -6.299401076687714429, 41.97741539014224088, -69.49222273704066311 ) ) ;
#28507 = CARTESIAN_POINT ( 'NONE',  ( -77.58781548604920886, -60.00000000000972733, -31.90504231437157756 ) ) ;
#28508 = CARTESIAN_POINT ( 'NONE',  ( 7.003653396366580353, -66.05706205559678779, -3.866846144092868531 ) ) ;
#28509 = CARTESIAN_POINT ( 'NONE',  ( 81.75077423159443413, -59.99999999999513989, -29.65143176264461999 ) ) ;
#28510 = DIRECTION ( 'NONE',  ( 1.000000000000000000, -0.000000000000000000, -0.000000000000000000 ) ) ;
#28511 = CARTESIAN_POINT ( 'NONE',  ( -6.586014515853777951, 41.68775576351381318, -58.88021171896449601 ) ) ;
#28512 = AXIS2_PLACEMENT_3D ( 'NONE', #102269, #29487, #12188 ) ;
#28514 = CARTESIAN_POINT ( 'NONE',  ( 3.977723760351280724, -22.06712578761976928, 27.56078887507262820 ) ) ;
#28513 = CARTESIAN_POINT ( 'NONE',  ( -110.2447566669111154, -59.99999999999998579, 128.1452744908969521 ) ) ;
#28515 = FACE_OUTER_BOUND ( 'NONE', #86087, .T. ) ;
#28516 = CARTESIAN_POINT ( 'NONE',  ( -47.55744046191945529, -60.27975237171524014, 53.32522255953509926 ) ) ;
#28517 = ORIENTED_EDGE ( 'NONE', *, *, #69339, .T. ) ;
#28518 = CARTESIAN_POINT ( 'NONE',  ( 0.000000000000000000, -30.00000000000000000, 0.000000000000000000 ) ) ;
#28519 = AXIS2_PLACEMENT_3D ( 'NONE', #30196, #62556, #38813 ) ;
#28520 = EDGE_LOOP ( 'NONE', ( #26718, #82678, #43626, #53902, #44313, #28252 ) ) ;
#28521 = CARTESIAN_POINT ( 'NONE',  ( -1.411247199636991373E-12, 7.746009256445978153, -51.75000000000450484 ) ) ;
#28522 = AXIS2_PLACEMENT_3D ( 'NONE', #9731, #9202, #1641 ) ;
#28523 = AXIS2_PLACEMENT_3D ( 'NONE', #100205, #92108, #51111 ) ;
#28524 = CARTESIAN_POINT ( 'NONE',  ( 17.39344025253047477, 36.29830519803331867, 24.14278306258518469 ) ) ;
#28525 = EDGE_CURVE ( 'NONE', #42350, #37712, #100958, .T. ) ;
#28526 = CARTESIAN_POINT ( 'NONE',  ( 5.909259836070536842, -6.137227957579323601, -1.072443315311453205 ) ) ;
#28527 = ORIENTED_EDGE ( 'NONE', *, *, #48323, .F. ) ;
#28528 = CARTESIAN_POINT ( 'NONE',  ( 5.910690929868576582, 246.1350409390679772, -1.065041252563917906 ) ) ;
#28529 = AXIS2_PLACEMENT_3D ( 'NONE', #91549, #9532, #32791 ) ;
#28530 = ORIENTED_EDGE ( 'NONE', *, *, #46857, .F. ) ;
#28531 = CARTESIAN_POINT ( 'NONE',  ( 89.50673784543010925, -30.00000000007396039, 3.352248442594707889 ) ) ;
#28532 =( NAMED_UNIT ( * ) SI_UNIT ( $, .STERADIAN. ) SOLID_ANGLE_UNIT ( ) );
#28533 = SURFACE_STYLE_FILL_AREA ( #59815 ) ;
#28534 = DIRECTION ( 'NONE',  ( 0.000000000000000000, -0.000000000000000000, 1.000000000000000000 ) ) ;
#28535 =( GEOMETRIC_REPRESENTATION_CONTEXT ( 3 ) GLOBAL_UNCERTAINTY_ASSIGNED_CONTEXT ( ( #63126 ) ) GLOBAL_UNIT_ASSIGNED_CONTEXT ( ( #1729, #91826, #43270 ) ) REPRESENTATION_CONTEXT ( 'NONE', 'WORKASPACE' ) );
#28536 = CARTESIAN_POINT ( 'NONE',  ( -29.83308852634790043, 42.00000000000000000, -51.76085035113232635 ) ) ;
#28537 = CARTESIAN_POINT ( 'NONE',  ( 98.01492924831322284, -30.00000000000000000, 190.5156199418535152 ) ) ;
#28538 = DIRECTION ( 'NONE',  ( 0.000000000000000000, -1.000000000000000000, 0.000000000000000000 ) ) ;
#28539 = EDGE_LOOP ( 'NONE', ( #104291, #45055, #39155, #85816, #58873, #95227 ) ) ;
#28540 = B_SPLINE_CURVE_WITH_KNOTS ( 'NONE', 3,
 ( #28941, #53689, #4619, #60221, #93089, #62333 ),
 .UNSPECIFIED., .F., .F.,
 ( 4, 2, 4 ),
 ( 2.380729204624338438E-07, 0.003943479449179648072, 0.007886720825438833446 ),
 .UNSPECIFIED. ) ;
#28541 = ORIENTED_EDGE ( 'NONE', *, *, #72828, .F. ) ;
#28542 = ORIENTED_EDGE ( 'NONE', *, *, #75093, .F. ) ;
#28543 = CARTESIAN_POINT ( 'NONE',  ( 55.26521301051785429, -29.08954164444167034, 56.68115046284776781 ) ) ;
#28544 = CARTESIAN_POINT ( 'NONE',  ( 7.040774347399621824, 41.35742771039598153, -58.68913404742972517 ) ) ;
#28545 = DIRECTION ( 'NONE',  ( 0.000000000000000000, -1.000000000000000000, 0.000000000000000000 ) ) ;
#28546 = ORIENTED_EDGE ( 'NONE', *, *, #24209, .F. ) ;
#28547 = CARTESIAN_POINT ( 'NONE',  ( -91.42805026571208771, -38.39309202493998185, -8.617090538173520997 ) ) ;
#28548 = ORIENTED_EDGE ( 'NONE', *, *, #34956, .F. ) ;
#28549 = CARTESIAN_POINT ( 'NONE',  ( -33.94783393359910662, 484.1261039197349305, 1.321740980884785532 ) ) ;
#28550 = CARTESIAN_POINT ( 'NONE',  ( 88.56961690390389208, -38.54355387740943684, 200.1502377494141456 ) ) ;
#28551 = CARTESIAN_POINT ( 'NONE',  ( 12.53384725709329750, 20.77238591696947267, 6.330773932024738926 ) ) ;
#28552 = CARTESIAN_POINT ( 'NONE',  ( 83.86163892754350968, -45.28585860511496719, 5.009633451048947528 ) ) ;
#28553 = CARTESIAN_POINT ( 'NONE',  ( 40.87706463175591409, 434.1066599708036051, 26.33551600060701858 ) ) ;
#28554 = CARTESIAN_POINT ( 'NONE',  ( -24.00296863125211644, 25.16459671810052257, -32.94325037771057652 ) ) ;
#28555 = AXIS2_PLACEMENT_3D ( 'NONE', #39045, #96222, #94086 ) ;
#28556 = CARTESIAN_POINT ( 'NONE',  ( -44.35819766388001284, 435.2221642642158486, 12.65712761108313522 ) ) ;
#28557 = CARTESIAN_POINT ( 'NONE',  ( 3.021271035815610073, 47.67815885094228179, 5.000000000000000000 ) ) ;
#28558 = ORIENTED_EDGE ( 'NONE', *, *, #69083, .F. ) ;
#28559 = CARTESIAN_POINT ( 'NONE',  ( -9.246271506234601034, 16.00000000000000000, -3.826949319562308105 ) ) ;
#28560 = CARTESIAN_POINT ( 'NONE',  ( 7.311411528619694344, 40.00000000267693423, -70.68779756257029590 ) ) ;
#28561 = CARTESIAN_POINT ( 'NONE',  ( -32.09911992168216699, 438.9232547152094526, 23.66653216045977004 ) ) ;
#28562 = ORIENTED_EDGE ( 'NONE', *, *, #83989, .F. ) ;
#28563 = CARTESIAN_POINT ( 'NONE',  ( -3.901433755053307362E-15, 6.534749472788146107, 4.681481898397000130 ) ) ;
#28564 = CARTESIAN_POINT ( 'NONE',  ( -38.19251921417566109, 310.5472675333638790, 5.678690236465158137 ) ) ;
#28565 = CARTESIAN_POINT ( 'NONE',  ( 14.83349330513380693, -3.851859888774471706E-31, 4.000000000000001776 ) ) ;
#28566 = DIRECTION ( 'NONE',  ( 0.000000000000000000, 1.000000000000000000, 0.000000000000000000 ) ) ;
#28567 = CARTESIAN_POINT ( 'NONE',  ( -8.000000000000000000, -23.74999999999999289, -9.797174393178825657E-16 ) ) ;
#28568 = CARTESIAN_POINT ( 'NONE',  ( 11.94032942385361018, -16.68599286367008716, 34.79957533961248117 ) ) ;
#28569 = ADVANCED_FACE ( 'NONE', ( #76344 ), #28927, .T. ) ;
#28570 = CARTESIAN_POINT ( 'NONE',  ( -3.400000000000000355, 4.163799117101001052E-16, -4.987924522925830217 ) ) ;
#28571 = ORIENTED_EDGE ( 'NONE', *, *, #72519, .F. ) ;
#28572 = CARTESIAN_POINT ( 'NONE',  ( 85.93733347156485536, -24.97102198799566253, 178.1358747736554164 ) ) ;
#28573 = CARTESIAN_POINT ( 'NONE',  ( -30.00000000000000000, 0.000000000000000000, 0.000000000000000000 ) ) ;
#28574 =( GEOMETRIC_REPRESENTATION_CONTEXT ( 3 ) GLOBAL_UNCERTAINTY_ASSIGNED_CONTEXT ( ( #34346 ) ) GLOBAL_UNIT_ASSIGNED_CONTEXT ( ( #91963, #18638, #26218 ) ) REPRESENTATION_CONTEXT ( 'NONE', 'WORKASPACE' ) );
#28575 = CARTESIAN_POINT ( 'NONE',  ( 0.000000000000000000, 0.000000000000000000, 0.000000000000000000 ) ) ;
#28576 = ORIENTED_EDGE ( 'NONE', *, *, #84920, .T. ) ;
#28577 = CARTESIAN_POINT ( 'NONE',  ( -91.04256780768773183, -60.15438401438225924, 61.63257487189168415 ) ) ;
#28578 = CARTESIAN_POINT ( 'NONE',  ( 0.000000000000000000, -5.629165124598843661, 3.250000000000011990 ) ) ;
#28579 = CARTESIAN_POINT ( 'NONE',  ( 10.19007819943910143, -5.000000000014482637, -96.34610920171921578 ) ) ;
#28580 = CARTESIAN_POINT ( 'NONE',  ( 0.000000000000000000, 273.9999999999999432, -6.999999999999982236 ) ) ;
#28581 = EDGE_CURVE ( 'NONE', #84797, #93508, #68244, .T. ) ;
#28582 = SURFACE_STYLE_USAGE ( .BOTH. , #78676 ) ;
#28583 = ADVANCED_FACE ( 'NONE', ( #84987 ), #91470, .T. ) ;
#28584 = MECHANICAL_DESIGN_GEOMETRIC_PRESENTATION_REPRESENTATION (  '', ( #61289 ), #25111 ) ;
#28585 =( NAMED_UNIT ( * ) PLANE_ANGLE_UNIT ( ) SI_UNIT ( $, .RADIAN. ) );
#28586 = CARTESIAN_POINT ( 'NONE',  ( 33.60718460261718121, -60.00000000000000000, 45.28735806869271840 ) ) ;
#28587 = CONICAL_SURFACE ( 'NONE', #68118, 4.000000000000007105, 0.9599310885968835860 ) ;
#28588 = CARTESIAN_POINT ( 'NONE',  ( 6.493927703541009677, -18.97370440754745857, 35.15281767446274586 ) ) ;
#28589 = CARTESIAN_POINT ( 'NONE',  ( 1.257641187073857525, -2.476915083462004360E-10, 101.3278948774975561 ) ) ;
#28590 = CARTESIAN_POINT ( 'NONE',  ( 42.00705846777699293, -27.16471903480216454, 37.37245921768317203 ) ) ;
#28592 = CARTESIAN_POINT ( 'NONE',  ( -12.80228504472586692, 18.84866368018861493, 8.115852207351810677 ) ) ;
#28591 = DIRECTION ( 'NONE',  ( 0.000000000000000000, 1.000000000000000000, 0.000000000000000000 ) ) ;
#28593 = CARTESIAN_POINT ( 'NONE',  ( 4.023953349526805390, 300.5162199157299483, -10.00978861085792104 ) ) ;
#28594 = CARTESIAN_POINT ( 'NONE',  ( 45.50145573691759182, 405.2496736015978627, 8.430338687477670234 ) ) ;
#28595 = ORIENTED_EDGE ( 'NONE', *, *, #50411, .T. ) ;
#28596 = CARTESIAN_POINT ( 'NONE',  ( 43.51697068632529408, 365.4421646331526858, 13.28917352912563032 ) ) ;
#28597 = CARTESIAN_POINT ( 'NONE',  ( -42.57704743493907529, 486.1612337113410831, 7.852296464539637810 ) ) ;
#28598 = AXIS2_PLACEMENT_3D ( 'NONE', #47985, #80892, #58080 ) ;
#28599 = AXIS2_PLACEMENT_3D ( 'NONE', #72108, #23589, #30620 ) ;
#28600 = CARTESIAN_POINT ( 'NONE',  ( -33.00000000000000000, 450.0000000000002274, 13.20242257375370976 ) ) ;
#28601 = AXIS2_PLACEMENT_3D ( 'NONE', #10395, #93468, #44924 ) ;
#28602 = VERTEX_POINT ( 'NONE', #94138 ) ;
#28603 = CARTESIAN_POINT ( 'NONE',  ( 84.15356149169568312, -5.000000000000000000, 0.000000000000000000 ) ) ;
#28604 = CARTESIAN_POINT ( 'NONE',  ( -17.49999999999997513, 52.00000000000000711, 59.91915230424417160 ) ) ;
#28605 = ORIENTED_EDGE ( 'NONE', *, *, #98111, .F. ) ;
#28606 = CARTESIAN_POINT ( 'NONE',  ( -13.57352674565050776, 1.209266042179385936, 14.95197387114457399 ) ) ;
#28607 = SURFACE_SIDE_STYLE ('',( #69044 ) ) ;
#28608 = AXIS2_PLACEMENT_3D ( 'NONE', #77235, #86418, #53998 ) ;
#28609 = CARTESIAN_POINT ( 'NONE',  ( 92.53532739719321398, -5.000000000000000000, 6.123233995736778115E-16 ) ) ;
#28611 = CARTESIAN_POINT ( 'NONE',  ( -1.564112305163676497, -34.58958035781643758, -32.65456768497247708 ) ) ;
#28610 = CARTESIAN_POINT ( 'NONE',  ( 9.948561005166148163, 253.8699027374819934, -1.045755304005147490 ) ) ;
#28612 = ORIENTED_EDGE ( 'NONE', *, *, #86341, .F. ) ;
#28613 = B_SPLINE_CURVE_WITH_KNOTS ( 'NONE', 3,
 ( #95785, #89287, #21918, #80112, #81168, #7278 ),
 .UNSPECIFIED., .F., .F.,
 ( 4, 2, 4 ),
 ( 0.01913986446880884540, 0.02104055318064343080, 0.02294124189247801621 ),
 .UNSPECIFIED. ) ;
#28614 = DIRECTION ( 'NONE',  ( -1.000000000000000000, -0.000000000000000000, -0.000000000000000000 ) ) ;
#28615 = DIRECTION ( 'NONE',  ( -1.000000000000000000, 0.000000000000000000, 0.000000000000000000 ) ) ;
#28616 = ORIENTED_EDGE ( 'NONE', *, *, #60694, .F. ) ;
#28617 = EDGE_CURVE ( 'NONE', #76468, #98133, #85498, .T. ) ;
#28618 = CARTESIAN_POINT ( 'NONE',  ( 0.000000000000000000, 5.629165124598848102, -3.250000000000007105 ) ) ;
#28619 = DIRECTION ( 'NONE',  ( 0.5735764363510470476, -0.8191520442889911324, 1.003171929053524007E-16 ) ) ;
#28620 = CARTESIAN_POINT ( 'NONE',  ( -92.00833143843689754, -60.00000000000000711, 6.014465541360822343 ) ) ;
#28621 = VERTEX_POINT ( 'NONE', #78478 ) ;
#28622 = CARTESIAN_POINT ( 'NONE',  ( 52.81650669486619165, 6.856755485862130937E-15, 0.000000000000000000 ) ) ;
#28623 = DIRECTION ( 'NONE',  ( 0.000000000000000000, 0.000000000000000000, -1.000000000000000000 ) ) ;
#28624 = DIRECTION ( 'NONE',  ( 0.000000000000000000, 0.000000000000000000, 1.000000000000000000 ) ) ;
#28625 = CARTESIAN_POINT ( 'NONE',  ( -9.918325909156573417, 26.20764768292568903, 1.298699613733151459 ) ) ;
#28626 = SURFACE_STYLE_USAGE ( .BOTH. , #94937 ) ;
#28627 = CARTESIAN_POINT ( 'NONE',  ( -82.28676419405165632, -42.97473223736994896, 168.7210715244461312 ) ) ;
#28628 = ORIENTED_EDGE ( 'NONE', *, *, #46991, .T. ) ;
#28629 = CARTESIAN_POINT ( 'NONE',  ( 97.73333333333333428, 1.023464760207051730E-14, 0.000000000000000000 ) ) ;
#28630 = VERTEX_POINT ( 'NONE', #4604 ) ;
#28631 = CIRCLE ( 'NONE', #59567, 15.00000000000000000 ) ;
#28632 = ORIENTED_EDGE ( 'NONE', *, *, #37700, .T. ) ;
#28633 = CARTESIAN_POINT ( 'NONE',  ( -13.20528892216319683, -4.332661967060645658, 12.52414413171502439 ) ) ;
#28634 = EDGE_CURVE ( 'NONE', #5888, #77883, #95817, .T. ) ;
#28635 = CARTESIAN_POINT ( 'NONE',  ( -6.923875968562938965, -12.36264606019533474, 8.501481527782761560 ) ) ;
#28636 = CARTESIAN_POINT ( 'NONE',  ( 14.29190075645216851, 12.99999999999999289, 10.00000000000000000 ) ) ;
#28637 = ORIENTED_EDGE ( 'NONE', *, *, #87065, .T. ) ;
#28638 = FACE_OUTER_BOUND ( 'NONE', #40179, .T. ) ;
#28639 = CARTESIAN_POINT ( 'NONE',  ( -64.02773510654475331, -57.67113784069211135, -36.59462343474526591 ) ) ;
#28640 = CARTESIAN_POINT ( 'NONE',  ( -4.656749229489883568, -66.31760408126432083, -3.785628640239150133 ) ) ;
#28641 = CARTESIAN_POINT ( 'NONE',  ( 0.1306530452038104362, 7.903938623646867612, 2.309976723937611887 ) ) ;
#28642 = DIRECTION ( 'NONE',  ( 0.000000000000000000, 1.000000000000000000, 0.000000000000000000 ) ) ;
#28643 = CARTESIAN_POINT ( 'NONE',  ( 4.210530276628051460, 15.00000000000000000, -9.999999999999998224 ) ) ;
#28644 = CARTESIAN_POINT ( 'NONE',  ( 72.33341283407553135, -14.21045842199439235, -25.95464913363236548 ) ) ;
#28645 = CARTESIAN_POINT ( 'NONE',  ( -89.23267494088513274, -59.99999999999987921, 204.3671292578742680 ) ) ;
#28646 = B_SPLINE_CURVE_WITH_KNOTS ( 'NONE', 3,
 ( #74657, #743, #54100, #37446 ),
 .UNSPECIFIED., .F., .F.,
 ( 4, 4 ),
 ( 4.718958039861916012E-17, 0.002032023592278147089 ),
 .UNSPECIFIED. ) ;
#28647 = CARTESIAN_POINT ( 'NONE',  ( -55.86786607641659685, -36.02883296429982352, 60.77031267314215768 ) ) ;
#28648 = ORIENTED_EDGE ( 'NONE', *, *, #51386, .F. ) ;
#28649 = CARTESIAN_POINT ( 'NONE',  ( 42.08762648273149409, 487.0030674539048618, 9.106351919857861077 ) ) ;
#28650 = ORIENTED_EDGE ( 'NONE', *, *, #103942, .F. ) ;
#28651 = CARTESIAN_POINT ( 'NONE',  ( -100.4719902400335343, -45.25992542466413227, 192.0840524196355830 ) ) ;
#28652 = CARTESIAN_POINT ( 'NONE',  ( 100.2031709646873310, -38.00000000000000000, 190.2875524083539744 ) ) ;
#28653 = CARTESIAN_POINT ( 'NONE',  ( -5.290067270632216712, 51.34639538792298907, 8.531152949374556371 ) ) ;
#28654 = EDGE_CURVE ( 'NONE', #90336, #35664, #76855, .T. ) ;
#28655 = ORIENTED_EDGE ( 'NONE', *, *, #56417, .T. ) ;
#28656 = LINE ( 'NONE', #35690, #57992 ) ;
#28657 = SURFACE_STYLE_FILL_AREA ( #102513 ) ;
#28658 = DIRECTION ( 'NONE',  ( -1.000000000000000000, 0.000000000000000000, -0.000000000000000000 ) ) ;
#28659 = CARTESIAN_POINT ( 'NONE',  ( -7.188101187500000044, -14.28125000204838457, -8.802885111219163269E-16 ) ) ;
#28660 = CARTESIAN_POINT ( 'NONE',  ( 33.08751701378358945, 301.6823158026044780, 11.49690784967660662 ) ) ;
#28661 = DIRECTION ( 'NONE',  ( 0.000000000000000000, 0.7605354461462350280, -0.6492964154799772958 ) ) ;
#28662 = CARTESIAN_POINT ( 'NONE',  ( 7.619701877737479201, -81.82557840467232779, -2.447562251315979598 ) ) ;
#28663 = CARTESIAN_POINT ( 'NONE',  ( 68.78515106805255641, -30.00000000000000000, 91.48474193797456167 ) ) ;
#28664 = SURFACE_SIDE_STYLE ('',( #27611 ) ) ;
#28665 = EDGE_CURVE ( 'NONE', #56180, #88131, #33860, .T. ) ;
#28666 = CARTESIAN_POINT ( 'NONE',  ( -9.443162145033490162, 44.08363004829780607, -13.23108312906848560 ) ) ;
#28667 = AXIS2_PLACEMENT_3D ( 'NONE', #88239, #103361, #104402 ) ;
#28668 = CARTESIAN_POINT ( 'NONE',  ( -7.500000000000007105, 40.95611321456068055, -60.73832539154658861 ) ) ;
#28669 = CARTESIAN_POINT ( 'NONE',  ( -29.17244825486319471, -39.48658745795624014, 32.84959031112921224 ) ) ;
#28670 = CARTESIAN_POINT ( 'NONE',  ( 47.95189470694865719, -49.89909759463478878, 50.75627975532390224 ) ) ;
#28671 = CARTESIAN_POINT ( 'NONE',  ( -1.469576158976823947E-15, -14.37499999999999112, 8.000000000000000000 ) ) ;
#28672 = EDGE_CURVE ( 'NONE', #47934, #7556, #68333, .T. ) ;
#28673 = LINE ( 'NONE', #77188, #104650 ) ;
#28674 = CARTESIAN_POINT ( 'NONE',  ( -86.58980629399917461, -38.61205887094109812, 199.3558248615631214 ) ) ;
#28675 = AXIS2_PLACEMENT_3D ( 'NONE', #49917, #7858, #48316 ) ;
#28676 = ORIENTED_EDGE ( 'NONE', *, *, #51316, .F. ) ;
#28677 = CARTESIAN_POINT ( 'NONE',  ( -41.46910480218704009, 484.7338956289818270, -3.418960549715579500 ) ) ;
#28678 = CARTESIAN_POINT ( 'NONE',  ( 81.86055861641301590, -59.99999999999994316, 186.9037213880110926 ) ) ;
#28679 = CARTESIAN_POINT ( 'NONE',  ( -49.24240974153273243, 8.191948471291029321, -15.29453271768056766 ) ) ;
#28681 = DIRECTION ( 'NONE',  ( -1.000000000000000000, -8.881784197001252323E-16, 0.000000000000000000 ) ) ;
#28680 = AXIS2_PLACEMENT_3D ( 'NONE', #76931, #84504, #60252 ) ;
#28682 =( GEOMETRIC_REPRESENTATION_CONTEXT ( 3 ) GLOBAL_UNCERTAINTY_ASSIGNED_CONTEXT ( ( #62167 ) ) GLOBAL_UNIT_ASSIGNED_CONTEXT ( ( #43860, #76219, #60603 ) ) REPRESENTATION_CONTEXT ( 'NONE', 'WORKASPACE' ) );
#28683 = CARTESIAN_POINT ( 'NONE',  ( 6.472171899339533852, 40.92674694738754226, -71.09138916011745835 ) ) ;
#28684 = CARTESIAN_POINT ( 'NONE',  ( -33.74590002647645548, 434.0087204318717795, 12.79521435343652236 ) ) ;
#28685 = COLOUR_RGB ( '', 0.31764706, 0.68627451, 0.89019608) ;
#28686 = CARTESIAN_POINT ( 'NONE',  ( -32.46586666335682736, 488.6856797978888380, 9.810357008062371875 ) ) ;
#28687 = FACE_BOUND ( 'NONE', #94466, .T. ) ;
#28688 = CARTESIAN_POINT ( 'NONE',  ( 112.1074610866378691, -60.00000000000000711, 166.9029264543243301 ) ) ;
#28689 = ADVANCED_FACE ( 'NONE', ( #105926 ), #87123, .F. ) ;
#28690 = EDGE_CURVE ( 'NONE', #63378, #55614, #23978, .T. ) ;
#28691 = AXIS2_PLACEMENT_3D ( 'NONE', #103515, #77660, #69571 ) ;
#28692 = CYLINDRICAL_SURFACE ( 'NONE', #40479, 4.250000000000000000 ) ;
#28693 = VERTEX_POINT ( 'NONE', #105412 ) ;
#28694 = B_SPLINE_CURVE_WITH_KNOTS ( 'NONE', 3,
 ( #51993, #85994, #12067, #62252, #2906, #19156, #86530, #46045, #12592, #37455 ),
 .UNSPECIFIED., .F., .F.,
 ( 4, 2, 2, 2, 4 ),
 ( -5.999999999514162541E-08, 0.002466202848293326880, 0.004932465696586649066, 0.009864991393173294307, 0.01973004278634659173 ),
 .UNSPECIFIED. ) ;
#28695 = CARTESIAN_POINT ( 'NONE',  ( 7.046357527897571416, 31.30615650601003352, -3.789683693877207826 ) ) ;
#28696 = CARTESIAN_POINT ( 'NONE',  ( -71.80342408229677176, -30.00000000000000711, -19.71767938363505834 ) ) ;
#28697 = EDGE_LOOP ( 'NONE', ( #60346, #31466 ) ) ;
#28699 = CARTESIAN_POINT ( 'NONE',  ( 32.02014133911703908, 464.7988840750959980, 11.81894500396711933 ) ) ;
#28698 = CARTESIAN_POINT ( 'NONE',  ( -58.27688207720395752, -38.34417119533264184, 91.02890418086518309 ) ) ;
#28700 = CARTESIAN_POINT ( 'NONE',  ( 46.00000000000000000, 437.9690125970931831, 14.09127711025711349 ) ) ;
#28701 = CARTESIAN_POINT ( 'NONE',  ( -15.00099999999999767, 12.99999999999999289, -10.00000000000000178 ) ) ;
#28702 = CARTESIAN_POINT ( 'NONE',  ( 97.73333333333333428, -4.171999999999998820, 0.000000000000000000 ) ) ;
#28703 = CARTESIAN_POINT ( 'NONE',  ( 2.977408999572650927, -11.75000000204838813, -7.188101187500001821 ) ) ;
#28704 = CARTESIAN_POINT ( 'NONE',  ( 3.140974613991526887, -5.000000000000002665, -96.68767211932356531 ) ) ;
#28705 = PRODUCT ( '5. Joint', '5. Joint', '', ( #102175 ) ) ;
#28707 = ORIENTED_EDGE ( 'NONE', *, *, #5792, .T. ) ;
#28706 = CARTESIAN_POINT ( 'NONE',  ( 0.000000000000000000, 274.9999999999999432, -10.00000000000000533 ) ) ;
#28708 = CARTESIAN_POINT ( 'NONE',  ( 84.34664725709313871, -29.01649459423289557, 165.8781276598768954 ) ) ;
#28710 = AXIS2_PLACEMENT_3D ( 'NONE', #17101, #55523, #88463 ) ;
#28709 = CARTESIAN_POINT ( 'NONE',  ( -45.99999999999999289, 462.1567080628744293, 5.830853676147882858 ) ) ;
#28711 = CARTESIAN_POINT ( 'NONE',  ( 4.555432764205790797, -5.242992371775952343, -6.208169345099798342 ) ) ;
#28712 = ORIENTED_EDGE ( 'NONE', *, *, #73393, .T. ) ;
#28713 = CARTESIAN_POINT ( 'NONE',  ( -32.84237740334658895, 485.2251842821276568, 5.746442123023856041 ) ) ;
#28714 = CARTESIAN_POINT ( 'NONE',  ( 16.75187969033571989, 34.25544727262119693, 24.30698433968583316 ) ) ;
#28715 = CARTESIAN_POINT ( 'NONE',  ( 0.5204879950541950739, 7.205049615410636044, -0.5609245978742248839 ) ) ;
#28716 = DIRECTION ( 'NONE',  ( -1.000000000000000000, 0.000000000000000000, 0.000000000000000000 ) ) ;
#28717 = CARTESIAN_POINT ( 'NONE',  ( 0.000000000000000000, 0.000000000000000000, 0.000000000000000000 ) ) ;
#28718 = CARTESIAN_POINT ( 'NONE',  ( 1.235988652327632664, 15.32448820071590134, 50.72415524448811652 ) ) ;
#28719 =( NAMED_UNIT ( * ) SI_UNIT ( $, .STERADIAN. ) SOLID_ANGLE_UNIT ( ) );
#28720 = EDGE_CURVE ( 'NONE', #24620, #69218, #43244, .T. ) ;
#28721 = EDGE_LOOP ( 'NONE', ( #34322, #56946, #28748 ) ) ;
#28722 = CARTESIAN_POINT ( 'NONE',  ( -3.271359168585607158, 300.0885221343756371, 9.452922326459093583 ) ) ;
#28723 = EDGE_CURVE ( 'NONE', #12582, #72821, #92481, .T. ) ;
#28724 = DIRECTION ( 'NONE',  ( 0.8308658609248538163, -0.5564727496918439043, -1.776356839400249479E-15 ) ) ;
#28725 = LINE ( 'NONE', #5471, #18352 ) ;
#28727 =( LENGTH_UNIT ( ) NAMED_UNIT ( * ) SI_UNIT ( .MILLI., .METRE. ) );
#28726 = DIRECTION ( 'NONE',  ( -1.000000000000000000, -1.224606353822377258E-16, -0.000000000000000000 ) ) ;
#28728 = CARTESIAN_POINT ( 'NONE',  ( -7.188101187500001821, -24.50000000204839168, -2.977408999572651371 ) ) ;
#28729 = CARTESIAN_POINT ( 'NONE',  ( 11.46329167404285343, 294.5997526591420410, -10.05357486629153030 ) ) ;
#28730 = APPLICATION_CONTEXT ( 'automotive_design' ) ;
#28731 = DIRECTION ( 'NONE',  ( 0.000000000000000000, -1.000000000000000000, 0.000000000000000000 ) ) ;
#28732 = COLOUR_RGB ( '', 0.31764706, 0.68627451, 0.89019608) ;
#28733 = CARTESIAN_POINT ( 'NONE',  ( 9.610124387818546055, -5.000000000000000000, -77.63937538515727965 ) ) ;
#28734 = AXIS2_PLACEMENT_3D ( 'NONE', #10606, #3057, #27921 ) ;
#28735 = CONTEXT_DEPENDENT_SHAPE_REPRESENTATION ( #72163, #102786 ) ;
#28736 = VERTEX_POINT ( 'NONE', #22408 ) ;
#28737 = CARTESIAN_POINT ( 'NONE',  ( 27.61650669486618881, 1.474610560812782335E-15, 0.000000000000000000 ) ) ;
#28738 = CARTESIAN_POINT ( 'NONE',  ( 7.499999999999650058, 0.7577384720645206073, -7.446470314338821339 ) ) ;
#28739 = CARTESIAN_POINT ( 'NONE',  ( -8.824767335865399076, 18.31512251394013191, 0.000000000000000000 ) ) ;
#28740 = CARTESIAN_POINT ( 'NONE',  ( 2.235495008889195345E-15, -15.58845726811994759, -13.00000000000000000 ) ) ;
#28741 = ADVANCED_FACE ( 'NONE', ( #29959 ), #14944, .F. ) ;
#28742 = AXIS2_PLACEMENT_3D ( 'NONE', #2545, #99101, #25262 ) ;
#28743 = ORIENTED_EDGE ( 'NONE', *, *, #42507, .T. ) ;
#28744 = DIRECTION ( 'NONE',  ( 0.000000000000000000, 0.000000000000000000, -1.000000000000000000 ) ) ;
#28745 = CARTESIAN_POINT ( 'NONE',  ( -2.354803500934600891, 50.00000000000001421, -100.0000000000000000 ) ) ;
#28746 = AXIS2_PLACEMENT_3D ( 'NONE', #36188, #85221, #43696 ) ;
#28747 = AXIS2_PLACEMENT_3D ( 'NONE', #4053, #54697, #87108 ) ;
#28748 = ORIENTED_EDGE ( 'NONE', *, *, #72002, .T. ) ;
#28749 = CARTESIAN_POINT ( 'NONE',  ( -27.42583773761564103, 34.37177070069997598, 10.02613003525735991 ) ) ;
#28750 = EDGE_CURVE ( 'NONE', #70900, #74905, #58715, .T. ) ;
#28751 = FACE_OUTER_BOUND ( 'NONE', #82475, .T. ) ;
#28752 = CARTESIAN_POINT ( 'NONE',  ( 9.380894568449075877, 102.9886936688906047, -3.467341429141160170 ) ) ;
#28753 = CARTESIAN_POINT ( 'NONE',  ( -17.97174518249929420, 36.40624878439880518, 23.34175835912197883 ) ) ;
#28754 = UNCERTAINTY_MEASURE_WITH_UNIT (LENGTH_MEASURE( 1.000000000000000082E-05 ), #93708, 'distance_accuracy_value', 'NONE');
#28755 = CARTESIAN_POINT ( 'NONE',  ( -106.6453062919850225, -60.00000000000000000, 197.5725164084929872 ) ) ;
#28756 = AXIS2_PLACEMENT_3D ( 'NONE', #9270, #43253, #83172 ) ;
#28757 = AXIS2_PLACEMENT_3D ( 'NONE', #82416, #65166, #91060 ) ;
#28758 = DIRECTION ( 'NONE',  ( -1.000000000000000000, -1.224606353822377258E-16, -0.000000000000000000 ) ) ;
#28759 = AXIS2_PLACEMENT_3D ( 'NONE', #62488, #67526, #21516 ) ;
#28760 = VECTOR ( 'NONE', #29299, 999.9999999999998863 ) ;
#28761 = CARTESIAN_POINT ( 'NONE',  ( 0.000000000000000000, 0.000000000000000000, -4.987924522925830217 ) ) ;
#28762 = CARTESIAN_POINT ( 'NONE',  ( -4.905843853654967113, -4.999999999999999112, -16.52456679617691293 ) ) ;
#28763 = DIRECTION ( 'NONE',  ( -1.000000000000000000, -1.224606353822377258E-16, -0.000000000000000000 ) ) ;
#28764 = CARTESIAN_POINT ( 'NONE',  ( -82.57751153944624889, -53.60564265856869071, 184.4179057790843217 ) ) ;
#28765 = CARTESIAN_POINT ( 'NONE',  ( 34.55744730647673890, 42.66432393376602761, -62.99136456808676598 ) ) ;
#28766 = AXIS2_PLACEMENT_3D ( 'NONE', #16518, #58031, #8423 ) ;
#28767 = VECTOR ( 'NONE', #54152, 1000.000000000000227 ) ;
#28768 = ORIENTED_EDGE ( 'NONE', *, *, #77774, .T. ) ;
#28769 = CARTESIAN_POINT ( 'NONE',  ( -13.69034148509428839, 302.5483970265941593, 9.872518330349395299 ) ) ;
#28770 = EDGE_CURVE ( 'NONE', #43, #21338, #54507, .T. ) ;
#28771 = SURFACE_STYLE_USAGE ( .BOTH. , #96116 ) ;
#28772 = CARTESIAN_POINT ( 'NONE',  ( -84.13707156515019392, -45.27010591465764833, 0.6314432930867477367 ) ) ;
#28773 = CARTESIAN_POINT ( 'NONE',  ( 30.59999999999999787, 1.533819458162526451E-15, 0.000000000000000000 ) ) ;
#28774 = DIRECTION ( 'NONE',  ( -0.000000000000000000, 1.000000000000000000, -0.000000000000000000 ) ) ;
#28775 = CARTESIAN_POINT ( 'NONE',  ( 4.258978623648461692, 140.4056380026280237, -5.000000000000000000 ) ) ;
#28776 = CARTESIAN_POINT ( 'NONE',  ( -0.5619217318086657809, -7.564468822943342552, -6.443866470201776053 ) ) ;
#28777 = CARTESIAN_POINT ( 'NONE',  ( 47.37019975563026719, 41.99999999991776178, 36.40416150969240050 ) ) ;
#28778 = CARTESIAN_POINT ( 'NONE',  ( 62.45579587598661675, -29.99999999999998934, 99.43503315974342627 ) ) ;
#28779 = CARTESIAN_POINT ( 'NONE',  ( -87.19976908022060513, -14.21045842199435860, -12.72659765151139233 ) ) ;
#28780 = CARTESIAN_POINT ( 'NONE',  ( -63.81267340554329337, -53.39190204468273038, 89.97204334792978386 ) ) ;
#28781 = ORIENTED_EDGE ( 'NONE', *, *, #106748, .T. ) ;
#28782 = CARTESIAN_POINT ( 'NONE',  ( 89.23375057675741573, -59.99999999999977973, 204.3679297810271862 ) ) ;
#28783 = CARTESIAN_POINT ( 'NONE',  ( 65.26569950619781935, 39.42419746932910840, 0.7618753667456097389 ) ) ;
#28784 = CARTESIAN_POINT ( 'NONE',  ( 9.918622661780615246, -60.00000000000981970, 42.00659582329527097 ) ) ;
#28785 = B_SPLINE_CURVE_WITH_KNOTS ( 'NONE', 3,
 ( #81695, #48806, #83315, #82246, #32133, #106520, #99483, #7821, #9953, #57969, #66605, #65011, #50401 ),
 .UNSPECIFIED., .F., .F.,
 ( 4, 1, 1, 1, 1, 1, 2, 2, 4 ),
 ( 0.000000000000000000, 0.2500000000000132117, 0.3750000000000142109, 0.4375000000000099920, 0.4687500000000078826, 0.4843750000000114908, 0.4921875000000120459, 0.5000000000000125455, 1.000000000000000000 ),
 .UNSPECIFIED. ) ;
#28786 = ORIENTED_EDGE ( 'NONE', *, *, #67309, .T. ) ;
#28787 = CARTESIAN_POINT ( 'NONE',  ( 13.38090213880806978, -54.00000000000000711, 31.11721482942554928 ) ) ;
#28788 = CARTESIAN_POINT ( 'NONE',  ( 4.401442555609581635E-16, -23.65625000204838457, -7.188101187500000044 ) ) ;
#28789 = ADVANCED_FACE ( 'NONE', ( #87651 ), #102824, .T. ) ;
#28790 = DIRECTION ( 'NONE',  ( 0.000000000000000000, -1.000000000000000000, 0.000000000000000000 ) ) ;
#28791 = VERTEX_POINT ( 'NONE', #47690 ) ;
#28792 = AXIS2_PLACEMENT_3D ( 'NONE', #83775, #16396, #99419 ) ;
#28793 = ORIENTED_EDGE ( 'NONE', *, *, #90396, .T. ) ;
#28794 = LINE ( 'NONE', #27190, #50974 ) ;
#28795 = CARTESIAN_POINT ( 'NONE',  ( 75.30000000000001137, 0.000000000000000000, 3.309499999999999886 ) ) ;
#28796 = CARTESIAN_POINT ( 'NONE',  ( -80.27472688732939332, -60.00000000000000000, -27.80218209016123510 ) ) ;
#28797 = CARTESIAN_POINT ( 'NONE',  ( 25.02598631787318695, 305.0623641175172338, -9.737168983575548609 ) ) ;
#28798 = CARTESIAN_POINT ( 'NONE',  ( 5.082755093536325930, -32.84375000204838813, -5.082755093536325042 ) ) ;
#28799 = DIRECTION ( 'NONE',  ( -0.000000000000000000, 1.000000000000000000, 0.000000000000000000 ) ) ;
#28800 = STYLED_ITEM ( 'NONE', ( #93648 ), #101096 ) ;
#28801 = CARTESIAN_POINT ( 'NONE',  ( 12.64023069600375315, -4.285714285714297134, 21.88880945939638778 ) ) ;
#28802 = CARTESIAN_POINT ( 'NONE',  ( 3.857142857142850101, -48.79941684889506348, 103.1763305333244176 ) ) ;
#28803 = CARTESIAN_POINT ( 'NONE',  ( -6.043427762773251111, 50.00000000000000000, -95.48543666094653304 ) ) ;
#28804 = EDGE_CURVE ( 'NONE', #80206, #64859, #7232, .T. ) ;
#28805 = CARTESIAN_POINT ( 'NONE',  ( 32.88333705524082973, 439.7317646416722141, 24.13381181826093069 ) ) ;
#28806 = CARTESIAN_POINT ( 'NONE',  ( 40.32369798409568062, 437.3250542437401123, 5.179402639110887385 ) ) ;
#28807 = ORIENTED_EDGE ( 'NONE', *, *, #41815, .T. ) ;
#28808 = CARTESIAN_POINT ( 'NONE',  ( 0.000000000000000000, 0.000000000000000000, 8.000000000000000000 ) ) ;
#28809 = SURFACE_SIDE_STYLE ('',( #43352 ) ) ;
#28811 = CARTESIAN_POINT ( 'NONE',  ( 34.67182219425094303, -39.49850266814299715, 35.14395799684566413 ) ) ;
#28810 = DIRECTION ( 'NONE',  ( 0.000000000000000000, 0.000000000000000000, 1.000000000000000000 ) ) ;
#28812 = FILL_AREA_STYLE_COLOUR ( '', #12759 ) ;
#28813 = EDGE_LOOP ( 'NONE', ( #46656, #99329, #83423 ) ) ;
#28814 = EDGE_CURVE ( 'NONE', #104331, #16154, #40141, .T. ) ;
#28815 = CARTESIAN_POINT ( 'NONE',  ( -42.18756898894582719, 484.4522853017719513, -2.425645685620470449 ) ) ;
#28817 = DIRECTION ( 'NONE',  ( 0.000000000000000000, -1.000000000000000000, 0.000000000000000000 ) ) ;
#28816 = SURFACE_STYLE_USAGE ( .BOTH. , #49297 ) ;
#28818 = CARTESIAN_POINT ( 'NONE',  ( -12.50000000000000000, -3.000000000000003109, -14.34180675897363599 ) ) ;
#28819 = CARTESIAN_POINT ( 'NONE',  ( -20.49977525862255590, 302.8459220885798686, -10.00124997875689203 ) ) ;
#28820 = DIRECTION ( 'NONE',  ( 0.000000000000000000, 0.000000000000000000, -1.000000000000000000 ) ) ;
#28821 = CARTESIAN_POINT ( 'NONE',  ( -40.60010613376132937, 436.1985323639528360, 6.054933560611875265 ) ) ;
#28823 = VECTOR ( 'NONE', #92633, 1000.000000000000000 ) ;
#28822 = CARTESIAN_POINT ( 'NONE',  ( 32.03720899076503059, 464.7921976803871758, 11.81820142135948437 ) ) ;
#28824 = LINE ( 'NONE', #84886, #81310 ) ;
#28825 = ORIENTED_EDGE ( 'NONE', *, *, #81751, .F. ) ;
#28826 = CARTESIAN_POINT ( 'NONE',  ( 91.87288384113435313, -60.00000000000000000, 10.25306695411674873 ) ) ;
#28828 = CONICAL_SURFACE ( 'NONE', #8115, 4.000000000000001776, 0.9599310885968808105 ) ;
#28827 = B_SPLINE_CURVE_WITH_KNOTS ( 'NONE', 3,
 ( #105652, #80307, #48474, #88953 ),
 .UNSPECIFIED., .F., .F.,
 ( 4, 4 ),
 ( 0.000000000000000000, 0.001935030059085813409 ),
 .UNSPECIFIED. ) ;
#28829 = DIRECTION ( 'NONE',  ( 0.000000000000000000, 0.000000000000000000, 1.000000000000000000 ) ) ;
#28831 = EDGE_CURVE ( 'NONE', #51169, #23419, #13258, .T. ) ;
#28830 =( LENGTH_UNIT ( ) NAMED_UNIT ( * ) SI_UNIT ( .MILLI., .METRE. ) );
#28832 =( BOUNDED_SURFACE ( )  B_SPLINE_SURFACE ( 2, 3, ( 
 ( #87361, #37243, #104052, #102475, #13441, #30190, #63625, #94396 ),
 ( #103532, #4843, #5377, #94933, #12909, #29167, #45835, #63079 ),
 ( #37776, #95979, #14492, #77675, #3785, #97024, #15037, #47927 ) ),
 .UNSPECIFIED., .F., .F., .F. ) 
 B_SPLINE_SURFACE_WITH_KNOTS ( ( 3, 3 ),
 ( 4, 2, 2, 4 ),
 ( 0.000000000000000000, 1.000000000000000000 ),
 ( 3.001947784535673236, 3.049999786562399784, 3.233185520617186448, 3.281237522643912996 ),
 .UNSPECIFIED. ) 
 GEOMETRIC_REPRESENTATION_ITEM ( )  RATIONAL_B_SPLINE_SURFACE ( (
 ( 1.000000000000000000, 1.000000000000000000, 1.000000000000000000, 1.000000000000000000, 1.000000000000000000, 1.000000000000000000, 1.000000000000000000, 1.000000000000000000),
 ( 1.857142857142858317, 1.857142857142858317, 1.857142857142858317, 1.857142857142858317, 1.857142857142858317, 1.857142857142858317, 1.857142857142858317, 1.857142857142858317),
 ( 1.000000000000000000, 1.000000000000000000, 1.000000000000000000, 1.000000000000000000, 1.000000000000000000, 1.000000000000000000, 1.000000000000000000, 1.000000000000000000) ) ) 
 REPRESENTATION_ITEM ( '' )  SURFACE ( )  );
#28833 = CARTESIAN_POINT ( 'NONE',  ( -6.309244321879762474, 40.00000000008454748, -71.19739392704494207 ) ) ;
#28834 = DIRECTION ( 'NONE',  ( -0.000000000000000000, -1.000000000000000000, -0.000000000000000000 ) ) ;
#28835 = ORIENTED_EDGE ( 'NONE', *, *, #28023, .F. ) ;
#28836 = CARTESIAN_POINT ( 'NONE',  ( -108.9347409199276342, -29.99999999999999289, 183.7868372424095185 ) ) ;
#28837 = ORIENTED_EDGE ( 'NONE', *, *, #10979, .F. ) ;
#28838 = DIRECTION ( 'NONE',  ( 0.000000000000000000, 0.000000000000000000, 1.000000000000000000 ) ) ;
#28839 = FACE_OUTER_BOUND ( 'NONE', #25776, .T. ) ;
#28840 = CARTESIAN_POINT ( 'NONE',  ( 16.11696382278844197, 21.57140452653176865, 2.149593460099603170 ) ) ;
#28841 = DIRECTION ( 'NONE',  ( -1.000000000000000000, 0.000000000000000000, 0.000000000000000000 ) ) ;
#28842 = VECTOR ( 'NONE', #36855, 999.9999999999998863 ) ;
#28843 = CARTESIAN_POINT ( 'NONE',  ( 7.188101187500001821, -28.43750000204839168, -2.977408999572650483 ) ) ;
#28844 = CARTESIAN_POINT ( 'NONE',  ( -17.53083185432715396, 45.00000000000000711, 63.44709590376286457 ) ) ;
#28845 = FACE_OUTER_BOUND ( 'NONE', #57861, .T. ) ;
#28846 = DIRECTION ( 'NONE',  ( -1.000000000000000000, 0.000000000000000000, 0.000000000000000000 ) ) ;
#28847 = ORIENTED_EDGE ( 'NONE', *, *, #58259, .F. ) ;
#28848 = CARTESIAN_POINT ( 'NONE',  ( 53.78349330513380266, 4.898587196589294500E-16, -4.000000000000007105 ) ) ;
#28849 = CIRCLE ( 'NONE', #44347, 2.000000000000000000 ) ;
#28850 = VECTOR ( 'NONE', #60301, 1000.000000000000000 ) ;
#28851 = VECTOR ( 'NONE', #12124, 999.9999999999998863 ) ;
#28852 = B_SPLINE_CURVE_WITH_KNOTS ( 'NONE', 3,
 ( #68908, #12232, #3090, #86164, #76973, #45163, #20928, #36036, #53763, #37627, #11695, #3631, #78561, #79099, #36567, #4694, #78044, #62404, #94236, #101784, #44630, #95298, #69436, #69957, #54267, #21427, #4161, #86691, #77518, #87209, #37092, #102855, #70490, #44089, #52164, #5222, #28467, #103383, #13284, #29532, #27952, #61345, #46213, #60815, #12760, #102315, #71008, #94782, #20399, #53243, #38151, #29022, #93705, #103901, #60294, #61887, #45683, #93168, #19334, #85076, #19857, #11160, #52692, #85619, #23018, #104428, #65035, #6796, #6253, #97930, #88267, #72067, #104977, #31636, #7315, #23548, #89324, #5740, #14880, #47251, #30577, #56390, #62932, #48305, #30045, #80675, #80152, #63471, #95827, #21957, #31118, #14346, #96367, #24082, #71527, #7849, #38660, #88789, #54808, #22497, #15418, #55337, #56923, #89849, #15954, #39715, #81201, #97387, #40229, #64006, #96881, #55849, #46733, #39190, #47773, #72591, #87740, #105497, #64519, #79623, #73097, #106010, #32156, #48832, #81722, #40754, #73644, #13819, #74707, #16487, #8915, #90918, #25138, #32701, #41820, #25691, #49366, #787, #83874, #82275, #91455, #33759, #100588, #257, #8387, #58555, #41289, #17569, #67177, #74177, #100057, #9986, #57996, #49907, #18102, #18646, #82815, #50961, #50430, #1880, #66632, #59084, #42889, #34836, #99516, #9432, #26747, #67707, #83342, #26224, #17031, #59624, #42353, #75240, #75786, #90374, #98455, #51504, #1337, #92494, #84420, #33224, #10513, #34301, #43428, #66099, #91970, #106548, #65568, #24607, #57456, #98973, #78438, #69311, #19199, #29405, #54146, #53115, #69828, #94101, #19728, #12109, #20267, #28337, #61761, #45038, #102188, #43955, #4562, #86036, #52565, #37499, #27821, #11569, #44499, #77923, #53636, #102727, #28889, #52036, #61213, #12632, #4032, #94657, #2422, #20803, #76309, #36962, #93579, #76846, #35365, #68234, #77388, #60691, #2951, #70363, #11037, #87086, #84948, #86569, #101127, #3502, #45566, #101663, #103258, #62286, #95177, #21308, #13161, #27288, #60171, #93038, #35908, #85490, #68782, #36443, #14223, #40110, #54677, #39600, #88143, #55216, #87614, #56263, #6671, #95695, #71404, #38027, #62807, #81087, #89199, #15297, #63345, #30451, #88663, #63875, #104849, #31518, #14753, #39065, #13696, #32038, #47127, #21838, #78971, #29921, #96241, #46608, #64400, #47656, #64918, #96763, #80551, #48184, #7197, #22894, #72472, #5096, #97274, #46089, #55732, #97801, #105379, #23421, #80024, #6136, #72985, #105891, #23966, #56808, #70886, #89732, #103779, #79504, #71946, #5615, #104301, #38539, #22372, #30993, #41701, #99379, #50310, #24495, #17443, #90253, #1202, #41173, #26101, #660, #58418, #81599, #7725, #49784, #15828, #99926, #8260, #65450, #17972, #98851, #67048, #33106, #82147, #83216, #40632, #25011, #74052, #32576, #66501, #16905, #91331, #73517, #34170, #50829, #57331, #65970, #25560, #42220, #82688, #9310, #75105, #49241, #140, #57865, #58956, #74584, #91844, #8793, #48710, #98341, #90792, #33627, #106417, #16356, #39309, #38774, #79215, #55974, #72191, #56515, #88386, #55451, #87852, #71123, #15535, #46326, #71640, #14459, #97500, #48428, #89445, #96996, #6373, #104549, #5850, #80799, #47371, #23133, #81320, #62518, #64121, #95403, #104013, #88904, #30157, #63043, #13933, #95946, #7431, #80261, #31233, #47892, #38262, #15001, #22069, #31751, #46845, #70602, #105095, #6912, #29644, #39832, #103495, #23664, #54927, #13403, #21543, #30700, #64632, #79745, #5340, #96477, #87323, #22615, #72708, #63588, #105608, #54378, #98576, #90496, #58671, #51078, #40880, #82402, #33882, #83460, #58119, #99643, #9560, #42467, #16605, #50027, #34426, #75363, #91047, #905, #57573, #67298, #25259, #66214, #99097, #41938, #33345, #17156, #100176, #16069, #24723, #73768, #1464, #8505, #26345, #48952, #66758, #41408, #83999, #74824, #49496, #74299, #59206, #82932, #89964, #57046, #92083, #18224, #40347, #375, #9029, #25818, #91573, #17680, #50544, #73225, #106126, #7968, #32282, #65152, #98051, #24200, #81846, #106667, #32815, #65688, #29013, #60288, #61337, #36027, #12224, #44080, #51623, #101257, #52154, #76426, #35484, #76965, #37084, #19848, #69948, #60804, #78035, #75903, #84542, #68901, #18775 ),
 .UNSPECIFIED., .F., .F.,
 ( 4, 2, 1, 1, 1, 1, 1, 1, 2, 2, 2, 2, 2, 2, 2, 1, 2, 2, 1, 1, 1, 2, 2, 2, 2, 2, 1, 2, 2, 1, 2, 2, 2, 1, 1, 1, 2, 2, 2, 1, 2, 2, 1, 1, 1, 2, 2, 2, 2, 1, 1, 2, 2, 1, 1, 2, 2, 2, 1, 1, 1, 2, 2, 1, 1, 2, 2, 2, 1, 1, 2, 2, 1, 1, 1, 1, 2, 2, 2, 2, 2, 2, 1, 2, 2, 1, 2, 2, 2, 2, 2, 1, 2, 2, 1, 1, 1, 1, 2, 2, 2, 1, 1, 2, 2, 1, 2, 2, 2, 1, 2, 2, 1, 1, 2, 2, 2, 2, 1, 2, 2, 2, 2, 2, 1, 2, 2, 1, 1, 2, 2, 2, 2, 1, 1, 2, 2, 2, 2, 2, 2, 1, 2, 2, 1, 2, 2, 2, 1, 2, 2, 1, 2, 2, 2, 1, 1, 1, 1, 2, 2, 2, 2, 1, 2, 2, 1, 1, 1, 2, 2, 2, 2, 2, 2, 1, 1, 1, 2, 2, 2, 2, 1, 2, 2, 1, 2, 2, 2, 2, 2, 2, 1, 1, 2, 2, 2, 2, 2, 2, 2, 1, 1, 2, 2, 1, 2, 2, 2, 2, 2, 2, 2, 2, 2, 1, 1, 2, 2, 1, 1, 1, 1, 2, 2, 2, 2, 2, 2, 2, 1, 1, 1, 1, 1, 2, 2, 1, 1, 2, 2, 2, 1, 1, 1, 2, 2, 1, 1, 1, 2, 2, 2, 2, 1, 1, 2, 2, 1, 1, 1, 2, 2, 2, 2, 1, 2, 2, 1, 1, 1, 2, 2, 2, 1, 1, 2, 2, 2, 2, 2, 2, 2, 1, 1, 1, 2, 2, 2, 2, 1, 2, 2, 1, 1, 1, 1, 2, 2, 2, 2, 2, 2, 1, 1, 1, 1, 2, 2, 2, 2, 2, 2, 2, 2, 2, 2, 2, 2, 4 ),
 ( 0.000000000000000000, 1.525878906243263716E-05, 3.051757812486527433E-05, 6.103515624973057576E-05, 0.0001220703124994611515, 0.0002441406249989222488, 0.0004882812499978443892, 0.0009765624999956887785, 0.001953124999991377123, 0.003906249999982753813, 0.007812499999965508493, 0.01562499999993101872, 0.02343749999989653068, 0.03124999999986202703, 0.03515624999984477694, 0.03564453124984255650, 0.03570556640609228588, 0.03573608398421715404, 0.03576660156234201526, 0.03588867187484149485, 0.03613281249984046095, 0.03710937499983629762, 0.03906249999982795706, 0.04687499999979457405, 0.05078124999977788601, 0.05273437499976953852, 0.05322265624976742215, 0.05346679687476636744, 0.05358886718726584703, 0.05371093749976533355, 0.05468749999976125348, 0.06249999999972860598, 0.06262207031222810638, 0.06274414062472760678, 0.06298828124972663534, 0.06347656249972469245, 0.06445312499972079279, 0.06640624999971297959, 0.07031249999969736708, 0.07128906249969346742, 0.07141113281219298170, 0.07147216796844274578, 0.07153320312469249598, 0.07177734374969177433, 0.07226562499969023390, 0.07421874999968423869, 0.07812499999967219277, 0.08593749999964817032, 0.08789062499964214736, 0.08886718749963912201, 0.08911132812463838648, 0.08923339843713799791, 0.08929443359338778974, 0.08935546874963759545, 0.08984374999963599950, 0.09374999999962320418, 0.1015624999995976691, 0.1054687499995848599, 0.1064453124995816818, 0.1069335937495801275, 0.1070556640620797112, 0.1071166992183295030, 0.1071472167964543920, 0.1071777343745792810, 0.1074218749995787259, 0.1093749999995740768, 0.1249999999995368705, 0.1406249999994996780, 0.1425781249994950706, 0.1428222656244944877, 0.1428527832026193767, 0.1428833007807442934, 0.1429443359369942934, 0.1430664062494943489, 0.1435546874994940714, 0.1445312499994932387, 0.1484374999994895750, 0.1562499999994824140, 0.1718749999994681199, 0.1874999999994538258, 0.2031249999994395317, 0.2109374999994323985, 0.2128906249994305944, 0.2138671874994296784, 0.2143554687494292066, 0.2148437499994287625, 0.2187499999994252653, 0.2499999999993973154, 0.2656249999993833266, 0.2812499999993693933, 0.2851562499993659516, 0.2856445312493656741, 0.2857055664056155075, 0.2857360839837404520, 0.2857666015618653965, 0.2858886718743650635, 0.2861328124993642308, 0.2871093749993612887, 0.2890624999993551825, 0.2968749999993313682, 0.3007812499993194333, 0.3027343749993134936, 0.3032226562493120503, 0.3034667968743114397, 0.3035888671868111066, 0.3037109374993107735, 0.3046874999993075539, 0.3124999999992819633, 0.3203124999992564281, 0.3212890624992533195, 0.3214111328117529309, 0.3215332031242525423, 0.3217773437492516542, 0.3222656249992499333, 0.3242187499992429944, 0.3281249999992290611, 0.3359374999992012500, 0.3378906249991942556, 0.3388671874991907584, 0.3391113281241897037, 0.3393554687491887045, 0.3398437499991866506, 0.3437499999991696087, 0.3476562499991526223, 0.3481445312491504573, 0.3482055664054001798, 0.3482666015616499022, 0.3483886718741493471, 0.3486328124991484589, 0.3496093749991446842, 0.3515624999991371902, 0.3554687499991220911, 0.3564453124991184274, 0.3569335937491165400, 0.3570556640616160404, 0.3571166992178658739, 0.3571777343741157074, 0.3574218749991152633, 0.3593749999991109889, 0.3632812499991022737, 0.3652343749990979993, 0.3657226562490968336, 0.3659667968740962785, 0.3660888671865960009, 0.3662109374990956678, 0.3671874999990931143, 0.3691406249990881738, 0.3701171874990857313, 0.3703613281240851762, 0.3704833984365848987, 0.3705444335928347321, 0.3706054687490845656, 0.3710937499990832333, 0.3749999999990726307, 0.3750610351553224642, 0.3751220703115722976, 0.3752441406240719091, 0.3754882812490710209, 0.3759765624990693555, 0.3769531249990659139, 0.3789062499990589750, 0.3828124999990452082, 0.3837890624990417665, 0.3839111328115412669, 0.3839263916006037114, 0.3839416503896661559, 0.3839721679677911004, 0.3840332031240412114, 0.3842773437490414334, 0.3847656249990420996, 0.3867187499990447086, 0.3906249999990498156, 0.3925781249990523691, 0.3928222656240527022, 0.3928833007803027577, 0.3929443359365528132, 0.3930664062490529798, 0.3935546874990535904, 0.3945312499990548671, 0.3984374999990598076, 0.4003906249990623056, 0.4013671874990635269, 0.4016113281240637489, 0.4017333984365638044, 0.4017944335928138044, 0.4018554687490638044, 0.4023437499990634714, 0.4062499999990610844, 0.4101562499990586419, 0.4106445312490583088, 0.4107055664053083088, 0.4107666015615583643, 0.4108886718740583088, 0.4111328124990581423, 0.4121093749990578092, 0.4140624999990570876, 0.4179687499990558108, 0.4199218749990552002, 0.4218749999990546451, 0.4257812499990533128, 0.4277343749990527022, 0.4282226562490524802, 0.4284667968740524802, 0.4285278320303024802, 0.4285888671865524802, 0.4287109374990525912, 0.4296874999990539790, 0.4374999999990648036, 0.4453124999990756838, 0.4531249999990865640, 0.4687499999991082134, 0.4843749999991299182, 0.4999999999991515676, 0.5312499999991950883, 0.5624999999992387201, 0.5703124999992494892, 0.5712890624992508215, 0.5714111328117509325, 0.5714721679680011546, 0.5715332031242513766, 0.5717773437492519317, 0.5722656249992531530, 0.5742187499992581490, 0.5781249999992679189, 0.5937499999993074429, 0.6249999999993862687, 0.6562499999994652056, 0.6874999999995440314, 0.7031249999995835553, 0.7109374999996032063, 0.7128906249996082023, 0.7138671874996106448, 0.7141113281246111999, 0.7142333984371115330, 0.7142639160152366440, 0.7142791748042991440, 0.7142944335933617550, 0.7143554687496118660, 0.7148437499996128652, 0.7187499999996208588, 0.7343749999996527222, 0.7421874999996688205, 0.7426757812496697087, 0.7427978515621699307, 0.7428283691402950417, 0.7428436279293576527, 0.7428588867184201527, 0.7429199218746702638, 0.7431640624996705968, 0.7441406249996721511, 0.7460937499996752598, 0.7499999999996815880, 0.7578124999996940225, 0.7617187499997003508, 0.7636718749997034594, 0.7641601562497042366, 0.7642822265622044586, 0.7643127441403295697, 0.7643432617184546807, 0.7644042968747046807, 0.7646484374997051248, 0.7656249999997067901, 0.7734374999997198907, 0.7812499999997329914, 0.7851562499997395417, 0.7856445312497404299, 0.7857055664059904299, 0.7857666015622405409, 0.7858886718747407629, 0.7861328124997410960, 0.7871093749997426503, 0.7890624999997459810, 0.7968749999997589706, 0.8007812499997655209, 0.8027343749997687405, 0.8032226562497696287, 0.8034667968747699618, 0.8037109374997702949, 0.8046874999997718492, 0.8124999999997845057, 0.8144531249997876143, 0.8154296874997891686, 0.8154907226560392797, 0.8155517578122892797, 0.8156738281247896127, 0.8159179687497900568, 0.8164062499997909450, 0.8183593749997947198, 0.8203124999997983835, 0.8212890624998001599, 0.8214111328123003819, 0.8214263916013629929, 0.8214416503904254929, 0.8214721679685504929, 0.8215332031248006039, 0.8217773437498008260, 0.8222656249998012701, 0.8242187499998036015, 0.8281249999998080424, 0.8359374999998170352, 0.8398437499998213651, 0.8417968749998236966, 0.8418579101560736966, 0.8419189453123238076, 0.8420410156248239186, 0.8422851562498241407, 0.8427734374998246958, 0.8437499999998258060, 0.8515624999998342437, 0.8554687499998385736, 0.8564453124998395728, 0.8574218749998405720, 0.8593749999998427924, 0.8749999999998602229, 0.8906249999998777644, 0.9062499999998953060, 0.9374999999999301670, 0.9687499999999651390, 0.9843749999999825695, 1.000000000000000000 ),
 .UNSPECIFIED. ) ;
#28854 = VERTEX_POINT ( 'NONE', #38574 ) ;
#28853 = CARTESIAN_POINT ( 'NONE',  ( 8.866506694866188809, 1.474610560812782335E-15, 0.000000000000000000 ) ) ;
#28855 = CARTESIAN_POINT ( 'NONE',  ( 78.67412638886875698, -56.84030183992913265, 157.0013697797242003 ) ) ;
#28856 = VERTEX_POINT ( 'NONE', #6710 ) ;
#28857 = CARTESIAN_POINT ( 'NONE',  ( 1.918196553303399110, -49.89542747347661589, 44.77704491145068744 ) ) ;
#28858 = AXIS2_PLACEMENT_3D ( 'NONE', #103140, #30323, #71813 ) ;
#28859 = CARTESIAN_POINT ( 'NONE',  ( -5.082755093536326818, -21.21875000204838457, 5.082755093536325042 ) ) ;
#28860 = CARTESIAN_POINT ( 'NONE',  ( -74.79081370483122271, -57.58316160299655451, 190.1003635006443346 ) ) ;
#28861 = EDGE_CURVE ( 'NONE', #26579, #91673, #71763, .T. ) ;
#28862 = ORIENTED_EDGE ( 'NONE', *, *, #38175, .T. ) ;
#28863 =( LENGTH_UNIT ( ) NAMED_UNIT ( * ) SI_UNIT ( .MILLI., .METRE. ) );
#28864 = CARTESIAN_POINT ( 'NONE',  ( -4.815811321232737363, -11.80076707697374516, 3.581116321197038932 ) ) ;
#28865 = EDGE_CURVE ( 'NONE', #34382, #87882, #72507, .T. ) ;
#28866 = CARTESIAN_POINT ( 'NONE',  ( -9.989690267985798400, 81.02555583405090545, -0.5238310916885774438 ) ) ;
#28867 = CARTESIAN_POINT ( 'NONE',  ( 0.5846921733595837889, -70.55117423362948159, 13.00919072386916397 ) ) ;
#28868 = VECTOR ( 'NONE', #1564, 1000.000000000000000 ) ;
#28869 = CARTESIAN_POINT ( 'NONE',  ( 5.656854249492378806, -15.87500000409677092, 5.656854249492381470 ) ) ;
#28870 = CARTESIAN_POINT ( 'NONE',  ( -40.04143003125063416, -26.34375225975082202, 35.98697943332009430 ) ) ;
#28871 = FACE_OUTER_BOUND ( 'NONE', #56780, .T. ) ;
#28872 = CARTESIAN_POINT ( 'NONE',  ( -7.000000000000000000, 8.572527594031471218E-16, -9.975036109638290682 ) ) ;
#28873 = VECTOR ( 'NONE', #83524, 1000.000000000000000 ) ;
#28874 = CARTESIAN_POINT ( 'NONE',  ( 7.421727621019012844, -2.999999999999999112, -70.37058875308096617 ) ) ;
#28875 = CARTESIAN_POINT ( 'NONE',  ( 4.152134392769949223, 52.11347441213486320, 6.757182654997005322 ) ) ;
#28876 = CARTESIAN_POINT ( 'NONE',  ( 51.88291765283141643, 135.6183258647170078, 182.1969486012845891 ) ) ;
#28877 = CARTESIAN_POINT ( 'NONE',  ( -12.31568180227341891, -4.628506154427563857, 20.34130839979936312 ) ) ;
#28878 = ORIENTED_EDGE ( 'NONE', *, *, #45394, .F. ) ;
#28879 = CARTESIAN_POINT ( 'NONE',  ( -6.358572135259356273, -49.57572298635458452, 39.47396800149780205 ) ) ;
#28880 = DIRECTION ( 'NONE',  ( 0.000000000000000000, 1.000000000000000000, 0.000000000000000000 ) ) ;
#28881 = AXIS2_PLACEMENT_3D ( 'NONE', #33853, #49461, #89931 ) ;
#28882 = FACE_OUTER_BOUND ( 'NONE', #39938, .T. ) ;
#28883 = CARTESIAN_POINT ( 'NONE',  ( 72.41334042352660560, -30.15556180264357167, -28.78532156097261563 ) ) ;
#28884 = CARTESIAN_POINT ( 'NONE',  ( -73.96231721666636361, -30.00000000000000000, 108.7202594212511286 ) ) ;
#28885 = DIRECTION ( 'NONE',  ( -1.000000000000000000, -1.224606353822377258E-16, -0.000000000000000000 ) ) ;
#28886 = ADVANCED_FACE ( 'NONE', ( #6170 ), #82727, .T. ) ;
#28887 = ORIENTED_EDGE ( 'NONE', *, *, #92131, .F. ) ;
#28888 = CARTESIAN_POINT ( 'NONE',  ( -26.48510057655429506, 37.08852406309646454, -7.709608770315281134 ) ) ;
#28889 = CARTESIAN_POINT ( 'NONE',  ( 77.70094160008299866, -57.51527222009625007, 196.1490637833984181 ) ) ;
#28890 = CARTESIAN_POINT ( 'NONE',  ( 6.145467199749146125, 47.99999999999999289, -92.99666842398180222 ) ) ;
#28891 = DIRECTION ( 'NONE',  ( 0.000000000000000000, -1.000000000000000000, 0.000000000000000000 ) ) ;
#28892 = CARTESIAN_POINT ( 'NONE',  ( -15.68546860017134748, 21.68927415055489405, -4.769872285932397205 ) ) ;
#28893 = DIRECTION ( 'NONE',  ( 0.000000000000000000, 0.000000000000000000, -1.000000000000000000 ) ) ;
#28894 = CARTESIAN_POINT ( 'NONE',  ( -58.54394063265895909, -60.00000000000000711, 95.84204639138707194 ) ) ;
#28895 = DIRECTION ( 'NONE',  ( -1.000000000000000000, -0.000000000000000000, -0.000000000000000000 ) ) ;
#28896 = CARTESIAN_POINT ( 'NONE',  ( 0.000000000000000000, 0.000000000000000000, -10.00000000000000355 ) ) ;
#28897 = CARTESIAN_POINT ( 'NONE',  ( 22.66220480930525127, 50.00000000000000000, 59.06576954297840842 ) ) ;
#28898 = MECHANICAL_DESIGN_GEOMETRIC_PRESENTATION_REPRESENTATION (  '', ( #39178 ), #15044 ) ;
#28899 = CARTESIAN_POINT ( 'NONE',  ( -85.11955292133191620, -50.19866990164982212, 189.4213824591150228 ) ) ;
#28900 = VERTEX_POINT ( 'NONE', #106457 ) ;
#28901 = CARTESIAN_POINT ( 'NONE',  ( 35.51316232729440259, 414.8269433707833969, 6.894890188973520573 ) ) ;
#28902 = CARTESIAN_POINT ( 'NONE',  ( -3.020169591079187033, -35.99429810687945519, 29.88393149923355452 ) ) ;
#28903 = CARTESIAN_POINT ( 'NONE',  ( -5.744149845079463468, 41.99823332147487065, -59.60979981975896891 ) ) ;
#28904 = CARTESIAN_POINT ( 'NONE',  ( 0.000000000000000000, -30.00000000000000000, 0.000000000000000000 ) ) ;
#28905 = FACE_OUTER_BOUND ( 'NONE', #76646, .T. ) ;
#28906 = CARTESIAN_POINT ( 'NONE',  ( 29.99397490504468067, 1.005902684993158047, -14.99698745252235099 ) ) ;
#28907 = CARTESIAN_POINT ( 'NONE',  ( 38.67643969787641822, 490.7806551866269160, 11.84688141262719441 ) ) ;
#28908 = CARTESIAN_POINT ( 'NONE',  ( 44.17836536378482748, 435.2619773020558682, 14.65562696767865170 ) ) ;
#28909 = CIRCLE ( 'NONE', #89149, 3.309500000000001663 ) ;
#28910 = ORIENTED_EDGE ( 'NONE', *, *, #38555, .T. ) ;
#28911 = AXIS2_PLACEMENT_3D ( 'NONE', #41059, #49673, #66391 ) ;
#28912 = CARTESIAN_POINT ( 'NONE',  ( 21.29592979798552577, 302.9478885984597127, -9.979576327195278651 ) ) ;
#28913 = CARTESIAN_POINT ( 'NONE',  ( 13.22204626516810322, 24.10488446132543316, 3.477574009107253339 ) ) ;
#28914 = CARTESIAN_POINT ( 'NONE',  ( -13.66642973271509831, 3.860411657743955287E-12, 17.78317311657911404 ) ) ;
#28915 = CARTESIAN_POINT ( 'NONE',  ( 9.481087872249203130, 53.60657805712472879, -1.932842531519640250 ) ) ;
#28916 = CARTESIAN_POINT ( 'NONE',  ( 99.06540890750190442, -59.99999999999989342, 60.62284496578245552 ) ) ;
#28917 = CARTESIAN_POINT ( 'NONE',  ( -78.59050543240782360, -42.96833819150651124, 140.9031260219249759 ) ) ;
#28918 = EDGE_LOOP ( 'NONE', ( #51134, #10444, #90988, #85874, #990 ) ) ;
#28919 = CARTESIAN_POINT ( 'NONE',  ( 22.33349330513380693, 1.593028355512270962E-15, 0.000000000000000000 ) ) ;
#28920 = FACE_OUTER_BOUND ( 'NONE', #14751, .T. ) ;
#28921 = AXIS2_PLACEMENT_3D ( 'NONE', #1207, #34176, #98347 ) ;
#28922 = CARTESIAN_POINT ( 'NONE',  ( 19.63101818396287257, -57.67185339817164191, 42.14267493330406467 ) ) ;
#28923 = CONICAL_SURFACE ( 'NONE', #23734, 4.000000000000001776, 0.9599310885968774798 ) ;
#28924 = AXIS2_PLACEMENT_3D ( 'NONE', #86491, #30366, #55646 ) ;
#28925 = SURFACE_STYLE_USAGE ( .BOTH. , #79536 ) ;
#28926 = CARTESIAN_POINT ( 'NONE',  ( 41.66809339685227087, 324.8386627565116100, 5.312837162286244919 ) ) ;
#28927 = CYLINDRICAL_SURFACE ( 'NONE', #21776, 5.000000000000002665 ) ;
#28928 = ORIENTED_EDGE ( 'NONE', *, *, #100102, .T. ) ;
#28929 = DIRECTION ( 'NONE',  ( 0.5735764363510466035, -0.8191520442889914655, 1.003171929053524500E-16 ) ) ;
#28930 = DIRECTION ( 'NONE',  ( 0.000000000000000000, 1.000000000000000000, 0.000000000000000000 ) ) ;
#28931 = CARTESIAN_POINT ( 'NONE',  ( -2.977408999572650039, -27.68750000204838813, -7.188101187500001821 ) ) ;
#28932 = ORIENTED_EDGE ( 'NONE', *, *, #53491, .T. ) ;
#28933 = CARTESIAN_POINT ( 'NONE',  ( 0.000000000000000000, 0.000000000000000000, 0.000000000000000000 ) ) ;
#28934 = AXIS2_PLACEMENT_3D ( 'NONE', #77406, #28358, #86589 ) ;
#28935 = CARTESIAN_POINT ( 'NONE',  ( 101.4868948250290259, 1.016364837396684119E-14, 0.000000000000000000 ) ) ;
#28936 = CARTESIAN_POINT ( 'NONE',  ( 6.675188390063539146, 41.63185015293624502, -70.36443416096713577 ) ) ;
#28937 = EDGE_CURVE ( 'NONE', #15295, #28791, #99325, .T. ) ;
#28938 = CARTESIAN_POINT ( 'NONE',  ( -16.80257523370084272, 45.55115703057131071, -6.650239426131814291 ) ) ;
#28939 = EDGE_CURVE ( 'NONE', #98966, #42513, #83252, .T. ) ;
#28940 = ORIENTED_EDGE ( 'NONE', *, *, #52749, .T. ) ;
#28941 = CARTESIAN_POINT ( 'NONE',  ( 2.602085213965210642E-15, 15.58845726811991561, -11.79422863405993382 ) ) ;
#28943 = CARTESIAN_POINT ( 'NONE',  ( 27.89594507718583571, -53.38588701379882906, 34.87338555987020072 ) ) ;
#28942 = CARTESIAN_POINT ( 'NONE',  ( -66.64776185298879341, -30.00000000000000711, 114.0837597745640721 ) ) ;
#28944 = CARTESIAN_POINT ( 'NONE',  ( 26.13315753361836613, 60.33964880548970910, -13.06657876680917774 ) ) ;
#28945 = ORIENTED_EDGE ( 'NONE', *, *, #69551, .T. ) ;
#28946 = EDGE_CURVE ( 'NONE', #9279, #81048, #90731, .T. ) ;
#28947 = CARTESIAN_POINT ( 'NONE',  ( -35.43501430766470861, -53.36447985331461297, 38.23648758541151693 ) ) ;
#28948 = UNCERTAINTY_MEASURE_WITH_UNIT (LENGTH_MEASURE( 1.000000000000000082E-05 ), #80219, 'distance_accuracy_value', 'NONE');
#28949 = ORIENTED_EDGE ( 'NONE', *, *, #74261, .F. ) ;
#28950 =( NAMED_UNIT ( * ) PLANE_ANGLE_UNIT ( ) SI_UNIT ( $, .RADIAN. ) );
#28951 = CARTESIAN_POINT ( 'NONE',  ( -43.71037717921183230, 462.3391554988663756, 4.824299547743598815 ) ) ;
#28952 = CARTESIAN_POINT ( 'NONE',  ( -1.096874481644934729, 51.92397332506016028, -8.379925569044138101 ) ) ;
#28953 = CARTESIAN_POINT ( 'NONE',  ( 42.40769230769231513, 4.172000000000003261, 5.109226446042759579E-16 ) ) ;
#28954 = SURFACE_STYLE_USAGE ( .BOTH. , #20870 ) ;
#28956 = ORIENTED_EDGE ( 'NONE', *, *, #2626, .T. ) ;
#28955 = AXIS2_PLACEMENT_3D ( 'NONE', #78615, #4216, #36623 ) ;
#28957 = CARTESIAN_POINT ( 'NONE',  ( -51.86356884536327527, -38.33854880839309232, 73.08413421716038272 ) ) ;
#28958 = CARTESIAN_POINT ( 'NONE',  ( 17.50000000000002487, 45.90000000000000568, 62.61746187599675295 ) ) ;
#28959 = CARTESIAN_POINT ( 'NONE',  ( 98.90803512229713590, -29.99999999999997868, 189.0481524369670012 ) ) ;
#28960 = CARTESIAN_POINT ( 'NONE',  ( -13.24996097722020139, 3.894558718262700392, -6.960810507241065537 ) ) ;
#28962 = EDGE_CURVE ( 'NONE', #58076, #92260, #1148, .T. ) ;
#28961 = CARTESIAN_POINT ( 'NONE',  ( 4.165977904505308693, 16.00000000000000000, 9.090909090909091717 ) ) ;
#28963 =( GEOMETRIC_REPRESENTATION_CONTEXT ( 3 ) GLOBAL_UNCERTAINTY_ASSIGNED_CONTEXT ( ( #29445 ) ) GLOBAL_UNIT_ASSIGNED_CONTEXT ( ( #13655, #95138, #4516 ) ) REPRESENTATION_CONTEXT ( 'NONE', 'WORKASPACE' ) );
#28964 = CARTESIAN_POINT ( 'NONE',  ( 81.43483218857002726, -30.00000000000000355, -9.794887574534724806 ) ) ;
#28965 = LINE ( 'NONE', #5688, #46731 ) ;
#28966 = ORIENTED_EDGE ( 'NONE', *, *, #2395, .T. ) ;
#28967 = B_SPLINE_CURVE_WITH_KNOTS ( 'NONE', 3,
 ( #104664, #30816, #56632, #55561, #90075, #80379, #106239, #23785, #48540, #98161, #88497, #6491, #39942, #64743, #32399, #7545, #72813, #5962, #55037, #38886, #40461, #30273, #22186, #56081, #16182, #63702, #73341, #96589, #39422, #80914, #105720, #87969, #7025, #72297, #14049, #23243, #65271, #24316, #22723, #14575, #47481, #57163, #79329, #15120, #105204, #5448, #31350, #97619 ),
 .UNSPECIFIED., .F., .F.,
 ( 4, 2, 2, 2, 2, 2, 2, 2, 2, 2, 2, 2, 2, 2, 2, 2, 2, 2, 2, 2, 2, 2, 2, 4 ),
 ( -5.999999999670915252E-08, 0.001090263057642365876, 0.002180586115284728361, 0.003270909172927090412, 0.003816070701748271003, 0.004361232230569451161, 0.004906393759390633054, 0.005451555288211814079, 0.006541878345854297561, 0.008722524461139262789, 0.01090317057642422628, 0.01308381669170918804, 0.01744510892227911850, 0.02616769338341913553, 0.03052898561398914926, 0.03489027784455915604, 0.04361286230569918348, 0.05233544676683919011, 0.06978061568911922419, 0.08722578461139925132, 0.1046709535336792785, 0.1221161224559593056, 0.1308387069170994232, 0.1395612913782395270 ),
 .UNSPECIFIED. ) ;
#28968 = VERTEX_POINT ( 'NONE', #98377 ) ;
#28969 = VECTOR ( 'NONE', #71403, 1000.000000000000000 ) ;
#28970 = EDGE_LOOP ( 'NONE', ( #4212, #721, #837, #80820, #10524 ) ) ;
#28971 = DIRECTION ( 'NONE',  ( -1.000000000000000000, 0.000000000000000000, 0.000000000000000000 ) ) ;
#28972 = CARTESIAN_POINT ( 'NONE',  ( 52.56491209535273867, 39.42572890907101169, -38.23519342730394044 ) ) ;
#28973 = CARTESIAN_POINT ( 'NONE',  ( -36.81733651310691613, 25.76199643843586173, -13.21939386992400500 ) ) ;
#28974 = CARTESIAN_POINT ( 'NONE',  ( 17.33349330513380337, 1.593028355512270567E-15, 0.000000000000000000 ) ) ;
#28975 = CARTESIAN_POINT ( 'NONE',  ( -1.366857229432719700, -69.63343833532438509, 12.80410507582288560 ) ) ;
#28976 = CARTESIAN_POINT ( 'NONE',  ( -7.801339272325196639, -88.58731471959700343, -1.788609912539668612 ) ) ;
#28977 = SURFACE_STYLE_FILL_AREA ( #19296 ) ;
#28978 = VECTOR ( 'NONE', #92156, 1000.000000000000227 ) ;
#28979 = ORIENTED_EDGE ( 'NONE', *, *, #61711, .F. ) ;
#28980 = CARTESIAN_POINT ( 'NONE',  ( 5.036189802310915731, 48.00000000000000000, -76.26213611587833441 ) ) ;
#28981 = ORIENTED_EDGE ( 'NONE', *, *, #41792, .F. ) ;
#28982 = CARTESIAN_POINT ( 'NONE',  ( -4.472135954999576057, -64.72670096487361491, -4.000000000000002665 ) ) ;
#28983 = DIRECTION ( 'NONE',  ( -1.000000000000000000, -0.000000000000000000, -0.000000000000000000 ) ) ;
#28984 = CARTESIAN_POINT ( 'NONE',  ( 46.36650669486618881, 1.474610560812782335E-15, 0.000000000000000000 ) ) ;
#28985 = CARTESIAN_POINT ( 'NONE',  ( 25.04416970470931147, 295.6688433518704642, 2.112457367892493831 ) ) ;
#28986 = STYLED_ITEM ( 'NONE', ( #32467 ), #205 ) ;
#28987 = CARTESIAN_POINT ( 'NONE',  ( 6.562974947121715807, -7.579827465851462165, -0.5629870116737624164 ) ) ;
#28988 = CARTESIAN_POINT ( 'NONE',  ( 63.03724330110081553, -49.91051537755201650, 85.83604783815560779 ) ) ;
#28989 = VERTEX_POINT ( 'NONE', #41205 ) ;
#28990 = CARTESIAN_POINT ( 'NONE',  ( 29.68315524076926337, 8.302504244945327017, -42.10535821593530414 ) ) ;
#28991 = CARTESIAN_POINT ( 'NONE',  ( 35.58361799548379167, 1.482358050883964840E-15, 0.000000000000000000 ) ) ;
#28992 = CARTESIAN_POINT ( 'NONE',  ( -5.744562646538028616, 12.99999999999999289, -4.000000000000000000 ) ) ;
#28993 = CARTESIAN_POINT ( 'NONE',  ( -8.720088082017248610, 51.50350844580864162, 4.031152949374572358 ) ) ;
#28994 = EDGE_CURVE ( 'NONE', #44795, #25681, #61484, .T. ) ;
#28995 = ORIENTED_EDGE ( 'NONE', *, *, #56093, .F. ) ;
#28996 = B_SPLINE_CURVE_WITH_KNOTS ( 'NONE', 3,
 ( #92112, #85094, #60313, #26897, #18255, #75935, #76456, #59772, #51651, #84575, #68392, #51114, #10134, #10652, #43570, #101286 ),
 .UNSPECIFIED., .F., .F.,
 ( 4, 2, 2, 2, 2, 2, 2, 4 ),
 ( 6.992893892674702526E-18, 0.0001384951335132145981, 0.0002769902670264222030, 0.0005539805340528701017, 0.0008309708010793181087, 0.001107961068105766007, 0.001661941602158780850, 0.002215922136211795259 ),
 .UNSPECIFIED. ) ;
#28997 = SHAPE_REPRESENTATION_RELATIONSHIP ( 'NONE' , 'NONE' ,  #52881, #75546 ) ;
#28998 = CARTESIAN_POINT ( 'NONE',  ( 0.5805565836007618996, 3.752776749732569250, 6.499999999999997335 ) ) ;
#28999 = CIRCLE ( 'NONE', #92675, 1.000000000000000888 ) ;
#29000 = AXIS2_PLACEMENT_3D ( 'NONE', #60081, #33672, #9892 ) ;
#29001 = CIRCLE ( 'NONE', #87706, 4.000000000000001776 ) ;
#29002 = EDGE_CURVE ( 'NONE', #49140, #10334, #106249, .T. ) ;
#29003 = EDGE_CURVE ( 'NONE', #25050, #87544, #76943, .T. ) ;
#29004 = CARTESIAN_POINT ( 'NONE',  ( 0.000000000000000000, 0.000000000000000000, -3.393184225085859929 ) ) ;
#29005 = CARTESIAN_POINT ( 'NONE',  ( -4.989154468854752454E-15, -18.92596047533412573, -20.36976895023282097 ) ) ;
#29006 = MECHANICAL_DESIGN_GEOMETRIC_PRESENTATION_REPRESENTATION (  '', ( #40945 ), #58185 ) ;
#29007 = FILL_AREA_STYLE ('',( #69943 ) ) ;
#29008 = AXIS2_PLACEMENT_3D ( 'NONE', #35581, #19416, #52250 ) ;
#29009 = CARTESIAN_POINT ( 'NONE',  ( 86.38779590130293684, -17.19466876150733370, 181.4510809460217615 ) ) ;
#29010 = CARTESIAN_POINT ( 'NONE',  ( -5.354260345751012728, 36.72647500040412183, -54.26263299992344713 ) ) ;
#29011 = CARTESIAN_POINT ( 'NONE',  ( -9.465790868675496128, 9.886732697667790504, 0.000000000000000000 ) ) ;
#29012 = ORIENTED_EDGE ( 'NONE', *, *, #97494, .T. ) ;
#29013 = CARTESIAN_POINT ( 'NONE',  ( 76.23378044719352431, -57.67121141546430607, -32.09450996628105912 ) ) ;
#29014 = CARTESIAN_POINT ( 'NONE',  ( 58.71306015749776464, -29.11378994003339216, -25.44451803556423641 ) ) ;
#29015 = CARTESIAN_POINT ( 'NONE',  ( 26.84999999999999787, -3.309499999999999886, 0.000000000000000000 ) ) ;
#29016 = CARTESIAN_POINT ( 'NONE',  ( 13.64640293162734785, -51.35851448446996415, 30.13230102324352799 ) ) ;
#29017 = CARTESIAN_POINT ( 'NONE',  ( 5.000000000000000000, -15.43641607416063266, 12.61250543006137725 ) ) ;
#29018 = CARTESIAN_POINT ( 'NONE',  ( -101.1538706603591180, -30.00000000000000355, 168.9986721791281639 ) ) ;
#29019 = EDGE_CURVE ( 'NONE', #81142, #38220, #66617, .T. ) ;
#29020 = CIRCLE ( 'NONE', #44519, 3.309500000000007880 ) ;
#29021 = DIRECTION ( 'NONE',  ( -0.5735764363510497121, 0.8191520442889892450, 1.003171929053521665E-16 ) ) ;
#29022 = CARTESIAN_POINT ( 'NONE',  ( 31.98563216593261416, -57.68901072815521758, 46.54681308492085634 ) ) ;
#29023 = DIRECTION ( 'NONE',  ( -1.000000000000000000, -1.224606353822377258E-16, -0.000000000000000000 ) ) ;
#29024 = ADVANCED_FACE ( 'NONE', ( #32615 ), #52836, .T. ) ;
#29025 = AXIS2_PLACEMENT_3D ( 'NONE', #13233, #21374, #5165 ) ;
#29026 = CARTESIAN_POINT ( 'NONE',  ( -36.15880341458275637, 40.31104264147870708, -58.06768400292240528 ) ) ;
#29027 = CARTESIAN_POINT ( 'NONE',  ( -18.09799070311343527, 49.99999999999999289, 61.76230565999977529 ) ) ;
#29028 =( LENGTH_UNIT ( ) NAMED_UNIT ( * ) SI_UNIT ( .MILLI., .METRE. ) );
#29029 = DIRECTION ( 'NONE',  ( 0.000000000000000000, -0.9221233147934838614, -0.3868961001538753219 ) ) ;
#29030 = ADVANCED_FACE ( 'NONE', ( #1790, #698, #64950, #9346, #74619 ), #95889, .T. ) ;
#29031 = CIRCLE ( 'NONE', #49662, 4.172000000000001485 ) ;
#29032 = ORIENTED_EDGE ( 'NONE', *, *, #94907, .T. ) ;
#29033 = CARTESIAN_POINT ( 'NONE',  ( 40.22629662633006831, 485.6695299958086594, -4.459425866601474553 ) ) ;
#29034 = CARTESIAN_POINT ( 'NONE',  ( -9.536842176398140580, 107.6423536988398553, 3.014135744008186624 ) ) ;
#29035 = CARTESIAN_POINT ( 'NONE',  ( -18.30425709642254972, -60.36451714365048105, 34.31014664571683426 ) ) ;
#29037 = CARTESIAN_POINT ( 'NONE',  ( 1.130211174915330963, 36.55067354015870507, -29.03997593543449796 ) ) ;
#29036 = CARTESIAN_POINT ( 'NONE',  ( 0.000000000000000000, 0.9999999999999970024, 7.000000000000000000 ) ) ;
#29038 = ORIENTED_EDGE ( 'NONE', *, *, #14582, .T. ) ;
#29039 = VECTOR ( 'NONE', #16500, 1000.000000000000000 ) ;
#29040 = CARTESIAN_POINT ( 'NONE',  ( 15.64030048137866835, 6.456385560667919243, -7.561819230143238535 ) ) ;
#29041 = EDGE_LOOP ( 'NONE', ( #56918, #37421, #95664, #10376, #3795, #69425 ) ) ;
#29042 = CARTESIAN_POINT ( 'NONE',  ( -12.44754381327812354, 42.20908535986962562, -93.38745647781213677 ) ) ;
#29043 = AXIS2_PLACEMENT_3D ( 'NONE', #38483, #88084, #47065 ) ;
#29044 = DIRECTION ( 'NONE',  ( 1.000000000000000000, -0.000000000000000000, -0.000000000000000000 ) ) ;
#29045 = DIRECTION ( 'NONE',  ( -1.000000000000000000, -1.224606353822377258E-16, -0.000000000000000000 ) ) ;
#29046 = EDGE_LOOP ( 'NONE', ( #752, #98944, #42281, #80518, #48238, #15966 ) ) ;
#29047 = SURFACE_STYLE_FILL_AREA ( #86716 ) ;
#29048 = SURFACE_SIDE_STYLE ('',( #53270 ) ) ;
#29049 = CARTESIAN_POINT ( 'NONE',  ( 101.0450726704344646, -45.28112087516579010, 191.2503734327964366 ) ) ;
#29050 = AXIS2_PLACEMENT_3D ( 'NONE', #52874, #36210, #93346 ) ;
#29052 = LINE ( 'NONE', #14375, #25430 ) ;
#29051 = FILL_AREA_STYLE_COLOUR ( '', #63056 ) ;
#29053 = EDGE_LOOP ( 'NONE', ( #78466, #79266, #22340, #17961 ) ) ;
#29054 = ORIENTED_EDGE ( 'NONE', *, *, #31655, .T. ) ;
#29055 = EDGE_LOOP ( 'NONE', ( #101048, #44579, #91610, #98305 ) ) ;
#29056 = CARTESIAN_POINT ( 'NONE',  ( 26.49263286547231644, 310.1913357440211030, 10.20160702900524008 ) ) ;
#29057 = CARTESIAN_POINT ( 'NONE',  ( -1.469576158976823947E-15, -14.56250000409677092, 8.000000000000000000 ) ) ;
#29058 = PRESENTATION_STYLE_ASSIGNMENT (( #77015 ) ) ;
#29059 = ORIENTED_EDGE ( 'NONE', *, *, #79102, .F. ) ;
#29060 = EDGE_CURVE ( 'NONE', #99083, #13309, #24002, .T. ) ;
#29061 = CARTESIAN_POINT ( 'NONE',  ( -1.494796585009948497, -5.000000000000002665, -71.77219432632048779 ) ) ;
#29062 = CARTESIAN_POINT ( 'NONE',  ( -5.788216603250401882, 41.97741512851646917, -69.85767952489079846 ) ) ;
#29063 = CARTESIAN_POINT ( 'NONE',  ( -96.34159525672876612, -59.99999999990227906, 41.34496478704701872 ) ) ;
#29064 = CARTESIAN_POINT ( 'NONE',  ( 0.000000000000000000, 45.89575828009193259, 0.000000000000000000 ) ) ;
#29065 = CARTESIAN_POINT ( 'NONE',  ( 51.58253327500602126, -59.99999999998549782, -40.00153396047142706 ) ) ;
#29066 = CARTESIAN_POINT ( 'NONE',  ( -11.77542311866812774, -5.000000000000000000, -11.45362038306368646 ) ) ;
#29067 = CARTESIAN_POINT ( 'NONE',  ( -5.668939695963768344, 41.88723863199725628, -59.02759498664629945 ) ) ;
#29068 = CIRCLE ( 'NONE', #72051, 5.000000000000010658 ) ;
#29070 = CARTESIAN_POINT ( 'NONE',  ( 11.40768022813701243, -46.43473930232784141, 31.65783319488408409 ) ) ;
#29069 = CARTESIAN_POINT ( 'NONE',  ( -97.09821068641753072, -30.00000000000001776, 79.69957433219180132 ) ) ;
#29071 = CIRCLE ( 'NONE', #23890, 5.000000000000002665 ) ;
#29072 = ADVANCED_FACE ( 'NONE', ( #98887 ), #57984, .T. ) ;
#29073 = EDGE_CURVE ( 'NONE', #93124, #6205, #18456, .T. ) ;
#29074 = CARTESIAN_POINT ( 'NONE',  ( -48.45733930310002080, -56.82700549898684983, 53.79929747904154169 ) ) ;
#29075 = CARTESIAN_POINT ( 'NONE',  ( -2.654566931710991007, 20.85574759830042524, 6.480122636992501128 ) ) ;
#29076 = ORIENTED_EDGE ( 'NONE', *, *, #7193, .T. ) ;
#29077 = CARTESIAN_POINT ( 'NONE',  ( 41.74778363246261392, 460.3875427940046166, 2.379529480111751916 ) ) ;
#29078 = AXIS2_PLACEMENT_3D ( 'NONE', #23254, #31874, #65813 ) ;
#29079 = CARTESIAN_POINT ( 'NONE',  ( 16.91815790875667602, 37.08283480489694028, 21.80698433968582961 ) ) ;
#29080 = EDGE_CURVE ( 'NONE', #33265, #37041, #20171, .T. ) ;
#29081 = CARTESIAN_POINT ( 'NONE',  ( 74.60950000000003968, 0.000000000000000000, 0.000000000000000000 ) ) ;
#29082 = EDGE_LOOP ( 'NONE', ( #72035, #39931, #47091, #65842 ) ) ;
#29083 = CARTESIAN_POINT ( 'NONE',  ( -14.85144930561877175, -6.995911484127552704, 13.28113257175721706 ) ) ;
#29084 = ORIENTED_EDGE ( 'NONE', *, *, #62503, .T. ) ;
#29085 = CARTESIAN_POINT ( 'NONE',  ( 108.6711098457755611, -30.00000000000668621, 155.0946490741732191 ) ) ;
#29087 = ADVANCED_FACE ( 'NONE', ( #66542 ), #66009, .T. ) ;
#29086 = CARTESIAN_POINT ( 'NONE',  ( 7.054522925320324767, 41.71556257522360767, -59.55896313260248576 ) ) ;
#29088 = CARTESIAN_POINT ( 'NONE',  ( -5.022013495247517945, 18.64316884711714195, -38.36535705883633085 ) ) ;
#29089 = CARTESIAN_POINT ( 'NONE',  ( 100.7015874939240376, -30.00000000000000000, 161.8710660039678828 ) ) ;
#29090 = CARTESIAN_POINT ( 'NONE',  ( 6.249999999999998224, 0.000000000000000000, 0.000000000000000000 ) ) ;
#29091 = ORIENTED_EDGE ( 'NONE', *, *, #15124, .F. ) ;
#29092 = EDGE_LOOP ( 'NONE', ( #25526, #71995, #99182, #74564 ) ) ;
#29093 = VERTEX_POINT ( 'NONE', #34212 ) ;
#29094 = CARTESIAN_POINT ( 'NONE',  ( 54.36390350096709057, -49.90582396615677396, 63.10843653790805519 ) ) ;
#29095 = CIRCLE ( 'NONE', #3241, 8.000000000000000000 ) ;
#29096 = CARTESIAN_POINT ( 'NONE',  ( 42.33349330513380693, 1.593028355512270567E-15, 0.000000000000000000 ) ) ;
#29097 = DIRECTION ( 'NONE',  ( 0.000000000000000000, -1.000000000000000000, 0.000000000000000000 ) ) ;
#29099 = VERTEX_POINT ( 'NONE', #82183 ) ;
#29098 = COLOUR_RGB ( '', 0.09019608, 0.27058824, 0.51372549) ;
#29100 = CARTESIAN_POINT ( 'NONE',  ( 9.221216839714873714, 106.0475974816897917, 3.869414262756992517 ) ) ;
#29101 = AXIS2_PLACEMENT_3D ( 'NONE', #81397, #83536, #8586 ) ;
#29102 = VERTEX_POINT ( 'NONE', #16944 ) ;
#29103 = CARTESIAN_POINT ( 'NONE',  ( -29.00000000000000355, 0.000000000000000000, 4.999999999999999112 ) ) ;
#29104 = CARTESIAN_POINT ( 'NONE',  ( 98.56158271022805195, -38.47369220965149594, 200.8892253048653629 ) ) ;
#29105 = CARTESIAN_POINT ( 'NONE',  ( 13.02890126842911123, 21.69022161494968159, 4.974805862544680046 ) ) ;
#29106 = CARTESIAN_POINT ( 'NONE',  ( 85.05651546852904232, -52.70738422179273641, 5.798279539873188781 ) ) ;
#29107 = DIRECTION ( 'NONE',  ( -1.734723475976807094E-16, -0.000000000000000000, -1.000000000000000000 ) ) ;
#29108 = CARTESIAN_POINT ( 'NONE',  ( 33.14162648300398928, 381.8286340670186405, 24.93812587160989480 ) ) ;
#29109 = DIRECTION ( 'NONE',  ( 0.000000000000000000, 1.000000000000000000, 0.000000000000000000 ) ) ;
#29110 = CIRCLE ( 'NONE', #96282, 4.000000000000000888 ) ;
#29111 = DIRECTION ( 'NONE',  ( -1.000000000000000000, -1.224606353822377258E-16, -0.000000000000000000 ) ) ;
#29112 = CARTESIAN_POINT ( 'NONE',  ( -39.17204790862007968, 459.8623611124606896, 1.900463024343122420 ) ) ;
#29113 = DIRECTION ( 'NONE',  ( 1.000000000000000000, 0.000000000000000000, 0.000000000000000000 ) ) ;
#29114 = ORIENTED_EDGE ( 'NONE', *, *, #23623, .F. ) ;
#29115 = FILL_AREA_STYLE_COLOUR ( '', #44501 ) ;
#29116 = CARTESIAN_POINT ( 'NONE',  ( 16.42257055868354598, 36.46149248629888007, -24.27355254955534036 ) ) ;
#29117 = CARTESIAN_POINT ( 'NONE',  ( -3.293777686966706142, 33.35761369607794791, 5.000000000000000888 ) ) ;
#29118 = ORIENTED_EDGE ( 'NONE', *, *, #38306, .T. ) ;
#29119 = CARTESIAN_POINT ( 'NONE',  ( -25.22202552652619190, 306.3045764116132545, -8.682614143662695128 ) ) ;
#29120 = CIRCLE ( 'NONE', #20578, 0.5000000000000004441 ) ;
#29121 = CARTESIAN_POINT ( 'NONE',  ( -28.62134865195630695, 310.7073307092337586, 11.81453451529568888 ) ) ;
#29122 = CARTESIAN_POINT ( 'NONE',  ( -12.03765877768534942, -4.743370302668000527, -76.84911689414364844 ) ) ;
#29123 = CARTESIAN_POINT ( 'NONE',  ( -5.656854249492379694, -19.43749999999999289, -5.656854249492380582 ) ) ;
#29124 = CARTESIAN_POINT ( 'NONE',  ( 37.81320834215699733, -27.69356383356495854, 44.71441020632808971 ) ) ;
#29125 = EDGE_CURVE ( 'NONE', #79927, #87702, #35633, .T. ) ;
#29126 = DIRECTION ( 'NONE',  ( -1.000000000000000000, -1.224606353822377258E-16, -0.000000000000000000 ) ) ;
#29127 = ORIENTED_EDGE ( 'NONE', *, *, #44168, .F. ) ;
#29128 = CARTESIAN_POINT ( 'NONE',  ( 86.18054470901965658, -21.36750242109700793, 176.9380357467274507 ) ) ;
#29129 = CARTESIAN_POINT ( 'NONE',  ( -38.64320596748726899, 27.44866006653725776, 11.54985041964670067 ) ) ;
#29130 = AXIS2_PLACEMENT_3D ( 'NONE', #54142, #103776, #38024 ) ;
#29131 = DIRECTION ( 'NONE',  ( 0.000000000000000000, 0.000000000000000000, 1.000000000000000000 ) ) ;
#29132 = ORIENTED_EDGE ( 'NONE', *, *, #27802, .F. ) ;
#29133 = CARTESIAN_POINT ( 'NONE',  ( -99.60505029529538490, -52.71012916261938130, 120.4313145599469408 ) ) ;
#29134 = DIRECTION ( 'NONE',  ( 0.000000000000000000, -1.000000000000000000, 0.000000000000000000 ) ) ;
#29135 = CARTESIAN_POINT ( 'NONE',  ( -4.766030446259712505, -5.000000000000002665, -97.32770387339404294 ) ) ;
#29136 = DIRECTION ( 'NONE',  ( 0.000000000000000000, -1.000000000000000000, 0.000000000000000000 ) ) ;
#29137 = CARTESIAN_POINT ( 'NONE',  ( -9.186147765600862769, -22.42665461655586157, -38.54335720488538897 ) ) ;
#29138 =( BOUNDED_CURVE ( )  B_SPLINE_CURVE ( 2, ( #95992, #71687, #56022 ),
 .UNSPECIFIED., .F., .F. ) 
 B_SPLINE_CURVE_WITH_KNOTS ( ( 3, 3 ),
 ( 0.000000000000000000, 1.000000000000000000 ),
 .UNSPECIFIED. ) 
 CURVE ( )  GEOMETRIC_REPRESENTATION_ITEM ( )  RATIONAL_B_SPLINE_CURVE ( ( 1.000000000000000000, 1.857142857142858317, 1.000000000000000000 ) ) 
 REPRESENTATION_ITEM ( '' )  );
#29139 = CARTESIAN_POINT ( 'NONE',  ( 15.03942254395109046, -22.71148339282385820, 35.93912477487155854 ) ) ;
#29140 = CARTESIAN_POINT ( 'NONE',  ( 46.54793763053436351, -28.81014148338916314, 41.79554432402118636 ) ) ;
#29141 = AXIS2_PLACEMENT_3D ( 'NONE', #75343, #43533, #26327 ) ;
#29143 = CARTESIAN_POINT ( 'NONE',  ( -11.65430815032340206, 15.87850340580320641, 9.580969490850751669 ) ) ;
#29142 = LINE ( 'NONE', #104557, #82709 ) ;
#29144 = CARTESIAN_POINT ( 'NONE',  ( 8.557829126397788144, 294.6841484303158154, -5.194105103951514479 ) ) ;
#29145 = CARTESIAN_POINT ( 'NONE',  ( -16.09848981374117471, 43.93711403859757780, -4.279955985616452629 ) ) ;
#29146 = CARTESIAN_POINT ( 'NONE',  ( 38.56934373940381988, 309.6127934295942623, 1.496663477255220531 ) ) ;
#29147 = LINE ( 'NONE', #62017, #49335 ) ;
#29148 = ORIENTED_EDGE ( 'NONE', *, *, #14456, .F. ) ;
#29149 = EDGE_CURVE ( 'NONE', #38179, #45114, #39434, .T. ) ;
#29150 = DIRECTION ( 'NONE',  ( -1.000000000000000000, -0.000000000000000000, -0.000000000000000000 ) ) ;
#29151 = ORIENTED_EDGE ( 'NONE', *, *, #58479, .F. ) ;
#29152 = CARTESIAN_POINT ( 'NONE',  ( -12.39018079436049113, -3.230755885516240156, 20.63706837319177723 ) ) ;
#29153 = SURFACE_STYLE_USAGE ( .BOTH. , #28607 ) ;
#29154 = DIRECTION ( 'NONE',  ( 0.000000000000000000, 0.000000000000000000, 1.000000000000000000 ) ) ;
#29156 = CARTESIAN_POINT ( 'NONE',  ( 6.278603737950535724, -34.58964686943891564, -32.56275994427586795 ) ) ;
#29155 = CARTESIAN_POINT ( 'NONE',  ( 9.221249107921769550, 251.0482137149848256, 3.869340886054255968 ) ) ;
#29157 = ORIENTED_EDGE ( 'NONE', *, *, #41966, .F. ) ;
#29158 = LINE ( 'NONE', #88412, #54790 ) ;
#29159 = CARTESIAN_POINT ( 'NONE',  ( -43.51602118134770336, 463.0217804479698884, 9.924213970829672604 ) ) ;
#29160 = VERTEX_POINT ( 'NONE', #94009 ) ;
#29161 = AXIS2_PLACEMENT_3D ( 'NONE', #1145, #58355, #2221 ) ;
#29162 = CARTESIAN_POINT ( 'NONE',  ( 0.06682554136337871820, 4.993536075455421219, -4.350941807883113022 ) ) ;
#29163 = AXIS2_PLACEMENT_3D ( 'NONE', #41283, #9427, #253 ) ;
#29164 = CARTESIAN_POINT ( 'NONE',  ( -5.833333333333329485, -50.00000000000000000, 103.8776713793258608 ) ) ;
#29165 = CARTESIAN_POINT ( 'NONE',  ( -91.93118328357623170, -60.00000000000001421, 7.837162816498209672 ) ) ;
#29166 = VERTEX_POINT ( 'NONE', #36352 ) ;
#29167 = CARTESIAN_POINT ( 'NONE',  ( -6.362990258380357034, 42.00000000000000711, -58.90232955951056226 ) ) ;
#29168 = CARTESIAN_POINT ( 'NONE',  ( 0.000000000000000000, 23.58303312036771615, 0.000000000000000000 ) ) ;
#29169 = DIRECTION ( 'NONE',  ( -1.000000000000000000, -1.224606353822377258E-16, -0.000000000000000000 ) ) ;
#29170 = CARTESIAN_POINT ( 'NONE',  ( -9.797936955406314041, 26.53328310229516518, -2.012343231877595340 ) ) ;
#29172 = CARTESIAN_POINT ( 'NONE',  ( 0.000000000000000000, -30.00000000000000000, 0.000000000000000000 ) ) ;
#29171 = CARTESIAN_POINT ( 'NONE',  ( -8.000000000000000000, -26.84374999999999289, -3.313708498984762496 ) ) ;
#29173 = CIRCLE ( 'NONE', #94596, 5.000000000000011546 ) ;
#29174 = CARTESIAN_POINT ( 'NONE',  ( -82.83002596087247582, -39.49110685017327427, 168.2621467706148906 ) ) ;
#29175 = VERTEX_POINT ( 'NONE', #43858 ) ;
#29176 = CARTESIAN_POINT ( 'NONE',  ( -37.83989825151947173, 491.6297408768480750, 12.44743998624971049 ) ) ;
#29177 = VERTEX_POINT ( 'NONE', #85943 ) ;
#29178 = ORIENTED_EDGE ( 'NONE', *, *, #90736, .F. ) ;
#29179 = CARTESIAN_POINT ( 'NONE',  ( 3.328192429499065685, -5.000000000000000000, 16.34245136408155830 ) ) ;
#29180 = DIRECTION ( 'NONE',  ( -1.000000000000000000, -1.224606353822377258E-16, -0.000000000000000000 ) ) ;
#29181 = ORIENTED_EDGE ( 'NONE', *, *, #5026, .T. ) ;
#29182 = CARTESIAN_POINT ( 'NONE',  ( -43.21667697146752118, 434.4554196591588493, 16.17972000939132116 ) ) ;
#29183 = FACE_OUTER_BOUND ( 'NONE', #5637, .T. ) ;
#29184 = CARTESIAN_POINT ( 'NONE',  ( -98.27571109168336250, -57.67134109913899209, 58.06786128689789450 ) ) ;
#29185 = CARTESIAN_POINT ( 'NONE',  ( 32.94330508143927716, 6.123233995736770227E-16, -5.000000000000002665 ) ) ;
#29186 = AXIS2_PLACEMENT_3D ( 'NONE', #82831, #34317, #26764 ) ;
#29187 = EDGE_CURVE ( 'NONE', #80223, #10937, #49355, .T. ) ;
#29188 = CARTESIAN_POINT ( 'NONE',  ( -3.935526831180291373E-15, 7.124194613927623543, 3.660532965668822136 ) ) ;
#29189 = CARTESIAN_POINT ( 'NONE',  ( 9.609486011791450011, 8.908497650347621644, 0.000000000000000000 ) ) ;
#29190 = CARTESIAN_POINT ( 'NONE',  ( -13.48753244636324489, -52.95794048676148691, 23.24642415514733429 ) ) ;
#29191 = CARTESIAN_POINT ( 'NONE',  ( -17.39344025253030424, 36.29830519803331867, -24.14278306258530193 ) ) ;
#29192 = CIRCLE ( 'NONE', #51530, 4.172000000000009479 ) ;
#29193 = CARTESIAN_POINT ( 'NONE',  ( 61.70037527280209844, -30.00000000000006040, -32.45262418874342103 ) ) ;
#29194 = ADVANCED_FACE ( 'NONE', ( #3940, #19101 ), #92400, .T. ) ;
#29195 = CARTESIAN_POINT ( 'NONE',  ( -67.93243969554674777, -60.00000000000000711, 143.1807200622937728 ) ) ;
#29196 = CARTESIAN_POINT ( 'NONE',  ( -54.05961884913804738, -56.85113118587781145, 65.25060302166593829 ) ) ;
#29197 = EDGE_LOOP ( 'NONE', ( #32567, #92417, #37723 ) ) ;
#29198 = CARTESIAN_POINT ( 'NONE',  ( 6.481161585458342422, 16.00528638454814256, -2.652050489361057029 ) ) ;
#29199 = EDGE_LOOP ( 'NONE', ( #53468, #69596, #79367, #80091, #41635, #34774 ) ) ;
#29200 = CARTESIAN_POINT ( 'NONE',  ( -101.4140262225946003, -52.72498359022472414, 192.9040562268387191 ) ) ;
#29201 = CARTESIAN_POINT ( 'NONE',  ( -30.93190593211504691, 14.41219003788192055, -40.70233947780400996 ) ) ;
#29202 = VECTOR ( 'NONE', #87479, 1000.000000000000000 ) ;
#29203 = ORIENTED_EDGE ( 'NONE', *, *, #69888, .F. ) ;
#29204 = CARTESIAN_POINT ( 'NONE',  ( 19.25558504890851097, 49.82459671548976843, 61.44364156091821627 ) ) ;
#29205 = CARTESIAN_POINT ( 'NONE',  ( 0.000000000000000000, -100.0000000000000000, 0.000000000000000000 ) ) ;
#29206 = CARTESIAN_POINT ( 'NONE',  ( -7.188101187500001821, -14.37500000204838635, -2.977408999572651371 ) ) ;
#29207 = DIRECTION ( 'NONE',  ( -0.000000000000000000, -0.000000000000000000, 1.000000000000000000 ) ) ;
#29209 = EDGE_CURVE ( 'NONE', #65228, #36313, #44599, .T. ) ;
#29208 = FILL_AREA_STYLE ('',( #70677 ) ) ;
#29210 = CARTESIAN_POINT ( 'NONE',  ( 6.928203230275509661, -84.73473843067414180, 4.000000000000001776 ) ) ;
#29211 = CARTESIAN_POINT ( 'NONE',  ( 56.86967849623623295, -29.99999999999999645, 59.52404653438935611 ) ) ;
#29212 = EDGE_CURVE ( 'NONE', #4725, #36986, #76657, .T. ) ;
#29213 = CYLINDRICAL_SURFACE ( 'NONE', #24882, 5.000000000000002665 ) ;
#29214 = CARTESIAN_POINT ( 'NONE',  ( -8.000000000000000000, -15.03125000409677092, -3.313708498984762496 ) ) ;
#29215 = DIRECTION ( 'NONE',  ( 0.000000000000000000, -1.000000000000000000, 0.000000000000000000 ) ) ;
#29216 = CARTESIAN_POINT ( 'NONE',  ( -27.49130160687422375, -29.05394088803144115, 30.53830709630566531 ) ) ;
#29217 = VERTEX_POINT ( 'NONE', #63243 ) ;
#29218 = CARTESIAN_POINT ( 'NONE',  ( 48.06845630413710069, -36.06226588698234536, 46.66767315606317368 ) ) ;
#29219 = CARTESIAN_POINT ( 'NONE',  ( -0.7709651574482678793, 13.06628101731643810, 49.51182408176356375 ) ) ;
#29220 = MECHANICAL_DESIGN_GEOMETRIC_PRESENTATION_REPRESENTATION (  '', ( #34359 ), #42948 ) ;
#29221 = LINE ( 'NONE', #79827, #47888 ) ;
#29222 = CARTESIAN_POINT ( 'NONE',  ( -89.30654270732652833, -38.52662107162988292, 200.3831435256876432 ) ) ;
#29223 = ORIENTED_EDGE ( 'NONE', *, *, #17884, .F. ) ;
#29224 = CARTESIAN_POINT ( 'NONE',  ( 90.39058703242112358, -38.40011783027308212, -14.99676332985419691 ) ) ;
#29225 = CARTESIAN_POINT ( 'NONE',  ( -48.59958381656765170, 10.21806572665720658, -14.48686862603874559 ) ) ;
#29226 = DIRECTION ( 'NONE',  ( 0.000000000000000000, 1.000000000000000000, 0.000000000000000000 ) ) ;
#29227 = CARTESIAN_POINT ( 'NONE',  ( 6.035608966186244650, 41.34018742956621395, -70.92167700592624158 ) ) ;
#29228 = COLOUR_RGB ( '', 0.31764706, 0.68627451, 0.89019608) ;
#29229 = CARTESIAN_POINT ( 'NONE',  ( -33.17861982450024527, 435.0122478756496207, 15.11176251742224608 ) ) ;
#29230 = CARTESIAN_POINT ( 'NONE',  ( 0.2573354458087866448, -6.889406814520517841, 1.067197363239228203 ) ) ;
#29231 = CARTESIAN_POINT ( 'NONE',  ( 112.1662010274523453, -59.99999999999999289, 176.3906357321001508 ) ) ;
#29232 = CARTESIAN_POINT ( 'NONE',  ( -8.000086790516059310, -69.00017358106005361, 0.2639471549312808474 ) ) ;
#29233 = EDGE_LOOP ( 'NONE', ( #49849, #88941, #33384, #3174, #47527, #45622 ) ) ;
#29234 = CARTESIAN_POINT ( 'NONE',  ( 7.344133061198930612, 32.44494392680575601, 3.176267128233873471 ) ) ;
#29235 = ORIENTED_EDGE ( 'NONE', *, *, #51268, .T. ) ;
#29237 = CARTESIAN_POINT ( 'NONE',  ( 0.000000000000000000, -30.00000000000000000, 8.000000000000000000 ) ) ;
#29236 = CARTESIAN_POINT ( 'NONE',  ( -91.06811619128255586, -38.35144331576948673, 1.256099165720845345 ) ) ;
#29238 = CARTESIAN_POINT ( 'NONE',  ( 12.48484554125298907, -3.563252358774177342, -13.68093487574958012 ) ) ;
#29239 = LINE ( 'NONE', #48006, #38097 ) ;
#29240 =( LENGTH_UNIT ( ) NAMED_UNIT ( * ) SI_UNIT ( .MILLI., .METRE. ) );
#29241 = CARTESIAN_POINT ( 'NONE',  ( -2.977408999572654480, -15.50000000204838635, 7.188101187499999156 ) ) ;
#29242 = CARTESIAN_POINT ( 'NONE',  ( 1.308996937483426937, -5.000000000000002665, -75.00000000000001421 ) ) ;
#29243 = MECHANICAL_DESIGN_GEOMETRIC_PRESENTATION_REPRESENTATION (  '', ( #20636 ), #56734 ) ;
#29244 = EDGE_CURVE ( 'NONE', #6335, #47934, #88570, .T. ) ;
#29245 = DIRECTION ( 'NONE',  ( 0.000000000000000000, 1.000000000000000000, 0.000000000000000000 ) ) ;
#29247 = ORIENTED_EDGE ( 'NONE', *, *, #14700, .F. ) ;
#29246 = DIRECTION ( 'NONE',  ( 0.000000000000000000, 0.000000000000000000, 1.000000000000000000 ) ) ;
#29248 = CARTESIAN_POINT ( 'NONE',  ( 85.74730987966626117, -18.52705124433025219, 162.5160542404693444 ) ) ;
#29249 = CARTESIAN_POINT ( 'NONE',  ( 0.000000000000000000, -46.00000000000000000, 122.0000000000000000 ) ) ;
#29250 = CARTESIAN_POINT ( 'NONE',  ( 46.85000000000000142, 0.000000000000000000, 4.171999999999999709 ) ) ;
#29251 = ORIENTED_EDGE ( 'NONE', *, *, #54806, .F. ) ;
#29252 = CARTESIAN_POINT ( 'NONE',  ( -36.89065814680163413, 342.5445545919167785, -0.5098802229861002511 ) ) ;
#29253 = CARTESIAN_POINT ( 'NONE',  ( -47.14503195514129885, 18.54431490492956769, 14.71570748879569202 ) ) ;
#29254 = CARTESIAN_POINT ( 'NONE',  ( 2.133938722758562001, 6.273523403446319868, -0.09463688534106554084 ) ) ;
#29255 = CARTESIAN_POINT ( 'NONE',  ( 5.290067270632161645, -1.200000000000000030E-05, -7.281152949374595451 ) ) ;
#29256 = CARTESIAN_POINT ( 'NONE',  ( 17.72007123370824644, 43.32272278278890809, 4.751713957287425849 ) ) ;
#29257 = B_SPLINE_SURFACE_WITH_KNOTS ( 'NONE', 3, 3, ( 
 ( #35924, #42909, #51519, #74721, #68795, #58571, #1895, #805, #66650, #67194 ),
 ( #83356, #34849, #67718, #35383, #58011, #68250, #90936, #8930, #99532, #91468 ),
 ( #17584, #86583, #94115, #69846, #36458, #45578, #13179, #20818, #53652, #12123 ),
 ( #53131, #78987, #28349, #5111, #37515, #38042, #61229, #70903, #103793, #78459 ),
 ( #102742, #4579, #45052, #27836, #70378, #60707, #86048, #20280, #77937, #21323 ),
 ( #4045, #12647, #36978, #93590, #61776, #103273, #29423, #29936, #28903, #94673 ),
 ( #62300, #95192, #54159, #87102, #46104, #62821, #19742, #52580, #85504, #11585 ),
 ( #44512, #77401, #3517, #69324, #102204, #25524, #65413, #90216, #56769, #89693 ) ),
 .UNSPECIFIED., .F., .F., .F.,
 ( 4, 2, 2, 4 ),
 ( 4, 2, 2, 2, 4 ),
 ( 0.000000000000000000, 0.2500000000000000000, 0.5000000000000000000, 1.000000000000000000 ),
 ( 0.000000000000000000, 0.1250000000000000000, 0.2500000000000000000, 0.5000000000000000000, 1.000000000000000000 ),
 .UNSPECIFIED. ) ;
#29258 = ORIENTED_EDGE ( 'NONE', *, *, #1653, .T. ) ;
#29259 = AXIS2_PLACEMENT_3D ( 'NONE', #61461, #79743, #55449 ) ;
#29260 = CARTESIAN_POINT ( 'NONE',  ( -72.75733770493380348, -30.00000000000000355, -19.25270559974459061 ) ) ;
#29261 = CARTESIAN_POINT ( 'NONE',  ( -5.000000000000000888, -48.53184174324966449, 2.645245988191155639 ) ) ;
#29262 = DIRECTION ( 'NONE',  ( 1.000000000000000000, 0.000000000000000000, -1.224646799147353207E-16 ) ) ;
#29264 = DIRECTION ( 'NONE',  ( -1.000000000000000000, -1.224606353822377258E-16, -0.000000000000000000 ) ) ;
#29263 = DIRECTION ( 'NONE',  ( 0.000000000000000000, 0.000000000000000000, 1.000000000000000000 ) ) ;
#29265 = AXIS2_PLACEMENT_3D ( 'NONE', #28933, #19250, #52077 ) ;
#29266 = CARTESIAN_POINT ( 'NONE',  ( -7.188101187500001821, -20.00000000204838813, -2.977408999572651371 ) ) ;
#29267 = CARTESIAN_POINT ( 'NONE',  ( 13.31041225640290548, 294.5490349693251346, -2.064332924270082970 ) ) ;
#29268 = CARTESIAN_POINT ( 'NONE',  ( 0.000000000000000000, -4.000000000000003553, 112.0000000000000000 ) ) ;
#29269 = EDGE_CURVE ( 'NONE', #99841, #16577, #16648, .T. ) ;
#29270 = ITEM_DEFINED_TRANSFORMATION ( 'NONE', 'NONE', #23159,  #10728 ) ;
#29271 = EDGE_LOOP ( 'NONE', ( #60334, #68463, #105247, #83621 ) ) ;
#29272 = CARTESIAN_POINT ( 'NONE',  ( -37.02109538778312725, 490.9589098422684401, 12.45652899166105243 ) ) ;
#29273 = DIRECTION ( 'NONE',  ( 0.9921085174016837094, -0.1089071661329407970, 0.06212824529894127312 ) ) ;
#29274 = CARTESIAN_POINT ( 'NONE',  ( -5.155570458487308549, 6.081290275064629824, -4.999999999999999112 ) ) ;
#29275 = ADVANCED_FACE ( 'NONE', ( #79930 ), #3897, .F. ) ;
#29276 = DIRECTION ( 'NONE',  ( 0.000000000000000000, 1.000000000000000000, 0.000000000000000000 ) ) ;
#29277 = VERTEX_POINT ( 'NONE', #96136 ) ;
#29278 = DIRECTION ( 'NONE',  ( -3.673940397442057649E-17, 0.000000000000000000, -1.000000000000000000 ) ) ;
#29279 = CARTESIAN_POINT ( 'NONE',  ( -33.72687874427343502, 464.0440927327247209, 18.49751758948643499 ) ) ;
#29280 = ORIENTED_EDGE ( 'NONE', *, *, #69941, .F. ) ;
#29281 = MECHANICAL_DESIGN_GEOMETRIC_PRESENTATION_REPRESENTATION (  '', ( #5152 ), #65426 ) ;
#29282 = CARTESIAN_POINT ( 'NONE',  ( 104.0908829527487711, 1.030564683017419500E-14, 0.000000000000000000 ) ) ;
#29283 = LINE ( 'NONE', #62165, #24302 ) ;
#29284 = LINE ( 'NONE', #92365, #23731 ) ;
#29285 = CARTESIAN_POINT ( 'NONE',  ( -94.64169479211049918, -60.00000000000000000, 202.5669859057673534 ) ) ;
#29286 = SURFACE_STYLE_FILL_AREA ( #6011 ) ;
#29287 = CARTESIAN_POINT ( 'NONE',  ( 6.683837171061802529, 3.955946848495962787, 6.851900933636986935 ) ) ;
#29288 = FACE_OUTER_BOUND ( 'NONE', #43104, .T. ) ;
#29289 = CARTESIAN_POINT ( 'NONE',  ( 17.39562436205969931, 34.16980401269882606, -24.14171231524191086 ) ) ;
#29290 = CARTESIAN_POINT ( 'NONE',  ( -86.30021902774615228, -18.16438055758039027, 170.9070947866538575 ) ) ;
#29291 = EDGE_CURVE ( 'NONE', #52539, #9067, #30463, .T. ) ;
#29292 = CARTESIAN_POINT ( 'NONE',  ( 52.56483885390523625, 40.83906611471594061, -38.23529411764706509 ) ) ;
#29293 = ORIENTED_EDGE ( 'NONE', *, *, #73248, .T. ) ;
#29294 = FILL_AREA_STYLE ('',( #37384 ) ) ;
#29295 = CARTESIAN_POINT ( 'NONE',  ( 1.000000000000000000, -63.14890303518984638, 9.346194641690638960 ) ) ;
#29296 = CARTESIAN_POINT ( 'NONE',  ( -86.97225581348263290, -60.15082631087481957, 29.24283001683475192 ) ) ;
#29297 = DIRECTION ( 'NONE',  ( -1.000000000000000000, -1.224606353822377258E-16, -0.000000000000000000 ) ) ;
#29298 = CARTESIAN_POINT ( 'NONE',  ( 8.830611806797369567, 133.7952729321875438, 6.141763964344532733E-13 ) ) ;
#29299 = DIRECTION ( 'NONE',  ( 0.8191520442889884679, 0.000000000000000000, 0.5735764363510509334 ) ) ;
#29300 = CARTESIAN_POINT ( 'NONE',  ( 33.52312678243841759, 18.64316884716171785, -19.32152200345659665 ) ) ;
#29301 = CARTESIAN_POINT ( 'NONE',  ( 97.80297141475710987, -14.21045842199415432, 197.6895799465713708 ) ) ;
#29302 = CARTESIAN_POINT ( 'NONE',  ( 9.830769230769229594, -4.171999999999999709, 0.000000000000000000 ) ) ;
#29303 = CARTESIAN_POINT ( 'NONE',  ( -97.09821068641753072, -30.00000000000001776, 79.69957433219180132 ) ) ;
#29304 = CARTESIAN_POINT ( 'NONE',  ( -63.47421256789260724, -42.96224801778237889, 83.53665870048976672 ) ) ;
#29305 = ORIENTED_EDGE ( 'NONE', *, *, #1825, .F. ) ;
#29306 = CARTESIAN_POINT ( 'NONE',  ( 107.3649583438541271, -29.99999999999998579, 190.7484263893222192 ) ) ;
#29307 = CARTESIAN_POINT ( 'NONE',  ( -64.12661792344870548, 39.42592270507808649, -11.02918813174155588 ) ) ;
#29308 = CARTESIAN_POINT ( 'NONE',  ( 53.27405869684046991, -60.00000000005845635, 87.46234259303579961 ) ) ;
#29309 = VERTEX_POINT ( 'NONE', #104208 ) ;
#29310 = CARTESIAN_POINT ( 'NONE',  ( -33.89250494191498575, 463.6575930728432127, 6.993601543837932866 ) ) ;
#29311 = CARTESIAN_POINT ( 'NONE',  ( 5.082755093536324154, -18.21875000204838457, 5.082755093536326818 ) ) ;
#29312 = AXIS2_PLACEMENT_3D ( 'NONE', #97577, #23743, #81928 ) ;
#29313 = VERTEX_POINT ( 'NONE', #71838 ) ;
#29314 = CARTESIAN_POINT ( 'NONE',  ( 3.433097715925975013, -49.17502020225290948, 103.8029788753759703 ) ) ;
#29315 = ORIENTED_EDGE ( 'NONE', *, *, #63234, .F. ) ;
#29316 = CARTESIAN_POINT ( 'NONE',  ( 1.966965783804971668, 41.99999999999999289, -67.70628254661242806 ) ) ;
#29317 = CARTESIAN_POINT ( 'NONE',  ( -92.06659163830985904, -60.00000000000001421, -13.68159610222980760 ) ) ;
#29318 = CARTESIAN_POINT ( 'NONE',  ( -23.21751746555168339, 27.38103382803512176, 33.20617127781681432 ) ) ;
#29319 = CARTESIAN_POINT ( 'NONE',  ( -7.188101187500000044, -32.28125000204838813, -8.802885111219163269E-16 ) ) ;
#29320 = DIRECTION ( 'NONE',  ( -0.000000000000000000, -0.000000000000000000, 1.000000000000000000 ) ) ;
#29321 = ADVANCED_FACE ( 'NONE', ( #89102 ), #21926, .F. ) ;
#29322 = CARTESIAN_POINT ( 'NONE',  ( 3.301565691951512616, -4.285714285714295357, 25.05982991920904013 ) ) ;
#29323 = AXIS2_PLACEMENT_3D ( 'NONE', #42417, #65101, #97998 ) ;
#29324 = DIRECTION ( 'NONE',  ( 1.000000000000000000, 0.000000000000000000, -1.224646799147353207E-16 ) ) ;
#29325 = EDGE_CURVE ( 'NONE', #83521, #8349, #68403, .T. ) ;
#29326 = DIRECTION ( 'NONE',  ( -1.000000000000000000, -1.224606353822377258E-16, -0.000000000000000000 ) ) ;
#29327 = DIRECTION ( 'NONE',  ( 0.000000000000000000, 1.000000000000000000, 0.000000000000000000 ) ) ;
#29328 = AXIS2_PLACEMENT_3D ( 'NONE', #79484, #29899, #30429 ) ;
#29329 = ORIENTED_EDGE ( 'NONE', *, *, #40738, .F. ) ;
#29330 = CYLINDRICAL_SURFACE ( 'NONE', #45373, 4.000000000000000888 ) ;
#29331 = CARTESIAN_POINT ( 'NONE',  ( -16.51907061138353683, 42.00139744608745218, -87.79003255390435356 ) ) ;
#29332 = CARTESIAN_POINT ( 'NONE',  ( 32.59170211760999081, -29.08667747155562822, 32.21612061202412036 ) ) ;
#29333 = CARTESIAN_POINT ( 'NONE',  ( 3.301606509414339641, -4.285714285714286476, -25.22241582816893413 ) ) ;
#29334 = EDGE_CURVE ( 'NONE', #18823, #34787, #103596, .T. ) ;
#29335 = VERTEX_POINT ( 'NONE', #569 ) ;
#29336 = CARTESIAN_POINT ( 'NONE',  ( 34.16218064238238128, 484.1154536690855821, 0.7177099017922428104 ) ) ;
#29337 = VECTOR ( 'NONE', #9233, 1000.000000000000000 ) ;
#29338 = B_SPLINE_CURVE_WITH_KNOTS ( 'NONE', 3,
 ( #70348, #47111, #62274, #104836, #94089, #53099, #86022, #87072, #12092, #48170, #9164, #1601, #56791, #64903, #76036, #66901, #31504, #67438, #43154, #26473, #32022, #15285, #14739, #89716, #105364, #97785, #42608, #64385, #97261, #34028, #55717, #80539, #18365, #58815 ),
 .UNSPECIFIED., .F., .F.,
 ( 4, 2, 2, 2, 2, 2, 2, 2, 2, 2, 2, 2, 2, 2, 2, 2, 4 ),
 ( 1.422579022190208801E-17, 0.0007899309203816185692, 0.001579861840763223044, 0.002369792761144827193, 0.003159723681526431776, 0.003949654601908035925, 0.004739585522289639641, 0.005529516442671244224, 0.006319447363052848807, 0.007109378283434453390, 0.007899309203816057973, 0.008689240124197661688, 0.009479171044579265404, 0.01026910196496087085, 0.01105903288534247457, 0.01184896380572408002, 0.01263889472610568374 ),
 .UNSPECIFIED. ) ;
#29340 = CARTESIAN_POINT ( 'NONE',  ( -22.18906107735381283, 305.1406206946286943, -9.938500898754245583 ) ) ;
#29339 = CARTESIAN_POINT ( 'NONE',  ( 6.837824896291513355, -3.947820044545448326, -6.564402953523719830 ) ) ;
#29341 = DIRECTION ( 'NONE',  ( 0.000000000000000000, -1.000000000000000000, 0.000000000000000000 ) ) ;
#29342 = CARTESIAN_POINT ( 'NONE',  ( 11.08349330513380515, 1.593028355512270962E-15, 0.000000000000000000 ) ) ;
#29343 = CARTESIAN_POINT ( 'NONE',  ( -46.00000000000000000, 500.0000000000002274, 0.000000000000000000 ) ) ;
#29344 = CARTESIAN_POINT ( 'NONE',  ( -39.82092066244458550, 436.5808519682735209, 5.503544575421002172 ) ) ;
#29345 = CARTESIAN_POINT ( 'NONE',  ( -49.03408319953958738, 14.13974658789107330, -14.85990013744726923 ) ) ;
#29346 = ORIENTED_EDGE ( 'NONE', *, *, #97905, .F. ) ;
#29347 = AXIS2_PLACEMENT_3D ( 'NONE', #31540, #97292, #48205 ) ;
#29348 = CARTESIAN_POINT ( 'NONE',  ( 92.56983564317958724, -60.00000000000000000, -2.305466784945364278 ) ) ;
#29349 = CARTESIAN_POINT ( 'NONE',  ( 38.09999999999999432, 1.533819458162526451E-15, 0.000000000000000000 ) ) ;
#29350 = CARTESIAN_POINT ( 'NONE',  ( -5.563665798473262036, 41.08730335088894492, -70.97074924948610430 ) ) ;
#29351 = CARTESIAN_POINT ( 'NONE',  ( 21.84999999999999787, 3.309500000000003439, 4.052968581778167743E-16 ) ) ;
#29352 = ORIENTED_EDGE ( 'NONE', *, *, #60099, .T. ) ;
#29353 = CARTESIAN_POINT ( 'NONE',  ( -83.51106636389977211, -30.00000000000859757, 196.0047889519032935 ) ) ;
#29354 = VERTEX_POINT ( 'NONE', #8702 ) ;
#29355 = DIRECTION ( 'NONE',  ( -0.000000000000000000, 1.000000000000000000, -0.000000000000000000 ) ) ;
#29356 = SURFACE_STYLE_USAGE ( .BOTH. , #102138 ) ;
#29357 = DIRECTION ( 'NONE',  ( 0.000000000000000000, 0.000000000000000000, 1.000000000000000000 ) ) ;
#29358 = CARTESIAN_POINT ( 'NONE',  ( 15.68557340203072137, 21.69024387810497956, 4.767881275881356906 ) ) ;
#29359 = CARTESIAN_POINT ( 'NONE',  ( 84.58342993391340769, -60.18021989816856632, -16.69648072670474193 ) ) ;
#29360 = CARTESIAN_POINT ( 'NONE',  ( -2.977408999572654480, -32.00000000204838813, 7.188101187499999156 ) ) ;
#29361 = AXIS2_PLACEMENT_3D ( 'NONE', #93566, #21823, #87596 ) ;
#29362 = CARTESIAN_POINT ( 'NONE',  ( -13.00000000000003730, -10.00000000000000888, 0.000000000000000000 ) ) ;
#29363 = CARTESIAN_POINT ( 'NONE',  ( 9.721687949930782224, 46.20860120156268636, -13.03939565591218397 ) ) ;
#29364 = CARTESIAN_POINT ( 'NONE',  ( 7.500000000000000000, 4.330127018922189208, -10.00000000000000000 ) ) ;
#29365 = ORIENTED_EDGE ( 'NONE', *, *, #258, .F. ) ;
#29366 = EDGE_CURVE ( 'NONE', #33682, #104233, #54661, .T. ) ;
#29368 = ORIENTED_EDGE ( 'NONE', *, *, #46650, .F. ) ;
#29367 =( LENGTH_UNIT ( ) NAMED_UNIT ( * ) SI_UNIT ( .MILLI., .METRE. ) );
#29369 = CARTESIAN_POINT ( 'NONE',  ( 77.57230420934776305, -49.90228353259792726, 141.6236765526268186 ) ) ;
#29370 = EDGE_CURVE ( 'NONE', #92586, #89220, #7622, .T. ) ;
#29371 = ORIENTED_EDGE ( 'NONE', *, *, #54216, .F. ) ;
#29372 = CARTESIAN_POINT ( 'NONE',  ( -12.50000000000000711, 39.61136555405652615, -64.51031429804609729 ) ) ;
#29373 = CARTESIAN_POINT ( 'NONE',  ( 7.188101187500000933, -16.06250000204838457, -2.977408999572650483 ) ) ;
#29374 = CARTESIAN_POINT ( 'NONE',  ( -76.05665976993959987, -57.54410268428485153, 193.2876952671887523 ) ) ;
#29375 = EDGE_CURVE ( 'NONE', #58207, #68198, #58872, .T. ) ;
#29376 = ADVANCED_BREP_SHAPE_REPRESENTATION ( '', ( #90230, #10728 ), #7340 ) ;
#29377 = ORIENTED_EDGE ( 'NONE', *, *, #23686, .F. ) ;
#29378 = AXIS2_PLACEMENT_3D ( 'NONE', #15086, #63125, #12956 ) ;
#29379 = SHAPE_REPRESENTATION_RELATIONSHIP ( 'NONE' , 'NONE' ,  #22667, #38340 ) ;
#29380 = B_SPLINE_CURVE_WITH_KNOTS ( 'NONE', 3,
 ( #104853, #78976, #87088, #38030 ),
 .UNSPECIFIED., .F., .F.,
 ( 4, 4 ),
 ( 6.651595791536764171E-17, 0.003677212860670132834 ),
 .UNSPECIFIED. ) ;
#29381 = CARTESIAN_POINT ( 'NONE',  ( 4.086350204929704688, 13.71221235928050497, 5.000000000000000888 ) ) ;
#29382 = CIRCLE ( 'NONE', #39680, 2.000000000000000000 ) ;
#29383 = CARTESIAN_POINT ( 'NONE',  ( 6.933421894041627453, 41.67527100805288853, -59.13217572147580370 ) ) ;
#29384 = DIRECTION ( 'NONE',  ( 0.000000000000000000, -1.000000000000000000, 0.000000000000000000 ) ) ;
#29385 = CARTESIAN_POINT ( 'NONE',  ( 8.000000000000000000, -15.59375000409677270, -3.313708498984761608 ) ) ;
#29386 = CARTESIAN_POINT ( 'NONE',  ( -53.08935917470201815, -30.00000000000000000, 52.21147893555080799 ) ) ;
#29387 = CARTESIAN_POINT ( 'NONE',  ( 9.999999999999996447, 15.00000000000000000, 4.582575694955847823 ) ) ;
#29388 = CARTESIAN_POINT ( 'NONE',  ( 0.000000000000000000, 32.68727484027578356, 0.000000000000000000 ) ) ;
#29389 = CARTESIAN_POINT ( 'NONE',  ( 7.500000000000001776, -7.939616441372559841, -16.39477006944641957 ) ) ;
#29390 = CARTESIAN_POINT ( 'NONE',  ( 4.062953383280827779, 52.05749732319144130, 6.990574348803606064 ) ) ;
#29391 = PRODUCT_CONTEXT ( 'NONE', #12143, 'mechanical' ) ;
#29392 = CARTESIAN_POINT ( 'NONE',  ( 38.17827875822268879, 27.65674091414286195, 11.10456740074647897 ) ) ;
#29393 = ORIENTED_EDGE ( 'NONE', *, *, #26635, .T. ) ;
#29394 = CARTESIAN_POINT ( 'NONE',  ( -3.559384062307034302, -53.17517428501233212, 40.54544626083967529 ) ) ;
#29395 = CARTESIAN_POINT ( 'NONE',  ( 16.08349330513380337, -3.851859888774471706E-31, 4.000000000000001776 ) ) ;
#29396 = CARTESIAN_POINT ( 'NONE',  ( -3.585543761590458178, 16.06066171126383324, -6.013148396082499403 ) ) ;
#29397 = CIRCLE ( 'NONE', #39694, 1.000000000000000000 ) ;
#29398 = CARTESIAN_POINT ( 'NONE',  ( -26.58951646937336122, -22.83209710930301384, -37.42561714443979781 ) ) ;
#29399 = CARTESIAN_POINT ( 'NONE',  ( -82.13850053252956229, -30.00000000000000000, 146.8543398922747372 ) ) ;
#29400 = ADVANCED_FACE ( 'NONE', ( #49692 ), #44305, .T. ) ;
#29401 = CARTESIAN_POINT ( 'NONE',  ( 7.500000000000007105, 42.00000000000000711, -65.90297133634214788 ) ) ;
#29402 = ORIENTED_EDGE ( 'NONE', *, *, #65588, .T. ) ;
#29403 = AXIS2_PLACEMENT_3D ( 'NONE', #102981, #106678, #57059 ) ;
#29404 = DIRECTION ( 'NONE',  ( -1.000000000000000000, -1.224606353822377258E-16, -0.000000000000000000 ) ) ;
#29405 = CARTESIAN_POINT ( 'NONE',  ( 74.07983334089789196, -57.61003258331666643, 187.3778442680205387 ) ) ;
#29406 = DIRECTION ( 'NONE',  ( 0.2021170706129989947, -0.9793613683246955581, 0.000000000000000000 ) ) ;
#29407 = EDGE_CURVE ( 'NONE', #104315, #71046, #46073, .T. ) ;
#29409 = CARTESIAN_POINT ( 'NONE',  ( -1.098735407080257076, -7.248058225760418694, -6.326622577870835151 ) ) ;
#29408 = CIRCLE ( 'NONE', #77572, 4.000000000000001776 ) ;
#29410 = EDGE_CURVE ( 'NONE', #44580, #103542, #65007, .T. ) ;
#29411 = DIRECTION ( 'NONE',  ( 0.000000000000000000, -1.000000000000000000, 0.000000000000000000 ) ) ;
#29412 = DIRECTION ( 'NONE',  ( -0.5735764363510497121, 0.8191520442889892450, 1.003171929053521665E-16 ) ) ;
#29413 = CARTESIAN_POINT ( 'NONE',  ( -65.49076136059264286, -60.00000000000000711, 120.3024543388731047 ) ) ;
#29414 = ADVANCED_FACE ( 'NONE', ( #26010 ), #1214, .T. ) ;
#29415 = DIRECTION ( 'NONE',  ( -1.000000000000000000, -1.224606353822377258E-16, -0.000000000000000000 ) ) ;
#29416 = DIRECTION ( 'NONE',  ( 0.000000000000000000, -0.5000000000000008882, 0.8660254037844382635 ) ) ;
#29417 = AXIS2_PLACEMENT_3D ( 'NONE', #73275, #96524, #81366 ) ;
#29418 = CARTESIAN_POINT ( 'NONE',  ( -64.32759900504490247, 48.00000000000000000, -11.06576400629244361 ) ) ;
#29419 = CARTESIAN_POINT ( 'NONE',  ( -86.32942810031956071, -21.03686018850741846, 180.4869550100015942 ) ) ;
#29420 = VERTEX_POINT ( 'NONE', #64823 ) ;
#29421 = CARTESIAN_POINT ( 'NONE',  ( 36.69625031493811917, 379.3716818342556394, 5.006538804195920456 ) ) ;
#29422 = CARTESIAN_POINT ( 'NONE',  ( -14.07141259107696918, 41.78883758875669230, -79.52223649356207602 ) ) ;
#29423 = CARTESIAN_POINT ( 'NONE',  ( -6.364223809941345067, 41.95991738832010043, -59.61869671383132641 ) ) ;
#29424 = CARTESIAN_POINT ( 'NONE',  ( 37.51625577699761038, 491.7333577044556705, 12.51656167145575083 ) ) ;
#29425 = CARTESIAN_POINT ( 'NONE',  ( 12.12955763321374114, -4.669738190590866367, -76.82128316853251704 ) ) ;
#29426 = CARTESIAN_POINT ( 'NONE',  ( -32.01402575875847845, 314.0648241496062951, -7.572118188761770341 ) ) ;
#29427 = DIRECTION ( 'NONE',  ( 0.5735764363510442720, -0.8191520442889930198, 1.003171929053526349E-16 ) ) ;
#29428 = DIRECTION ( 'NONE',  ( 0.000000000000000000, -1.000000000000000000, 0.000000000000000000 ) ) ;
#29429 = B_SPLINE_CURVE_WITH_KNOTS ( 'NONE', 3,
 ( #21180, #20667, #95045, #70747 ),
 .UNSPECIFIED., .F., .F.,
 ( 4, 4 ),
 ( 1.486235917163331928E-15, 0.001704530934783209063 ),
 .UNSPECIFIED. ) ;
#29430 = CARTESIAN_POINT ( 'NONE',  ( 18.86650669486618881, 1.474610560812782335E-15, 0.000000000000000000 ) ) ;
#29431 = ORIENTED_EDGE ( 'NONE', *, *, #10125, .T. ) ;
#29432 = VECTOR ( 'NONE', #81995, 1000.000000000000000 ) ;
#29433 = CARTESIAN_POINT ( 'NONE',  ( 17.61650669486618881, 1.474610560812782335E-15, 0.000000000000000000 ) ) ;
#29434 = CARTESIAN_POINT ( 'NONE',  ( 10.14382783504288632, 15.68598017974148107, 10.24918285280354624 ) ) ;
#29435 = CARTESIAN_POINT ( 'NONE',  ( -21.65942590380950605, 4.828984019150144164E-12, 5.820808985950977288 ) ) ;
#29436 =( NAMED_UNIT ( * ) SI_UNIT ( $, .STERADIAN. ) SOLID_ANGLE_UNIT ( ) );
#29437 = CARTESIAN_POINT ( 'NONE',  ( 108.9225596800844897, -59.99999999999995737, 119.6931403564588123 ) ) ;
#29438 = AXIS2_PLACEMENT_3D ( 'NONE', #89417, #7940, #73739 ) ;
#29439 = CARTESIAN_POINT ( 'NONE',  ( -77.19855406467927139, -56.84693317175008787, 146.5104320596075240 ) ) ;
#29440 = ORIENTED_EDGE ( 'NONE', *, *, #2196, .F. ) ;
#29441 = DIRECTION ( 'NONE',  ( -1.000000000000000000, -1.224606353822377258E-16, -0.000000000000000000 ) ) ;
#29442 = DIRECTION ( 'NONE',  ( -1.000000000000000000, -1.224606353822377258E-16, -0.000000000000000000 ) ) ;
#29443 = CARTESIAN_POINT ( 'NONE',  ( 75.69611295408795115, -57.55331998792648562, 192.5082608592401812 ) ) ;
#29444 = PRESENTATION_STYLE_ASSIGNMENT (( #28925 ) ) ;
#29445 = UNCERTAINTY_MEASURE_WITH_UNIT (LENGTH_MEASURE( 1.000000000000000082E-05 ), #13655, 'distance_accuracy_value', 'NONE');
#29446 = CARTESIAN_POINT ( 'NONE',  ( 44.17878650602291657, 334.0442197469624830, -0.5072527954545905660 ) ) ;
#29447 = CARTESIAN_POINT ( 'NONE',  ( 44.29460294111461138, 463.8401613562670605, 7.966579552400246733 ) ) ;
#29448 = ORIENTED_EDGE ( 'NONE', *, *, #50201, .F. ) ;
#29449 = CARTESIAN_POINT ( 'NONE',  ( 0.000000000000000000, 25.16329480281783759, 0.000000000000000000 ) ) ;
#29450 = CARTESIAN_POINT ( 'NONE',  ( 15.88167336557654430, 44.00174513017344680, 4.402966589011110266 ) ) ;
#29451 = CARTESIAN_POINT ( 'NONE',  ( 7.188101187500001821, -25.06250000204838457, -2.977408999572650483 ) ) ;
#29452 = VERTEX_POINT ( 'NONE', #23866 ) ;
#29453 =( BOUNDED_SURFACE ( )  B_SPLINE_SURFACE ( 3, 2, ( 
 ( #87550, #79440, #29864 ),
 ( #94593, #6076, #104241 ),
 ( #20741, #21772, #70302 ),
 ( #103198, #53578, #22834 ),
 ( #28821, #96175, #22304 ),
 ( #86510, #12570, #78378 ),
 ( #29344, #41113, #98280 ),
 ( #40576, #81532, #24951 ),
 ( #24437, #31975, #65388 ),
 ( #31457, #88603, #32516 ),
 ( #64852, #33048, #14688 ),
 ( #90192, #57269, #106354 ) ),
 .UNSPECIFIED., .F., .F., .F. ) 
 B_SPLINE_SURFACE_WITH_KNOTS ( ( 4, 2, 2, 2, 2, 4 ),
 ( 3, 3 ),
 ( 4.336808689942017736E-18, 0.001679904595664889885, 0.003359809191329775433, 0.004199761489162218316, 0.005039713786994660764, 0.006719618382659546529 ),
 ( 0.000000000000000000, 1.000000000000000000 ),
 .UNSPECIFIED. ) 
 GEOMETRIC_REPRESENTATION_ITEM ( )  RATIONAL_B_SPLINE_SURFACE ( (
 ( 1.000000000000000000, 0.8014084173415133572, 1.000000000000000000),
 ( 1.000000000000000000, 0.8133474198053308735, 1.000000000000000000),
 ( 1.000000000000000000, 0.8251589633820495262, 1.000000000000000000),
 ( 1.000000000000000000, 0.8478574907211462452, 1.000000000000000000),
 ( 1.000000000000000000, 0.8587488926515607357, 1.000000000000000000),
 ( 1.000000000000000000, 0.8739423948897212524, 1.000000000000000000),
 ( 1.000000000000000000, 0.8787956638559124567, 1.000000000000000000),
 ( 1.000000000000000000, 0.8878757020716896431, 1.000000000000000000),
 ( 1.000000000000000000, 0.8921241670187577411, 1.000000000000000000),
 ( 1.000000000000000000, 0.9038999154881867115, 1.000000000000000000),
 ( 1.000000000000000000, 0.9104653308039090120, 1.000000000000000000),
 ( 1.000000000000000000, 0.9153908114177995436, 1.000000000000000000) ) ) 
 REPRESENTATION_ITEM ( '' )  SURFACE ( )  );
#29454 = FACE_OUTER_BOUND ( 'NONE', #10795, .T. ) ;
#29455 = CARTESIAN_POINT ( 'NONE',  ( 6.074379128844155318, 41.75280174920714416, -70.48890179791422383 ) ) ;
#29456 = EDGE_CURVE ( 'NONE', #32552, #88140, #19966, .T. ) ;
#29457 = DIRECTION ( 'NONE',  ( -1.000000000000000000, -0.000000000000000000, -0.000000000000000000 ) ) ;
#29458 = CARTESIAN_POINT ( 'NONE',  ( 5.140490343214302094, -10.64767277737062301, -10.57915202476631578 ) ) ;
#29459 = VECTOR ( 'NONE', #55408, 1000.000000000000000 ) ;
#29460 = CARTESIAN_POINT ( 'NONE',  ( -37.05595180434684011, 463.3109355731702408, 20.11755950910318447 ) ) ;
#29461 = ORIENTED_EDGE ( 'NONE', *, *, #94904, .F. ) ;
#29462 = AXIS2_PLACEMENT_3D ( 'NONE', #9372, #2356, #16970 ) ;
#29463 = CARTESIAN_POINT ( 'NONE',  ( 60.59807815084354132, -59.99999999999997868, -35.49710509377640477 ) ) ;
#29465 = CARTESIAN_POINT ( 'NONE',  ( 26.49659615693567005, -49.91097369680763052, 33.89243893083332893 ) ) ;
#29464 = CARTESIAN_POINT ( 'NONE',  ( -49.67087318978585841, -59.99999999999999289, 77.31351762338060496 ) ) ;
#29466 = CARTESIAN_POINT ( 'NONE',  ( 26.13315753361836613, 60.33964880548970910, 13.06657876680918839 ) ) ;
#29467 = EDGE_CURVE ( 'NONE', #32062, #7306, #16729, .T. ) ;
#29468 = VERTEX_POINT ( 'NONE', #52347 ) ;
#29469 = ORIENTED_EDGE ( 'NONE', *, *, #93163, .T. ) ;
#29470 =( LENGTH_UNIT ( ) NAMED_UNIT ( * ) SI_UNIT ( .MILLI., .METRE. ) );
#29471 = CARTESIAN_POINT ( 'NONE',  ( 1.469576158976823671E-14, 0.000000000000000000, -60.00000000000000000 ) ) ;
#29472 = CARTESIAN_POINT ( 'NONE',  ( 14.63297776001217798, 0.3240115842722206541, 14.99725733981229325 ) ) ;
#29473 = CARTESIAN_POINT ( 'NONE',  ( -16.13590653351290527, 6.313628335808340708, 5.716602451450103928 ) ) ;
#29474 = ORIENTED_EDGE ( 'NONE', *, *, #60499, .F. ) ;
#29475 = CARTESIAN_POINT ( 'NONE',  ( 43.00000000000000000, 436.0987441542287115, 7.567257455462724991 ) ) ;
#29476 = CARTESIAN_POINT ( 'NONE',  ( 22.88862750579858130, 25.33095312007748134, -33.17288371515036260 ) ) ;
#29477 = CARTESIAN_POINT ( 'NONE',  ( -12.85904595378377735, 23.43151218796164059, -4.877252156032461095 ) ) ;
#29479 = CARTESIAN_POINT ( 'NONE',  ( -5.382954851612917757, -82.00012508510555165, -2.657971597726724866 ) ) ;
#29478 = CIRCLE ( 'NONE', #89722, 9.999999999999994671 ) ;
#29480 = CARTESIAN_POINT ( 'NONE',  ( 81.33754917041331112, -29.99999999999999645, -1.044461975028134759 ) ) ;
#29481 = CARTESIAN_POINT ( 'NONE',  ( 4.699999999999999289, 6.499999999999999112, 0.000000000000000000 ) ) ;
#29482 = ORIENTED_EDGE ( 'NONE', *, *, #13975, .F. ) ;
#29483 = ADVANCED_FACE ( 'NONE', ( #67490 ), #92268, .T. ) ;
#29484 = AXIS2_PLACEMENT_3D ( 'NONE', #62933, #102856, #94784 ) ;
#29485 = VERTEX_POINT ( 'NONE', #76621 ) ;
#29486 = EDGE_LOOP ( 'NONE', ( #38209, #61098, #8146, #94621 ) ) ;
#29487 = DIRECTION ( 'NONE',  ( 0.000000000000000000, 1.000000000000000000, 0.000000000000000000 ) ) ;
#29488 = CARTESIAN_POINT ( 'NONE',  ( 0.000000000000000000, 0.000000000000000000, -6.800000000000000711 ) ) ;
#29489 = DIRECTION ( 'NONE',  ( 0.000000000000000000, 0.000000000000000000, 1.000000000000000000 ) ) ;
#29491 = PRESENTATION_LAYER_ASSIGNMENT (  '', '', ( #20887 ) ) ;
#29490 = CARTESIAN_POINT ( 'NONE',  ( -43.67962475666660538, 397.2192610118504490, 16.03014433720793264 ) ) ;
#29492 = FILL_AREA_STYLE_COLOUR ( '', #4250 ) ;
#29493 = CARTESIAN_POINT ( 'NONE',  ( -7.045965687440310710, -86.30392463786033375, 3.790395326974321133 ) ) ;
#29494 = CARTESIAN_POINT ( 'NONE',  ( 28.58349330513380337, 1.593028355512270962E-15, 0.000000000000000000 ) ) ;
#29495 = ORIENTED_EDGE ( 'NONE', *, *, #51592, .T. ) ;
#29496 = CARTESIAN_POINT ( 'NONE',  ( 7.996668422908976837, 49.99999999999999289, -78.85453279918145597 ) ) ;
#29497 = AXIS2_PLACEMENT_3D ( 'NONE', #39947, #74416, #64752 ) ;
#29498 = ORIENTED_EDGE ( 'NONE', *, *, #61575, .F. ) ;
#29499 = EDGE_CURVE ( 'NONE', #33789, #70286, #378, .T. ) ;
#29500 = CARTESIAN_POINT ( 'NONE',  ( -5.910690929868580135, -61.13504093906806247, -1.065041252563912133 ) ) ;
#29501 = DIRECTION ( 'NONE',  ( -1.000000000000000000, -0.000000000000000000, -0.000000000000000000 ) ) ;
#29502 = CARTESIAN_POINT ( 'NONE',  ( 31.63326088424243920, 436.4600345790572078, 18.87307648235493573 ) ) ;
#29503 = CARTESIAN_POINT ( 'NONE',  ( 22.10125386972620376, 303.2174250443505343, 10.01554689547207744 ) ) ;
#29504 = CARTESIAN_POINT ( 'NONE',  ( -82.14545208350013183, -60.00000000000006395, 187.9265396763507567 ) ) ;
#29505 = CARTESIAN_POINT ( 'NONE',  ( 64.14738722512768732, -42.95805876620670460, 85.49931417512519261 ) ) ;
#29506 = ORIENTED_EDGE ( 'NONE', *, *, #86051, .T. ) ;
#29507 = CARTESIAN_POINT ( 'NONE',  ( 42.20540931547678554, 464.9254549434356250, 14.73500713293391229 ) ) ;
#29508 = CARTESIAN_POINT ( 'NONE',  ( -46.27818643745989391, -34.68435135132106240, -36.71170783072079047 ) ) ;
#29509 = CARTESIAN_POINT ( 'NONE',  ( -37.85084083633361729, 438.0234350436313093, 4.171260309356228824 ) ) ;
#29510 = DIRECTION ( 'NONE',  ( 0.000000000000000000, -1.000000000000000000, 0.000000000000000000 ) ) ;
#29511 = EDGE_CURVE ( 'NONE', #63262, #73090, #97703, .T. ) ;
#29512 = VERTEX_POINT ( 'NONE', #94431 ) ;
#29513 = CIRCLE ( 'NONE', #20908, 4.000000000000000888 ) ;
#29514 = DIRECTION ( 'NONE',  ( 0.2255559232117683721, 0.1250062448739182319, 0.9661769839147531513 ) ) ;
#29515 = SURFACE_STYLE_FILL_AREA ( #53224 ) ;
#29516 = AXIS2_PLACEMENT_3D ( 'NONE', #10761, #78169, #60942 ) ;
#29517 = DIRECTION ( 'NONE',  ( 0.000000000000000000, 0.000000000000000000, 1.000000000000000000 ) ) ;
#29518 = VECTOR ( 'NONE', #8478, 1000.000000000000000 ) ;
#29519 = LINE ( 'NONE', #95284, #13595 ) ;
#29520 = CARTESIAN_POINT ( 'NONE',  ( 4.574783636564629496, 5.228990388887477359, -6.171384342982557669 ) ) ;
#29521 = CARTESIAN_POINT ( 'NONE',  ( 86.58602178717934805, -20.72065498216530699, 184.1443362589780008 ) ) ;
#29522 = CARTESIAN_POINT ( 'NONE',  ( 0.000000000000000000, 43.00000000000000000, 57.86910460382442523 ) ) ;
#29523 = CARTESIAN_POINT ( 'NONE',  ( -9.999142969110272006, 7.501227345713487260, 5.000000000000000888 ) ) ;
#29524 =( LENGTH_UNIT ( ) NAMED_UNIT ( * ) SI_UNIT ( .MILLI., .METRE. ) );
#29525 = CARTESIAN_POINT ( 'NONE',  ( -42.79914298581935839, 484.2777690190095541, -1.375851118298070164 ) ) ;
#29526 = CARTESIAN_POINT ( 'NONE',  ( 13.50905259634051170, -52.70511631464653846, 23.32354201833150853 ) ) ;
#29527 = CARTESIAN_POINT ( 'NONE',  ( 5.000000000000000000, -14.73352921087159295, 12.39872608460982661 ) ) ;
#29528 = CARTESIAN_POINT ( 'NONE',  ( -100.7573317175203584, -29.99999999999998934, 180.7148766695847542 ) ) ;
#29529 = EDGE_CURVE ( 'NONE', #95250, #55889, #77705, .T. ) ;
#29530 = COLOUR_RGB ( '', 0.66274510, 0.83137255, 0.94901961) ;
#29531 = DIRECTION ( 'NONE',  ( 0.000000000000000000, 0.000000000000000000, -1.000000000000000000 ) ) ;
#29532 = CARTESIAN_POINT ( 'NONE',  ( 27.29310425584678157, -57.67805528695544126, 43.98917206289641513 ) ) ;
#29534 = CARTESIAN_POINT ( 'NONE',  ( -7.000000000000000000, 8.572527594031471218E-16, -4.425378966781146950 ) ) ;
#29533 = CARTESIAN_POINT ( 'NONE',  ( -9.176645556628276523, 249.4726096759326310, 3.973966573947711023 ) ) ;
#29535 = EDGE_CURVE ( 'NONE', #39668, #61495, #78776, .T. ) ;
#29536 =( LENGTH_UNIT ( ) NAMED_UNIT ( * ) SI_UNIT ( .MILLI., .METRE. ) );
#29537 = CARTESIAN_POINT ( 'NONE',  ( -18.92758526587351398, 50.00000000000000711, 60.68418741241684700 ) ) ;
#29538 = DIRECTION ( 'NONE',  ( -0.2280158659362349349, 0.1533051183515994065, 0.9615125093146479340 ) ) ;
#29539 = FACE_OUTER_BOUND ( 'NONE', #88590, .T. ) ;
#29540 = FACE_OUTER_BOUND ( 'NONE', #35512, .T. ) ;
#29541 = FILL_AREA_STYLE ('',( #13296 ) ) ;
#29542 = CARTESIAN_POINT ( 'NONE',  ( -86.95016803385389892, -20.65679883627421987, 186.2957625121753722 ) ) ;
#29544 = EDGE_CURVE ( 'NONE', #67639, #53305, #94642, .T. ) ;
#29543 = AXIS2_PLACEMENT_3D ( 'NONE', #93146, #12743, #36546 ) ;
#29545 = VERTEX_POINT ( 'NONE', #12943 ) ;
#29546 = CARTESIAN_POINT ( 'NONE',  ( 40.67924138885037166, 485.8013567632063996, -4.837443355053446581 ) ) ;
#29547 = CARTESIAN_POINT ( 'NONE',  ( -13.22635504380575355, -22.06836642973110330, 27.64052428449707577 ) ) ;
#29548 = COLOUR_RGB ( '', 0.31764706, 0.68627451, 0.89019608) ;
#29550 = LINE ( 'NONE', #4711, #6077 ) ;
#29549 = CARTESIAN_POINT ( 'NONE',  ( -86.67772857939944231, -60.00000000000007816, -11.42669097351372187 ) ) ;
#29551 = ORIENTED_EDGE ( 'NONE', *, *, #38218, .F. ) ;
#29553 = B_SPLINE_CURVE_WITH_KNOTS ( 'NONE', 3,
 ( #4851, #53913, #86845, #5384, #28100, #101940, #60975, #62052, #52863, #95446, #13978, #20021, #38304, #95988, #71164, #104059, #4315, #11865, #77683, #20567, #63087, #12920, #30201, #85791, #22113, #86324, #29688, #102486, #69594, #44794, #45842, #37250, #70113, #37785 ),
 .UNSPECIFIED., .F., .F.,
 ( 4, 2, 2, 2, 2, 2, 2, 2, 2, 2, 2, 2, 2, 2, 2, 2, 4 ),
 ( 0.5000000000000000000, 0.5312500000000000000, 0.5625000000000000000, 0.5937500000000000000, 0.6250000000000000000, 0.6562500000000000000, 0.6875000000000000000, 0.7187500000000000000, 0.7500000000000000000, 0.7812500000000000000, 0.8125000000000000000, 0.8437500000000000000, 0.8750000000000000000, 0.9062500000000000000, 0.9375000000000000000, 0.9687500000000000000, 1.000000000000000000 ),
 .UNSPECIFIED. ) ;
#29552 = AXIS2_PLACEMENT_3D ( 'NONE', #30177, #30726, #46349 ) ;
#29554 = CARTESIAN_POINT ( 'NONE',  ( 7.432714112156483503E-16, -0.6346842323187762425, -6.500000000000000888 ) ) ;
#29555 = CONICAL_SURFACE ( 'NONE', #101887, 4.000000000000001776, 0.9599310885968774798 ) ;
#29556 = CIRCLE ( 'NONE', #79399, 4.000000000000001776 ) ;
#29557 = CARTESIAN_POINT ( 'NONE',  ( 16.03938085755554255, 4.451364308013095794, -3.146830695484701845 ) ) ;
#29558 = CARTESIAN_POINT ( 'NONE',  ( -42.09210974227526947, 317.4093497706929270, -4.557617623460385126 ) ) ;
#29559 = ORIENTED_EDGE ( 'NONE', *, *, #54518, .T. ) ;
#29560 = CARTESIAN_POINT ( 'NONE',  ( 32.73226863436134693, 439.3384463444876360, 23.76670009903627800 ) ) ;
#29561 = DIRECTION ( 'NONE',  ( -1.000000000000000000, -0.000000000000000000, -0.000000000000000000 ) ) ;
#29563 =( LENGTH_UNIT ( ) NAMED_UNIT ( * ) SI_UNIT ( .MILLI., .METRE. ) );
#29562 = CARTESIAN_POINT ( 'NONE',  ( 50.54929637512975660, -37.96391612271221305, 51.13126295237949392 ) ) ;
#29564 = LINE ( 'NONE', #59925, #59608 ) ;
#29565 = ORIENTED_EDGE ( 'NONE', *, *, #70730, .T. ) ;
#29566 = ORIENTED_EDGE ( 'NONE', *, *, #70750, .F. ) ;
#29567 = ORIENTED_EDGE ( 'NONE', *, *, #60558, .F. ) ;
#29568 = CARTESIAN_POINT ( 'NONE',  ( -40.89305344739149461, 461.0673237560018833, 2.333915627062479903 ) ) ;
#29569 = DIRECTION ( 'NONE',  ( 0.000000000000000000, -1.000000000000000000, 0.000000000000000000 ) ) ;
#29570 = ORIENTED_EDGE ( 'NONE', *, *, #55075, .F. ) ;
#29571 = ADVANCED_FACE ( 'NONE', ( #30224 ), #22138, .T. ) ;
#29572 = CARTESIAN_POINT ( 'NONE',  ( 17.50000000000004974, 48.00000000000341771, 64.09949417230997426 ) ) ;
#29573 = CARTESIAN_POINT ( 'NONE',  ( -6.403344576203515714, 41.95607710195889695, -69.22843915075077348 ) ) ;
#29575 = CARTESIAN_POINT ( 'NONE',  ( -114.2613009911679427, -59.99999999997056221, 181.1642683633762942 ) ) ;
#29574 = AXIS2_PLACEMENT_3D ( 'NONE', #60969, #62044, #20013 ) ;
#29576 = LINE ( 'NONE', #62448, #27355 ) ;
#29577 = CARTESIAN_POINT ( 'NONE',  ( 93.94581488726784357, -60.00000000000240874, -15.82352347238299650 ) ) ;
#29578 = CARTESIAN_POINT ( 'NONE',  ( 6.575918192882431512, 3.850883087735901711, -6.669925161966311578 ) ) ;
#29579 = CARTESIAN_POINT ( 'NONE',  ( -5.662864552301164700, 41.84935256917250967, -58.94136742042883981 ) ) ;
#29580 = CIRCLE ( 'NONE', #58810, 4.000000000000000888 ) ;
#29582 = CARTESIAN_POINT ( 'NONE',  ( 10.44722405557104494, -56.87790227778863539, 33.38355414254041165 ) ) ;
#29581 = CARTESIAN_POINT ( 'NONE',  ( -104.0151861009774166, -30.00000000000006750, 120.6691871043967126 ) ) ;
#29584 = EDGE_CURVE ( 'NONE', #12412, #53703, #96543, .T. ) ;
#29583 = CARTESIAN_POINT ( 'NONE',  ( -7.473472438902638793, 52.16903957423301108, 2.156585108680202367 ) ) ;
#29585 = CARTESIAN_POINT ( 'NONE',  ( -48.11708999912524121, -29.14444454005715102, 44.62783549548100837 ) ) ;
#29586 = CIRCLE ( 'NONE', #101834, 14.99698745252234566 ) ;
#29587 = DIRECTION ( 'NONE',  ( 0.000000000000000000, 0.000000000000000000, 1.000000000000000000 ) ) ;
#29588 = EDGE_LOOP ( 'NONE', ( #52114, #74857, #100245, #13383, #94025, #80438 ) ) ;
#29589 = CARTESIAN_POINT ( 'NONE',  ( 0.8472790622787957915, 12.94205918040166203, -49.56287671100434267 ) ) ;
#29590 = CARTESIAN_POINT ( 'NONE',  ( 0.000000000000000000, 0.000000000000000000, -8.000000000000000000 ) ) ;
#29591 = LINE ( 'NONE', #51690, #17201 ) ;
#29592 = ORIENTED_EDGE ( 'NONE', *, *, #97761, .F. ) ;
#29593 = CARTESIAN_POINT ( 'NONE',  ( -6.408521271130449115, -15.51162931541124124, 14.54064475688238822 ) ) ;
#29594 = ORIENTED_EDGE ( 'NONE', *, *, #36377, .F. ) ;
#29595 = CARTESIAN_POINT ( 'NONE',  ( 46.12602165870173820, -38.31898768030290370, 59.97271842373840656 ) ) ;
#29596 = SURFACE_STYLE_FILL_AREA ( #103964 ) ;
#29597 = FACE_OUTER_BOUND ( 'NONE', #14128, .T. ) ;
#29598 = CARTESIAN_POINT ( 'NONE',  ( -47.37019975550713724, 41.99999999999999289, 36.40416150952766827 ) ) ;
#29599 = CARTESIAN_POINT ( 'NONE',  ( 95.99411590063971289, -30.00000000000000000, 191.2869372966427193 ) ) ;
#29600 = CARTESIAN_POINT ( 'NONE',  ( -10.28624191511820207, -1.200000000000000030E-05, 15.40779740156164124 ) ) ;
#29601 = VERTEX_POINT ( 'NONE', #37274 ) ;
#29602 = EDGE_CURVE ( 'NONE', #1636, #82896, #71840, .T. ) ;
#29603 = ORIENTED_EDGE ( 'NONE', *, *, #62421, .F. ) ;
#29604 = ORIENTED_EDGE ( 'NONE', *, *, #9174, .F. ) ;
#29605 = CARTESIAN_POINT ( 'NONE',  ( 54.56792591830877370, -22.15785971680534416, 52.62277654788229597 ) ) ;
#29606 = CARTESIAN_POINT ( 'NONE',  ( -46.00000000000000000, 438.0901456946749022, 11.29311581785933072 ) ) ;
#29607 = LINE ( 'NONE', #5816, #106487 ) ;
#29608 = EDGE_CURVE ( 'NONE', #23483, #73133, #7105, .T. ) ;
#29609 = ORIENTED_EDGE ( 'NONE', *, *, #54901, .T. ) ;
#29610 = CARTESIAN_POINT ( 'NONE',  ( -18.00000000000000355, 12.99999999999999289, 0.000000000000000000 ) ) ;
#29611 = VERTEX_POINT ( 'NONE', #14000 ) ;
#29612 = CARTESIAN_POINT ( 'NONE',  ( -3.981862520314373377, 4.887481193368610871E-16, -0.01269999999999786924 ) ) ;
#29613 = CARTESIAN_POINT ( 'NONE',  ( 88.56294407034239669, -38.54372130031631372, 200.1479997606907659 ) ) ;
#29614 = CARTESIAN_POINT ( 'NONE',  ( 10.65767722103599979, 14.87225365928225607, 9.828355766833842821 ) ) ;
#29615 = CARTESIAN_POINT ( 'NONE',  ( 86.55999845485922606, -60.13929112694511048, 1.461019888335082673 ) ) ;
#29616 = PLANE ( 'NONE',  #28759 ) ;
#29617 = CARTESIAN_POINT ( 'NONE',  ( 42.70246075394577900, 373.2460375941973894, 18.12284514452785089 ) ) ;
#29618 = DIRECTION ( 'NONE',  ( 0.000000000000000000, 0.000000000000000000, 1.000000000000000000 ) ) ;
#29619 = EDGE_CURVE ( 'NONE', #70575, #55309, #25386, .T. ) ;
#29620 = COLOUR_RGB ( '', 0.66274510, 0.83137255, 0.94901961) ;
#29621 = DIRECTION ( 'NONE',  ( 0.000000000000000000, 0.000000000000000000, 1.000000000000000000 ) ) ;
#29622 = CIRCLE ( 'NONE', #55432, 4.000000000000007105 ) ;
#29623 = PRESENTATION_STYLE_ASSIGNMENT (( #5318 ) ) ;
#29624 = ORIENTED_EDGE ( 'NONE', *, *, #79527, .T. ) ;
#29625 = CARTESIAN_POINT ( 'NONE',  ( -9.380155525692149610, 15.95825086476136967, -3.484792534604211234 ) ) ;
#29626 = CARTESIAN_POINT ( 'NONE',  ( 69.18888888888888289, -3.309500000000000774, 4.475777889183797681E-16 ) ) ;
#29627 = DIRECTION ( 'NONE',  ( 0.000000000000000000, 0.000000000000000000, 1.000000000000000000 ) ) ;
#29628 = EDGE_LOOP ( 'NONE', ( #79791, #20350 ) ) ;
#29629 = CARTESIAN_POINT ( 'NONE',  ( 0.06809871960542691893, 6.146186931204407067, 5.354491962338125077 ) ) ;
#29630 = CARTESIAN_POINT ( 'NONE',  ( -30.94128241318078665, 298.6042193091406602, 2.768098133593460908 ) ) ;
#29631 = CARTESIAN_POINT ( 'NONE',  ( 36.36650669486618881, 1.474610560812782335E-15, 0.000000000000000000 ) ) ;
#29632 = FACE_OUTER_BOUND ( 'NONE', #23160, .T. ) ;
#29633 = CARTESIAN_POINT ( 'NONE',  ( 8.000000000000000000, -22.90624999999999645, -3.313708498984761608 ) ) ;
#29634 = CARTESIAN_POINT ( 'NONE',  ( 45.71963875501243280, -29.99999999999999645, 56.30994126864628413 ) ) ;
#29635 = PRESENTATION_LAYER_ASSIGNMENT (  '', '', ( #103650 ) ) ;
#29636 = VECTOR ( 'NONE', #11551, 1000.000000000000000 ) ;
#29637 = PRODUCT_DEFINITION_SHAPE ( 'NONE', 'NONE',  #106814 ) ;
#29638 = CARTESIAN_POINT ( 'NONE',  ( -43.00000000000000000, 488.3725375423296100, 3.127739281037506647 ) ) ;
#29639 = VERTEX_POINT ( 'NONE', #105156 ) ;
#29640 = CARTESIAN_POINT ( 'NONE',  ( 83.65579274812736799, -50.12940242402542879, 185.8577423453587585 ) ) ;
#29641 = CARTESIAN_POINT ( 'NONE',  ( 6.575918192882435953, -7.701766175471826514, -3.282668101273427886E-15 ) ) ;
#29642 = CARTESIAN_POINT ( 'NONE',  ( 3.857142857142854542, -1.200583151104942070, 103.1763305333244318 ) ) ;
#29643 = ORIENTED_EDGE ( 'NONE', *, *, #9276, .T. ) ;
#29644 = CARTESIAN_POINT ( 'NONE',  ( 93.83764888837048090, -57.67474972874411066, 11.09789775104367848 ) ) ;
#29645 = CARTESIAN_POINT ( 'NONE',  ( 16.36650669486618881, 1.474610560812782335E-15, 0.000000000000000000 ) ) ;
#29646 = CARTESIAN_POINT ( 'NONE',  ( -2.751706330279349633, -5.000000000000015987, -99.99999999999998579 ) ) ;
#29647 = CARTESIAN_POINT ( 'NONE',  ( -30.77208753046711820, 10.36816855262254933, 40.23037088889264368 ) ) ;
#29648 = DIRECTION ( 'NONE',  ( -1.000000000000000000, -1.224606353822377258E-16, -0.000000000000000000 ) ) ;
#29649 = EDGE_CURVE ( 'NONE', #25485, #101, #14738, .T. ) ;
#29650 = SURFACE_STYLE_FILL_AREA ( #98965 ) ;
#29651 = CIRCLE ( 'NONE', #69201, 5.000000000000011546 ) ;
#29652 = MECHANICAL_DESIGN_GEOMETRIC_PRESENTATION_REPRESENTATION (  '', ( #22726 ), #45121 ) ;
#29653 = CARTESIAN_POINT ( 'NONE',  ( 13.00603131147514802, -21.61757453066702439, 35.67497680198176369 ) ) ;
#29654 = CARTESIAN_POINT ( 'NONE',  ( 3.363648053944605198, -1.214821636234522995, 104.5995868353016505 ) ) ;
#29655 = CARTESIAN_POINT ( 'NONE',  ( 45.19148592063464065, -28.36164282789344071, 40.27822637177104070 ) ) ;
#29657 = CARTESIAN_POINT ( 'NONE',  ( -10.65078532968085590, 18.17514175625904826, 9.445934609551695615 ) ) ;
#29656 = DIRECTION ( 'NONE',  ( 0.5735764363510440500, 0.8191520442889932418, 0.000000000000000000 ) ) ;
#29658 = EDGE_CURVE ( 'NONE', #55349, #100024, #64698, .T. ) ;
#29659 = PRESENTATION_LAYER_ASSIGNMENT (  '', '', ( #24499 ) ) ;
#29660 = CARTESIAN_POINT ( 'NONE',  ( 8.849035312350377325, 302.6218124188690126, -10.03679229143238594 ) ) ;
#29661 = CARTESIAN_POINT ( 'NONE',  ( -16.56380429469772153, 43.78423957885634366, -4.157797401561426298 ) ) ;
#29662 = CARTESIAN_POINT ( 'NONE',  ( 37.12595521884477989, 306.0480932226964796, 0.6086346269186700964 ) ) ;
#29663 = CARTESIAN_POINT ( 'NONE',  ( -43.03185303983481447, 485.3613526602391062, 6.073233449168579767 ) ) ;
#29664 = CARTESIAN_POINT ( 'NONE',  ( -83.70148025459225494, -38.00000000000000000, 34.15054458896100442 ) ) ;
#29665 = EDGE_CURVE ( 'NONE', #44183, #26535, #48492, .T. ) ;
#29666 = VERTEX_POINT ( 'NONE', #24789 ) ;
#29667 = CARTESIAN_POINT ( 'NONE',  ( -12.30573667306818031, 1.921380894879668233, 14.87702195164505348 ) ) ;
#29668 = DIRECTION ( 'NONE',  ( 0.000000000000000000, 1.000000000000000000, 0.000000000000000000 ) ) ;
#29669 = CARTESIAN_POINT ( 'NONE',  ( 4.903871675326605839, -62.97914192698504365, -3.461400506969857016 ) ) ;
#29671 = CARTESIAN_POINT ( 'NONE',  ( -7.761546958154228903, -21.77037872703017385, -30.37584562454359727 ) ) ;
#29670 = DIRECTION ( 'NONE',  ( -1.000000000000000000, 0.000000000000000000, 0.000000000000000000 ) ) ;
#29672 = ORIENTED_EDGE ( 'NONE', *, *, #47917, .T. ) ;
#29673 = B_SPLINE_CURVE_WITH_KNOTS ( 'NONE', 3,
 ( #103551, #80314, #31286, #23719, #70656, #38314, #15057, #29701, #63098, #95458 ),
 .UNSPECIFIED., .F., .F.,
 ( 4, 2, 2, 2, 4 ),
 ( 0.0005274614566083536769, 0.002396735553633655511, 0.003331372602146292008, 0.003798691126402609607, 0.004266009650658927205 ),
 .UNSPECIFIED. ) ;
#29674 = CARTESIAN_POINT ( 'NONE',  ( 1.282512619719359481, 8.391164935523910628, -7.795653906408836598 ) ) ;
#29675 = CARTESIAN_POINT ( 'NONE',  ( 0.2573354458087865893, -4.368923434677202344, -5.432802636760777126 ) ) ;
#29676 = ORIENTED_EDGE ( 'NONE', *, *, #4195, .F. ) ;
#29677 = FACE_OUTER_BOUND ( 'NONE', #74110, .T. ) ;
#29678 = DIRECTION ( 'NONE',  ( 0.000000000000000000, 1.000000000000000000, 0.000000000000000000 ) ) ;
#29679 = CARTESIAN_POINT ( 'NONE',  ( -92.74820878259032497, -59.99999999999999289, -6.808916855407564306 ) ) ;
#29680 = ORIENTED_EDGE ( 'NONE', *, *, #68800, .T. ) ;
#29681 = LINE ( 'NONE', #78707, #82455 ) ;
#29682 = CARTESIAN_POINT ( 'NONE',  ( 0.000000000000000000, 0.000000000000000000, 4.000000000000000888 ) ) ;
#29683 = CARTESIAN_POINT ( 'NONE',  ( -9.165151389911679658, 30.00000000000000000, 4.000000000000000000 ) ) ;
#29685 = CARTESIAN_POINT ( 'NONE',  ( 6.999999999999997335, -80.00000000000000000, 39.12435565298213902 ) ) ;
#29684 = DIRECTION ( 'NONE',  ( 0.000000000000000000, 0.000000000000000000, -1.000000000000000000 ) ) ;
#29686 = CARTESIAN_POINT ( 'NONE',  ( -85.55402800175718880, -18.57074191616040792, 160.4554053421518915 ) ) ;
#29687 = ORIENTED_EDGE ( 'NONE', *, *, #6332, .F. ) ;
#29688 = CARTESIAN_POINT ( 'NONE',  ( -10.38441970549191495, 0.000000000000000000, 13.52487676487815271 ) ) ;
#29689 = AXIS2_PLACEMENT_3D ( 'NONE', #40881, #83461, #51624 ) ;
#29690 = EDGE_LOOP ( 'NONE', ( #2432, #75539, #67378, #7214, #18256, #19957 ) ) ;
#29691 = ORIENTED_EDGE ( 'NONE', *, *, #4531, .T. ) ;
#29692 = CARTESIAN_POINT ( 'NONE',  ( 0.000000000000000000, 0.000000000000000000, -60.00000000000000000 ) ) ;
#29693 = CARTESIAN_POINT ( 'NONE',  ( -1.919652159211370224, -70.56598577336447420, 13.12977962495732420 ) ) ;
#29694 =( NAMED_UNIT ( * ) SI_UNIT ( $, .STERADIAN. ) SOLID_ANGLE_UNIT ( ) );
#29695 = ORIENTED_EDGE ( 'NONE', *, *, #64219, .T. ) ;
#29696 = EDGE_CURVE ( 'NONE', #71461, #85977, #27161, .T. ) ;
#29697 = B_SPLINE_CURVE_WITH_KNOTS ( 'NONE', 3,
 ( #89927, #39797, #66180, #99058, #56481, #24688, #97470, #23095, #58079, #47854, #80762, #6876, #82899, #81807, #40840, #81283, #32239, #72673, #105573, #90459 ),
 .UNSPECIFIED., .F., .F.,
 ( 4, 2, 2, 2, 2, 2, 2, 2, 2, 4 ),
 ( 0.005450101279021335281, 0.005953876227450323640, 0.006457651175879311999, 0.006709538650093809647, 0.006961426124308298623, 0.007465201072737251420, 0.007968976021166205084, 0.008472750969595158749, 0.008976525918024112413, 0.009480300866453066078 ),
 .UNSPECIFIED. ) ;
#29698 = DIRECTION ( 'NONE',  ( 0.000000000000000000, -1.000000000000000000, 0.000000000000000000 ) ) ;
#29699 = CYLINDRICAL_SURFACE ( 'NONE', #78813, 63.00000000000000000 ) ;
#29700 = CARTESIAN_POINT ( 'NONE',  ( -110.1907765348834403, -57.67120634471875462, 130.2639824976604643 ) ) ;
#29701 = CARTESIAN_POINT ( 'NONE',  ( 1.226852121894917547, -49.99514363866957467, 101.2646212623072870 ) ) ;
#29702 = CARTESIAN_POINT ( 'NONE',  ( 43.55333112596304090, 465.2342844084867011, 9.238213423009598912 ) ) ;
#29703 = CARTESIAN_POINT ( 'NONE',  ( -9.699121749566359085, 101.8233123972417928, 2.444499528233565755 ) ) ;
#29704 = CARTESIAN_POINT ( 'NONE',  ( -16.91815790875651260, 37.08283480489694028, -21.80698433968595751 ) ) ;
#29705 = CARTESIAN_POINT ( 'NONE',  ( 81.17508142137076277, -14.21045842199431952, -20.85096179708197184 ) ) ;
#29706 = EDGE_CURVE ( 'NONE', #71316, #43097, #39159, .T. ) ;
#29707 = CARTESIAN_POINT ( 'NONE',  ( -76.24265395543058332, -14.21045842199434794, 145.5858823757693301 ) ) ;
#29708 = CARTESIAN_POINT ( 'NONE',  ( -54.95499996707611245, -46.44145850250006191, 63.02118750885743736 ) ) ;
#29709 = ORIENTED_EDGE ( 'NONE', *, *, #48303, .T. ) ;
#29710 = PRESENTATION_STYLE_ASSIGNMENT (( #61533 ) ) ;
#29711 = EDGE_LOOP ( 'NONE', ( #68008, #99420, #38575, #73143, #75102, #85770, #98200, #95692, #89679, #42419, #72305 ) ) ;
#29712 = CARTESIAN_POINT ( 'NONE',  ( -99.36458642854884715, -37.79545065244527535, 191.5056538517512195 ) ) ;
#29713 = DIRECTION ( 'NONE',  ( 0.000000000000000000, -1.000000000000000000, 0.000000000000000000 ) ) ;
#29714 = ADVANCED_FACE ( 'NONE', ( #17225 ), #21884, .T. ) ;
#29715 = VERTEX_POINT ( 'NONE', #52219 ) ;
#29716 = CARTESIAN_POINT ( 'NONE',  ( 19.37147048651776871, 49.91798333626284290, 61.09697252333796769 ) ) ;
#29717 = CARTESIAN_POINT ( 'NONE',  ( -42.75139825103929070, 485.3314578938633304, -3.157348782696939971 ) ) ;
#29718 = CARTESIAN_POINT ( 'NONE',  ( 2.977408999572650927, -14.75000000204838457, -7.188101187500001821 ) ) ;
#29719 = CARTESIAN_POINT ( 'NONE',  ( 35.76379064120181539, 307.0162303970107587, 12.81051142610679960 ) ) ;
#29720 = LINE ( 'NONE', #19520, #59970 ) ;
#29721 = CARTESIAN_POINT ( 'NONE',  ( 72.17674141521742115, -29.99999999999999645, 102.2643789533765784 ) ) ;
#29722 = CARTESIAN_POINT ( 'NONE',  ( 22.57792046605466041, 5.000000000000004441, 6.123233995736770227E-16 ) ) ;
#29723 = DIRECTION ( 'NONE',  ( 0.000000000000000000, -0.6886991506751505288, 0.7250472259510594153 ) ) ;
#29724 = CARTESIAN_POINT ( 'NONE',  ( 37.56673239365870387, -1.200000000000000030E-05, 10.95617127780998956 ) ) ;
#29725 = UNCERTAINTY_MEASURE_WITH_UNIT (LENGTH_MEASURE( 1.000000000000000082E-05 ), #4652, 'distance_accuracy_value', 'NONE');
#29726 = EDGE_CURVE ( 'NONE', #492, #91653, #52923, .T. ) ;
#29727 = CARTESIAN_POINT ( 'NONE',  ( -28.40130354532971779, -36.00929858293697805, 32.00103210455104374 ) ) ;
#29728 = AXIS2_PLACEMENT_3D ( 'NONE', #77024, #36087, #3143 ) ;
#29729 = VERTEX_POINT ( 'NONE', #11220 ) ;
#29730 = VERTEX_POINT ( 'NONE', #92689 ) ;
#29731 = CARTESIAN_POINT ( 'NONE',  ( 47.70061809322042023, -39.52289543229544933, 47.20263342004708562 ) ) ;
#29732 = AXIS2_PLACEMENT_3D ( 'NONE', #31452, #64334, #96692 ) ;
#29733 = CARTESIAN_POINT ( 'NONE',  ( -1.117054149123908102, 9.317683682317568383, 51.07842190223516354 ) ) ;
#29734 = DIRECTION ( 'NONE',  ( -1.000000000000000000, -1.224606353822377258E-16, -0.000000000000000000 ) ) ;
#29735 = CARTESIAN_POINT ( 'NONE',  ( -110.5701501222436605, -38.35612523280028796, 181.7181079214109047 ) ) ;
#29736 = VERTEX_POINT ( 'NONE', #26408 ) ;
#29737 = CARTESIAN_POINT ( 'NONE',  ( 90.64011768444591155, -38.34321871509011004, 9.780805722092965837 ) ) ;
#29738 = CARTESIAN_POINT ( 'NONE',  ( 14.04769258328531834, 4.430038579581392355, -5.212585019726944324 ) ) ;
#29739 = CARTESIAN_POINT ( 'NONE',  ( -6.917891564935159998, 41.82074884801031800, -68.91429205806258551 ) ) ;
#29740 = CARTESIAN_POINT ( 'NONE',  ( 5.556067581535544697, 40.28998946031890682, -71.04001546082351126 ) ) ;
#29741 = DIRECTION ( 'NONE',  ( -1.000000000000000000, -1.224606353822377258E-16, -0.000000000000000000 ) ) ;
#29742 = CARTESIAN_POINT ( 'NONE',  ( -31.88073664226197934, 435.8776075131638663, 17.60257548430462293 ) ) ;
#29744 = AXIS2_PLACEMENT_3D ( 'NONE', #5693, #88219, #55806 ) ;
#29743 = CARTESIAN_POINT ( 'NONE',  ( 10.50000000000000711, -5.000000000000000000, -79.51734232575269345 ) ) ;
#29745 = EDGE_CURVE ( 'NONE', #45187, #87964, #85679, .T. ) ;
#29746 = CARTESIAN_POINT ( 'NONE',  ( 93.66759751282268098, -60.00000000000001421, 202.5255995218111877 ) ) ;
#29747 = B_SPLINE_CURVE_WITH_KNOTS ( 'NONE', 3,
 ( #80385, #98684, #31357, #105724, #39430, #72303 ),
 .UNSPECIFIED., .F., .F.,
 ( 4, 2, 4 ),
 ( 0.004615310220740741730, 0.006918661718823352832, 0.009222013216905963068 ),
 .UNSPECIFIED. ) ;
#29748 =( BOUNDED_SURFACE ( )  B_SPLINE_SURFACE ( 3, 2, ( 
 ( #73463, #49731, #25503 ),
 ( #99879, #50773, #33572 ),
 ( #16298, #33053, #59442 ),
 ( #74533, #75057, #1152 ) ),
 .UNSPECIFIED., .F., .F., .F. ) 
 B_SPLINE_SURFACE_WITH_KNOTS ( ( 4, 4 ),
 ( 3, 3 ),
 ( 0.05518226518917336565, 0.08125438797488282461 ),
 ( 0.3700808604202216467, 1.000000000000000000 ),
 .UNSPECIFIED. ) 
 GEOMETRIC_REPRESENTATION_ITEM ( )  RATIONAL_B_SPLINE_SURFACE ( (
 ( 0.8634406061711257241, 0.8155005994179043149, 1.000000000000000000),
 ( 0.8634403698514303560, 0.8155002801367408072, 1.000000000000000000),
 ( 0.8634404275997331624, 0.8155003581579370886, 1.000000000000000000),
 ( 0.8634406601346265031, 0.8155006723256206236, 1.000000000000000000) ) ) 
 REPRESENTATION_ITEM ( '' )  SURFACE ( )  );
#29749 = CARTESIAN_POINT ( 'NONE',  ( -15.73921121718460014, 35.05971934485130959, 22.31943800541765910 ) ) ;
#29750 = ORIENTED_EDGE ( 'NONE', *, *, #2319, .T. ) ;
#29751 = CARTESIAN_POINT ( 'NONE',  ( -34.96345651127622034, 302.4133583293575498, -0.2769688069068840242 ) ) ;
#29752 = CARTESIAN_POINT ( 'NONE',  ( 6.944031699373469202, 30.53460654556128162, 3.972913591453821613 ) ) ;
#29753 = CARTESIAN_POINT ( 'NONE',  ( -6.928203230275510549, 29.73520732746428408, 3.999999999999999112 ) ) ;
#29754 = EDGE_LOOP ( 'NONE', ( #46018, #84585, #39393 ) ) ;
#29756 = CARTESIAN_POINT ( 'NONE',  ( 5.202160958754947551, 4.715235442947979472, -25.39438984414672262 ) ) ;
#29755 = CARTESIAN_POINT ( 'NONE',  ( -110.9831532232078075, -38.35615782300705945, 171.0432724854665594 ) ) ;
#29757 = CARTESIAN_POINT ( 'NONE',  ( 4.898587196589412829E-16, -21.12499999999999289, -8.000000000000000000 ) ) ;
#29758 = CARTESIAN_POINT ( 'NONE',  ( 43.18793366350566032, 465.6364658675358328, 10.75294125769881148 ) ) ;
#29759 = CARTESIAN_POINT ( 'NONE',  ( 4.401442555609581635E-16, -14.65625000204838457, -7.188101187500000044 ) ) ;
#29760 = CARTESIAN_POINT ( 'NONE',  ( 7.996668422911924701, -3.000000000000002665, -78.85453279918097280 ) ) ;
#29761 = DIRECTION ( 'NONE',  ( 0.000000000000000000, -1.000000000000000000, 0.000000000000000000 ) ) ;
#29762 = AXIS2_PLACEMENT_3D ( 'NONE', #62315, #95208, #5129 ) ;
#29763 = EDGE_LOOP ( 'NONE', ( #39878, #102042, #71050, #54537, #16634 ) ) ;
#29764 = CARTESIAN_POINT ( 'NONE',  ( 81.29766393407724934, -56.98409711725605575, 180.9609411103209879 ) ) ;
#29765 = DIRECTION ( 'NONE',  ( -0.5735764363510497121, 0.8191520442889892450, 1.003171929053521665E-16 ) ) ;
#29766 = FACE_OUTER_BOUND ( 'NONE', #50450, .T. ) ;
#29767 = ORIENTED_EDGE ( 'NONE', *, *, #72401, .T. ) ;
#29768 = AXIS2_PLACEMENT_3D ( 'NONE', #22617, #63044, #22070 ) ;
#29769 = CARTESIAN_POINT ( 'NONE',  ( -37.67790193267708077, 380.9199617470918611, 5.379015220008868781 ) ) ;
#29770 = DIRECTION ( 'NONE',  ( 0.000000000000000000, 0.000000000000000000, 1.000000000000000000 ) ) ;
#29771 = DIRECTION ( 'NONE',  ( 1.000000000000000000, -0.000000000000000000, 1.224646799147353207E-16 ) ) ;
#29772 = DIRECTION ( 'NONE',  ( 0.000000000000000000, 0.000000000000000000, -1.000000000000000000 ) ) ;
#29773 = CARTESIAN_POINT ( 'NONE',  ( 73.33904886068935980, 6.975173280561618775E-15, 0.000000000000000000 ) ) ;
#29774 = AXIS2_PLACEMENT_3D ( 'NONE', #41431, #91594, #50048 ) ;
#29775 =( NAMED_UNIT ( * ) SI_UNIT ( $, .STERADIAN. ) SOLID_ANGLE_UNIT ( ) );
#29776 = DIRECTION ( 'NONE',  ( -0.000000000000000000, -0.000000000000000000, -1.000000000000000000 ) ) ;
#29777 = ORIENTED_EDGE ( 'NONE', *, *, #83427, .T. ) ;
#29778 = EDGE_CURVE ( 'NONE', #48427, #76319, #89104, .T. ) ;
#29780 = CARTESIAN_POINT ( 'NONE',  ( -3.750000000000004441, -6.495190528383288253, 1.734723475976807094E-15 ) ) ;
#29779 = AXIS2_PLACEMENT_3D ( 'NONE', #30389, #15237, #13633 ) ;
#29781 = CARTESIAN_POINT ( 'NONE',  ( 11.84999999999999787, 1.533819458162526451E-15, 0.000000000000000000 ) ) ;
#29782 = DIRECTION ( 'NONE',  ( -1.224646799147353454E-16, 0.000000000000000000, -1.000000000000000000 ) ) ;
#29783 = EDGE_CURVE ( 'NONE', #52539, #94742, #34088, .T. ) ;
#29785 = CARTESIAN_POINT ( 'NONE',  ( -13.67306322407435815, 5.033750017361354523, -6.094185097971928755 ) ) ;
#29784 = CARTESIAN_POINT ( 'NONE',  ( -43.00000000000000000, 500.0000000000002274, 12.00000000000000711 ) ) ;
#29786 = EDGE_CURVE ( 'NONE', #73528, #88469, #3026, .T. ) ;
#29787 = CARTESIAN_POINT ( 'NONE',  ( -5.082755093536325042, -21.59375000204838457, -5.082755093536325930 ) ) ;
#29788 = CYLINDRICAL_SURFACE ( 'NONE', #11251, 4.000000000000000000 ) ;
#29789 = FACE_BOUND ( 'NONE', #46451, .T. ) ;
#29790 = ORIENTED_EDGE ( 'NONE', *, *, #44073, .F. ) ;
#29791 = EDGE_CURVE ( 'NONE', #39953, #60654, #44689, .T. ) ;
#29792 = DIRECTION ( 'NONE',  ( -1.000000000000000000, -1.224606353822377258E-16, -0.000000000000000000 ) ) ;
#29793 = CARTESIAN_POINT ( 'NONE',  ( -8.473474469330019687, 27.00279687854979827, -5.000000000000000000 ) ) ;
#29794 = PRESENTATION_LAYER_ASSIGNMENT (  '', '', ( #26349 ) ) ;
#29795 =( LENGTH_UNIT ( ) NAMED_UNIT ( * ) SI_UNIT ( .MILLI., .METRE. ) );
#29796 = CARTESIAN_POINT ( 'NONE',  ( 6.281178480976146616, 3.752776749732564809, 6.499999999999995559 ) ) ;
#29797 = ORIENTED_EDGE ( 'NONE', *, *, #102462, .T. ) ;
#29798 = DIRECTION ( 'NONE',  ( 0.000000000000000000, -1.000000000000000000, 0.000000000000000000 ) ) ;
#29799 = DIRECTION ( 'NONE',  ( 0.000000000000000000, 0.000000000000000000, 1.000000000000000000 ) ) ;
#29800 = CIRCLE ( 'NONE', #72786, 5.000000000000002665 ) ;
#29801 = EDGE_LOOP ( 'NONE', ( #24890, #64411, #95922, #76193 ) ) ;
#29802 = CARTESIAN_POINT ( 'NONE',  ( -27.73690841305016264, 34.52476796560765848, 7.681267181438511393 ) ) ;
#29803 =( NAMED_UNIT ( * ) PLANE_ANGLE_UNIT ( ) SI_UNIT ( $, .RADIAN. ) );
#29804 = SURFACE_SIDE_STYLE ('',( #64273 ) ) ;
#29805 = CARTESIAN_POINT ( 'NONE',  ( -17.83130206370017845, 36.70573752982816274, 22.40672895700082634 ) ) ;
#29806 = UNCERTAINTY_MEASURE_WITH_UNIT (LENGTH_MEASURE( 1.000000000000000082E-05 ), #47658, 'distance_accuracy_value', 'NONE');
#29807 = CARTESIAN_POINT ( 'NONE',  ( -98.84102348079841249, -59.99999999999999289, 202.1787051656507685 ) ) ;
#29808 = DIRECTION ( 'NONE',  ( 0.000000000000000000, -1.000000000000000000, 0.000000000000000000 ) ) ;
#29810 = AXIS2_PLACEMENT_3D ( 'NONE', #71889, #48134, #30943 ) ;
#29809 = CARTESIAN_POINT ( 'NONE',  ( 6.289692432696784685, 1.244853941008388061E-13, 6.828989928337166226 ) ) ;
#29811 = CARTESIAN_POINT ( 'NONE',  ( -4.284822031654912600, -48.90716638558775031, 104.4267991316945228 ) ) ;
#29812 = CARTESIAN_POINT ( 'NONE',  ( 16.75187969033515145, 34.25544727262118982, -24.30698433968624883 ) ) ;
#29813 = CARTESIAN_POINT ( 'NONE',  ( -85.51529951615857783, -28.66441007062391932, 177.8911255557245283 ) ) ;
#29814 = CARTESIAN_POINT ( 'NONE',  ( 25.69972685279896751, 43.60477215666053752, -75.16871690720786603 ) ) ;
#29815 = ORIENTED_EDGE ( 'NONE', *, *, #10972, .F. ) ;
#29816 = CARTESIAN_POINT ( 'NONE',  ( 4.472135954999578722, -65.00000000000000000, -4.000000000000002665 ) ) ;
#29817 = CARTESIAN_POINT ( 'NONE',  ( -82.42959359406624742, -37.82875958912266867, 13.21936520248347868 ) ) ;
#29818 = CARTESIAN_POINT ( 'NONE',  ( 0.000000000000000000, 0.9999999999999970024, 8.000000000000000000 ) ) ;
#29819 = CARTESIAN_POINT ( 'NONE',  ( -3.058374439072180095, 45.00124159115523526, -4.999999999999998224 ) ) ;
#29820 = CARTESIAN_POINT ( 'NONE',  ( 4.086459164113057874, 138.2893333910580509, -5.000000000000000000 ) ) ;
#29821 = CYLINDRICAL_SURFACE ( 'NONE', #18345, 35.82893434829263413 ) ;
#29822 = CARTESIAN_POINT ( 'NONE',  ( -30.67950393659633335, 18.64316884710269662, -23.57730434127810426 ) ) ;
#29823 = CARTESIAN_POINT ( 'NONE',  ( 101.7112553140276390, -14.21045842199441367, 195.4619641463733615 ) ) ;
#29824 = CARTESIAN_POINT ( 'NONE',  ( -7.420756919583589587E-15, 4.501353321498349658, 60.59507871780017751 ) ) ;
#29825 = EDGE_CURVE ( 'NONE', #88573, #31318, #67883, .T. ) ;
#29826 = CARTESIAN_POINT ( 'NONE',  ( -105.9103127569300966, -29.99999999999996092, 132.9890815309780123 ) ) ;
#29827 = CARTESIAN_POINT ( 'NONE',  ( -65.02951926827741147, -29.05579461752434511, 80.86596411567830955 ) ) ;
#29828 = ORIENTED_EDGE ( 'NONE', *, *, #106598, .F. ) ;
#29829 = CARTESIAN_POINT ( 'NONE',  ( 28.77268538114685015, 39.42481758554652060, 58.36079874883185425 ) ) ;
#29830 = CARTESIAN_POINT ( 'NONE',  ( 50.47126045336576539, -59.99999999997075406, 79.55909678837365107 ) ) ;
#29831 = VERTEX_POINT ( 'NONE', #22558 ) ;
#29832 = CARTESIAN_POINT ( 'NONE',  ( 32.61650669486618881, 1.474610560812782335E-15, 0.000000000000000000 ) ) ;
#29833 = CARTESIAN_POINT ( 'NONE',  ( 7.188101187499999156, -21.12500000204838813, 2.977408999572654924 ) ) ;
#29834 = CIRCLE ( 'NONE', #9071, 0.5000000000000004441 ) ;
#29835 = ORIENTED_EDGE ( 'NONE', *, *, #80933, .F. ) ;
#29836 = CARTESIAN_POINT ( 'NONE',  ( -11.27392099353256505, 45.76150927139936897, 13.37519430359083472 ) ) ;
#29837 = VERTEX_POINT ( 'NONE', #102374 ) ;
#29838 = CARTESIAN_POINT ( 'NONE',  ( 11.04556819181643768, 45.87714785467576917, -13.15211296974108635 ) ) ;
#29839 = CIRCLE ( 'NONE', #65920, 4.000000000000000000 ) ;
#29840 = CARTESIAN_POINT ( 'NONE',  ( 46.83368825528961565, 18.87956456981591202, -15.22947487995093496 ) ) ;
#29841 = CARTESIAN_POINT ( 'NONE',  ( -88.80181889419175434, -59.99999999999998579, -20.61832237384453492 ) ) ;
#29842 = CARTESIAN_POINT ( 'NONE',  ( 36.54310633446583978, 363.9539195057402594, 3.129522754832409603 ) ) ;
#29843 = CARTESIAN_POINT ( 'NONE',  ( -7.188101187500000044, -30.78125000204838813, -8.802885111219163269E-16 ) ) ;
#29844 = DIRECTION ( 'NONE',  ( -0.000000000000000000, 1.000000000000000000, 1.877893248421449282E-16 ) ) ;
#29845 = AXIS2_PLACEMENT_3D ( 'NONE', #546, #15178, #14628 ) ;
#29846 = CARTESIAN_POINT ( 'NONE',  ( -33.07276483573667747, 438.9325140356154975, 23.89537236861306013 ) ) ;
#29847 = CARTESIAN_POINT ( 'NONE',  ( -2.617478844988693432, 48.00000000000000000, -94.73972676610495114 ) ) ;
#29848 = ADVANCED_FACE ( 'NONE', ( #86748 ), #56429, .F. ) ;
#29849 = DIRECTION ( 'NONE',  ( 0.000000000000000000, 0.000000000000000000, 1.000000000000000000 ) ) ;
#29850 = CARTESIAN_POINT ( 'NONE',  ( -40.31555625028288148, 316.2223002904267446, 3.164403933231767052 ) ) ;
#29851 = CARTESIAN_POINT ( 'NONE',  ( 36.34421051467749209, 333.8189236619288067, -2.452241787315455390 ) ) ;
#29852 = ORIENTED_EDGE ( 'NONE', *, *, #2980, .T. ) ;
#29853 = CARTESIAN_POINT ( 'NONE',  ( 1.647285698089613781, 39.99999999999999289, -70.00000000000000000 ) ) ;
#29854 = TOROIDAL_SURFACE ( 'NONE', #102187, 74.46152422706630603, 60.00000000000000000 ) ;
#29855 = CARTESIAN_POINT ( 'NONE',  ( 34.21697539897928664, -53.36349323917029608, 37.55009111937090438 ) ) ;
#29856 = CARTESIAN_POINT ( 'NONE',  ( 21.65942590380180022, -2.602085213965209853E-15, -5.820808985962528936 ) ) ;
#29857 = ORIENTED_EDGE ( 'NONE', *, *, #36388, .F. ) ;
#29858 = CARTESIAN_POINT ( 'NONE',  ( 6.445370176742148516, -4.584736124524471101, 5.738941594275039471 ) ) ;
#29859 = ORIENTED_EDGE ( 'NONE', *, *, #661, .F. ) ;
#29861 = CARTESIAN_POINT ( 'NONE',  ( -20.24579557674108088, 304.8297271373347144, -10.00469232190996749 ) ) ;
#29860 = CARTESIAN_POINT ( 'NONE',  ( 7.711337099629008485, -4.999999999999998224, -15.67927777788488974 ) ) ;
#29862 = DIRECTION ( 'NONE',  ( 0.000000000000000000, 0.000000000000000000, -1.000000000000000000 ) ) ;
#29863 = LINE ( 'NONE', #104237, #82717 ) ;
#29864 = CARTESIAN_POINT ( 'NONE',  ( -43.00000000000000000, 436.0987441542287115, 7.567257455462743643 ) ) ;
#29865 = CARTESIAN_POINT ( 'NONE',  ( 4.472135954999579610, -85.00000000000000000, 4.000000000000001776 ) ) ;
#29866 = CARTESIAN_POINT ( 'NONE',  ( -4.846576637897429762, -47.10533319821855258, 42.76191327062164049 ) ) ;
#29867 = ORIENTED_EDGE ( 'NONE', *, *, #4626, .F. ) ;
#29868 = EDGE_CURVE ( 'NONE', #50026, #23499, #97784, .T. ) ;
#29869 = CARTESIAN_POINT ( 'NONE',  ( 91.96602543791587436, -60.00000000000001421, 6.905806405724360886 ) ) ;
#29870 = SURFACE_STYLE_FILL_AREA ( #13637 ) ;
#29871 = CARTESIAN_POINT ( 'NONE',  ( 23.73746414932995208, 5.000000000000003553, 0.000000000000000000 ) ) ;
#29872 = CIRCLE ( 'NONE', #90107, 1.000000000000016209 ) ;
#29873 = CIRCLE ( 'NONE', #50446, 63.00000000000000000 ) ;
#29874 = CARTESIAN_POINT ( 'NONE',  ( -4.852941176470602080, 40.00000000000033396, -70.80672828634229177 ) ) ;
#29875 = CARTESIAN_POINT ( 'NONE',  ( -13.72062045121628415, 20.42744233313543489, -6.730531604610976437 ) ) ;
#29876 = ORIENTED_EDGE ( 'NONE', *, *, #31053, .T. ) ;
#29877 = CARTESIAN_POINT ( 'NONE',  ( -81.70366676428112385, -30.00000000000000711, 144.0154804593513802 ) ) ;
#29878 = ORIENTED_EDGE ( 'NONE', *, *, #6996, .T. ) ;
#29879 = CARTESIAN_POINT ( 'NONE',  ( -9.609486011791419813, 143.0915023496522736, 0.000000000000000000 ) ) ;
#29880 = CARTESIAN_POINT ( 'NONE',  ( 14.45674127754722349, 21.77180424839734485, -4.838420908114524188 ) ) ;
#29881 = SURFACE_SIDE_STYLE ('',( #54626 ) ) ;
#29882 = CARTESIAN_POINT ( 'NONE',  ( 7.188101187500000044, -31.53125000204838457, 0.000000000000000000 ) ) ;
#29883 = FACE_OUTER_BOUND ( 'NONE', #24806, .T. ) ;
#29884 = SURFACE_SIDE_STYLE ('',( #21794 ) ) ;
#29885 = ORIENTED_EDGE ( 'NONE', *, *, #61904, .F. ) ;
#29887 = ORIENTED_EDGE ( 'NONE', *, *, #92312, .F. ) ;
#29886 = CARTESIAN_POINT ( 'NONE',  ( 0.000000000000000000, -78.00000000000000000, 27.00000000000000000 ) ) ;
#29888 = CARTESIAN_POINT ( 'NONE',  ( 78.42944077827469584, -32.55433236142065567, 130.6023639830650325 ) ) ;
#29889 = FACE_OUTER_BOUND ( 'NONE', #94389, .T. ) ;
#29890 = ORIENTED_EDGE ( 'NONE', *, *, #17342, .F. ) ;
#29891 = CARTESIAN_POINT ( 'NONE',  ( 19.83349330513380693, 4.898587196589411843E-16, -4.000000000000001776 ) ) ;
#29892 = CARTESIAN_POINT ( 'NONE',  ( 4.401442555609581635E-16, -21.78125000204838457, -7.188101187500000044 ) ) ;
#29893 = CARTESIAN_POINT ( 'NONE',  ( -99.73481241717010448, -57.62673548571369508, 203.9935789388791250 ) ) ;
#29894 = CARTESIAN_POINT ( 'NONE',  ( 13.81785577674642873, 302.5467234193154127, 9.872154563399625715 ) ) ;
#29895 = EDGE_LOOP ( 'NONE', ( #23463, #37123, #105013 ) ) ;
#29896 = DIRECTION ( 'NONE',  ( -0.000000000000000000, 1.000000000000000000, -0.000000000000000000 ) ) ;
#29897 = CARTESIAN_POINT ( 'NONE',  ( -4.503026011213026258, -10.54341862283317965, 3.965236350746919936 ) ) ;
#29898 = CARTESIAN_POINT ( 'NONE',  ( 6.831363830528337289, 41.73171983268898089, -59.17722554277374059 ) ) ;
#29899 = DIRECTION ( 'NONE',  ( -0.000000000000000000, -0.000000000000000000, 1.000000000000000000 ) ) ;
#29900 = CARTESIAN_POINT ( 'NONE',  ( 5.656854249492380582, -12.50000000409676915, -5.656854249492379694 ) ) ;
#29901 = CARTESIAN_POINT ( 'NONE',  ( -0.9091344387254992609, -12.57755568720529027, 32.18680658398173478 ) ) ;
#29902 = CARTESIAN_POINT ( 'NONE',  ( -36.31365659032788074, 26.07273513814342181, 12.06405704682174651 ) ) ;
#29903 = CARTESIAN_POINT ( 'NONE',  ( -46.00000000000000000, 488.3725375423296668, 3.127739281037490215 ) ) ;
#29904 = DIRECTION ( 'NONE',  ( -1.000000000000000000, -1.224606353822377258E-16, -0.000000000000000000 ) ) ;
#29905 = CARTESIAN_POINT ( 'NONE',  ( 5.656854249492380582, -19.81249999999999289, -5.656854249492379694 ) ) ;
#29906 = CIRCLE ( 'NONE', #497, 5.000000000000002665 ) ;
#29907 = DIRECTION ( 'NONE',  ( 0.000000000000000000, 0.000000000000000000, 1.000000000000000000 ) ) ;
#29908 = CARTESIAN_POINT ( 'NONE',  ( -9.989435848181784650, 33.97380292528427503, -0.5278651953176126677 ) ) ;
#29909 = ORIENTED_EDGE ( 'NONE', *, *, #18802, .F. ) ;
#29910 = PLANE ( 'NONE',  #49151 ) ;
#29911 = EDGE_CURVE ( 'NONE', #28086, #84887, #68562, .T. ) ;
#29912 = AXIS2_PLACEMENT_3D ( 'NONE', #79009, #78474, #6166 ) ;
#29913 = CARTESIAN_POINT ( 'NONE',  ( 42.98746414932995208, 6.123233995736772199E-16, -5.000000000000001776 ) ) ;
#29914 = CARTESIAN_POINT ( 'NONE',  ( 42.34475754208664000, -27.06717000920707861, -36.11866503128073447 ) ) ;
#29915 = CARTESIAN_POINT ( 'NONE',  ( -81.04018713825384168, -30.00000000000000711, 140.2278789465622140 ) ) ;
#29916 = EDGE_CURVE ( 'NONE', #9396, #102684, #84018, .T. ) ;
#29917 = CARTESIAN_POINT ( 'NONE',  ( 6.249999999999998224, 0.000000000000000000, 0.000000000000000000 ) ) ;
#29918 = ORIENTED_EDGE ( 'NONE', *, *, #75137, .T. ) ;
#29919 = CARTESIAN_POINT ( 'NONE',  ( -25.85382071165692253, 37.19470222756634570, -8.744493950090857837 ) ) ;
#29920 = AXIS2_PLACEMENT_3D ( 'NONE', #53073, #44453, #43913 ) ;
#29921 = CARTESIAN_POINT ( 'NONE',  ( 96.61421562474644986, -57.62226520396125551, 204.4765988090299800 ) ) ;
#29922 = CARTESIAN_POINT ( 'NONE',  ( 62.18148360307306888, -60.22838722633849073, -29.09035595218466952 ) ) ;
#29923 = CARTESIAN_POINT ( 'NONE',  ( -6.725979247667767780, -3.622307570260332454, -6.470294263593363127 ) ) ;
#29924 = CARTESIAN_POINT ( 'NONE',  ( -15.79067987436804188, 22.71383723441329394, 1.248691266770723285 ) ) ;
#29925 = CARTESIAN_POINT ( 'NONE',  ( 9.739726766683151737, -3.000000000000003109, -82.38252115640720774 ) ) ;
#29926 = CARTESIAN_POINT ( 'NONE',  ( -60.69885249676274697, -60.00000000000000711, 102.8462125076963360 ) ) ;
#29927 = ADVANCED_FACE ( 'NONE', ( #54869 ), #46272, .F. ) ;
#29928 = CARTESIAN_POINT ( 'NONE',  ( -5.589124336234561063, 4.278671059405865229, -6.219623095966342774 ) ) ;
#29929 = DIRECTION ( 'NONE',  ( 0.000000000000000000, -1.000000000000000000, 0.000000000000000000 ) ) ;
#29930 = CARTESIAN_POINT ( 'NONE',  ( 43.69716417795766006, 49.99999999997997691, 48.48761666245326296 ) ) ;
#29931 = CARTESIAN_POINT ( 'NONE',  ( -84.56126607524946337, -57.46072418158504291, 191.5362485997459885 ) ) ;
#29933 = ORIENTED_EDGE ( 'NONE', *, *, #49947, .F. ) ;
#29932 = PRESENTATION_LAYER_ASSIGNMENT (  '', '', ( #76401 ) ) ;
#29934 = CARTESIAN_POINT ( 'NONE',  ( 34.76497128141613047, 338.4643821587915227, -1.841863933405186282 ) ) ;
#29935 = CARTESIAN_POINT ( 'NONE',  ( 9.999999999999996447, 0.000000000000000000, -10.00000000000000000 ) ) ;
#29936 = CARTESIAN_POINT ( 'NONE',  ( -5.989969354119776490, 41.99624786690075950, -59.62337049591117477 ) ) ;
#29937 = CARTESIAN_POINT ( 'NONE',  ( 34.59893540551180990, 491.2022546151283109, 12.15065315885511765 ) ) ;
#29938 = CARTESIAN_POINT ( 'NONE',  ( 12.42907082493752569, -4.067133856148627657, -76.73301493501968196 ) ) ;
#29939 =( NAMED_UNIT ( * ) PLANE_ANGLE_UNIT ( ) SI_UNIT ( $, .RADIAN. ) );
#29940 = PRESENTATION_LAYER_ASSIGNMENT (  '', '', ( #33329 ) ) ;
#29941 = CARTESIAN_POINT ( 'NONE',  ( -82.62686422651856333, -45.26163198499813234, -15.10635754027111055 ) ) ;
#29942 = CARTESIAN_POINT ( 'NONE',  ( 0.000000000000000000, 6.123233995736770227E-16, -5.000000000000002665 ) ) ;
#29943 = CARTESIAN_POINT ( 'NONE',  ( 20.59999999999999787, 1.533819458162526451E-15, 0.000000000000000000 ) ) ;
#29944 = VECTOR ( 'NONE', #40599, 1000.000000000000000 ) ;
#29945 = ORIENTED_EDGE ( 'NONE', *, *, #7312, .T. ) ;
#29946 = FACE_OUTER_BOUND ( 'NONE', #105335, .T. ) ;
#29947 = CARTESIAN_POINT ( 'NONE',  ( 10.18660115262752086, 16.00273039107469941, 10.17531074053961682 ) ) ;
#29948 = CARTESIAN_POINT ( 'NONE',  ( -15.50035291838204721, -4.285714285714287364, -20.16952962162827845 ) ) ;
#29949 = CARTESIAN_POINT ( 'NONE',  ( -32.94021323899831799, 485.0599191339510980, 5.361609822536971492 ) ) ;
#29950 = EDGE_CURVE ( 'NONE', #74421, #4914, #59866, .T. ) ;
#29951 = CARTESIAN_POINT ( 'NONE',  ( 80.19743504398171297, -30.00000000000002487, -24.77996380036185187 ) ) ;
#29952 = CARTESIAN_POINT ( 'NONE',  ( -79.65043784881741828, -39.49985926501358335, 143.6092781588031642 ) ) ;
#29953 = ORIENTED_EDGE ( 'NONE', *, *, #24251, .T. ) ;
#29954 = CARTESIAN_POINT ( 'NONE',  ( 43.27459526351800179, 485.1620945307548141, -2.264801863435696561 ) ) ;
#29955 = CARTESIAN_POINT ( 'NONE',  ( -1.104211576045348808, -14.95094041744786040, -12.16229915940863116 ) ) ;
#29956 = CARTESIAN_POINT ( 'NONE',  ( 95.97031388804177254, -57.62154756878710771, 204.5181911369658394 ) ) ;
#29957 = CARTESIAN_POINT ( 'NONE',  ( 60.68787119177670064, 50.00000000000000000, 17.09822573326192696 ) ) ;
#29958 = CARTESIAN_POINT ( 'NONE',  ( 30.90190637651703653, 309.2317938240619810, -8.529668860358439630 ) ) ;
#29959 = FACE_OUTER_BOUND ( 'NONE', #53859, .T. ) ;
#29960 = VERTEX_POINT ( 'NONE', #79687 ) ;
#29961 = CARTESIAN_POINT ( 'NONE',  ( 9.797174393178825657E-16, -30.00000000000000000, -8.000000000000000000 ) ) ;
#29962 =( NAMED_UNIT ( * ) PLANE_ANGLE_UNIT ( ) SI_UNIT ( $, .RADIAN. ) );
#29963 = FACE_OUTER_BOUND ( 'NONE', #94187, .T. ) ;
#29964 = CARTESIAN_POINT ( 'NONE',  ( 5.082755093536324154, -23.84375000204838457, 5.082755093536326818 ) ) ;
#29965 = ORIENTED_EDGE ( 'NONE', *, *, #4714, .F. ) ;
#29966 = CARTESIAN_POINT ( 'NONE',  ( 9.165151389911681434, 30.00000000000000000, -4.000000000000000000 ) ) ;
#29967 = CARTESIAN_POINT ( 'NONE',  ( -8.000000000000001776, -23.65624999999999645, 3.313708498984759387 ) ) ;
#29968 = CARTESIAN_POINT ( 'NONE',  ( 0.000000000000000000, 44.84115912518001323, 0.000000000000000000 ) ) ;
#29969 = ADVANCED_FACE ( 'NONE', ( #55398 ), #38719, .F. ) ;
#29970 = ADVANCED_FACE ( 'NONE', ( #4747, #103439 ), #9364, .T. ) ;
#29971 = DIRECTION ( 'NONE',  ( -1.000000000000000000, -1.224606353822377258E-16, -0.000000000000000000 ) ) ;
#29972 = FACE_OUTER_BOUND ( 'NONE', #49211, .T. ) ;
#29973 = STYLED_ITEM ( 'NONE', ( #92811 ), #61612 ) ;
#29974 = CARTESIAN_POINT ( 'NONE',  ( 17.88147771104465988, 43.22047798057329260, -5.216096487390331049 ) ) ;
#29975 = ORIENTED_EDGE ( 'NONE', *, *, #2132, .T. ) ;
#29976 = CARTESIAN_POINT ( 'NONE',  ( -6.733158593834142280, 41.46658730094299017, -70.54360490943875561 ) ) ;
#29978 = CARTESIAN_POINT ( 'NONE',  ( 26.84979521222222587, -42.95598080738816549, 32.78234588387326198 ) ) ;
#29977 = CARTESIAN_POINT ( 'NONE',  ( -72.40149263128425616, -29.99999999999999289, 139.7559031367707405 ) ) ;
#29979 = CARTESIAN_POINT ( 'NONE',  ( 24.46206431567186002, 27.53832621860373209, -31.75666539158959623 ) ) ;
#29980 = ORIENTED_EDGE ( 'NONE', *, *, #8896, .F. ) ;
#29981 = UNCERTAINTY_MEASURE_WITH_UNIT (LENGTH_MEASURE( 1.000000000000000082E-05 ), #67456, 'distance_accuracy_value', 'NONE');
#29982 = ORIENTED_EDGE ( 'NONE', *, *, #101587, .F. ) ;
#29983 = PRESENTATION_STYLE_ASSIGNMENT (( #37560 ) ) ;
#29984 = CYLINDRICAL_SURFACE ( 'NONE', #49093, 5.000000000000002665 ) ;
#29985 = FACE_OUTER_BOUND ( 'NONE', #6042, .T. ) ;
#29986 = CARTESIAN_POINT ( 'NONE',  ( 4.010857135589731489E-16, 21.85270131633359014, 7.000000000000016875 ) ) ;
#29987 = CARTESIAN_POINT ( 'NONE',  ( -7.500000000000000888, 3.639598441879738910, -0.7155132341745207292 ) ) ;
#29988 = ORIENTED_EDGE ( 'NONE', *, *, #61904, .T. ) ;
#29989 = EDGE_CURVE ( 'NONE', #32781, #34804, #88127, .T. ) ;
#29990 = DIRECTION ( 'NONE',  ( 1.000000000000000000, 0.000000000000000000, 0.000000000000000000 ) ) ;
#29991 = CARTESIAN_POINT ( 'NONE',  ( 87.60795424214978766, -30.00000000000000000, 185.8138595367513233 ) ) ;
#29992 = CARTESIAN_POINT ( 'NONE',  ( -13.54312819440545113, 24.68321509063727248, 1.318894457162179235 ) ) ;
#29993 = CONICAL_SURFACE ( 'NONE', #59226, 5.000000000000001776, 0.9599310885968803664 ) ;
#29994 = CARTESIAN_POINT ( 'NONE',  ( 4.154708322984369194E-08, -57.67120202538961138, 41.61186700422869933 ) ) ;
#29995 = CARTESIAN_POINT ( 'NONE',  ( 77.19385768473838993, -30.00000000000000355, -16.50491056378216115 ) ) ;
#29996 = CIRCLE ( 'NONE', #104018, 2.999999999999999112 ) ;
#29997 = EDGE_CURVE ( 'NONE', #97524, #76274, #32387, .T. ) ;
#29998 = DIRECTION ( 'NONE',  ( 0.000000000000000000, -1.000000000000000000, 0.000000000000000000 ) ) ;
#29999 = EDGE_LOOP ( 'NONE', ( #23988, #73292, #59447, #61387, #35532 ) ) ;
#30000 = VERTEX_POINT ( 'NONE', #17502 ) ;
#30001 = ORIENTED_EDGE ( 'NONE', *, *, #17288, .F. ) ;
#30002 = CARTESIAN_POINT ( 'NONE',  ( 74.07777777777778283, -3.309500000000000774, 0.000000000000000000 ) ) ;
#30003 = LINE ( 'NONE', #37044, #98254 ) ;
#30004 = CARTESIAN_POINT ( 'NONE',  ( 33.70427618943720205, 490.4072845429053018, 11.54254722977849745 ) ) ;
#30005 =( LENGTH_UNIT ( ) NAMED_UNIT ( * ) SI_UNIT ( .MILLI., .METRE. ) );
#30006 = EDGE_CURVE ( 'NONE', #105730, #8358, #74640, .T. ) ;
#30007 = CARTESIAN_POINT ( 'NONE',  ( -6.943926999490791729, -85.53300992626148513, -3.973092371898547803 ) ) ;
#30008 = DIRECTION ( 'NONE',  ( 0.000000000000000000, -1.000000000000000000, 0.000000000000000000 ) ) ;
#30009 = EDGE_LOOP ( 'NONE', ( #29181, #23456, #7233, #19289 ) ) ;
#30010 = CARTESIAN_POINT ( 'NONE',  ( 29.77450884433743639, 8.177050405881830741, 42.10535821593491335 ) ) ;
#30011 = ORIENTED_EDGE ( 'NONE', *, *, #75288, .T. ) ;
#30012 = LINE ( 'NONE', #88753, #70822 ) ;
#30013 = CARTESIAN_POINT ( 'NONE',  ( 60.37731204512586913, -38.34250980313896662, 97.59513848696614957 ) ) ;
#30014 = CARTESIAN_POINT ( 'NONE',  ( -39.65839090363253661, 485.8593493675159039, -5.004208577436008554 ) ) ;
#30015 = ADVANCED_FACE ( 'NONE', ( #105037 ), #77089, .F. ) ;
#30016 = CARTESIAN_POINT ( 'NONE',  ( 6.562934840145641324, -4.277581483015143959, -6.282640795011894319 ) ) ;
#30017 = CARTESIAN_POINT ( 'NONE',  ( 65.00163223881457952, -18.62600959983467774, 75.47887303634519185 ) ) ;
#30018 = ORIENTED_EDGE ( 'NONE', *, *, #5663, .T. ) ;
#30019 = CARTESIAN_POINT ( 'NONE',  ( -7.251642494156320673, 41.54835750584366849, -68.91429205799529711 ) ) ;
#30020 = CARTESIAN_POINT ( 'NONE',  ( -55.88663790324028469, -36.71134587742232469, -35.08381123762609377 ) ) ;
#30021 = CARTESIAN_POINT ( 'NONE',  ( -6.999814028509885766, 9.000325450264105243, -0.2742116757349308265 ) ) ;
#30022 = CIRCLE ( 'NONE', #90267, 5.000000000000011546 ) ;
#30023 = CARTESIAN_POINT ( 'NONE',  ( 29.98176661990081371, 6.123233995736770227E-16, -5.000000000000002665 ) ) ;
#30025 = ORIENTED_EDGE ( 'NONE', *, *, #29456, .F. ) ;
#30024 = CIRCLE ( 'NONE', #4140, 4.000000000000000888 ) ;
#30026 = SURFACE_SIDE_STYLE ('',( #45663 ) ) ;
#30027 = CARTESIAN_POINT ( 'NONE',  ( 0.000000000000000000, 0.000000000000000000, 0.000000000000000000 ) ) ;
#30028 = CARTESIAN_POINT ( 'NONE',  ( -2.857580275982106954, -59.99999999999997868, -36.86911833281171624 ) ) ;
#30029 = CARTESIAN_POINT ( 'NONE',  ( 67.22793774957824553, 4.000000000000014211, 0.000000000000000000 ) ) ;
#30030 = CARTESIAN_POINT ( 'NONE',  ( -8.000000000000001776, -29.84375000409677270, 3.313708498984758943 ) ) ;
#30031 = CARTESIAN_POINT ( 'NONE',  ( 0.9108756637677339896, 6.979659189795291319, -6.219623095965904902 ) ) ;
#30032 = CARTESIAN_POINT ( 'NONE',  ( 86.88686737857604214, -39.10008494188175376, 188.8693110577609957 ) ) ;
#30033 = CARTESIAN_POINT ( 'NONE',  ( 89.99999999999997158, -60.00000000000000000, 196.0238439516549818 ) ) ;
#30034 = CARTESIAN_POINT ( 'NONE',  ( -3.833148349061555216, 18.02117837737563377, 4.999999999999999112 ) ) ;
#30035 = CARTESIAN_POINT ( 'NONE',  ( -0.5620262070071395666, 7.564407249984303583, -6.443844059477449981 ) ) ;
#30036 = CARTESIAN_POINT ( 'NONE',  ( 24.87981348507249990, -20.00187728542004706, -33.03831867686129442 ) ) ;
#30037 = CARTESIAN_POINT ( 'NONE',  ( 18.15174345153223712, 304.6383688000003076, 8.891572165220576807 ) ) ;
#30038 = ORIENTED_EDGE ( 'NONE', *, *, #95678, .T. ) ;
#30039 = LINE ( 'NONE', #20394, #80012 ) ;
#30040 = CARTESIAN_POINT ( 'NONE',  ( 34.89266211578681975, 436.0682616543206223, 7.611940783812184641 ) ) ;
#30041 = CARTESIAN_POINT ( 'NONE',  ( -100.3779187766488405, -30.00000000000000355, 157.7784893630589522 ) ) ;
#30042 = ADVANCED_FACE ( 'NONE', ( #66030 ), #4801, .T. ) ;
#30043 = STYLED_ITEM ( 'NONE', ( #42690 ), #62053 ) ;
#30044 = CARTESIAN_POINT ( 'NONE',  ( -32.15963082908692172, 464.7082849654399865, 10.94047064224899835 ) ) ;
#30045 = CARTESIAN_POINT ( 'NONE',  ( 40.77881392998116183, -57.69042326476748883, 56.97214866716775106 ) ) ;
#30046 = EDGE_CURVE ( 'NONE', #75387, #7582, #43034, .T. ) ;
#30048 = CARTESIAN_POINT ( 'NONE',  ( 43.50250715914180688, 464.6389613228375310, 9.611700240007991169 ) ) ;
#30047 = CARTESIAN_POINT ( 'NONE',  ( 9.645652298885325493, 44.08758678901953942, 13.07143836443655616 ) ) ;
#30049 = CARTESIAN_POINT ( 'NONE',  ( -42.23079339798738374, 460.7352525929354101, 2.726051457480726636 ) ) ;
#30050 = CARTESIAN_POINT ( 'NONE',  ( -18.04869413793490551, 50.00000000000000711, 61.82439970906034432 ) ) ;
#30051 = CARTESIAN_POINT ( 'NONE',  ( -41.50820411079202188, 461.5963371455320612, 2.703439750996428081 ) ) ;
#30052 = AXIS2_PLACEMENT_3D ( 'NONE', #51470, #84915, #84385 ) ;
#30053 = CARTESIAN_POINT ( 'NONE',  ( 46.00000000000000000, 486.4340384878591408, 3.748479173862500513 ) ) ;
#30054 = CONICAL_SURFACE ( 'NONE', #9298, 3.309500000000007880, 0.9599310885968770357 ) ;
#30055 = CARTESIAN_POINT ( 'NONE',  ( 13.58349330513380160, 1.593028355512270567E-15, 0.000000000000000000 ) ) ;
#30056 = DIRECTION ( 'NONE',  ( 8.355988613032100413E-17, 0.7310552682428690385, -0.6823182503600110360 ) ) ;
#30057 = VECTOR ( 'NONE', #7881, 1000.000000000000000 ) ;
#30058 = SURFACE_STYLE_USAGE ( .BOTH. , #78570 ) ;
#30059 = ORIENTED_EDGE ( 'NONE', *, *, #11543, .T. ) ;
#30060 = CARTESIAN_POINT ( 'NONE',  ( 38.81358894280344884, 485.1131561813197095, -4.191378885297267765 ) ) ;
#30061 = CARTESIAN_POINT ( 'NONE',  ( -1.458873328850117668, -49.96632135588456691, 101.6361877027969740 ) ) ;
#30062 = CARTESIAN_POINT ( 'NONE',  ( -13.56997494041515218, -46.43935299279289808, 31.71586160483574091 ) ) ;
#30063 =( BOUNDED_SURFACE ( )  B_SPLINE_SURFACE ( 3, 2, ( 
 ( #10658, #44113, #61368 ),
 ( #68933, #43573, #17714 ),
 ( #101807, #77540, #11718 ),
 ( #27972, #44657, #50575 ),
 ( #83492, #84034, #67850 ),
 ( #76460, #9591, #34462 ),
 ( #100212, #59240, #10137 ),
 ( #43051, #104454, #70514 ),
 ( #22520, #103404, #30602 ),
 ( #63492, #103923, #12784 ),
 ( #4180, #55363, #20953 ),
 ( #96390, #46757, #102878 ),
 ( #21979, #62428, #30070 ),
 ( #53784, #88292, #71032 ),
 ( #14367, #47276, #95318 ),
 ( #79122, #87762, #79651 ),
 ( #5248, #62953, #61912 ),
 ( #53267, #6278, #29557 ),
 ( #94804, #37653, #95849 ),
 ( #54834, #46237, #80174 ) ),
 .UNSPECIFIED., .F., .F., .T. ) 
 B_SPLINE_SURFACE_WITH_KNOTS ( ( 4, 2, 2, 2, 2, 2, 2, 2, 2, 4 ),
 ( 3, 3 ),
 ( 0.001112359326668568328, 0.002061628542468994449, 0.003010897758269421003, 0.003960166974069847558, 0.004909436189870273679, 0.005858705405670700667, 0.006807974621471126787, 0.007282609229371340281, 0.007757243837271552908, 0.008706513053071979896 ),
 ( 0.000000000000000000, 1.000000000000000000 ),
 .UNSPECIFIED. ) 
 GEOMETRIC_REPRESENTATION_ITEM ( )  RATIONAL_B_SPLINE_SURFACE ( (
 ( 1.000000000000000000, 0.9115707425106703843, 1.000000000000000000),
 ( 1.000000000000000000, 0.9186010707723997193, 1.000000000000000000),
 ( 1.000000000000000000, 0.9248333139228899213, 1.000000000000000000),
 ( 1.000000000000000000, 0.9351156329914673826, 1.000000000000000000),
 ( 1.000000000000000000, 0.9392288573273753771, 1.000000000000000000),
 ( 1.000000000000000000, 0.9457209207428006748, 1.000000000000000000),
 ( 1.000000000000000000, 0.9480998420262755078, 1.000000000000000000),
 ( 1.000000000000000000, 0.9511999291517022614, 1.000000000000000000),
 ( 1.000000000000000000, 0.9519548416862092521, 1.000000000000000000),
 ( 1.000000000000000000, 0.9519314736513960762, 1.000000000000000000),
 ( 1.000000000000000000, 0.9511539719351175259, 1.000000000000000000),
 ( 1.000000000000000000, 0.9480480161104184456, 1.000000000000000000),
 ( 1.000000000000000000, 0.9457194361327755372, 1.000000000000000000),
 ( 1.000000000000000000, 0.9408176163900222599, 1.000000000000000000),
 ( 1.000000000000000000, 0.9389456878146280605, 1.000000000000000000),
 ( 1.000000000000000000, 0.9347647373046783503, 1.000000000000000000),
 ( 1.000000000000000000, 0.9324473665774060116, 1.000000000000000000),
 ( 1.000000000000000000, 0.9247734139713987833, 1.000000000000000000),
 ( 1.000000000000000000, 0.9186884142194181591, 1.000000000000000000),
 ( 1.000000000000000000, 0.9115707425106747142, 1.000000000000000000) ) ) 
 REPRESENTATION_ITEM ( '' )  SURFACE ( )  );
#30065 = CARTESIAN_POINT ( 'NONE',  ( -34.00007050920425655, 439.9158767981585356, 24.30698066181913575 ) ) ;
#30064 = CARTESIAN_POINT ( 'NONE',  ( -87.36849624350148247, -59.99999999999996447, 33.81939915725044443 ) ) ;
#30066 = ORIENTED_EDGE ( 'NONE', *, *, #49768, .T. ) ;
#30067 = LINE ( 'NONE', #14899, #104083 ) ;
#30068 = CARTESIAN_POINT ( 'NONE',  ( 16.14595037822608958, 7.274337365584599091, -6.616591826375524121 ) ) ;
#30069 = CARTESIAN_POINT ( 'NONE',  ( -13.43456000506750847, 42.84369539968772500, -92.03053355450553852 ) ) ;
#30070 = CARTESIAN_POINT ( 'NONE',  ( 16.01731991787289999, 3.900165755866083828, -1.616345057638605143 ) ) ;
#30071 = CARTESIAN_POINT ( 'NONE',  ( 73.84586213920505315, -60.00000000000001421, 170.6559303522170694 ) ) ;
#30072 = EDGE_CURVE ( 'NONE', #35442, #69405, #571, .T. ) ;
#30073 = LINE ( 'NONE', #95320, #32024 ) ;
#30074 = ORIENTED_EDGE ( 'NONE', *, *, #10619, .T. ) ;
#30076 = CARTESIAN_POINT ( 'NONE',  ( 22.33349330513380337, 1.593028355512270567E-15, 0.000000000000000000 ) ) ;
#30075 = CARTESIAN_POINT ( 'NONE',  ( 38.21924934408536245, -34.43263479671050220, 36.26631857391012659 ) ) ;
#30077 = LINE ( 'NONE', #52324, #40641 ) ;
#30078 = ORIENTED_EDGE ( 'NONE', *, *, #3341, .T. ) ;
#30079 = ORIENTED_EDGE ( 'NONE', *, *, #12100, .F. ) ;
#30080 = CARTESIAN_POINT ( 'NONE',  ( -26.49347172118876514, 310.1936227282963046, 10.20217970970264609 ) ) ;
#30081 = ORIENTED_EDGE ( 'NONE', *, *, #89092, .F. ) ;
#30082 = SURFACE_STYLE_FILL_AREA ( #71565 ) ;
#30083 = CARTESIAN_POINT ( 'NONE',  ( 7.999999999999998224, -14.28125000409677092, 3.313708498984766049 ) ) ;
#30084 = FILL_AREA_STYLE ('',( #80190 ) ) ;
#30086 = EDGE_CURVE ( 'NONE', #30344, #3187, #21293, .T. ) ;
#30085 = EDGE_LOOP ( 'NONE', ( #31573, #250, #16311, #54199 ) ) ;
#30087 = PRESENTATION_LAYER_ASSIGNMENT (  '', '', ( #763 ) ) ;
#30088 =( NAMED_UNIT ( * ) PLANE_ANGLE_UNIT ( ) SI_UNIT ( $, .RADIAN. ) );
#30089 = CARTESIAN_POINT ( 'NONE',  ( -5.787480046464959393, 41.99999999999999289, -68.91429205815936143 ) ) ;
#30090 = VECTOR ( 'NONE', #103484, 1000.000000000000000 ) ;
#30091 = CARTESIAN_POINT ( 'NONE',  ( -87.01069910675980168, -60.00000000000727596, 203.6540258465300894 ) ) ;
#30092 = CARTESIAN_POINT ( 'NONE',  ( 6.287679341995269233, -1.331405739683436007, -6.828854810278214948 ) ) ;
#30093 = CARTESIAN_POINT ( 'NONE',  ( 90.24307525190243950, -60.00000000000001421, 202.0291797872075676 ) ) ;
#30094 = CARTESIAN_POINT ( 'NONE',  ( -1.663454779230262526, -5.000000000000002665, 16.34255157462185792 ) ) ;
#30095 = CARTESIAN_POINT ( 'NONE',  ( -6.592761362570266570, 41.57274138842281985, -58.68933574041189161 ) ) ;
#30097 = CARTESIAN_POINT ( 'NONE',  ( 9.217361846978604945, -39.47265868016614121, 30.47086924679750908 ) ) ;
#30096 = CARTESIAN_POINT ( 'NONE',  ( -108.2372990039095271, -60.00000000000000000, 115.4700740038245499 ) ) ;
#30098 = CARTESIAN_POINT ( 'NONE',  ( -49.54250463381430336, -25.66846576903583355, 45.52667409298107515 ) ) ;
#30099 = CARTESIAN_POINT ( 'NONE',  ( -3.782179052920016105, 19.16134848367324039, 5.890440751236702077 ) ) ;
#30100 = B_SPLINE_CURVE_WITH_KNOTS ( 'NONE', 3,
 ( #73156, #706, #17488, #33679, #31683, #30627 ),
 .UNSPECIFIED., .F., .F.,
 ( 4, 2, 4 ),
 ( -4.698498716302814272E-06, 0.0003457374136927988083, 0.0006961733261019004918 ),
 .UNSPECIFIED. ) ;
#30101 = ORIENTED_EDGE ( 'NONE', *, *, #82391, .T. ) ;
#30102 = CARTESIAN_POINT ( 'NONE',  ( 17.81438722625302518, 3.851859888774471706E-31, 5.000000000000001776 ) ) ;
#30103 = CARTESIAN_POINT ( 'NONE',  ( 17.97938082339186749, 36.40366709787542732, 23.34517568653148345 ) ) ;
#30104 = VERTEX_POINT ( 'NONE', #60100 ) ;
#30105 = CARTESIAN_POINT ( 'NONE',  ( -7.553239908583639028, -6.016880836006652800, 14.04797252150881981 ) ) ;
#30106 = ORIENTED_EDGE ( 'NONE', *, *, #34154, .F. ) ;
#30107 = CARTESIAN_POINT ( 'NONE',  ( 82.01977462800290652, -29.99999999997359623, 194.2710566929856952 ) ) ;
#30108 = CARTESIAN_POINT ( 'NONE',  ( 5.448357755207406505, 41.97585525106359228, -59.38396075874230462 ) ) ;
#30109 = CARTESIAN_POINT ( 'NONE',  ( -24.33159596665262470, 34.19642918197134662, 12.16579798332631768 ) ) ;
#30110 = CARTESIAN_POINT ( 'NONE',  ( 97.07539879229518931, -30.00000000000000000, 191.0633822395669768 ) ) ;
#30111 = ADVANCED_FACE ( 'NONE', ( #19127 ), #37566, .T. ) ;
#30112 = FACE_OUTER_BOUND ( 'NONE', #829, .T. ) ;
#30113 = ORIENTED_EDGE ( 'NONE', *, *, #90756, .F. ) ;
#30114 = CIRCLE ( 'NONE', #16301, 35.82893434829263413 ) ;
#30115 = ORIENTED_EDGE ( 'NONE', *, *, #3275, .F. ) ;
#30116 = ORIENTED_EDGE ( 'NONE', *, *, #2942, .T. ) ;
#30117 = DIRECTION ( 'NONE',  ( -0.000000000000000000, -1.000000000000000000, -0.000000000000000000 ) ) ;
#30118 = CARTESIAN_POINT ( 'NONE',  ( -46.00000000000000000, 438.4646224975035125, 9.895601460523737458 ) ) ;
#30119 = EDGE_CURVE ( 'NONE', #55315, #86295, #93281, .T. ) ;
#30120 = CARTESIAN_POINT ( 'NONE',  ( -45.99999999999998579, 461.2896359780384614, 8.857952602228083450 ) ) ;
#30121 = EDGE_CURVE ( 'NONE', #69327, #86608, #35871, .T. ) ;
#30122 = ORIENTED_EDGE ( 'NONE', *, *, #39704, .T. ) ;
#30123 = CARTESIAN_POINT ( 'NONE',  ( 0.000000000000000000, 0.000000000000000000, 0.000000000000000000 ) ) ;
#30124 = ORIENTED_EDGE ( 'NONE', *, *, #6996, .F. ) ;
#30125 = CARTESIAN_POINT ( 'NONE',  ( -42.99999999999847944, 487.1237704758270866, 9.497510897114741724 ) ) ;
#30126 = CARTESIAN_POINT ( 'NONE',  ( 102.8743298759455911, -38.42936654585968625, 199.1928420204874044 ) ) ;
#30127 = CARTESIAN_POINT ( 'NONE',  ( 15.05475665200631497, 5.402209584884851701, 6.523587638318953275 ) ) ;
#30128 = AXIS2_PLACEMENT_3D ( 'NONE', #90679, #16788, #49675 ) ;
#30129 = CARTESIAN_POINT ( 'NONE',  ( 86.27400346893527683, -60.13093677512101465, 5.975714098585993561 ) ) ;
#30130 = LINE ( 'NONE', #63017, #20138 ) ;
#30131 = AXIS2_PLACEMENT_3D ( 'NONE', #26665, #92412, #43871 ) ;
#30132 = CARTESIAN_POINT ( 'NONE',  ( 40.74486364038580888, 360.0828261927184144, 24.30144178707762848 ) ) ;
#30133 =( REPRESENTATION_RELATIONSHIP ('NONE','NONE', #69581, #44072 ) REPRESENTATION_RELATIONSHIP_WITH_TRANSFORMATION ( #86951 )SHAPE_REPRESENTATION_RELATIONSHIP( ) );
#30134 = AXIS2_PLACEMENT_3D ( 'NONE', #86619, #4615, #12682 ) ;
#30135 = CARTESIAN_POINT ( 'NONE',  ( 7.922281120364393914, 4.573931137438267847, -8.047472243342932430 ) ) ;
#30136 = VECTOR ( 'NONE', #8526, 1000.000000000000000 ) ;
#30137 = ADVANCED_FACE ( 'NONE', ( #56186 ), #39525, .F. ) ;
#30138 = AXIS2_PLACEMENT_3D ( 'NONE', #104938, #80110, #87696 ) ;
#30139 = CARTESIAN_POINT ( 'NONE',  ( -38.98764044588113364, 460.2978347093127809, 2.283752696491721856 ) ) ;
#30140 = CARTESIAN_POINT ( 'NONE',  ( 9.609486011791425142, 143.0915023496523304, 0.000000000000000000 ) ) ;
#30141 = ORIENTED_EDGE ( 'NONE', *, *, #592, .T. ) ;
#30142 = CYLINDRICAL_SURFACE ( 'NONE', #11748, 65.00000000000000000 ) ;
#30143 = CARTESIAN_POINT ( 'NONE',  ( -35.41620593328612188, 462.9429453004491961, 4.226634750751853353 ) ) ;
#30144 = CARTESIAN_POINT ( 'NONE',  ( -4.075111592545596295, 138.1305188241016424, 4.999999999999999112 ) ) ;
#30145 = ORIENTED_EDGE ( 'NONE', *, *, #72484, .F. ) ;
#30146 = FACE_OUTER_BOUND ( 'NONE', #98000, .T. ) ;
#30147 = CARTESIAN_POINT ( 'NONE',  ( -33.80382396800512623, 301.4638900151607572, 3.437251938379645821 ) ) ;
#30148 = CARTESIAN_POINT ( 'NONE',  ( -4.284822031654912600, -48.90716638558775031, 104.4267991316945228 ) ) ;
#30149 = CARTESIAN_POINT ( 'NONE',  ( 5.656854249492380582, -12.31249999999999289, -5.656854249492379694 ) ) ;
#30150 = CARTESIAN_POINT ( 'NONE',  ( -44.47534256803319153, -38.31161230092084224, 57.00189278798913506 ) ) ;
#30151 = DIRECTION ( 'NONE',  ( 0.000000000000000000, -1.000000000000000000, 0.000000000000000000 ) ) ;
#30152 = ORIENTED_EDGE ( 'NONE', *, *, #73393, .F. ) ;
#30153 = CARTESIAN_POINT ( 'NONE',  ( 85.23043926280386984, -39.32506677273280360, 184.5449207610389237 ) ) ;
#30154 = B_SPLINE_CURVE_WITH_KNOTS ( 'NONE', 3,
 ( #64767, #32953, #7048, #106262, #97124, #57183, #104688, #23264, #96610, #14595, #65822, #41021 ),
 .UNSPECIFIED., .F., .F.,
 ( 4, 2, 2, 2, 2, 4 ),
 ( 0.000000000000000000, 0.0008138854558913282463, 0.001220828183837001151, 0.001627770911782673840, 0.002441656367674002303, 0.003255541823565330332 ),
 .UNSPECIFIED. ) ;
#30155 = CARTESIAN_POINT ( 'NONE',  ( 6.683837171061806970, -7.911893696991936231, 5.688671339918660213E-17 ) ) ;
#30156 = VERTEX_POINT ( 'NONE', #13092 ) ;
#30157 = CARTESIAN_POINT ( 'NONE',  ( 94.16631605059897936, -57.67261574475512731, 22.14266882980151507 ) ) ;
#30158 = DIRECTION ( 'NONE',  ( 0.000000000000000000, -1.000000000000000000, 0.000000000000000000 ) ) ;
#30159 = CARTESIAN_POINT ( 'NONE',  ( 12.71180608318734251, -4.333298119783789204, 12.63015221159040991 ) ) ;
#30160 = CARTESIAN_POINT ( 'NONE',  ( 29.33008799483377871, 13.53038725678830367, 39.65490270819991281 ) ) ;
#30161 = ADVANCED_FACE ( 'NONE', ( #6064 ), #73685, .F. ) ;
#30162 = CARTESIAN_POINT ( 'NONE',  ( 51.88291765283383938, 283.6183258647156435, 267.1969486012856692 ) ) ;
#30163 = DIRECTION ( 'NONE',  ( -1.000000000000000000, -1.224606353822377258E-16, -0.000000000000000000 ) ) ;
#30164 = DIRECTION ( 'NONE',  ( 0.000000000000000000, 0.000000000000000000, -1.000000000000000000 ) ) ;
#30165 = CARTESIAN_POINT ( 'NONE',  ( 43.34668154757743963, -27.69613747131105796, 38.46247136646560705 ) ) ;
#30166 = ADVANCED_FACE ( 'NONE', ( #54078 ), #6477, .F. ) ;
#30168 = CARTESIAN_POINT ( 'NONE',  ( -10.89906287216224534, 8.997476634352441494, 10.00979493832057088 ) ) ;
#30167 = SURFACE_SIDE_STYLE ('',( #104024 ) ) ;
#30169 = CARTESIAN_POINT ( 'NONE',  ( 48.02835407290503866, 11.61227450977245468, -14.35535821593549954 ) ) ;
#30170 = CARTESIAN_POINT ( 'NONE',  ( 9.910377230549942240, 15.23810023151299653, -1.510421413154837245 ) ) ;
#30171 = CARTESIAN_POINT ( 'NONE',  ( 53.78349330513380266, -4.000000000000000000, 4.898587196589421703E-16 ) ) ;
#30172 = CARTESIAN_POINT ( 'NONE',  ( -82.66276222626812853, -38.00000000000004974, 21.06924847054219541 ) ) ;
#30173 = ORIENTED_EDGE ( 'NONE', *, *, #97914, .T. ) ;
#30174 = CARTESIAN_POINT ( 'NONE',  ( -10.31289488289771406, 2.633976217239669904, 14.76805301559119954 ) ) ;
#30175 = CARTESIAN_POINT ( 'NONE',  ( 7.960204194457797252E-15, 0.000000000000000000, -65.00000000000000000 ) ) ;
#30176 = DIRECTION ( 'NONE',  ( 0.000000000000000000, -1.000000000000000000, 0.000000000000000000 ) ) ;
#30178 = CARTESIAN_POINT ( 'NONE',  ( -38.30773932209359600, -47.40885879408931913, -31.93446002179309318 ) ) ;
#30177 = CARTESIAN_POINT ( 'NONE',  ( 32.61650669486618881, 1.474610560812782335E-15, 0.000000000000000000 ) ) ;
#30179 = EDGE_CURVE ( 'NONE', #72871, #457, #58521, .T. ) ;
#30180 = PRESENTATION_LAYER_ASSIGNMENT (  '', '', ( #9518 ) ) ;
#30181 = VERTEX_POINT ( 'NONE', #30379 ) ;
#30182 = CARTESIAN_POINT ( 'NONE',  ( 20.00100000000000122, 12.99999999999999289, 0.000000000000000000 ) ) ;
#30183 = ORIENTED_EDGE ( 'NONE', *, *, #42972, .T. ) ;
#30184 = CIRCLE ( 'NONE', #73186, 62.00000000000000000 ) ;
#30185 = CARTESIAN_POINT ( 'NONE',  ( 29.77394335381455903, 8.177826981235266857, -42.10535821593531125 ) ) ;
#30186 = DIRECTION ( 'NONE',  ( -1.000000000000000000, -1.224606353822377258E-16, -0.000000000000000000 ) ) ;
#30187 = STYLED_ITEM ( 'NONE', ( #65734 ), #88186 ) ;
#30188 = CARTESIAN_POINT ( 'NONE',  ( -91.92679597868495023, -60.00000000000000711, -14.22741696697412017 ) ) ;
#30189 = ORIENTED_EDGE ( 'NONE', *, *, #6869, .F. ) ;
#30190 = CARTESIAN_POINT ( 'NONE',  ( -6.459123244420534427, 42.00000000000000000, -59.79223455627018780 ) ) ;
#30191 = VECTOR ( 'NONE', #32218, 1000.000000000000000 ) ;
#30192 = PRESENTATION_STYLE_ASSIGNMENT (( #23701 ) ) ;
#30193 = VECTOR ( 'NONE', #26513, 1000.000000000000000 ) ;
#30194 = CARTESIAN_POINT ( 'NONE',  ( -9.165151389911684987, 29.73289218717087223, -4.000000000000000888 ) ) ;
#30195 = AXIS2_PLACEMENT_3D ( 'NONE', #44514, #86586, #59639 ) ;
#30197 = CARTESIAN_POINT ( 'NONE',  ( 27.02022815836235026, -5.000000000000000000, 0.000000000000000000 ) ) ;
#30196 = CARTESIAN_POINT ( 'NONE',  ( 88.20199406385988539, 1.030564683017419500E-14, 0.000000000000000000 ) ) ;
#30198 = CARTESIAN_POINT ( 'NONE',  ( -83.21178524358640516, -29.08282875446304772, 155.6723645619419472 ) ) ;
#30199 = ORIENTED_EDGE ( 'NONE', *, *, #105092, .T. ) ;
#30200 = CIRCLE ( 'NONE', #88704, 4.000000000000001776 ) ;
#30201 = CARTESIAN_POINT ( 'NONE',  ( -14.76969908562827349, 0.000000000000000000, 8.521411446768476949 ) ) ;
#30202 = ORIENTED_EDGE ( 'NONE', *, *, #56646, .F. ) ;
#30203 = CIRCLE ( 'NONE', #93952, 5.000000000000002665 ) ;
#30204 = ORIENTED_EDGE ( 'NONE', *, *, #6526, .T. ) ;
#30205 = CARTESIAN_POINT ( 'NONE',  ( 52.81650669486619165, 6.856755485862130937E-15, 0.000000000000000000 ) ) ;
#30206 = CARTESIAN_POINT ( 'NONE',  ( -6.846801517543320337, -12.21872792266663588, 8.794481130079006448 ) ) ;
#30207 = CARTESIAN_POINT ( 'NONE',  ( 38.54515645702225868, -5.000000000000000888, 6.123233995736769241E-16 ) ) ;
#30208 = ORIENTED_EDGE ( 'NONE', *, *, #8972, .F. ) ;
#30209 = B_SPLINE_CURVE_WITH_KNOTS ( 'NONE', 3,
 ( #58546, #10507, #98967, #1327, #91447, #49900, #18637, #91962, #51497 ),
 .UNSPECIFIED., .F., .F.,
 ( 4, 2, 1, 2, 4 ),
 ( 6.245710625686469831E-20, 0.002165063509461098799, 0.004330127018922196730, 0.006495190528383295095, 0.008660254037844391725 ),
 .UNSPECIFIED. ) ;
#30210 = CARTESIAN_POINT ( 'NONE',  ( 36.64823341582350480, 437.5392299810053487, 4.281405873620231617 ) ) ;
#30211 = CARTESIAN_POINT ( 'NONE',  ( -9.090909090909095269, 15.00000000000000000, -4.165977904505304252 ) ) ;
#30212 = CARTESIAN_POINT ( 'NONE',  ( -92.76516906498835624, -57.61752273625296539, 204.4213914816233739 ) ) ;
#30213 = CARTESIAN_POINT ( 'NONE',  ( -5.911778709945830101, -68.86661839416569819, 1.058844270818174227 ) ) ;
#30214 = CARTESIAN_POINT ( 'NONE',  ( -37.48925363931288501, 48.00000000000000711, 53.34938573421634800 ) ) ;
#30215 = DIRECTION ( 'NONE',  ( 0.000000000000000000, 0.000000000000000000, 1.000000000000000000 ) ) ;
#30216 = SURFACE_STYLE_USAGE ( .BOTH. , #36745 ) ;
#30217 = CARTESIAN_POINT ( 'NONE',  ( 86.89874827037927218, -29.99999999999997868, -18.81865104787653920 ) ) ;
#30218 = CARTESIAN_POINT ( 'NONE',  ( -72.31573431813527009, -14.21045842199431064, 125.5062215401438266 ) ) ;
#30219 = CARTESIAN_POINT ( 'NONE',  ( -54.21185734353947083, -53.38106178705758964, 64.18017538421840129 ) ) ;
#30220 = ORIENTED_EDGE ( 'NONE', *, *, #25518, .F. ) ;
#30221 = CARTESIAN_POINT ( 'NONE',  ( 43.75010090114224681, 464.8337800386878484, 11.75004750934975029 ) ) ;
#30222 = ORIENTED_EDGE ( 'NONE', *, *, #106727, .T. ) ;
#30223 = CARTESIAN_POINT ( 'NONE',  ( -102.8276541885064717, -60.17762386373496497, 193.1075909480691166 ) ) ;
#30224 = FACE_OUTER_BOUND ( 'NONE', #22574, .T. ) ;
#30225 = ORIENTED_EDGE ( 'NONE', *, *, #5206, .F. ) ;
#30226 = CARTESIAN_POINT ( 'NONE',  ( 18.97538325432419981, 49.43284846044564063, 61.96509015790782371 ) ) ;
#30227 = CARTESIAN_POINT ( 'NONE',  ( 90.71044788504735834, -38.34175721622889910, 7.076824436591243384 ) ) ;
#30228 =( NAMED_UNIT ( * ) SI_UNIT ( $, .STERADIAN. ) SOLID_ANGLE_UNIT ( ) );
#30229 = CARTESIAN_POINT ( 'NONE',  ( 4.401442555609581635E-16, -10.15625000204838457, -7.188101187500000044 ) ) ;
#30230 = CARTESIAN_POINT ( 'NONE',  ( -13.68624448364603374, 294.5456259610601251, 1.871922272540206045 ) ) ;
#30231 = COLOUR_RGB ( '', 0.31764706, 0.68627451, 0.89019608) ;
#30232 = CARTESIAN_POINT ( 'NONE',  ( 1.152188841818234133E-13, -1.200000000000000030E-05, 51.75000000000000711 ) ) ;
#30233 = CARTESIAN_POINT ( 'NONE',  ( 53.08934989192464826, -30.00000000000000000, 52.21148837440648549 ) ) ;
#30234 = CARTESIAN_POINT ( 'NONE',  ( -8.671807383147852377, 21.54545697599958842, -0.000000000000000000 ) ) ;
#30235 = CARTESIAN_POINT ( 'NONE',  ( 4.551587301587293410, -48.79941684889506348, 104.4018401814738013 ) ) ;
#30236 = ADVANCED_FACE ( 'NONE', ( #95626 ), #59029, .F. ) ;
#30237 = CARTESIAN_POINT ( 'NONE',  ( 8.000000000000000000, -24.40624999999999289, -3.313708498984761164 ) ) ;
#30238 = CARTESIAN_POINT ( 'NONE',  ( -29.49181701981505910, -46.43697584440771919, 34.18020204610339619 ) ) ;
#30239 = ADVANCED_FACE ( 'NONE', ( #97723 ), #14150, .F. ) ;
#30240 = ORIENTED_EDGE ( 'NONE', *, *, #89542, .F. ) ;
#30241 = EDGE_LOOP ( 'NONE', ( #7754, #26372, #75671, #84316, #84461 ) ) ;
#30242 = CARTESIAN_POINT ( 'NONE',  ( 48.55458696805421681, -49.90003314422357050, 51.74501749119150418 ) ) ;
#30243 = CARTESIAN_POINT ( 'NONE',  ( 46.00000000000000000, 450.0000000000002274, 25.20242257375371864 ) ) ;
#30244 = ADVANCED_FACE ( 'NONE', ( #55658 ), #44544, .F. ) ;
#30245 = DIRECTION ( 'NONE',  ( -1.000000000000000000, -2.168404344971008868E-17, 0.000000000000000000 ) ) ;
#30246 = ADVANCED_FACE ( 'NONE', ( #105824 ), #31965, .T. ) ;
#30247 = CARTESIAN_POINT ( 'NONE',  ( -110.5250911598958226, -38.35611436153418197, 182.1522587334059722 ) ) ;
#30248 = ORIENTED_EDGE ( 'NONE', *, *, #30311, .T. ) ;
#30249 = CARTESIAN_POINT ( 'NONE',  ( 91.32589455155351743, -38.36701310358807149, -2.641594532008445739 ) ) ;
#30250 = CARTESIAN_POINT ( 'NONE',  ( 12.35621370429071675, 9.768256507115607334, -9.479262080219816866 ) ) ;
#30251 = DIRECTION ( 'NONE',  ( 1.000000000000000000, 0.000000000000000000, 0.000000000000000000 ) ) ;
#30252 = CARTESIAN_POINT ( 'NONE',  ( 0.000000000000000000, 0.000000000000000000, 0.000000000000000000 ) ) ;
#30253 = CARTESIAN_POINT ( 'NONE',  ( 0.000000000000000000, 0.000000000000000000, -13.00000000000000000 ) ) ;
#30254 = CARTESIAN_POINT ( 'NONE',  ( -31.61667038019096410, 439.3937981091067968, 23.34452816489683258 ) ) ;
#30255 = CARTESIAN_POINT ( 'NONE',  ( 8.000000000000000000, -26.09375000409676915, -3.313708498984761164 ) ) ;
#30256 = CARTESIAN_POINT ( 'NONE',  ( -35.46167881839126323, 432.6462199839393179, 5.655415401830411248 ) ) ;
#30257 = CARTESIAN_POINT ( 'NONE',  ( 4.898587196589412829E-16, -16.81250000409677270, -8.000000000000000000 ) ) ;
#30258 = CARTESIAN_POINT ( 'NONE',  ( 12.50000000000000711, -4.999999999999999112, -79.51734232575269345 ) ) ;
#30259 = CARTESIAN_POINT ( 'NONE',  ( 83.15400578599735582, -59.99999999999999289, 198.9384841273030986 ) ) ;
#30260 = VECTOR ( 'NONE', #11561, 1000.000000000000227 ) ;
#30261 = ADVANCED_FACE ( 'NONE', ( #49715 ), #59661, .F. ) ;
#30262 = CARTESIAN_POINT ( 'NONE',  ( 18.43654383764750548, 45.00000000000002132, 62.34954961627184389 ) ) ;
#30263 = ORIENTED_EDGE ( 'NONE', *, *, #95268, .F. ) ;
#30264 = CARTESIAN_POINT ( 'NONE',  ( 57.26729019237954788, -25.61006374783701034, 59.45692232418873147 ) ) ;
#30265 = CARTESIAN_POINT ( 'NONE',  ( -28.74670144010507400, 306.4392983594438533, -9.196308249178452243 ) ) ;
#30266 = CARTESIAN_POINT ( 'NONE',  ( 7.934996450857311423, 33.86862456472530170, -1.050865690281770126 ) ) ;
#30267 = CONICAL_SURFACE ( 'NONE', #92281, 6.500000000000000000, 1.047197551196600296 ) ;
#30268 = ORIENTED_EDGE ( 'NONE', *, *, #19572, .F. ) ;
#30269 = B_SPLINE_CURVE_WITH_KNOTS ( 'NONE', 3,
 ( #21661, #61045, #52934, #69659, #85860, #87442 ),
 .UNSPECIFIED., .F., .F.,
 ( 4, 2, 4 ),
 ( 0.004444412883774348857, 0.006655097293744438938, 0.008865781703714529019 ),
 .UNSPECIFIED. ) ;
#30271 = CARTESIAN_POINT ( 'NONE',  ( -18.00000000000000355, 12.99999999999999467, -9.500000000000000000 ) ) ;
#30270 = CARTESIAN_POINT ( 'NONE',  ( -96.39762838794068500, -38.48434118611966426, 201.1825086705471506 ) ) ;
#30272 = CARTESIAN_POINT ( 'NONE',  ( 14.54015256618498242, 142.2617268803927288, 0.000000000000000000 ) ) ;
#30273 = CARTESIAN_POINT ( 'NONE',  ( 27.22388839005207828, 312.2963372293064026, 10.72986269782501623 ) ) ;
#30274 = CARTESIAN_POINT ( 'NONE',  ( -7.188101187500002709, -11.18750000204838457, 2.977408999572648707 ) ) ;
#30275 = STYLED_ITEM ( 'NONE', ( #17633 ), #11922 ) ;
#30276 = AXIS2_PLACEMENT_3D ( 'NONE', #12567, #54605, #61695 ) ;
#30277 = CARTESIAN_POINT ( 'NONE',  ( 7.996668422910221175, -5.000000000000002665, -78.85453279918266389 ) ) ;
#30278 =( GEOMETRIC_REPRESENTATION_CONTEXT ( 3 ) GLOBAL_UNCERTAINTY_ASSIGNED_CONTEXT ( ( #23744 ) ) GLOBAL_UNIT_ASSIGNED_CONTEXT ( ( #26669, #57921, #75709 ) ) REPRESENTATION_CONTEXT ( 'NONE', 'WORKASPACE' ) );
#30279 = CARTESIAN_POINT ( 'NONE',  ( 30.42537733501877639, 12.90981014178660757, -41.86413436173263136 ) ) ;
#30280 = CONICAL_SURFACE ( 'NONE', #59531, 5.000000000000000000, 0.9599310885968913576 ) ;
#30282 = ORIENTED_EDGE ( 'NONE', *, *, #88929, .T. ) ;
#30281 =( NAMED_UNIT ( * ) SI_UNIT ( $, .STERADIAN. ) SOLID_ANGLE_UNIT ( ) );
#30283 = CARTESIAN_POINT ( 'NONE',  ( 85.06960557373632525, -25.47056552230032977, 167.4782931879399257 ) ) ;
#30284 = CARTESIAN_POINT ( 'NONE',  ( 9.413227697955839801, 10.29402594059818021, 0.000000000000000000 ) ) ;
#30285 = DIRECTION ( 'NONE',  ( 1.000000000000000000, 1.224606353822377258E-16, 0.000000000000000000 ) ) ;
#30286 = ORIENTED_EDGE ( 'NONE', *, *, #29786, .T. ) ;
#30287 = CARTESIAN_POINT ( 'NONE',  ( -30.87619945487599082, 309.1625279880333892, -8.547083864057238856 ) ) ;
#30288 = CARTESIAN_POINT ( 'NONE',  ( 17.73840306501246289, 34.63647015383776306, 22.27315226561848149 ) ) ;
#30289 = DIRECTION ( 'NONE',  ( -0.000000000000000000, -0.000000000000000000, -1.000000000000000000 ) ) ;
#30290 = CARTESIAN_POINT ( 'NONE',  ( 33.00000000000000000, 500.0000000000002274, 0.000000000000000000 ) ) ;
#30291 = CIRCLE ( 'NONE', #92219, 15.00000000000001243 ) ;
#30292 = CARTESIAN_POINT ( 'NONE',  ( 33.58349330513379982, 1.593028355512270567E-15, 0.000000000000000000 ) ) ;
#30293 = EDGE_LOOP ( 'NONE', ( #31065, #7260, #45068, #58300 ) ) ;
#30294 = EDGE_CURVE ( 'NONE', #1378, #104577, #82241, .T. ) ;
#30295 = CARTESIAN_POINT ( 'NONE',  ( -81.12865512346820651, -30.00000000000000355, 1.958835504223271018 ) ) ;
#30296 = CARTESIAN_POINT ( 'NONE',  ( -5.000000000000000888, -26.68136363036281722, -6.178889730593319030 ) ) ;
#30297 = CARTESIAN_POINT ( 'NONE',  ( 0.06809871960542752956, 6.146186931204407067, 5.354491962338127742 ) ) ;
#30298 = EDGE_CURVE ( 'NONE', #56071, #90051, #36783, .T. ) ;
#30299 = EDGE_CURVE ( 'NONE', #101089, #57615, #20339, .T. ) ;
#30301 = CARTESIAN_POINT ( 'NONE',  ( -10.76670854121271326, 15.75155368674281675, -9.619787616750810955 ) ) ;
#30300 = CARTESIAN_POINT ( 'NONE',  ( 8.866506694866188809, 4.000000000000003553, 4.898587196589414801E-16 ) ) ;
#30302 = CARTESIAN_POINT ( 'NONE',  ( 5.082755093536325930, -17.46875000204838457, -5.082755093536325042 ) ) ;
#30303 = CARTESIAN_POINT ( 'NONE',  ( 16.92021657089327746, 302.5811070205058968, -10.05744944873218572 ) ) ;
#30304 = DIRECTION ( 'NONE',  ( -1.000000000000000000, -1.224606353822377258E-16, -0.000000000000000000 ) ) ;
#30305 = VERTEX_POINT ( 'NONE', #36771 ) ;
#30306 = DIRECTION ( 'NONE',  ( -1.000000000000000000, -1.224606353822377258E-16, -0.000000000000000000 ) ) ;
#30307 = CARTESIAN_POINT ( 'NONE',  ( 7.500000000000698996, -1.614186302714018861, -7.450236204327475242 ) ) ;
#30308 = AXIS2_PLACEMENT_3D ( 'NONE', #82420, #58687, #100195 ) ;
#30309 = CARTESIAN_POINT ( 'NONE',  ( -9.460558175396068137, 9.928212646412896802, -5.000000000000000888 ) ) ;
#30310 = DIRECTION ( 'NONE',  ( -1.000000000000000000, -1.224606353822377258E-16, -0.000000000000000000 ) ) ;
#30311 = EDGE_CURVE ( 'NONE', #5264, #53678, #28673, .T. ) ;
#30312 = EDGE_LOOP ( 'NONE', ( #23859, #20652, #47213, #102827 ) ) ;
#30313 = LINE ( 'NONE', #97139, #65349 ) ;
#30314 = DIRECTION ( 'NONE',  ( -1.000000000000000000, -1.224606353822377258E-16, -0.000000000000000000 ) ) ;
#30315 = ORIENTED_EDGE ( 'NONE', *, *, #63299, .T. ) ;
#30316 = ADVANCED_FACE ( 'NONE', ( #101986 ), #37294, .T. ) ;
#30317 = CARTESIAN_POINT ( 'NONE',  ( -28.29505784598654472, 34.17090463856185067, 9.198890806811057530 ) ) ;
#30318 = CARTESIAN_POINT ( 'NONE',  ( -51.48757442383523397, 38.95383793070303113, -37.45149417477429665 ) ) ;
#30319 = CARTESIAN_POINT ( 'NONE',  ( -23.21751746555280249, -1.200000000000000030E-05, -31.95617127781034839 ) ) ;
#30320 = CARTESIAN_POINT ( 'NONE',  ( -112.1996801038472995, -59.99999999999999289, 170.0554107543789257 ) ) ;
#30321 = SURFACE_SIDE_STYLE ('',( #29286 ) ) ;
#30322 = PRESENTATION_STYLE_ASSIGNMENT (( #53521 ) ) ;
#30323 = DIRECTION ( 'NONE',  ( 1.000000000000000000, 0.000000000000000000, 0.000000000000000000 ) ) ;
#30324 = EDGE_CURVE ( 'NONE', #25443, #91936, #75313, .T. ) ;
#30325 =( NAMED_UNIT ( * ) PLANE_ANGLE_UNIT ( ) SI_UNIT ( $, .RADIAN. ) );
#30326 = CARTESIAN_POINT ( 'NONE',  ( -81.79652205476276094, -60.68003446516232913, 187.1438624714922980 ) ) ;
#30327 = COLOUR_RGB ( '', 0.09019608, 0.27058824, 0.51372549) ;
#30328 = VERTEX_POINT ( 'NONE', #85279 ) ;
#30329 = CARTESIAN_POINT ( 'NONE',  ( 43.59534864137770427, 41.43266498251605157, -50.56630447086893554 ) ) ;
#30330 = ORIENTED_EDGE ( 'NONE', *, *, #47971, .F. ) ;
#30331 = CARTESIAN_POINT ( 'NONE',  ( 28.58349330513380337, 1.593028355512270962E-15, 0.000000000000000000 ) ) ;
#30333 = FACE_OUTER_BOUND ( 'NONE', #42172, .T. ) ;
#30332 = AXIS2_PLACEMENT_3D ( 'NONE', #55312, #45139, #21403 ) ;
#30334 = CARTESIAN_POINT ( 'NONE',  ( -83.25482506818879358, -37.82319541480158875, 29.52994787646102637 ) ) ;
#30335 = DIRECTION ( 'NONE',  ( 0.000000000000000000, 0.000000000000000000, -1.000000000000000000 ) ) ;
#30336 = CARTESIAN_POINT ( 'NONE',  ( -16.05785784214673484, 4.775831776474318779, -3.710403933782550290 ) ) ;
#30337 = CARTESIAN_POINT ( 'NONE',  ( 8.361452242989621197, 121.1754334411836567, -4.999999999998772537 ) ) ;
#30338 = CARTESIAN_POINT ( 'NONE',  ( -2.352990130084491319E-16, 7.505553499465148271, -8.000000000000000000 ) ) ;
#30339 = CARTESIAN_POINT ( 'NONE',  ( -30.67950393662606956, 18.64316884711714906, 23.57730434126661834 ) ) ;
#30340 = CARTESIAN_POINT ( 'NONE',  ( 105.6362521817138713, -29.99999999999994671, 194.5266552104434368 ) ) ;
#30341 = CARTESIAN_POINT ( 'NONE',  ( -107.5810679786090702, -30.00000000000002487, 145.3413084537935163 ) ) ;
#30342 = CARTESIAN_POINT ( 'NONE',  ( -65.80800410575133697, -22.10322226003651380, 79.50655047398903719 ) ) ;
#30343 = VECTOR ( 'NONE', #44043, 1000.000000000000000 ) ;
#30344 = VERTEX_POINT ( 'NONE', #26555 ) ;
#30345 = CARTESIAN_POINT ( 'NONE',  ( -57.68978467818401157, 38.95207517830731092, -27.56125053296379690 ) ) ;
#30346 = CARTESIAN_POINT ( 'NONE',  ( 94.38326820372073200, -59.99999999999746336, 204.9998441075219091 ) ) ;
#30347 = AXIS2_PLACEMENT_3D ( 'NONE', #103070, #84757, #101473 ) ;
#30348 = VERTEX_POINT ( 'NONE', #60500 ) ;
#30349 = CARTESIAN_POINT ( 'NONE',  ( 13.93074145947618447, -57.79372918398592418, 28.41232622077120595 ) ) ;
#30351 = CIRCLE ( 'NONE', #83745, 4.000000000000001776 ) ;
#30350 = CARTESIAN_POINT ( 'NONE',  ( 7.188101187500000933, -17.93750000204838457, -2.977408999572650483 ) ) ;
#30352 = B_SPLINE_CURVE_WITH_KNOTS ( 'NONE', 3,
 ( #106585, #106041, #57490, #31669, #82848, #90415, #89881, #49407, #39746, #40263, #74741, #15991, #105529, #80709 ),
 .UNSPECIFIED., .F., .F.,
 ( 4, 2, 2, 2, 2, 2, 4 ),
 ( 2.602085213965210642E-18, 0.001028561904211934379, 0.002057123808423866156, 0.004114247616847721903, 0.005142809521059639802, 0.006171371425271557701, 0.008228495233695377886 ),
 .UNSPECIFIED. ) ;
#30353 = CARTESIAN_POINT ( 'NONE',  ( 32.15166163075743100, 486.0589784586656492, 5.199393881399972273 ) ) ;
#30354 = ORIENTED_EDGE ( 'NONE', *, *, #27043, .T. ) ;
#30355 = CARTESIAN_POINT ( 'NONE',  ( -11.39656771499227084, 45.34267223356314958, 14.75529722941189625 ) ) ;
#30356 = ORIENTED_EDGE ( 'NONE', *, *, #29244, .F. ) ;
#30357 = CARTESIAN_POINT ( 'NONE',  ( -43.18056654203904543, 485.1460802498594944, 5.477204712337340631 ) ) ;
#30358 = CARTESIAN_POINT ( 'NONE',  ( 0.000000000000000000, 0.000000000000000000, 0.000000000000000000 ) ) ;
#30359 = CARTESIAN_POINT ( 'NONE',  ( -83.77391689997462265, -59.99999999999995737, -25.46673677812911407 ) ) ;
#30360 = LINE ( 'NONE', #103696, #240 ) ;
#30361 = CARTESIAN_POINT ( 'NONE',  ( -7.188101187500000044, -24.78125000204838813, -8.802885111219163269E-16 ) ) ;
#30362 = LINE ( 'NONE', #94570, #36351 ) ;
#30363 = COLOUR_RGB ( '', 0.40784314, 0.44705882, 0.49803922) ;
#30364 =( BOUNDED_CURVE ( )  B_SPLINE_CURVE ( 2, ( #26873, #85072, #33885, #60290, #91050, #9033, #41941, #50030, #59742 ),
 .UNSPECIFIED., .F., .F. ) 
 B_SPLINE_CURVE_WITH_KNOTS ( ( 3, 2, 2, 2, 3 ),
 ( 0.6323529411764706731, 0.6397058823529412352, 0.6470588235294119084, 0.6544117647058823595, 0.6617647058823529216 ),
 .UNSPECIFIED. ) 
 CURVE ( )  GEOMETRIC_REPRESENTATION_ITEM ( )  RATIONAL_B_SPLINE_CURVE ( ( 0.9999999999999988898, 0.9238795325112878487, 1.000000000000000000, 0.9238795325112867385, 1.000000000000000000, 0.9238795325112867385, 1.000000000000000000, 0.9238795325112867385, 1.000000000000000000 ) ) 
 REPRESENTATION_ITEM ( '' )  );
#30365 = DIRECTION ( 'NONE',  ( 0.000000000000000000, -1.000000000000000000, 0.000000000000000000 ) ) ;
#30366 = DIRECTION ( 'NONE',  ( 1.000000000000000000, 1.224606353822377258E-16, 0.000000000000000000 ) ) ;
#30367 = CARTESIAN_POINT ( 'NONE',  ( 8.737863884121436442, 48.00000000000000000, -79.96381019768851672 ) ) ;
#30368 = FACE_OUTER_BOUND ( 'NONE', #81638, .T. ) ;
#30369 = CARTESIAN_POINT ( 'NONE',  ( -37.76893244230605262, 307.4136788487199965, 0.9472622734037586811 ) ) ;
#30370 = EDGE_CURVE ( 'NONE', #9249, #29960, #50841, .T. ) ;
#30371 = CARTESIAN_POINT ( 'NONE',  ( 103.9907751973010335, -59.99999999999997868, 190.8231350958398878 ) ) ;
#30372 = ORIENTED_EDGE ( 'NONE', *, *, #12233, .F. ) ;
#30373 = FACE_OUTER_BOUND ( 'NONE', #53853, .T. ) ;
#30374 = CARTESIAN_POINT ( 'NONE',  ( 56.22793774957824553, 6.975173280561618775E-15, 0.000000000000000000 ) ) ;
#30375 = CARTESIAN_POINT ( 'NONE',  ( 36.78615735600832437, -36.04596638446182766, 35.70108577633924085 ) ) ;
#30376 = CARTESIAN_POINT ( 'NONE',  ( -2.227375807149027054, -1.734723475976807094E-15, 17.01589776168603407 ) ) ;
#30377 = EDGE_LOOP ( 'NONE', ( #48508, #71765, #44248, #15886 ) ) ;
#30378 = EDGE_CURVE ( 'NONE', #21676, #54847, #21103, .T. ) ;
#30379 = CARTESIAN_POINT ( 'NONE',  ( -8.000000000000000000, 0.000000000000000000, -0.02540000000000007530 ) ) ;
#30380 = EDGE_CURVE ( 'NONE', #36732, #12690, #29031, .T. ) ;
#30381 = EDGE_LOOP ( 'NONE', ( #47286, #56498, #78798, #4587 ) ) ;
#30383 = CARTESIAN_POINT ( 'NONE',  ( 22.20318009218133071, 295.0333587257888439, 9.975590323731541531 ) ) ;
#30382 = FACE_OUTER_BOUND ( 'NONE', #63972, .T. ) ;
#30384 = CARTESIAN_POINT ( 'NONE',  ( 16.75187969033571989, 37.11970326878314097, 21.80698433968582961 ) ) ;
#30385 = DIRECTION ( 'NONE',  ( 0.000000000000000000, -1.000000000000000000, 0.000000000000000000 ) ) ;
#30386 = CARTESIAN_POINT ( 'NONE',  ( 31.03678703375144821, 438.6650838204807314, 21.86890379897223013 ) ) ;
#30387 = DIRECTION ( 'NONE',  ( 0.000000000000000000, -1.000000000000000000, -1.877893248421449282E-16 ) ) ;
#30388 = CARTESIAN_POINT ( 'NONE',  ( -49.18580537133279762, 13.60959006579542674, -15.12486994001303486 ) ) ;
#30389 = CARTESIAN_POINT ( 'NONE',  ( 0.000000000000000000, 0.000000000000000000, 0.000000000000000000 ) ) ;
#30390 = ADVANCED_FACE ( 'NONE', ( #21124 ), #78764, .T. ) ;
#30391 = AXIS2_PLACEMENT_3D ( 'NONE', #90961, #26261, #7885 ) ;
#30392 = CARTESIAN_POINT ( 'NONE',  ( 97.99660889140263009, -60.00000000000000711, 68.90520065234117908 ) ) ;
#30393 = CARTESIAN_POINT ( 'NONE',  ( 0.000000000000000000, 0.000000000000000000, 0.000000000000000000 ) ) ;
#30394 = EDGE_CURVE ( 'NONE', #57657, #3401, #37637, .T. ) ;
#30395 = VECTOR ( 'NONE', #17887, 1000.000000000000000 ) ;
#30396 = DIRECTION ( 'NONE',  ( -0.000000000000000000, -1.000000000000000000, -0.000000000000000000 ) ) ;
#30397 = FACE_BOUND ( 'NONE', #51167, .T. ) ;
#30398 = ORIENTED_EDGE ( 'NONE', *, *, #79381, .F. ) ;
#30399 = CARTESIAN_POINT ( 'NONE',  ( -88.86068578946498064, -29.99999999999961275, -15.16702001146615864 ) ) ;
#30400 = ORIENTED_EDGE ( 'NONE', *, *, #57435, .T. ) ;
#30401 = CARTESIAN_POINT ( 'NONE',  ( -15.50988061984491395, 2.604948194297879382, 0.4026888889386251447 ) ) ;
#30402 = CARTESIAN_POINT ( 'NONE',  ( 3.443342638033501490, 27.85812572534835496, 5.000000000000000000 ) ) ;
#30403 =( NAMED_UNIT ( * ) SI_UNIT ( $, .STERADIAN. ) SOLID_ANGLE_UNIT ( ) );
#30404 = FACE_OUTER_BOUND ( 'NONE', #35679, .T. ) ;
#30405 = CARTESIAN_POINT ( 'NONE',  ( 5.082755093536325930, -32.84375000204838813, -5.082755093536325042 ) ) ;
#30406 = DIRECTION ( 'NONE',  ( 0.000000000000000000, -0.6543614439331875143, -0.7561819230143458359 ) ) ;
#30407 = CARTESIAN_POINT ( 'NONE',  ( 0.000000000000000000, 49.50000000000000000, 0.000000000000000000 ) ) ;
#30408 = CARTESIAN_POINT ( 'NONE',  ( 31.88312681400266868, 463.8062021098571677, 15.68963310188262739 ) ) ;
#30409 = ORIENTED_EDGE ( 'NONE', *, *, #28861, .T. ) ;
#30411 = ORIENTED_EDGE ( 'NONE', *, *, #34009, .T. ) ;
#30410 = FACE_BOUND ( 'NONE', #80610, .T. ) ;
#30412 = CARTESIAN_POINT ( 'NONE',  ( 78.97029474429139384, -42.96455894964061883, 142.9603876401418461 ) ) ;
#30413 = CARTESIAN_POINT ( 'NONE',  ( -38.65357358930379661, 27.30496217644010315, -12.82931495569635238 ) ) ;
#30414 = ORIENTED_EDGE ( 'NONE', *, *, #55995, .F. ) ;
#30415 = CARTESIAN_POINT ( 'NONE',  ( -12.50000000000000533, 33.01231111522088923, -51.52182527394435141 ) ) ;
#30416 = CARTESIAN_POINT ( 'NONE',  ( 5.484632749660399931, 41.99999999999999289, -59.73832504088978368 ) ) ;
#30417 = CARTESIAN_POINT ( 'NONE',  ( 2.977408999572650927, -18.87500000204838457, -7.188101187500000933 ) ) ;
#30418 = CARTESIAN_POINT ( 'NONE',  ( 11.29905645152050475, 45.32368457861270628, 14.89516444794118222 ) ) ;
#30419 = CARTESIAN_POINT ( 'NONE',  ( 17.24515478965690818, 294.5883438517400918, 1.881387340289478516 ) ) ;
#30420 = AXIS2_PLACEMENT_3D ( 'NONE', #100050, #49361, #252 ) ;
#30421 = ORIENTED_EDGE ( 'NONE', *, *, #95673, .F. ) ;
#30422 = B_SPLINE_CURVE_WITH_KNOTS ( 'NONE', 3,
 ( #103499, #21546, #104551, #78155, #20523, #79218, #70605, #29647, #30702, #53357, #94896, #4275, #12878, #53874, #63590, #45795, #71125, #78674, #88388, #5344, #95406, #46847, #87327, #102972, #69548, #94360, #5852, #37203 ),
 .UNSPECIFIED., .F., .F.,
 ( 4, 2, 2, 2, 2, 2, 2, 2, 2, 2, 2, 2, 2, 4 ),
 ( 0.007813944516173620958, 0.008738276158831484106, 0.009662607801489347253, 0.01058693944414721040, 0.01151127108680507355, 0.01243560272946293843, 0.01289776855079186914, 0.01335993437212079984, 0.01382210019344973229, 0.01405318310411419851, 0.01428426601477866473, 0.01451534892544312921, 0.01474643183610759717, 0.01520859765743652441 ),
 .UNSPECIFIED. ) ;
#30423 = FILL_AREA_STYLE_COLOUR ( '', #5737 ) ;
#30424 = DIRECTION ( 'NONE',  ( 0.000000000000000000, 0.000000000000000000, 1.000000000000000000 ) ) ;
#30425 = AXIS2_PLACEMENT_3D ( 'NONE', #54022, #86965, #38417 ) ;
#30426 = CARTESIAN_POINT ( 'NONE',  ( 0.000000000000000000, 49.99999999999999289, -95.00000000000000000 ) ) ;
#30427 = CARTESIAN_POINT ( 'NONE',  ( 7.395123142502173508, 40.93288834207328364, -59.01287878374339613 ) ) ;
#30428 = EDGE_CURVE ( 'NONE', #74794, #97405, #23842, .T. ) ;
#30429 = DIRECTION ( 'NONE',  ( 1.000000000000000000, 0.000000000000000000, 0.000000000000000000 ) ) ;
#30430 = CARTESIAN_POINT ( 'NONE',  ( -8.000000000000001776, -11.84375000409677270, 3.313708498984758943 ) ) ;
#30431 = AXIS2_PLACEMENT_3D ( 'NONE', #33849, #66721, #99602 ) ;
#30432 = CARTESIAN_POINT ( 'NONE',  ( -13.42771739161924494, -14.69885084449941104, 31.71672228287745909 ) ) ;
#30433 = CIRCLE ( 'NONE', #90692, 4.000000000000001776 ) ;
#30434 = CYLINDRICAL_SURFACE ( 'NONE', #78412, 4.000000000000000888 ) ;
#30435 = AXIS2_PLACEMENT_3D ( 'NONE', #94545, #53535, #87505 ) ;
#30436 = CARTESIAN_POINT ( 'NONE',  ( 0.08432500865644583510, 52.17923068443688095, -7.750000000000010658 ) ) ;
#30437 = CARTESIAN_POINT ( 'NONE',  ( 6.256238905933717120, -3.000000000000470290, -71.20382035666703757 ) ) ;
#30438 = FILL_AREA_STYLE_COLOUR ( '', #28732 ) ;
#30439 = APPLICATION_PROTOCOL_DEFINITION ( 'draft international standard', 'automotive_design', 1998, #95471 ) ;
#30440 = CARTESIAN_POINT ( 'NONE',  ( -9.253817200599833370, 31.29992729916860483, -3.791916801615161869 ) ) ;
#30441 = VERTEX_POINT ( 'NONE', #64205 ) ;
#30443 = VECTOR ( 'NONE', #36296, 1000.000000000000000 ) ;
#30442 = CARTESIAN_POINT ( 'NONE',  ( 11.50595937734579799, 43.27894158476472342, 14.44327389318907073 ) ) ;
#30444 = DIRECTION ( 'NONE',  ( -3.673940397442057649E-17, 0.000000000000000000, -1.000000000000000000 ) ) ;
#30445 = CARTESIAN_POINT ( 'NONE',  ( 36.84999999999999432, 3.309500000000003439, 4.052968581778167743E-16 ) ) ;
#30446 = CARTESIAN_POINT ( 'NONE',  ( -69.22537020059996848, -29.97316140627671288, -21.14164747078667972 ) ) ;
#30447 = CARTESIAN_POINT ( 'NONE',  ( -63.07201610543538806, -29.99999999999999645, 74.88422784947999844 ) ) ;
#30448 = CARTESIAN_POINT ( 'NONE',  ( 5.500000000000006217, 42.00000000000000000, -59.28631038546474485 ) ) ;
#30449 = VERTEX_POINT ( 'NONE', #104103 ) ;
#30450 = CARTESIAN_POINT ( 'NONE',  ( -27.10511071441192144, 36.60571256639527604, -10.05698433968589178 ) ) ;
#30451 = CARTESIAN_POINT ( 'NONE',  ( 91.42196762672531918, -57.61411189307126790, 204.2437217276433046 ) ) ;
#30452 = LINE ( 'NONE', #5616, #38004 ) ;
#30453 = EDGE_CURVE ( 'NONE', #88504, #94858, #29221, .T. ) ;
#30454 = FACE_OUTER_BOUND ( 'NONE', #43920, .T. ) ;
#30455 = CARTESIAN_POINT ( 'NONE',  ( -15.79700980112394326, 22.78020937716808803, 0.4986931010682000287 ) ) ;
#30456 = CARTESIAN_POINT ( 'NONE',  ( 0.000000000000000000, 69.00000000000000000, 0.000000000000000000 ) ) ;
#30457 = PRODUCT_DEFINITION_SHAPE ( 'NONE', 'NONE',  #23923 ) ;
#30458 = CARTESIAN_POINT ( 'NONE',  ( -75.41463958967447923, -60.00000000000000711, 183.9905783904083592 ) ) ;
#30459 = CARTESIAN_POINT ( 'NONE',  ( 0.04050535873994128011, 7.919512791578243949, -6.573129608219097086 ) ) ;
#30460 = CARTESIAN_POINT ( 'NONE',  ( 32.04230769230768772, 4.172000000000003261, 5.109226446042759579E-16 ) ) ;
#30461 = ADVANCED_FACE ( 'NONE', ( #12963 ), #97073, .F. ) ;
#30462 = CARTESIAN_POINT ( 'NONE',  ( 28.89099332389485042, 49.99999999997997691, 58.53034795348389707 ) ) ;
#30463 = CIRCLE ( 'NONE', #44224, 2.999999999999999112 ) ;
#30464 = CARTESIAN_POINT ( 'NONE',  ( -85.99570664262481046, -35.58902874923357018, 185.3986280066468453 ) ) ;
#30465 = VERTEX_POINT ( 'NONE', #54469 ) ;
#30466 = CARTESIAN_POINT ( 'NONE',  ( 36.00963897964896177, 344.1584813113714176, -0.3684565162341075228 ) ) ;
#30467 = PRESENTATION_LAYER_ASSIGNMENT (  '', '', ( #28800 ) ) ;
#30468 = CARTESIAN_POINT ( 'NONE',  ( -7.619701877737481865, -13.17442159532768287, -2.447562251315977822 ) ) ;
#30469 = CARTESIAN_POINT ( 'NONE',  ( 42.44292469749079544, 488.6013120130130005, 9.763388545826034104 ) ) ;
#30470 = SURFACE_STYLE_FILL_AREA ( #102747 ) ;
#30471 = CARTESIAN_POINT ( 'NONE',  ( 31.14131030317610538, 5.000000000000003553, 0.000000000000000000 ) ) ;
#30472 = EDGE_LOOP ( 'NONE', ( #41859, #23092 ) ) ;
#30473 = CARTESIAN_POINT ( 'NONE',  ( 18.42142964856622811, 49.99999999999999289, 61.35851441441231913 ) ) ;
#30474 = CARTESIAN_POINT ( 'NONE',  ( 13.70945920918955174, 3.091663963860816988, 6.042453855890579817 ) ) ;
#30475 = PRESENTATION_STYLE_ASSIGNMENT (( #54171 ) ) ;
#30476 = CARTESIAN_POINT ( 'NONE',  ( -37.43096154125763064, 464.0779267918313735, 19.48675998633273920 ) ) ;
#30477 = CARTESIAN_POINT ( 'NONE',  ( 68.53628924694606894, -14.21045842199431597, -27.48009014525527860 ) ) ;
#30478 = CARTESIAN_POINT ( 'NONE',  ( -80.34670115289323178, -36.03127197182796237, 144.2402978679412229 ) ) ;
#30479 = PRODUCT_DEFINITION ( 'UNKNOWN', '', #73150, #10041 ) ;
#30480 = ORIENTED_EDGE ( 'NONE', *, *, #19724, .F. ) ;
#30481 = CARTESIAN_POINT ( 'NONE',  ( 16.61664997849939240, -30.00000000000006395, 37.21280938527437598 ) ) ;
#30482 = CARTESIAN_POINT ( 'NONE',  ( 4.478476647430158941, 250.2735207918204594, 3.992942460563207341 ) ) ;
#30483 = CARTESIAN_POINT ( 'NONE',  ( 72.11178192614376314, -57.67306540792444025, 173.1801346106868493 ) ) ;
#30484 = CARTESIAN_POINT ( 'NONE',  ( 62.57102314643675811, 50.00000000000000000, -7.448774052006193358 ) ) ;
#30485 = CARTESIAN_POINT ( 'NONE',  ( 35.48147139702570030, 303.1671216000320328, -0.09562962482448161827 ) ) ;
#30486 = CARTESIAN_POINT ( 'NONE',  ( -11.66623074095491752, 11.72717158878924693, 9.938064884429101298 ) ) ;
#30487 = VERTEX_POINT ( 'NONE', #88997 ) ;
#30488 = CARTESIAN_POINT ( 'NONE',  ( 94.84444444444443434, 1.023464760207051730E-14, 0.000000000000000000 ) ) ;
#30489 = DIRECTION ( 'NONE',  ( 1.000000000000000000, 0.000000000000000000, 0.000000000000000000 ) ) ;
#30491 = CARTESIAN_POINT ( 'NONE',  ( -102.9402037365450866, -45.26537910807851972, 153.9863529572914445 ) ) ;
#30490 = CARTESIAN_POINT ( 'NONE',  ( -2.499999999999996447, -30.00000000000000000, -13.00000000000000000 ) ) ;
#30492 = CARTESIAN_POINT ( 'NONE',  ( 7.188101187499999156, -25.25000000204839523, 2.977408999572654924 ) ) ;
#30493 = FACE_OUTER_BOUND ( 'NONE', #12830, .T. ) ;
#30494 = CARTESIAN_POINT ( 'NONE',  ( 71.63333333333333997, -3.309500000000000774, 0.000000000000000000 ) ) ;
#30495 = DIRECTION ( 'NONE',  ( 0.000000000000000000, 1.000000000000000000, 0.000000000000000000 ) ) ;
#30496 = CARTESIAN_POINT ( 'NONE',  ( 26.94613286657595097, 36.94238815830848210, 7.556984339685560492 ) ) ;
#30497 = FILL_AREA_STYLE_COLOUR ( '', #59375 ) ;
#30498 = CARTESIAN_POINT ( 'NONE',  ( 16.80185279643511720, 43.70018028759842110, -4.157797401561335704 ) ) ;
#30499 = ORIENTED_EDGE ( 'NONE', *, *, #86784, .T. ) ;
#30500 = ADVANCED_FACE ( 'NONE', ( #87418 ), #45885, .F. ) ;
#30501 = CARTESIAN_POINT ( 'NONE',  ( -5.787521267941007963, 41.99999999999999289, -59.87256577776128097 ) ) ;
#30502 = AXIS2_PLACEMENT_3D ( 'NONE', #62550, #29678, #4303 ) ;
#30503 =( GEOMETRIC_REPRESENTATION_CONTEXT ( 3 ) GLOBAL_UNCERTAINTY_ASSIGNED_CONTEXT ( ( #97666 ) ) GLOBAL_UNIT_ASSIGNED_CONTEXT ( ( #85512, #49263, #41191 ) ) REPRESENTATION_CONTEXT ( 'NONE', 'WORKASPACE' ) );
#30505 = CARTESIAN_POINT ( 'NONE',  ( 24.39961550212768415, -25.56170002018362553, 29.25281948027246059 ) ) ;
#30504 = CARTESIAN_POINT ( 'NONE',  ( 0.08224679563971343255, 7.710515798486365036, 2.644994884459111351 ) ) ;
#30506 = CARTESIAN_POINT ( 'NONE',  ( -24.17834536076760443, 25.18046967552916371, 32.76024643191446017 ) ) ;
#30507 = EDGE_LOOP ( 'NONE', ( #100600, #100809, #15502, #99719 ) ) ;
#30508 = EDGE_CURVE ( 'NONE', #82981, #6993, #15175, .T. ) ;
#30509 = ORIENTED_EDGE ( 'NONE', *, *, #63976, .T. ) ;
#30510 = PRODUCT_DEFINITION_SHAPE ( 'NONE', 'NONE',  #106816 ) ;
#30511 = PRESENTATION_LAYER_ASSIGNMENT (  '', '', ( #21818 ) ) ;
#30513 = CARTESIAN_POINT ( 'NONE',  ( 1.221257515003810079, 51.58212317033902394, 9.311104479422620983 ) ) ;
#30512 = FILL_AREA_STYLE ('',( #40163 ) ) ;
#30514 = DIRECTION ( 'NONE',  ( -1.000000000000000000, -0.000000000000000000, -0.000000000000000000 ) ) ;
#30515 = AXIS2_PLACEMENT_3D ( 'NONE', #18944, #2706, #68533 ) ;
#30516 = VECTOR ( 'NONE', #105545, 1000.000000000000000 ) ;
#30517 = CARTESIAN_POINT ( 'NONE',  ( -0.6461142731108306947, 51.32298069254813555, -10.08306419293876743 ) ) ;
#30518 = CARTESIAN_POINT ( 'NONE',  ( -30.00000000000000000, 488.8442721620238558, 4.433647275927475206 ) ) ;
#30519 = CARTESIAN_POINT ( 'NONE',  ( 0.07752439927408807940, 18.87382441218277407, -49.25000000000001421 ) ) ;
#30520 = ORIENTED_EDGE ( 'NONE', *, *, #105357, .T. ) ;
#30521 = CARTESIAN_POINT ( 'NONE',  ( 5.802656403430185961, -59.99999999999999289, -42.56106326075611435 ) ) ;
#30522 = DIRECTION ( 'NONE',  ( 0.5735764363510554853, 0.8191520442889852482, 0.000000000000000000 ) ) ;
#30523 = CARTESIAN_POINT ( 'NONE',  ( -10.04689216137323626, 14.71245185582296244, 10.43754960648917063 ) ) ;
#30524 = CARTESIAN_POINT ( 'NONE',  ( 0.000000000000000000, 0.000000000000000000, 4.000000000000000888 ) ) ;
#30525 = STYLED_ITEM ( 'NONE', ( #36322 ), #15527 ) ;
#30526 = EDGE_CURVE ( 'NONE', #68049, #35444, #57151, .T. ) ;
#30527 = CARTESIAN_POINT ( 'NONE',  ( -8.559508646656370345, 53.96349637827587031, 1.531152949374564365 ) ) ;
#30528 = ADVANCED_FACE ( 'NONE', ( #56605 ), #51362, .F. ) ;
#30529 = CARTESIAN_POINT ( 'NONE',  ( 28.86650669486618881, 1.474610560812782335E-15, 0.000000000000000000 ) ) ;
#30530 = ORIENTED_EDGE ( 'NONE', *, *, #72817, .T. ) ;
#30531 = ORIENTED_EDGE ( 'NONE', *, *, #32373, .F. ) ;
#30532 = VERTEX_POINT ( 'NONE', #49583 ) ;
#30533 = CARTESIAN_POINT ( 'NONE',  ( 46.00000000000000000, 500.0000000000002274, -15.00000000000000711 ) ) ;
#30534 = CARTESIAN_POINT ( 'NONE',  ( 1.836970198721029983E-15, 0.000000000000000000, -15.00000000000000178 ) ) ;
#30535 = CARTESIAN_POINT ( 'NONE',  ( -1.469576158976823947E-15, -16.06250000409677270, 8.000000000000000000 ) ) ;
#30536 = CARTESIAN_POINT ( 'NONE',  ( -43.65164521923173879, 485.1135274750027406, -1.117678676893244960 ) ) ;
#30537 = DIRECTION ( 'NONE',  ( -1.000000000000000000, -1.224606353822377258E-16, -0.000000000000000000 ) ) ;
#30538 = ORIENTED_EDGE ( 'NONE', *, *, #55932, .F. ) ;
#30539 = CARTESIAN_POINT ( 'NONE',  ( 1.308996937483426715, 48.00000000000000000, -95.00000000000000000 ) ) ;
#30540 = ORIENTED_EDGE ( 'NONE', *, *, #31787, .F. ) ;
#30541 = CARTESIAN_POINT ( 'NONE',  ( 0.000000000000000000, 0.000000000000000000, 0.000000000000000000 ) ) ;
#30542 = CARTESIAN_POINT ( 'NONE',  ( 60.38390319005696227, -38.34250386216492501, 97.61615657541973690 ) ) ;
#30543 = CARTESIAN_POINT ( 'NONE',  ( 0.000000000000000000, 0.000000000000000000, 4.000000000000000888 ) ) ;
#30544 = AXIS2_PLACEMENT_3D ( 'NONE', #51277, #2732, #77169 ) ;
#30545 = CARTESIAN_POINT ( 'NONE',  ( -80.33450311392522281, -60.00000000000002842, 177.7302725502722751 ) ) ;
#30546 = CARTESIAN_POINT ( 'NONE',  ( 62.70097925198960098, -49.91075561683145168, 84.84605103675988858 ) ) ;
#30547 = ORIENTED_EDGE ( 'NONE', *, *, #106259, .T. ) ;
#30548 = CARTESIAN_POINT ( 'NONE',  ( 37.88504238421554504, 463.4171042825134919, 19.90923349043870871 ) ) ;
#30549 = PRESENTATION_LAYER_ASSIGNMENT (  '', '', ( #77011 ) ) ;
#30550 = CARTESIAN_POINT ( 'NONE',  ( -59.38248720328446240, -37.25844438171453987, -34.32352965270520428 ) ) ;
#30551 = CARTESIAN_POINT ( 'NONE',  ( 0.000000000000000000, 4.898587196589412829E-16, -4.000000000000000000 ) ) ;
#30552 = CARTESIAN_POINT ( 'NONE',  ( -61.29065067449151627, -57.67115771167040350, -37.35479649122906665 ) ) ;
#30553 = ORIENTED_EDGE ( 'NONE', *, *, #38243, .T. ) ;
#30554 = CARTESIAN_POINT ( 'NONE',  ( -13.00000000000003730, -85.00000000000000000, 0.000000000000000000 ) ) ;
#30555 = FACE_OUTER_BOUND ( 'NONE', #2168, .T. ) ;
#30556 = EDGE_CURVE ( 'NONE', #88641, #95805, #62350, .T. ) ;
#30557 = B_SPLINE_CURVE_WITH_KNOTS ( 'NONE', 3,
 ( #14466, #95955, #31244, #46855, #86812, #78682 ),
 .UNSPECIFIED., .F., .F.,
 ( 4, 2, 4 ),
 ( 0.004444412883774324571, 0.006655097293744431132, 0.008865781703714535958 ),
 .UNSPECIFIED. ) ;
#30558 = CARTESIAN_POINT ( 'NONE',  ( -5.656854249492379694, -28.62500000409677270, -5.656854249492380582 ) ) ;
#30559 = CARTESIAN_POINT ( 'NONE',  ( 4.175893272575727622, -4.999999999998865796, -7.137815226411304614 ) ) ;
#30560 = CARTESIAN_POINT ( 'NONE',  ( 86.48923150265004267, -50.13329297819660013, 191.3735317416930286 ) ) ;
#30561 = STYLED_ITEM ( 'NONE', ( #55344 ), #7393 ) ;
#30562 = CARTESIAN_POINT ( 'NONE',  ( -5.292662561255604636, 18.30812576678731318, -37.69621763902263467 ) ) ;
#30563 = B_SPLINE_CURVE_WITH_KNOTS ( 'NONE', 3,
 ( #73933, #57740, #25981, #15, #99260, #8143, #50197, #97676, #33506, #91216 ),
 .UNSPECIFIED., .F., .F.,
 ( 4, 2, 2, 2, 4 ),
 ( 0.000000000000000000, 0.2500000000000000000, 0.5000000000000000000, 0.7500000000000000000, 1.000000000000000000 ),
 .UNSPECIFIED. ) ;
#30564 = UNCERTAINTY_MEASURE_WITH_UNIT (LENGTH_MEASURE( 1.000000000000000082E-05 ), #46710, 'distance_accuracy_value', 'NONE');
#30565 = CARTESIAN_POINT ( 'NONE',  ( -8.757836645960713540, 19.71581191398818333, 4.999999999999364952 ) ) ;
#30566 = DIRECTION ( 'NONE',  ( -9.567764352753668770E-16, 0.5617366626193331935, 0.8273160954975393722 ) ) ;
#30567 = CARTESIAN_POINT ( 'NONE',  ( -42.88788165701930666, 484.9809715185594996, -1.409177641707331619 ) ) ;
#30568 = ORIENTED_EDGE ( 'NONE', *, *, #88829, .F. ) ;
#30569 = CARTESIAN_POINT ( 'NONE',  ( 13.44288011066907096, -52.70710939378555793, 30.91149535780206747 ) ) ;
#30570 = DIRECTION ( 'NONE',  ( -1.000000000000000000, -1.224606353822377258E-16, -0.000000000000000000 ) ) ;
#30571 = CARTESIAN_POINT ( 'NONE',  ( 36.75192448471445061, -60.00000000000000000, 48.11202499009017686 ) ) ;
#30572 = CARTESIAN_POINT ( 'NONE',  ( -100.4436717631274405, -30.00000000000001066, 183.3501104447698253 ) ) ;
#30573 = EDGE_CURVE ( 'NONE', #98077, #85478, #32372, .T. ) ;
#30574 = AXIS2_PLACEMENT_3D ( 'NONE', #106700, #98084, #32851 ) ;
#30575 = DIRECTION ( 'NONE',  ( -1.000000000000000000, 0.000000000000000000, 0.000000000000000000 ) ) ;
#30576 = VECTOR ( 'NONE', #68672, 1000.000000000000227 ) ;
#30577 = CARTESIAN_POINT ( 'NONE',  ( 40.69853667173202894, -57.69061545352386133, 56.83570513438750993 ) ) ;
#30579 = CARTESIAN_POINT ( 'NONE',  ( 0.000000000000000000, -14.49999999999999822, 0.000000000000000000 ) ) ;
#30578 = CARTESIAN_POINT ( 'NONE',  ( 14.14239901661592214, 6.671053996447657397, -7.747582395498725738 ) ) ;
#30580 = CYLINDRICAL_SURFACE ( 'NONE', #88482, 5.000000000000002665 ) ;
#30581 = CARTESIAN_POINT ( 'NONE',  ( -18.27395090668250788, 50.00000000000000000, 61.54374581262641897 ) ) ;
#30582 = CARTESIAN_POINT ( 'NONE',  ( -9.606080321247056020, 15.83563386295778308, 2.802461721337994760 ) ) ;
#30583 = SURFACE_STYLE_FILL_AREA ( #95833 ) ;
#30584 = CARTESIAN_POINT ( 'NONE',  ( -13.47129954280381625, -60.00000000000000711, 39.72841581181796045 ) ) ;
#30585 = CIRCLE ( 'NONE', #8137, 0.9999999999999806821 ) ;
#30586 = VECTOR ( 'NONE', #48098, 999.9999999999998863 ) ;
#30587 = LINE ( 'NONE', #13295, #10600 ) ;
#30588 = ADVANCED_FACE ( 'NONE', ( #58210 ), #97872, .F. ) ;
#30589 = CARTESIAN_POINT ( 'NONE',  ( -87.01710432979982102, -57.37281113167114199, 193.9090236191709380 ) ) ;
#30590 = ORIENTED_EDGE ( 'NONE', *, *, #50404, .F. ) ;
#30591 = CARTESIAN_POINT ( 'NONE',  ( 17.50000000000003197, 50.00252300264495631, 59.96656198872853594 ) ) ;
#30592 = CARTESIAN_POINT ( 'NONE',  ( 38.93727158156521995, 438.0716948385729665, 23.12369454750587749 ) ) ;
#30593 = AXIS2_PLACEMENT_3D ( 'NONE', #99336, #48138, #65402 ) ;
#30594 = CARTESIAN_POINT ( 'NONE',  ( -14.77380270916763116, -53.40237792673437411, 32.92252495082122010 ) ) ;
#30595 = ADVANCED_FACE ( 'NONE', ( #16153 ), #10024, .T. ) ;
#30597 = CARTESIAN_POINT ( 'NONE',  ( 38.96902200852336051, 460.8405016383494512, 2.186950304201005224 ) ) ;
#30596 = CARTESIAN_POINT ( 'NONE',  ( -94.52029764136869971, -60.00000000000002132, 83.13177969407045964 ) ) ;
#30598 = ORIENTED_EDGE ( 'NONE', *, *, #76488, .T. ) ;
#30599 = CARTESIAN_POINT ( 'NONE',  ( 26.34328342495543751, 35.00028662264767121, 7.802099556721183049 ) ) ;
#30600 =( LENGTH_UNIT ( ) NAMED_UNIT ( * ) SI_UNIT ( .MILLI., .METRE. ) );
#30601 = CARTESIAN_POINT ( 'NONE',  ( 0.000000000000000000, 7.511572993685796142E-16, -6.500000000000000888 ) ) ;
#30602 = CARTESIAN_POINT ( 'NONE',  ( 16.01234866801993562, 3.721647123654680200, 0.3211924699178611009 ) ) ;
#30603 = CARTESIAN_POINT ( 'NONE',  ( 72.13637180897663370, -60.00000000000000711, 155.3038211014013257 ) ) ;
#30604 = VECTOR ( 'NONE', #82759, 1000.000000000000227 ) ;
#30605 = DIRECTION ( 'NONE',  ( -0.000000000000000000, -1.000000000000000000, -0.000000000000000000 ) ) ;
#30606 = ORIENTED_EDGE ( 'NONE', *, *, #83581, .T. ) ;
#30607 = DIRECTION ( 'NONE',  ( 1.000000000000000000, -0.000000000000000000, -0.000000000000000000 ) ) ;
#30608 = CARTESIAN_POINT ( 'NONE',  ( -3.313708498984798467, -21.21875000409677270, -7.999999999999961808 ) ) ;
#30609 = CARTESIAN_POINT ( 'NONE',  ( 20.75554216095374116, -29.99999999999998579, 37.60191050100322485 ) ) ;
#30611 = AXIS2_PLACEMENT_3D ( 'NONE', #11756, #59808, #36096 ) ;
#30610 = SURFACE_STYLE_USAGE ( .BOTH. , #47807 ) ;
#30612 = CARTESIAN_POINT ( 'NONE',  ( -5.164787682159484916, -1.887557197826900124, 104.1470044518084990 ) ) ;
#30613 = EDGE_LOOP ( 'NONE', ( #20815, #8319 ) ) ;
#30614 = ADVANCED_FACE ( 'NONE', ( #58761 ), #6719, .T. ) ;
#30615 = ORIENTED_EDGE ( 'NONE', *, *, #7200, .F. ) ;
#30617 = CARTESIAN_POINT ( 'NONE',  ( -27.76738912986519381, 314.2059264268535230, 11.21182569962504694 ) ) ;
#30616 = CIRCLE ( 'NONE', #49517, 8.000000000000000000 ) ;
#30618 = EDGE_LOOP ( 'NONE', ( #41564, #19492, #39620, #68513, #64813, #4732 ) ) ;
#30619 = FILL_AREA_STYLE_COLOUR ( '', #79337 ) ;
#30620 = DIRECTION ( 'NONE',  ( 0.000000000000000000, 0.000000000000000000, -1.000000000000000000 ) ) ;
#30621 =( NAMED_UNIT ( * ) SI_UNIT ( $, .STERADIAN. ) SOLID_ANGLE_UNIT ( ) );
#30622 = VERTEX_POINT ( 'NONE', #85700 ) ;
#30623 =( NAMED_UNIT ( * ) SI_UNIT ( $, .STERADIAN. ) SOLID_ANGLE_UNIT ( ) );
#30624 = CARTESIAN_POINT ( 'NONE',  ( -114.3478711580139304, -60.00000000001953282, 163.9674887148623839 ) ) ;
#30625 = CARTESIAN_POINT ( 'NONE',  ( 46.00000000000000000, 488.3725375423288710, 3.127739281034839003 ) ) ;
#30626 = CARTESIAN_POINT ( 'NONE',  ( 73.65925679185706088, -60.00000000000001421, 168.7609027532264179 ) ) ;
#30627 = CARTESIAN_POINT ( 'NONE',  ( 6.162888688655344893, 3.752776749732562589, -6.500000000000000888 ) ) ;
#30628 = DIRECTION ( 'NONE',  ( 1.000000000000000000, 1.224606353822377258E-16, 0.000000000000000000 ) ) ;
#30630 = CARTESIAN_POINT ( 'NONE',  ( 12.30984511850486740, -32.51068972755530950, 29.36027658876032120 ) ) ;
#30629 = CARTESIAN_POINT ( 'NONE',  ( -97.22630358410161477, -59.99999999999998579, 47.92073696641181613 ) ) ;
#30631 = CARTESIAN_POINT ( 'NONE',  ( 99.27397055116384195, -38.00000000000000711, 191.6755426901316071 ) ) ;
#30632 =( NAMED_UNIT ( * ) SI_UNIT ( $, .STERADIAN. ) SOLID_ANGLE_UNIT ( ) );
#30633 = AXIS2_PLACEMENT_3D ( 'NONE', #100904, #59955, #92822 ) ;
#30634 = CARTESIAN_POINT ( 'NONE',  ( -45.70114157808188082, -60.26445691949498951, 50.30722036196431901 ) ) ;
#30635 = DIRECTION ( 'NONE',  ( 0.000000000000000000, -1.000000000000000000, 0.000000000000000000 ) ) ;
#30636 = VERTEX_POINT ( 'NONE', #101861 ) ;
#30637 = CARTESIAN_POINT ( 'NONE',  ( 1.231118141235101326, 11.28179331793877438, -50.25142030543173632 ) ) ;
#30638 = PRESENTATION_LAYER_ASSIGNMENT (  '', '', ( #65022 ) ) ;
#30639 = SURFACE_STYLE_FILL_AREA ( #94838 ) ;
#30640 = CARTESIAN_POINT ( 'NONE',  ( 4.590682673078522846, -8.932082426878441339, 3.864023243754608927 ) ) ;
#30641 = CARTESIAN_POINT ( 'NONE',  ( 31.19652432992544888, 378.3327707670021027, 24.28948218791313707 ) ) ;
#30642 = VERTEX_POINT ( 'NONE', #19408 ) ;
#30643 = CARTESIAN_POINT ( 'NONE',  ( -8.451132639193684071, -14.18294114141584039, 15.83549708304340164 ) ) ;
#30644 = AXIS2_PLACEMENT_3D ( 'NONE', #21412, #79607, #54791 ) ;
#30645 = EDGE_LOOP ( 'NONE', ( #18751, #101509, #45226, #90243 ) ) ;
#30646 = CARTESIAN_POINT ( 'NONE',  ( 80.13328830561965788, -29.99999999999337064, 190.7101562830954720 ) ) ;
#30647 =( NAMED_UNIT ( * ) PLANE_ANGLE_UNIT ( ) SI_UNIT ( $, .RADIAN. ) );
#30648 = CARTESIAN_POINT ( 'NONE',  ( 0.000000000000000000, -15.00000000000000000, 0.000000000000000000 ) ) ;
#30650 = ADVANCED_FACE ( 'NONE', ( #1549 ), #43101, .T. ) ;
#30649 = FILL_AREA_STYLE ('',( #15495 ) ) ;
#30651 = CARTESIAN_POINT ( 'NONE',  ( 97.38464793213240966, -29.99999999999999645, 190.9410892311414614 ) ) ;
#30652 = EDGE_CURVE ( 'NONE', #87776, #106068, #76516, .T. ) ;
#30653 = LINE ( 'NONE', #45749, #65590 ) ;
#30654 = ORIENTED_EDGE ( 'NONE', *, *, #99863, .T. ) ;
#30655 = ORIENTED_EDGE ( 'NONE', *, *, #21344, .F. ) ;
#30656 = ORIENTED_EDGE ( 'NONE', *, *, #95335, .T. ) ;
#30657 = AXIS2_PLACEMENT_3D ( 'NONE', #25722, #76334, #19232 ) ;
#30658 = DIRECTION ( 'NONE',  ( -1.000000000000000000, -0.000000000000000000, -0.000000000000000000 ) ) ;
#30659 = CARTESIAN_POINT ( 'NONE',  ( -45.99999999999996447, 436.0910238442153855, 11.28143031774616567 ) ) ;
#30660 = AXIS2_PLACEMENT_3D ( 'NONE', #8686, #41590, #551 ) ;
#30661 = EDGE_CURVE ( 'NONE', #66199, #8292, #45534, .T. ) ;
#30662 = DIRECTION ( 'NONE',  ( 1.000000000000000000, 1.224606353822377258E-16, 0.000000000000000000 ) ) ;
#30663 = VERTEX_POINT ( 'NONE', #94320 ) ;
#30664 = CARTESIAN_POINT ( 'NONE',  ( 0.000000000000000000, 0.000000000000000000, 0.000000000000000000 ) ) ;
#30665 = ORIENTED_EDGE ( 'NONE', *, *, #58880, .T. ) ;
#30666 = CARTESIAN_POINT ( 'NONE',  ( 0.000000000000000000, 0.000000000000000000, -10.00000000000000000 ) ) ;
#30667 = CARTESIAN_POINT ( 'NONE',  ( 101.8625646185573856, -38.44601613749367885, 199.7504753397604986 ) ) ;
#30668 = CARTESIAN_POINT ( 'NONE',  ( 13.72259981623363245, 3.069379053792045564, 6.012713411074214420 ) ) ;
#30669 = CARTESIAN_POINT ( 'NONE',  ( 82.77473000103051959, -37.85543405128064620, 2.355868850680865823 ) ) ;
#30670 = CARTESIAN_POINT ( 'NONE',  ( -0.9999999999999943379, -50.00000000000000000, 101.0455488498966758 ) ) ;
#30671 = MECHANICAL_DESIGN_GEOMETRIC_PRESENTATION_REPRESENTATION (  '', ( #1347 ), #99523 ) ;
#30672 = AXIS2_PLACEMENT_3D ( 'NONE', #54421, #4847, #70109 ) ;
#30673 = CARTESIAN_POINT ( 'NONE',  ( 41.07051048954355821, 327.4162906337114691, 9.867383232854635366 ) ) ;
#30674 = AXIS2_PLACEMENT_3D ( 'NONE', #55823, #6230, #47222 ) ;
#30675 = FACE_OUTER_BOUND ( 'NONE', #99390, .T. ) ;
#30676 = FACE_OUTER_BOUND ( 'NONE', #64186, .T. ) ;
#30677 = FILL_AREA_STYLE ('',( #5317 ) ) ;
#30678 = CARTESIAN_POINT ( 'NONE',  ( 2.723995404495900718, -0.3641544584862766443, 102.8348527318366052 ) ) ;
#30679 = AXIS2_PLACEMENT_3D ( 'NONE', #100119, #27352, #60230 ) ;
#30680 = ORIENTED_EDGE ( 'NONE', *, *, #39252, .T. ) ;
#30681 = CARTESIAN_POINT ( 'NONE',  ( -9.701712097384769251, 15.75132464342601857, -2.450541714948249794 ) ) ;
#30682 = CARTESIAN_POINT ( 'NONE',  ( -38.51502786940056211, 460.0233756673464427, 2.043034587342818398 ) ) ;
#30683 = CARTESIAN_POINT ( 'NONE',  ( -26.78592122648698393, 36.71852912224116494, 10.02587077895928935 ) ) ;
#30684 = ORIENTED_EDGE ( 'NONE', *, *, #106332, .F. ) ;
#30685 = AXIS2_PLACEMENT_3D ( 'NONE', #63198, #87476, #55592 ) ;
#30686 = DIRECTION ( 'NONE',  ( -1.000000000000000000, 0.000000000000000000, 0.000000000000000000 ) ) ;
#30687 = CARTESIAN_POINT ( 'NONE',  ( -26.91834224567524814, 306.8661554697472980, 10.86152638338143994 ) ) ;
#30688 = CARTESIAN_POINT ( 'NONE',  ( 7.944798090354270315, 53.91010666794784356, -3.881035696276761815 ) ) ;
#30689 = CARTESIAN_POINT ( 'NONE',  ( 29.83349330513380337, 1.593028355512270567E-15, 0.000000000000000000 ) ) ;
#30690 = CARTESIAN_POINT ( 'NONE',  ( -3.313708498984760720, -18.03124999999999645, -8.000000000000000000 ) ) ;
#30691 = CARTESIAN_POINT ( 'NONE',  ( 34.45567488635992248, -26.24090404973739865, 41.62864160396504332 ) ) ;
#30692 = EDGE_CURVE ( 'NONE', #69600, #86973, #56512, .T. ) ;
#30693 = AXIS2_PLACEMENT_3D ( 'NONE', #85957, #21236, #36886 ) ;
#30694 = ORIENTED_EDGE ( 'NONE', *, *, #98938, .T. ) ;
#30695 = CARTESIAN_POINT ( 'NONE',  ( 84.38907022229382449, -53.80946252041021438, 189.6612499249015400 ) ) ;
#30696 = CARTESIAN_POINT ( 'NONE',  ( -38.31505842747957757, 27.60007494029672159, 11.19190443272380264 ) ) ;
#30697 = ADVANCED_FACE ( 'NONE', ( #67382 ), #36115, .T. ) ;
#30698 = PLANE ( 'NONE',  #2171 ) ;
#30699 = EDGE_LOOP ( 'NONE', ( #29559, #49204, #89510, #105783, #2607 ) ) ;
#30700 = CARTESIAN_POINT ( 'NONE',  ( 94.16204370421009173, -57.67429201036151909, 3.106671879859604246 ) ) ;
#30701 = CARTESIAN_POINT ( 'NONE',  ( 36.73553355714089008, 438.2340261154861309, 3.898456086351941074 ) ) ;
#30702 = CARTESIAN_POINT ( 'NONE',  ( -30.82729297445935401, 10.08692072324635269, 40.33672416147543771 ) ) ;
#30703 =( BOUNDED_SURFACE ( )  B_SPLINE_SURFACE ( 3, 2, ( 
 ( #97213, #56200, #23364 ),
 ( #14163, #5557, #54092 ),
 ( #80492, #79445, #89140 ),
 ( #88607, #15239, #14694 ) ),
 .UNSPECIFIED., .F., .F., .F. ) 
 B_SPLINE_SURFACE_WITH_KNOTS ( ( 4, 4 ),
 ( 3, 3 ),
 ( 1.322726650432315409E-17, 0.0002214634272574486900 ),
 ( 0.000000000000000000, 1.000000000000000000 ),
 .UNSPECIFIED. ) 
 GEOMETRIC_REPRESENTATION_ITEM ( )  RATIONAL_B_SPLINE_SURFACE ( (
 ( 1.000000000000000000, 0.8273155905869640225, 1.000000000000000000),
 ( 1.000000000000000000, 0.8262236971337512115, 1.000000000000000000),
 ( 1.000000000000000000, 0.8250826013137413373, 1.000000000000000000),
 ( 1.000000000000000000, 0.8238944711861589942, 1.000000000000000000) ) ) 
 REPRESENTATION_ITEM ( '' )  SURFACE ( )  );
#30704 = EDGE_CURVE ( 'NONE', #53832, #1254, #58222, .T. ) ;
#30706 = EDGE_LOOP ( 'NONE', ( #21739, #47370, #91619, #48872 ) ) ;
#30705 = B_SPLINE_CURVE_WITH_KNOTS ( 'NONE', 3,
 ( #21194, #3912, #13573, #87492, #36845, #45968, #13036, #78844, #4974, #61093 ),
 .UNSPECIFIED., .F., .F.,
 ( 4, 2, 2, 2, 4 ),
 ( -6.000000001405383295E-08, 0.002526620965178684626, 0.005053301930357382774, 0.01010666386071478948, 0.02021338772142960982 ),
 .UNSPECIFIED. ) ;
#30707 = CIRCLE ( 'NONE', #92648, 5.000000000000002665 ) ;
#30708 = CARTESIAN_POINT ( 'NONE',  ( 21.21144082669073327, -26.49527374954287495, 37.12913197614864202 ) ) ;
#30709 = DIRECTION ( 'NONE',  ( -1.000000000000000000, -1.224606353822377258E-16, -0.000000000000000000 ) ) ;
#30710 = VECTOR ( 'NONE', #17758, 1000.000000000000000 ) ;
#30712 = SURFACE_STYLE_FILL_AREA ( #46856 ) ;
#30711 = CARTESIAN_POINT ( 'NONE',  ( 41.58444831332685254, 481.6520554591356245, 13.64600804804222811 ) ) ;
#30713 =( LENGTH_UNIT ( ) NAMED_UNIT ( * ) SI_UNIT ( .MILLI., .METRE. ) );
#30714 = DIRECTION ( 'NONE',  ( 0.000000000000000000, 0.000000000000000000, -1.000000000000000000 ) ) ;
#30715 = CARTESIAN_POINT ( 'NONE',  ( -28.32674270491142821, 36.29719069258228359, -9.120579834107232386 ) ) ;
#30716 = DIRECTION ( 'NONE',  ( -1.000000000000000000, -1.224606353822377258E-16, -0.000000000000000000 ) ) ;
#30717 = CARTESIAN_POINT ( 'NONE',  ( -6.750000000000018652, 11.69134295108991317, -13.00000000000000000 ) ) ;
#30718 = TOROIDAL_SURFACE ( 'NONE', #77200, 11.00000000000000533, 4.000000000000000000 ) ;
#30719 = EDGE_CURVE ( 'NONE', #99128, #83726, #39306, .T. ) ;
#30720 = CARTESIAN_POINT ( 'NONE',  ( -102.6007910818582616, -38.00000000000002132, 179.5952160768334238 ) ) ;
#30721 = VERTEX_POINT ( 'NONE', #26427 ) ;
#30722 = CARTESIAN_POINT ( 'NONE',  ( 6.169949891408690767, -6.308465495018908520, -2.073417244830776163 ) ) ;
#30723 = FACE_OUTER_BOUND ( 'NONE', #13025, .T. ) ;
#30724 = CARTESIAN_POINT ( 'NONE',  ( -10.76224560403525032, -16.36478912462312252, -34.75025230997614756 ) ) ;
#30725 = EDGE_CURVE ( 'NONE', #78066, #99126, #82397, .T. ) ;
#30727 = CARTESIAN_POINT ( 'NONE',  ( -46.51767665254412520, -21.77006129918473576, -26.23258419899174498 ) ) ;
#30726 = DIRECTION ( 'NONE',  ( -1.000000000000000000, -1.224606353822377258E-16, -0.000000000000000000 ) ) ;
#30728 = ORIENTED_EDGE ( 'NONE', *, *, #38286, .T. ) ;
#30729 = DIRECTION ( 'NONE',  ( 0.8191520442889884679, 0.000000000000000000, 0.5735764363510508224 ) ) ;
#30730 = AXIS2_PLACEMENT_3D ( 'NONE', #37792, #56026, #87379 ) ;
#30731 = CIRCLE ( 'NONE', #53114, 8.900000000000000355 ) ;
#30732 = ORIENTED_EDGE ( 'NONE', *, *, #47847, .F. ) ;
#30733 = AXIS2_PLACEMENT_3D ( 'NONE', #100615, #90950, #92523 ) ;
#30734 = EDGE_CURVE ( 'NONE', #2627, #7097, #32456, .T. ) ;
#30735 = CARTESIAN_POINT ( 'NONE',  ( 6.692588830498425345, 3.932766476276031486, 6.892929031562513131 ) ) ;
#30736 = CARTESIAN_POINT ( 'NONE',  ( 29.83349330513380693, 4.000000000000002665, 0.000000000000000000 ) ) ;
#30737 = CARTESIAN_POINT ( 'NONE',  ( -92.38965560796522425, -59.99999999999999289, 0.2914275940444852053 ) ) ;
#30738 = ORIENTED_EDGE ( 'NONE', *, *, #100360, .T. ) ;
#30739 = DIRECTION ( 'NONE',  ( 0.000000000000000000, -1.000000000000000000, 0.000000000000000000 ) ) ;
#30740 = CARTESIAN_POINT ( 'NONE',  ( -10.00000000000000000, 15.11603512204006883, 0.3498606326563452606 ) ) ;
#30741 = CIRCLE ( 'NONE', #25596, 5.000000000000001776 ) ;
#30742 = CARTESIAN_POINT ( 'NONE',  ( 98.26932492730686874, -37.76192426467496688, 192.3739912550726956 ) ) ;
#30743 = DIRECTION ( 'NONE',  ( -1.000000000000000000, -1.224606353822377258E-16, -0.000000000000000000 ) ) ;
#30744 = CARTESIAN_POINT ( 'NONE',  ( -80.76959687771581287, -53.40869547565652198, 171.1175977112955877 ) ) ;
#30745 = VERTEX_POINT ( 'NONE', #61425 ) ;
#30746 = VERTEX_POINT ( 'NONE', #84086 ) ;
#30747 = VERTEX_POINT ( 'NONE', #75988 ) ;
#30748 = CARTESIAN_POINT ( 'NONE',  ( 8.354779502921196865, -5.000000000000000000, -14.10835818931967189 ) ) ;
#30749 = CARTESIAN_POINT ( 'NONE',  ( -3.339154757874568169, -69.93519652824339516, 13.40218433671247134 ) ) ;
#30750 = FACE_OUTER_BOUND ( 'NONE', #100018, .T. ) ;
#30751 = ORIENTED_EDGE ( 'NONE', *, *, #70267, .F. ) ;
#30752 = CARTESIAN_POINT ( 'NONE',  ( -34.90210962188712074, 473.1106922774044961, 16.89617127990342738 ) ) ;
#30753 = PRESENTATION_LAYER_ASSIGNMENT (  '', '', ( #4860 ) ) ;
#30754 = DIRECTION ( 'NONE',  ( -1.000000000000000000, -0.000000000000000000, -0.000000000000000000 ) ) ;
#30755 = CARTESIAN_POINT ( 'NONE',  ( -75.26480569136067800, -57.56533996972894585, 191.5310976926263322 ) ) ;
#30756 = CARTESIAN_POINT ( 'NONE',  ( 37.06438722625302518, 1.482358050883964840E-15, 0.000000000000000000 ) ) ;
#30757 = CARTESIAN_POINT ( 'NONE',  ( -57.77058984079067727, 47.99999999999999289, 30.23507972700047475 ) ) ;
#30758 = CARTESIAN_POINT ( 'NONE',  ( -13.97222917066916992, -50.12745207469774300, 26.08167946173673002 ) ) ;
#30759 = CARTESIAN_POINT ( 'NONE',  ( 1.510421413154031223, 15.23810023151232862, -9.910377230549265448 ) ) ;
#30760 = CARTESIAN_POINT ( 'NONE',  ( 87.60230161701383622, -14.21045842199431064, -3.802929300262678947 ) ) ;
#30761 = CARTESIAN_POINT ( 'NONE',  ( -76.85442806461188070, -14.21045842199432663, 149.6320961301125578 ) ) ;
#30762 = CARTESIAN_POINT ( 'NONE',  ( -53.00585131428307761, -49.90973205979414473, 60.14564158691946716 ) ) ;
#30763 = ORIENTED_EDGE ( 'NONE', *, *, #92466, .F. ) ;
#30764 = CARTESIAN_POINT ( 'NONE',  ( -17.49999999999999645, 2.500000000000000444, 25.00000000000000000 ) ) ;
#30765 = VERTEX_POINT ( 'NONE', #35039 ) ;
#30766 = CARTESIAN_POINT ( 'NONE',  ( -99.87378953022019346, -37.81191256832239134, 190.7979464389039208 ) ) ;
#30767 = APPLICATION_CONTEXT ( 'automotive_design' ) ;
#30768 = CARTESIAN_POINT ( 'NONE',  ( -30.36582766586210269, 16.93822630193516332, -39.80117229897623332 ) ) ;
#30769 = PRESENTATION_LAYER_ASSIGNMENT (  '', '', ( #56586 ) ) ;
#30770 = ORIENTED_EDGE ( 'NONE', *, *, #100975, .F. ) ;
#30771 = CARTESIAN_POINT ( 'NONE',  ( 19.13710312715079453, 49.71449728783072430, 61.67626017174043795 ) ) ;
#30772 = CARTESIAN_POINT ( 'NONE',  ( 109.6487595463947287, -38.35581244533405254, 151.0088976801097260 ) ) ;
#30773 = DIRECTION ( 'NONE',  ( -1.000000000000000000, -1.224606353822377258E-16, -0.000000000000000000 ) ) ;
#30774 = CARTESIAN_POINT ( 'NONE',  ( -4.413588872740236368, -9.563952367645420338, 5.751921314332417268 ) ) ;
#30775 = CARTESIAN_POINT ( 'NONE',  ( 6.683837171061806970, -7.911893696991936231, 5.688671339918660213E-17 ) ) ;
#30776 = CARTESIAN_POINT ( 'NONE',  ( -40.95595929481465447, 405.2208686710653183, 27.85131585683114963 ) ) ;
#30777 = B_SPLINE_SURFACE_WITH_KNOTS ( 'NONE', 3, 3, ( 
 ( #80569, #6688, #103797, #80041 ),
 ( #95718, #40126, #29941, #22389 ),
 ( #15315, #73003, #55749, #55233 ),
 ( #21856, #89216, #54696, #32058 ),
 ( #6153, #13181, #87629, #39615 ),
 ( #13715, #5634, #46624, #95195 ),
 ( #72488, #105395, #79521, #64421 ),
 ( #48203, #38558, #7217, #97290 ),
 ( #54165, #87107, #14241, #104322 ),
 ( #23444, #81104, #39086, #21328 ),
 ( #46110, #38047, #78992, #5115 ),
 ( #16373, #81618, #99397, #90810 ),
 ( #15846, #99947, #75668, #65468 ),
 ( #58438, #1223, #82708, #17461 ),
 ( #67066, #8279, #74601, #58977 ),
 ( #8812, #25580, #82165, #91864 ),
 ( #16926, #49802, #73535, #50327 ),
 ( #17990, #40653, #49262, #98359 ),
 ( #33123, #50850, #106437, #91349 ),
 ( #1769, #83234, #41189, #65992 ),
 ( #57885, #7743, #83756, #42776 ),
 ( #34190, #74071, #156, #682 ),
 ( #41717, #9328, #33644, #66525 ),
 ( #26120, #9865, #32596, #64935 ),
 ( #98869, #25029, #42237, #75126 ),
 ( #97823, #24513, #23985, #56828 ),
 ( #89749, #57350, #48727, #90272 ),
 ( #12519, #53531, #61103, #60058 ),
 ( #61651, #44382, #94541, #85369 ),
 ( #100477, #2299, #43839, #84303 ),
 ( #27707, #60581, #28772, #10398 ),
 ( #102614, #2841, #20692, #43314 ),
 ( #76728, #45452, #69200, #51920 ),
 ( #36854, #93471, #76197, #86459 ),
 ( #11456, #28231, #52454, #84836 ),
 ( #35248, #78327, #102071, #35793 ),
 ( #51389, #19082, #34726, #77277 ),
 ( #3387, #67599, #10919, #68113 ),
 ( #36331, #26638, #93991, #20151 ),
 ( #77809, #53002, #85923, #59508 ),
 ( #92382, #11994, #68671, #101011 ),
 ( #101551, #19621, #44926, #3922 ),
 ( #18528, #27168, #69722, #92916 ),
 ( #87501, #79914, #37913, #22781 ),
 ( #80441, #104190, #88029, #38947 ),
 ( #6023, #78855, #96646, #29817 ),
 ( #96118, #47014, #70247, #103149 ),
 ( #54033, #22251, #71824, #55099 ),
 ( #62695, #38433, #45977, #21203 ),
 ( #62182, #79390, #14108, #95068 ),
 ( #104726, #70776, #95587, #30879 ),
 ( #13047, #21723, #63757, #55618 ),
 ( #88555, #14635, #47543, #6549 ),
 ( #63227, #39484, #4443, #30334 ),
 ( #29296, #37387, #86977, #4985 ),
 ( #5508, #54565, #13582, #103670 ),
 ( #46497, #71298, #35609, #78670 ),
 ( #52816, #18899, #101375, #53354 ),
 ( #94892, #21036, #53871, #3750 ),
 ( #61464, #86274, #28055, #60928 ),
 ( #10745, #3211, #85187, #19444 ),
 ( #59869, #19970, #2660, #102435 ),
 ( #28577, #93814, #11272, #85742 ),
 ( #43660, #11813, #76548, #44744 ),
 ( #68485, #94357, #78152, #52274 ),
 ( #12348, #12875, #44206, #45274 ),
 ( #102969, #77630, #27528, #77092 ),
 ( #60405, #36151, #36681, #86802 ),
 ( #45791, #69545, #62003, #92743 ),
 ( #69021, #93285, #20520, #4272 ),
 ( #4803, #101895, #37200, #70067 ),
 ( #37742, #29133, #100823, #26990 ),
 ( #51743, #84661, #58318, #98759 ),
 ( #79545, #104342, #17351, #25466 ),
 ( #104898, #71987, #24913, #105418 ),
 ( #74491, #57767, #80595, #55256 ),
 ( #91244, #63392, #75015, #50225 ),
 ( #22935, #90695, #66406, #82596 ),
 ( #66957, #96287, #39642, #5657 ),
 ( #41608, #14266, #47167, #31037 ),
 ( #99836, #64441, #49689, #99290 ),
 ( #14801, #55773, #30491, #96804 ),
 ( #6175, #13738, #88708, #566 ),
 ( #16803, #9221, #8700, #26008 ),
 ( #34085, #83126, #47695, #39108 ),
 ( #6716, #33534, #22412, #42129 ),
 ( #63917, #72512, #1110, #87656 ),
 ( #46645, #31558, #38579, #71444 ),
 ( #88181, #80068, #18419, #84196 ),
 ( #85812, #68558, #11888, #2731 ),
 ( #17880, #26531, #68009, #1661 ),
 ( #27597, #27061, #77167, #20042 ),
 ( #67488, #58871, #59945, #52890 ),
 ( #18969, #93883, #100893, #101962 ),
 ( #28122, #101444, #10292, #50734 ),
 ( #44816, #60997, #77703, #76089 ),
 ( #60479, #76619, #10811, #44274 ),
 ( #51813, #59404, #3814, #36752 ),
 ( #69614, #102508, #92810, #84726 ),
 ( #93358, #91761, #35684, #19510 ),
 ( #83644, #52344, #85257, #9751 ),
 ( #42666, #75565, #34619, #11340 ),
 ( #43729, #3281, #69090, #36221 ),
 ( #2189, #100367, #92265, #51275 ),
 ( #43204, #35139, #96011, #78223 ),
 ( #5912, #86868, #78739, #46908 ),
 ( #4873, #79811, #54446, #30766 ),
 ( #70138, #12942, #70670, #94963 ),
 ( #95469, #55511, #38326, #88451 ),
 ( #96542, #94429, #103043, #37809 ),
 ( #30223, #21616, #87399, #22673 ),
 ( #38840, #37272, #28651, #29712 ),
 ( #22136, #103562, #39375, #63109 ),
 ( #62586, #29200, #63653, #4338 ),
 ( #6439, #5405, #54988, #46393 ),
 ( #87918, #62075, #14525, #13999 ),
 ( #71703, #45344, #45863, #47435 ),
 ( #104617, #71188, #80325, #13471 ),
 ( #72253, #61537, #20589, #79283 ),
 ( #53429, #86347, #104082, #12413 ),
 ( #21100, #53935, #49018, #15601 ),
 ( #40948, #32353, #40411, #8572 ),
 ( #24787, #9097, #97053, #98638 ),
 ( #57640, #65224, #16670, #23735 ),
 ( #25326, #99168, #8035, #90562 ),
 ( #49564, #98117, #24266, #73293 ),
 ( #17223, #73839, #82471, #64183 ),
 ( #57114, #6976, #106733, #41475 ),
 ( #47957, #32882, #90028, #16134 ),
 ( #80864, #89507, #31810, #66281 ),
 ( #58188, #39893, #74362, #106189 ),
 ( #440, #33411, #91114, #65757 ),
 ( #23196, #15072, #50097, #83002 ),
 ( #48491, #81386, #42005, #81917 ),
 ( #105155, #31297, #56039, #72767 ),
 ( #88972, #105673, #64697, #97568 ),
 ( #56584, #7496, #52218, #68426 ),
 ( #50606, #59807, #92146, #75436 ),
 ( #83522, #43081, #18842, #101839 ) ),
 .UNSPECIFIED., .F., .F., .F.,
 ( 4, 3, 3, 3, 3, 3, 3, 3, 3, 3, 3, 3, 3, 3, 3, 3, 3, 3, 3, 3, 3, 3, 3, 3, 3, 3, 3, 3, 3, 3, 3, 3, 3, 3, 3, 3, 3, 3, 3, 3, 3, 3, 3, 3, 3, 3, 4 ),
 ( 4, 4 ),
 ( 0.5869767053942211987, 0.5886709324131782495, 0.5895180459226567748, 0.5903651594321354112, 0.5937536134700496238, 0.5971420675079637252, 0.5988362945269207760, 0.6005305215458779378, 0.6022247485648350995, 0.6039189755837921503, 0.6073074296217062518, 0.6090016566406633025, 0.6106958836596204643, 0.6123901106785776260, 0.6140843376975346768, 0.6174727917354488893, 0.6208612457733631018, 0.6276381538491915268, 0.6344150619250199519, 0.6411919700008482659, 0.6547457861525050049, 0.6682996023041618550, 0.6954072346074753330, 0.7089610507591320721, 0.7225148669107888111, 0.7360686830624455501, 0.7428455911382738641, 0.7496224992141022891, 0.7563994072899307142, 0.7631763153657590282, 0.7699532234415873422, 0.7767301315174157672, 0.7801185855553299797, 0.7835070395932441922, 0.7868954936311584047, 0.7885897206501155665, 0.7902839476690726173, 0.7911310611785511426, 0.7919781746880296680, 0.7928252881975081934, 0.7936724017069868298, 0.7945195152164654662, 0.7953666287259439915, 0.7970608557449010423, 0.8004493097828151438, 0.8021435368017721945, 0.8038377638207293563 ),
 ( 0.03867574233413020868, 0.7831529818502380724 ),
 .UNSPECIFIED. ) ;
#30778 = CARTESIAN_POINT ( 'NONE',  ( 89.99999999999997158, -52.00000000000000000, 196.0238439516549818 ) ) ;
#30779 = CARTESIAN_POINT ( 'NONE',  ( 15.17407431220850533, 5.000000000000004441, 6.123233995736770227E-16 ) ) ;
#30780 = CARTESIAN_POINT ( 'NONE',  ( 3.643324519380566085E-15, 34.17188553058033307, 29.75000000000000355 ) ) ;
#30781 = ADVANCED_FACE ( 'NONE', ( #45755 ), #89343, .F. ) ;
#30782 = DIRECTION ( 'NONE',  ( 0.000000000000000000, -1.000000000000000000, 0.000000000000000000 ) ) ;
#30783 = UNCERTAINTY_MEASURE_WITH_UNIT (LENGTH_MEASURE( 1.000000000000000082E-05 ), #47651, 'distance_accuracy_value', 'NONE');
#30784 = CONICAL_SURFACE ( 'NONE', #42756, 3.309500000000001663, 0.9599310885968770357 ) ;
#30785 = ORIENTED_EDGE ( 'NONE', *, *, #81041, .F. ) ;
#30786 = ORIENTED_EDGE ( 'NONE', *, *, #44327, .F. ) ;
#30787 = CARTESIAN_POINT ( 'NONE',  ( 49.64451713816125533, -18.74260289896121634, 43.46749392098310949 ) ) ;
#30788 = CARTESIAN_POINT ( 'NONE',  ( -0.5332643207086228410, 8.008635151459630563, 51.63718666259362777 ) ) ;
#30789 = EDGE_CURVE ( 'NONE', #95206, #56333, #46222, .T. ) ;
#30790 = CARTESIAN_POINT ( 'NONE',  ( -6.981089760825446078, 16.96682926832163574, -0.5312715680615397451 ) ) ;
#30791 = CARTESIAN_POINT ( 'NONE',  ( -103.7057709786833897, -38.41803280166803347, 198.6430474523727980 ) ) ;
#30792 = VERTEX_POINT ( 'NONE', #46812 ) ;
#30793 = CARTESIAN_POINT ( 'NONE',  ( 90.80408946376662982, -38.34284569562218792, 5.322705216289786989 ) ) ;
#30794 = CARTESIAN_POINT ( 'NONE',  ( 12.59533268909488868, 9.265824853558118690, -9.291863273163992076 ) ) ;
#30795 = CARTESIAN_POINT ( 'NONE',  ( -19.35499308550004471, 49.90508958054942212, 61.16028107596535079 ) ) ;
#30796 = CARTESIAN_POINT ( 'NONE',  ( 100.0064967486124772, -37.84851846554567345, 139.8641161912917426 ) ) ;
#30797 = CARTESIAN_POINT ( 'NONE',  ( -31.52652959927143428, 438.9874841044786535, 23.28591655054718856 ) ) ;
#30798 = CARTESIAN_POINT ( 'NONE',  ( 22.57912246414751678, 28.20550200792851214, 30.87816999938226914 ) ) ;
#30799 = CARTESIAN_POINT ( 'NONE',  ( 32.22503847990213899, 485.9064490506210632, 4.829857536092947434 ) ) ;
#30800 = CARTESIAN_POINT ( 'NONE',  ( -32.70825224878974780, 489.1175319723178632, 10.34480600318775068 ) ) ;
#30801 = CARTESIAN_POINT ( 'NONE',  ( 10.50000000000000000, -5.000000000000000000, -34.12705337366765690 ) ) ;
#30802 = VECTOR ( 'NONE', #81776, 1000.000000000000000 ) ;
#30803 = CARTESIAN_POINT ( 'NONE',  ( 87.43192352441741377, -60.00000000000000711, 201.1725596287192275 ) ) ;
#30804 = VECTOR ( 'NONE', #92625, 1000.000000000000000 ) ;
#30805 = DIRECTION ( 'NONE',  ( -1.000000000000000000, -1.224606353822377258E-16, -0.000000000000000000 ) ) ;
#30806 = EDGE_LOOP ( 'NONE', ( #41793, #65332, #98543, #20365, #14038 ) ) ;
#30807 = CARTESIAN_POINT ( 'NONE',  ( 57.09735546842818366, -29.08113214485917197, 60.54316683975517321 ) ) ;
#30808 = CARTESIAN_POINT ( 'NONE',  ( -36.99835872953581628, 303.9880970021415578, -7.907733237980351326 ) ) ;
#30809 = EDGE_CURVE ( 'NONE', #26618, #17716, #29607, .T. ) ;
#30810 = LINE ( 'NONE', #21654, #86099 ) ;
#30811 = CARTESIAN_POINT ( 'NONE',  ( -7.896254658894418021, 26.21070817245799489, 1.307282859663298158 ) ) ;
#30812 = ORIENTED_EDGE ( 'NONE', *, *, #18177, .F. ) ;
#30814 = CARTESIAN_POINT ( 'NONE',  ( -9.960739174314243272, -50.12849100989416939, 26.07695415532590033 ) ) ;
#30813 = CARTESIAN_POINT ( 'NONE',  ( -101.1906192923223102, -38.45514854918585712, 200.0682938694438064 ) ) ;
#30815 = CARTESIAN_POINT ( 'NONE',  ( 0.000000000000000000, 34.19642918197134662, 0.000000000000000000 ) ) ;
#30816 = CARTESIAN_POINT ( 'NONE',  ( 20.09500326397664693, 304.8432866292113772, 8.935189372041850930 ) ) ;
#30817 = CARTESIAN_POINT ( 'NONE',  ( 38.56577463025284658, 437.0885780681464325, 4.837144025084519683 ) ) ;
#30818 = CARTESIAN_POINT ( 'NONE',  ( -3.313708498984765161, -32.46875000000000000, 7.999999999999998224 ) ) ;
#30819 = VECTOR ( 'NONE', #79529, 1000.000000000000000 ) ;
#30820 = CARTESIAN_POINT ( 'NONE',  ( -5.036189802311180408, -3.000000000000002665, -93.73786388412156612 ) ) ;
#30821 = CONICAL_SURFACE ( 'NONE', #22191, 4.000000000000001776, 0.9599310885968774798 ) ;
#30822 = CIRCLE ( 'NONE', #46343, 6.499999999999999112 ) ;
#30823 = FILL_AREA_STYLE ('',( #70721 ) ) ;
#30824 = ORIENTED_EDGE ( 'NONE', *, *, #89055, .T. ) ;
#30825 = CARTESIAN_POINT ( 'NONE',  ( 81.01602980331753656, -60.51226052367474040, 183.3185133159588531 ) ) ;
#30826 = CARTESIAN_POINT ( 'NONE',  ( 9.609486011791426918, 143.0915023496523020, 0.000000000000000000 ) ) ;
#30827 = CARTESIAN_POINT ( 'NONE',  ( -34.80007552946424454, 439.6089305507155132, 24.02984928258333142 ) ) ;
#30828 = ORIENTED_EDGE ( 'NONE', *, *, #81717, .T. ) ;
#30829 = CARTESIAN_POINT ( 'NONE',  ( -37.65940170220832783, 425.4627519512775393, 5.785112291392917605 ) ) ;
#30830 = CARTESIAN_POINT ( 'NONE',  ( 6.106525010887531302, -4.373161893764474506, -16.80699797897928605 ) ) ;
#30831 = CARTESIAN_POINT ( 'NONE',  ( 41.51027627991900459, 460.7143023130748816, 2.893840913533772152 ) ) ;
#30832 = DIRECTION ( 'NONE',  ( -1.000000000000000000, -1.224606353822377258E-16, -0.000000000000000000 ) ) ;
#30833 = CARTESIAN_POINT ( 'NONE',  ( -34.85541380047497739, 42.62464468236102988, -62.58172836409449502 ) ) ;
#30834 = CYLINDRICAL_SURFACE ( 'NONE', #33677, 4.000000000000000000 ) ;
#30835 = EDGE_CURVE ( 'NONE', #94772, #3167, #25546, .T. ) ;
#30836 = ORIENTED_EDGE ( 'NONE', *, *, #34953, .F. ) ;
#30837 = B_SPLINE_CURVE_WITH_KNOTS ( 'NONE', 3,
 ( #58937, #100442, #100972, #17418 ),
 .UNSPECIFIED., .F., .F.,
 ( 4, 4 ),
 ( 0.000000000000000000, 0.002847824002212700611 ),
 .UNSPECIFIED. ) ;
#30838 = CIRCLE ( 'NONE', #13542, 11.18527996897366528 ) ;
#30839 = CARTESIAN_POINT ( 'NONE',  ( 41.82792046605465686, 0.000000000000000000, 5.000000000000002665 ) ) ;
#30840 = CARTESIAN_POINT ( 'NONE',  ( 1.004575945865165298, 25.89076660835915789, 38.75180407462256937 ) ) ;
#30843 = CIRCLE ( 'NONE', #36020, 8.857142857142855874 ) ;
#30842 = CARTESIAN_POINT ( 'NONE',  ( -12.80299720903387772, 18.86371276137014874, -8.118784003668798377 ) ) ;
#30841 = DIRECTION ( 'NONE',  ( 0.000000000000000000, 1.000000000000000000, 0.000000000000000000 ) ) ;
#30844 =( GEOMETRIC_REPRESENTATION_CONTEXT ( 3 ) GLOBAL_UNCERTAINTY_ASSIGNED_CONTEXT ( ( #33334 ) ) GLOBAL_UNIT_ASSIGNED_CONTEXT ( ( #92893, #34699, #67574 ) ) REPRESENTATION_CONTEXT ( 'NONE', 'WORKASPACE' ) );
#30845 = CARTESIAN_POINT ( 'NONE',  ( -7.188101187500002709, -18.31250000204838457, 2.977408999572648707 ) ) ;
#30846 = CARTESIAN_POINT ( 'NONE',  ( -28.62002530331259109, 18.65065574497671719, -40.19565755993163947 ) ) ;
#30847 = CARTESIAN_POINT ( 'NONE',  ( -6.738100187484505454, 41.71798639774085160, -59.05424569925489209 ) ) ;
#30848 = AXIS2_PLACEMENT_3D ( 'NONE', #18558, #42805, #68702 ) ;
#30849 = ORIENTED_EDGE ( 'NONE', *, *, #35001, .F. ) ;
#30850 = FACE_BOUND ( 'NONE', #18254, .T. ) ;
#30851 = DIRECTION ( 'NONE',  ( -1.000000000000000000, 0.000000000000000000, 0.000000000000000000 ) ) ;
#30852 = CARTESIAN_POINT ( 'NONE',  ( -4.248647703895898964, 140.2890219024546354, -5.000000000000000000 ) ) ;
#30853 = B_SPLINE_CURVE_WITH_KNOTS ( 'NONE', 3,
 ( #58442, #51923, #76200, #34729, #84838, #684, #9330, #91350, #10921, #99950, #43841, #33646, #84308, #67069, #68673, #59510, #17464, #50329, #100479, #83236, #26639, #91866 ),
 .UNSPECIFIED., .F., .F.,
 ( 4, 2, 2, 2, 2, 2, 2, 2, 2, 2, 4 ),
 ( 0.002967698420317519022, 0.003472853738152583466, 0.003978009055987647910, 0.004230586714905180783, 0.004483164373822715390, 0.004988319691657781135, 0.005493475009492846881, 0.005746052668410379753, 0.005998630327327913493, 0.006503785645162972300, 0.007008940962998030239 ),
 .UNSPECIFIED. ) ;
#30854 = CARTESIAN_POINT ( 'NONE',  ( -5.693345023042894582, -5.000000000008853362, -71.09407786876178648 ) ) ;
#30855 = ADVANCED_FACE ( 'NONE', ( #71607 ), #96109, .T. ) ;
#30856 = DIRECTION ( 'NONE',  ( 0.000000000000000000, 0.000000000000000000, -1.000000000000000000 ) ) ;
#30857 = ORIENTED_EDGE ( 'NONE', *, *, #34126, .T. ) ;
#30858 = DIRECTION ( 'NONE',  ( -0.5735764363510512664, 0.8191520442889881348, 1.003171929053520309E-16 ) ) ;
#30859 = DIRECTION ( 'NONE',  ( -1.000000000000000000, -1.224606353822377258E-16, -0.000000000000000000 ) ) ;
#30860 = ORIENTED_EDGE ( 'NONE', *, *, #34019, .T. ) ;
#30861 =( BOUNDED_SURFACE ( )  B_SPLINE_SURFACE ( 3, 2, ( 
 ( #73190, #25786, #98020 ),
 ( #90463, #66726, #24172 ),
 ( #81286, #17123, #72676 ),
 ( #31717, #99065, #106094 ) ),
 .UNSPECIFIED., .F., .F., .F. ) 
 B_SPLINE_SURFACE_WITH_KNOTS ( ( 4, 4 ),
 ( 3, 3 ),
 ( -9.974659986866640793E-18, 0.002066227528073599946 ),
 ( 0.000000000000000000, 1.000000000000000000 ),
 .UNSPECIFIED. ) 
 GEOMETRIC_REPRESENTATION_ITEM ( )  RATIONAL_B_SPLINE_SURFACE ( (
 ( 1.000000000000000000, 0.7788880963805091540, 1.000000000000000000),
 ( 1.000000000000000000, 0.7743040464398368572, 1.000000000000000000),
 ( 1.000000000000000000, 0.7669333544817394932, 1.000000000000000000),
 ( 1.000000000000000000, 0.7583909709669780508, 1.000000000000000000) ) ) 
 REPRESENTATION_ITEM ( '' )  SURFACE ( )  );
#30862 = EDGE_CURVE ( 'NONE', #90581, #62158, #62480, .T. ) ;
#30863 = CARTESIAN_POINT ( 'NONE',  ( -2.120783755321927533, -0.2152620591958233909, 102.5525762030299859 ) ) ;
#30864 = FACE_OUTER_BOUND ( 'NONE', #1704, .T. ) ;
#30865 = PRESENTATION_STYLE_ASSIGNMENT (( #63210 ) ) ;
#30866 = UNCERTAINTY_MEASURE_WITH_UNIT (LENGTH_MEASURE( 1.000000000000000082E-05 ), #11343, 'distance_accuracy_value', 'NONE');
#30867 = CARTESIAN_POINT ( 'NONE',  ( -112.1945380839098192, -60.00000000000000000, 169.8055786374723084 ) ) ;
#30868 = LINE ( 'NONE', #62169, #63469 ) ;
#30869 = CARTESIAN_POINT ( 'NONE',  ( 6.536663219763930499, 53.53350969017542127, -7.404483222291337263 ) ) ;
#30870 =( BOUNDED_CURVE ( )  B_SPLINE_CURVE ( 2, ( #71160, #4310, #69590, #29171, #102481, #13445, #45838, #21072, #95442 ),
 .UNSPECIFIED., .F., .F. ) 
 B_SPLINE_CURVE_WITH_KNOTS ( ( 3, 2, 2, 2, 3 ),
 ( 0.3088235294117646634, 0.3161764705882352255, 0.3235294117647058432, 0.3308823529411764053, 0.3382352941176470229 ),
 .UNSPECIFIED. ) 
 CURVE ( )  GEOMETRIC_REPRESENTATION_ITEM ( )  RATIONAL_B_SPLINE_CURVE ( ( 1.000000000000000666, 0.9238795325112861834, 1.000000000000000000, 0.9238795325112867385, 1.000000000000000000, 0.9238795325112867385, 1.000000000000000000, 0.9238795325112872936, 0.9999999999999994449 ) ) 
 REPRESENTATION_ITEM ( '' )  );
#30871 = AXIS2_PLACEMENT_3D ( 'NONE', #21522, #4248, #45767 ) ;
#30872 = CARTESIAN_POINT ( 'NONE',  ( -82.62937363827076354, -50.03007458202083058, 181.3268356314227390 ) ) ;
#30873 = ORIENTED_EDGE ( 'NONE', *, *, #19474, .T. ) ;
#30874 = CARTESIAN_POINT ( 'NONE',  ( 40.59093392777655396, 41.82284918420663899, -54.69669182410383002 ) ) ;
#30875 = EDGE_CURVE ( 'NONE', #81388, #49340, #22139, .T. ) ;
#30876 = EDGE_LOOP ( 'NONE', ( #64713, #51994, #69068, #52341 ) ) ;
#30877 = PRESENTATION_STYLE_ASSIGNMENT (( #14105 ) ) ;
#30878 = CARTESIAN_POINT ( 'NONE',  ( 4.814352310392310486, -66.79678594103575051, -3.583053941560743194 ) ) ;
#30879 = CARTESIAN_POINT ( 'NONE',  ( -82.71436517315559911, -37.82479280323671844, 22.06480504041530466 ) ) ;
#30880 = DIRECTION ( 'NONE',  ( 0.000000000000000000, -1.000000000000000000, 0.000000000000000000 ) ) ;
#30881 = SURFACE_STYLE_FILL_AREA ( #104730 ) ;
#30882 = CARTESIAN_POINT ( 'NONE',  ( 9.300689189976395710, 11.36225021102802124, -5.000000000000920153 ) ) ;
#30883 = CARTESIAN_POINT ( 'NONE',  ( 0.1306530452038089374, 5.952467836904150822, -5.690023276062396107 ) ) ;
#30884 = AXIS2_PLACEMENT_3D ( 'NONE', #78285, #20107, #95027 ) ;
#30885 = CARTESIAN_POINT ( 'NONE',  ( 79.57068731991196842, -14.21045842199434794, 190.0104166006057085 ) ) ;
#30886 = CARTESIAN_POINT ( 'NONE',  ( -96.14371828217340976, -60.00000000000000711, 39.43406270914149303 ) ) ;
#30887 = CARTESIAN_POINT ( 'NONE',  ( -66.03000109903794623, -39.48590419423089060, 89.23932064986095725 ) ) ;
#30888 = ORIENTED_EDGE ( 'NONE', *, *, #15027, .T. ) ;
#30889 = CARTESIAN_POINT ( 'NONE',  ( 20.52959122607359532, 39.42505975791698347, 61.74424966332777842 ) ) ;
#30890 = CARTESIAN_POINT ( 'NONE',  ( 85.17823266485417832, -60.00000000000981970, 202.9514142658082960 ) ) ;
#30891 = CONICAL_SURFACE ( 'NONE', #53271, 3.400000000000000355, 0.9599310885968748153 ) ;
#30892 = ORIENTED_EDGE ( 'NONE', *, *, #22212, .F. ) ;
#30893 = CARTESIAN_POINT ( 'NONE',  ( 5.511955672705553421E-05, -56.87793864768104157, 33.36930640088255728 ) ) ;
#30894 = AXIS2_PLACEMENT_3D ( 'NONE', #69254, #35847, #2889 ) ;
#30895 = CARTESIAN_POINT ( 'NONE',  ( 7.188101187500000044, -16.53125000204838813, 0.000000000000000000 ) ) ;
#30896 = CARTESIAN_POINT ( 'NONE',  ( 32.89392925376883170, 485.8745504892934832, 5.316642333858703218 ) ) ;
#30897 = ORIENTED_EDGE ( 'NONE', *, *, #103365, .T. ) ;
#30898 = CARTESIAN_POINT ( 'NONE',  ( 52.56483885390523625, 48.00000000000000000, -38.23529411764706509 ) ) ;
#30899 = VERTEX_POINT ( 'NONE', #86240 ) ;
#30900 = DIRECTION ( 'NONE',  ( 0.000000000000000000, -1.000000000000000000, 0.000000000000000000 ) ) ;
#30901 = DIRECTION ( 'NONE',  ( 1.000000000000000000, 0.000000000000000000, 0.000000000000000000 ) ) ;
#30902 = CARTESIAN_POINT ( 'NONE',  ( -100.2951002466030417, -60.00000000000001421, 201.7966096354651029 ) ) ;
#30903 = CARTESIAN_POINT ( 'NONE',  ( 16.05785784214672773, 4.775831776474238843, 3.710403933782425057 ) ) ;
#30904 = CARTESIAN_POINT ( 'NONE',  ( 5.082755093536324154, -24.21875000204838813, 5.082755093536326818 ) ) ;
#30905 = DIRECTION ( 'NONE',  ( 0.000000000000000000, 0.000000000000000000, -1.000000000000000000 ) ) ;
#30906 = CARTESIAN_POINT ( 'NONE',  ( -32.82269234420702730, 485.2607240917816966, 5.823166218282519679 ) ) ;
#30907 = CARTESIAN_POINT ( 'NONE',  ( 1.000000000000000000, -70.02076148470871431, 13.01198664878534750 ) ) ;
#30908 = CARTESIAN_POINT ( 'NONE',  ( -1.308996937480702005, 48.00000000000000000, -75.00000000000001421 ) ) ;
#30909 = FACE_OUTER_BOUND ( 'NONE', #18329, .T. ) ;
#30910 = EDGE_CURVE ( 'NONE', #16452, #36720, #99555, .T. ) ;
#30911 = CARTESIAN_POINT ( 'NONE',  ( 97.47675437802963927, -60.00000000000000000, 196.6138812136176739 ) ) ;
#30912 = CARTESIAN_POINT ( 'NONE',  ( -37.92269680623696360, -36.05438877271811293, 36.40206401741252051 ) ) ;
#30913 = AXIS2_PLACEMENT_3D ( 'NONE', #88419, #12383, #30739 ) ;
#30914 = VERTEX_POINT ( 'NONE', #95371 ) ;
#30915 = CARTESIAN_POINT ( 'NONE',  ( -38.26360760319844445, 461.1057584915775465, 2.390039129069520207 ) ) ;
#30916 = CARTESIAN_POINT ( 'NONE',  ( 37.55314937966022626, -29.13011038508879125, 34.70950243149740544 ) ) ;
#30917 = CARTESIAN_POINT ( 'NONE',  ( 19.43146043915153953, -2.602085213965209853E-15, -11.19959342722011364 ) ) ;
#30918 = ORIENTED_EDGE ( 'NONE', *, *, #55419, .F. ) ;
#30919 = ADVANCED_FACE ( 'NONE', ( #37706 ), #5304, .F. ) ;
#30920 = EDGE_CURVE ( 'NONE', #75440, #35999, #3102, .T. ) ;
#30921 = CARTESIAN_POINT ( 'NONE',  ( 34.88900972248876542, 464.6206820656010450, 18.69027339340470562 ) ) ;
#30922 = CARTESIAN_POINT ( 'NONE',  ( -73.79179841926161032, -38.32627029603643365, 158.6094216522652971 ) ) ;
#30923 = ORIENTED_EDGE ( 'NONE', *, *, #40000, .T. ) ;
#30925 = CARTESIAN_POINT ( 'NONE',  ( -27.97565635352651015, 315.9216507687758053, 12.64980990155120999 ) ) ;
#30924 = DIRECTION ( 'NONE',  ( -1.000000000000000000, -0.000000000000000000, -0.000000000000000000 ) ) ;
#30926 = DIRECTION ( 'NONE',  ( -0.000000000000000000, 0.000000000000000000, -1.000000000000000000 ) ) ;
#30927 = CARTESIAN_POINT ( 'NONE',  ( -33.82591814952031939, 464.6968131430478479, 6.992934999028650900 ) ) ;
#30928 = CARTESIAN_POINT ( 'NONE',  ( 6.289692432696780244, 0.6618655008720334409, -6.828989928337168891 ) ) ;
#30929 = DIRECTION ( 'NONE',  ( 0.5735764363510442720, -0.8191520442889930198, 1.003171929053526349E-16 ) ) ;
#30930 = CARTESIAN_POINT ( 'NONE',  ( -48.59987877357447417, 15.38663336896752831, -14.48702310944117322 ) ) ;
#30931 = DIRECTION ( 'NONE',  ( 0.000000000000000000, -1.000000000000000000, 0.000000000000000000 ) ) ;
#30933 = EDGE_CURVE ( 'NONE', #22245, #18315, #27600, .T. ) ;
#30932 = TOROIDAL_SURFACE ( 'NONE', #20638, 10.00000000000000000, 5.000000000000000000 ) ;
#30934 = CARTESIAN_POINT ( 'NONE',  ( 94.31231819446564657, -59.99999999999999289, 43.83016036555673622 ) ) ;
#30935 = CARTESIAN_POINT ( 'NONE',  ( 0.000000000000000000, 9.237604307034020579, -1.850927914596627675E-15 ) ) ;
#30936 = FACE_OUTER_BOUND ( 'NONE', #37770, .T. ) ;
#30937 = CARTESIAN_POINT ( 'NONE',  ( -4.250000000000000000, 5.204748896376250699E-16, -6.235812796514431433 ) ) ;
#30938 = ORIENTED_EDGE ( 'NONE', *, *, #4796, .T. ) ;
#30939 = EDGE_CURVE ( 'NONE', #88504, #93532, #16893, .T. ) ;
#30940 = CARTESIAN_POINT ( 'NONE',  ( -85.06054849208743462, -29.99999999999999289, 170.9067780956840181 ) ) ;
#30941 = ORIENTED_EDGE ( 'NONE', *, *, #91080, .T. ) ;
#30942 = AXIS2_PLACEMENT_3D ( 'NONE', #7035, #64755, #9150 ) ;
#30943 = DIRECTION ( 'NONE',  ( 0.000000000000000000, -1.000000000000000000, 0.000000000000000000 ) ) ;
#30944 = CARTESIAN_POINT ( 'NONE',  ( -15.36292483821495125, 2.971926847717763831, -2.727430453969307944 ) ) ;
#30945 = CARTESIAN_POINT ( 'NONE',  ( 3.225593670035021177, 36.35169002663055693, 5.000000000000000888 ) ) ;
#30946 = CARTESIAN_POINT ( 'NONE',  ( 32.19467213680352558, 397.8364619396728585, 25.61660791817880067 ) ) ;
#30947 = CARTESIAN_POINT ( 'NONE',  ( -6.499999999999999112, 3.149025070564746898, -0.5705737632550961225 ) ) ;
#30948 = CARTESIAN_POINT ( 'NONE',  ( 7.188101187500000044, -27.03125000204838813, 0.000000000000000000 ) ) ;
#30949 = CARTESIAN_POINT ( 'NONE',  ( -44.15484044304455580, 485.1632656165609205, 0.5589787062256319494 ) ) ;
#30950 = CARTESIAN_POINT ( 'NONE',  ( -29.68315524076956891, -1.200000000000000030E-05, 40.85535821593508388 ) ) ;
#30951 = ADVANCED_FACE ( 'NONE', ( #103457 ), #11430, .F. ) ;
#30952 = CARTESIAN_POINT ( 'NONE',  ( 6.924711585765389366, 40.92328497145224020, -70.90711766198887744 ) ) ;
#30953 = ORIENTED_EDGE ( 'NONE', *, *, #37360, .F. ) ;
#30954 = AXIS2_PLACEMENT_3D ( 'NONE', #60085, #10946, #92408 ) ;
#30956 = VERTEX_POINT ( 'NONE', #48394 ) ;
#30955 = FACE_OUTER_BOUND ( 'NONE', #50324, .T. ) ;
#30957 = CARTESIAN_POINT ( 'NONE',  ( 83.08172053995880901, -25.61919862906970735, 150.1175688109731823 ) ) ;
#30958 = CIRCLE ( 'NONE', #22331, 3.309500000000007880 ) ;
#30959 = ORIENTED_EDGE ( 'NONE', *, *, #23551, .T. ) ;
#30960 = CARTESIAN_POINT ( 'NONE',  ( -12.50000000000000533, 26.94026082310467274, -44.46622975111661447 ) ) ;
#30961 = LINE ( 'NONE', #41143, #106284 ) ;
#30962 = CARTESIAN_POINT ( 'NONE',  ( -5.082755093536325042, -15.59375000204838635, -5.082755093536325930 ) ) ;
#30963 = CARTESIAN_POINT ( 'NONE',  ( 0.000000000000000000, -6.928203230275504332, 4.000000000000007105 ) ) ;
#30964 = CARTESIAN_POINT ( 'NONE',  ( -11.25203090971146302, -57.67122638729478723, 41.63652355756774881 ) ) ;
#30965 = CARTESIAN_POINT ( 'NONE',  ( 20.15799098111282461, 294.7575367430327447, 1.916962552282521548 ) ) ;
#30966 = ORIENTED_EDGE ( 'NONE', *, *, #64959, .F. ) ;
#30967 = DIRECTION ( 'NONE',  ( -1.000000000000000000, -1.224606353822377258E-16, -0.000000000000000000 ) ) ;
#30968 = CIRCLE ( 'NONE', #53346, 4.172000000000001485 ) ;
#30969 = CARTESIAN_POINT ( 'NONE',  ( 7.173660666193409696, 41.42016260144754369, -58.97621127612300285 ) ) ;
#30970 = SURFACE_SIDE_STYLE ('',( #56785 ) ) ;
#30971 = ORIENTED_EDGE ( 'NONE', *, *, #44988, .T. ) ;
#30972 = CARTESIAN_POINT ( 'NONE',  ( 3.313708498984762496, -12.96875000409676915, 7.999999999999998224 ) ) ;
#30973 = CARTESIAN_POINT ( 'NONE',  ( -19.29186002098929364, -16.81175181876205471, 31.48980669193186799 ) ) ;
#30974 = CARTESIAN_POINT ( 'NONE',  ( -40.80890826771884861, 489.2901651173327764, 10.52137389376217058 ) ) ;
#30975 = CIRCLE ( 'NONE', #61764, 4.250000000000000000 ) ;
#30976 = CARTESIAN_POINT ( 'NONE',  ( 0.5695365293531072792, 51.31240171329326216, -10.11587879637332854 ) ) ;
#30977 = CARTESIAN_POINT ( 'NONE',  ( 7.500000000000001776, 25.40357082213843753, -43.84441647605142123 ) ) ;
#30978 = FACE_OUTER_BOUND ( 'NONE', #36924, .T. ) ;
#30979 = APPLICATION_PROTOCOL_DEFINITION ( 'draft international standard', 'automotive_design', 1998, #100980 ) ;
#30980 = CARTESIAN_POINT ( 'NONE',  ( -11.70587015981644186, -8.262194459278509484, 19.31689096126753924 ) ) ;
#30981 = VERTEX_POINT ( 'NONE', #65658 ) ;
#30982 = DIRECTION ( 'NONE',  ( 0.000000000000000000, 0.000000000000000000, 1.000000000000000000 ) ) ;
#30983 = CARTESIAN_POINT ( 'NONE',  ( 6.123233995736772199E-16, 15.00000000000000000, 9.999999999999998224 ) ) ;
#30984 = CARTESIAN_POINT ( 'NONE',  ( 0.000000000000000000, 0.000000000000000000, 0.000000000000000000 ) ) ;
#30985 = CARTESIAN_POINT ( 'NONE',  ( -64.27136633399638299, -37.82663551496658982, -33.04686093788494361 ) ) ;
#30986 = CARTESIAN_POINT ( 'NONE',  ( -62.59165975746622479, -30.00000000000000355, 73.59412878083956855 ) ) ;
#30987 = CARTESIAN_POINT ( 'NONE',  ( 22.25669491856071858, 1.482358050883964840E-15, 0.000000000000000000 ) ) ;
#30988 = ADVANCED_FACE ( 'NONE', ( #99604 ), #7401, .T. ) ;
#30989 = AXIS2_PLACEMENT_3D ( 'NONE', #27322, #99007, #66128 ) ;
#30990 = ORIENTED_EDGE ( 'NONE', *, *, #74554, .F. ) ;
#30991 = AXIS2_PLACEMENT_3D ( 'NONE', #31623, #62395, #87731 ) ;
#30992 = CARTESIAN_POINT ( 'NONE',  ( 1.530808498934191324E-16, -1.200000000000000030E-05, -10.24999999999999822 ) ) ;
#30993 = CARTESIAN_POINT ( 'NONE',  ( 108.7532849881359738, -57.66361498164450694, 198.0832724003855105 ) ) ;
#30994 = CARTESIAN_POINT ( 'NONE',  ( 59.17992575935892319, -34.58953265655708975, -25.51721825149453693 ) ) ;
#30995 = ADVANCED_FACE ( 'NONE', ( #49456 ), #80618, .T. ) ;
#30996 = DIRECTION ( 'NONE',  ( 0.000000000000000000, -1.224646799147353700E-16, 1.000000000000000000 ) ) ;
#30997 = CARTESIAN_POINT ( 'NONE',  ( -15.66340762197392777, 21.48519827103249824, 5.204287273233059175 ) ) ;
#30998 = CARTESIAN_POINT ( 'NONE',  ( 0.3173508448886502298, -5.375634714784614410, 6.689127551062007626 ) ) ;
#30999 = CARTESIAN_POINT ( 'NONE',  ( -74.80069672659014657, -59.99999999999999289, 179.7118729274451425 ) ) ;
#31000 = CARTESIAN_POINT ( 'NONE',  ( -43.00000000000000000, 436.5989882784185170, 19.94133085611150591 ) ) ;
#31001 = CIRCLE ( 'NONE', #27546, 1.000000000000000888 ) ;
#31002 = CARTESIAN_POINT ( 'NONE',  ( -39.04923757934999884, 49.99999999997997691, 52.30342408740197158 ) ) ;
#31003 = CARTESIAN_POINT ( 'NONE',  ( -86.26451976794668042, -21.18125813129296020, 178.9885725162824599 ) ) ;
#31004 = ORIENTED_EDGE ( 'NONE', *, *, #53322, .F. ) ;
#31005 = CARTESIAN_POINT ( 'NONE',  ( 36.51687796781347828, 361.6932586242723460, 2.830374312397382575 ) ) ;
#31006 = ADVANCED_FACE ( 'NONE', ( #105575 ), #58081, .F. ) ;
#31007 =( BOUNDED_SURFACE ( )  B_SPLINE_SURFACE ( 2, 3, ( 
 ( #43208, #101448, #10813, #59949 ),
 ( #27065, #61002, #1664, #76093 ),
 ( #76622, #34621, #2733, #68563 ) ),
 .UNSPECIFIED., .F., .F., .F. ) 
 B_SPLINE_SURFACE_WITH_KNOTS ( ( 3, 3 ),
 ( 4, 4 ),
 ( 0.000000000000000000, 1.000000000000000000 ),
 ( -0.003055531191629554024, 0.000000000000000000 ),
 .UNSPECIFIED. ) 
 GEOMETRIC_REPRESENTATION_ITEM ( )  RATIONAL_B_SPLINE_SURFACE ( (
 ( 1.000000000000000000, 1.000000000000000000, 1.000000000000000000, 1.000000000000000000),
 ( 1.857142857142858317, 1.857142857142858317, 1.857142857142858317, 1.857142857142858317),
 ( 1.000000000000000000, 1.000000000000000000, 1.000000000000000000, 1.000000000000000000) ) ) 
 REPRESENTATION_ITEM ( '' )  SURFACE ( )  );
#31008 = VECTOR ( 'NONE', #94721, 1000.000000000000227 ) ;
#31009 = EDGE_LOOP ( 'NONE', ( #44251, #38942, #32990, #60260, #90939 ) ) ;
#31010 = LINE ( 'NONE', #47144, #95637 ) ;
#31011 = CARTESIAN_POINT ( 'NONE',  ( 2.898330757982067934E-15, 60.00000000000000000, -23.66666666666665719 ) ) ;
#31012 = B_SPLINE_CURVE_WITH_KNOTS ( 'NONE', 3,
 ( #52316, #13442, #70639, #12384 ),
 .UNSPECIFIED., .F., .F.,
 ( 4, 4 ),
 ( 0.000000000000000000, 0.0005776816123925365568 ),
 .UNSPECIFIED. ) ;
#31013 = CARTESIAN_POINT ( 'NONE',  ( 41.35127657993756856, 489.6199665183289653, 10.83744867395911982 ) ) ;
#31014 = AXIS2_PLACEMENT_3D ( 'NONE', #20245, #28316, #29384 ) ;
#31015 = CARTESIAN_POINT ( 'NONE',  ( -32.85155332502864667, 463.8111683108725174, 7.359358840565846549 ) ) ;
#31016 = CARTESIAN_POINT ( 'NONE',  ( -6.928203230275510549, 30.00000000000000000, 4.000000000000000000 ) ) ;
#31017 = ORIENTED_EDGE ( 'NONE', *, *, #94440, .T. ) ;
#31018 = CARTESIAN_POINT ( 'NONE',  ( 17.94500235637391938, 50.00000000000001421, 61.96179675157436151 ) ) ;
#31019 = CARTESIAN_POINT ( 'NONE',  ( 13.92274006198912950, 2.731168379989813211, 5.554047545514793072 ) ) ;
#31020 = CARTESIAN_POINT ( 'NONE',  ( -23.21751746555168339, 27.38103382803512176, 33.20617127781681432 ) ) ;
#31021 = CARTESIAN_POINT ( 'NONE',  ( -32.42656933073506309, 485.5064012031770631, 3.828740380151607781 ) ) ;
#31022 = CIRCLE ( 'NONE', #39627, 4.000000000000000888 ) ;
#31023 = CARTESIAN_POINT ( 'NONE',  ( 93.17370000506844008, -59.99999999999994316, -17.95777172718301173 ) ) ;
#31024 = CARTESIAN_POINT ( 'NONE',  ( -76.84998475036370280, -60.31673342858857012, 147.9117224744258579 ) ) ;
#31025 = EDGE_LOOP ( 'NONE', ( #8467, #16136, #89407, #20985, #66465 ) ) ;
#31026 = CARTESIAN_POINT ( 'NONE',  ( 35.94918560889485093, -14.21045842199434439, 40.02951443902858841 ) ) ;
#31027 = SURFACE_SIDE_STYLE ('',( #87647 ) ) ;
#31028 = CARTESIAN_POINT ( 'NONE',  ( 109.0603063891997095, -57.66547707161688407, 197.6446080142187895 ) ) ;
#31029 = LINE ( 'NONE', #81636, #56098 ) ;
#31030 = CARTESIAN_POINT ( 'NONE',  ( 36.17363157034238696, 304.2818952488495370, 0.1746411899071270979 ) ) ;
#31031 = VECTOR ( 'NONE', #37520, 1000.000000000000227 ) ;
#31032 = CARTESIAN_POINT ( 'NONE',  ( -12.67601371193146420, 9.116793994832203651, 9.219871167800874900 ) ) ;
#31033 = EDGE_LOOP ( 'NONE', ( #15354, #91600, #32166, #103228, #71721, #93595 ) ) ;
#31034 = CARTESIAN_POINT ( 'NONE',  ( 7.499999999999999112, 3.639598441879750901, -0.7155132341745242819 ) ) ;
#31035 =( LENGTH_UNIT ( ) NAMED_UNIT ( * ) SI_UNIT ( .MILLI., .METRE. ) );
#31037 = CARTESIAN_POINT ( 'NONE',  ( -101.1956550818799769, -37.82070586317561833, 149.2949577844976545 ) ) ;
#31036 = CARTESIAN_POINT ( 'NONE',  ( -16.00313894029476458, 43.99315672246724773, -88.49932133476114871 ) ) ;
#31038 = CARTESIAN_POINT ( 'NONE',  ( -7.188101187500002709, -18.31250000204838457, 2.977408999572648707 ) ) ;
#31039 = CARTESIAN_POINT ( 'NONE',  ( 43.35553785602063215, 484.2706869240204810, -0.02741892261372324072 ) ) ;
#31040 = DIRECTION ( 'NONE',  ( 0.000000000000000000, 1.000000000000000000, 0.000000000000000000 ) ) ;
#31041 = CARTESIAN_POINT ( 'NONE',  ( 1.250969861546604722, 34.50283871661307700, 28.81357323150970018 ) ) ;
#31042 = CARTESIAN_POINT ( 'NONE',  ( -33.84761347220299399, 488.7471039746336032, 11.01988148152527103 ) ) ;
#31043 = DIRECTION ( 'NONE',  ( 0.000000000000000000, 1.000000000000000000, 0.000000000000000000 ) ) ;
#31044 = EDGE_CURVE ( 'NONE', #51980, #85207, #42828, .T. ) ;
#31045 = B_SPLINE_CURVE_WITH_KNOTS ( 'NONE', 3,
 ( #46811, #45754, #87284, #53835 ),
 .UNSPECIFIED., .F., .F.,
 ( 4, 4 ),
 ( 0.000000000000000000, 0.001795780652499570293 ),
 .UNSPECIFIED. ) ;
#31046 = ORIENTED_EDGE ( 'NONE', *, *, #57990, .T. ) ;
#31047 = DIRECTION ( 'NONE',  ( -1.000000000000000000, -1.224606353822377258E-16, -0.000000000000000000 ) ) ;
#31049 = CARTESIAN_POINT ( 'NONE',  ( 24.27759548268132406, -22.08292253087573798, 28.63655142963175493 ) ) ;
#31048 = CARTESIAN_POINT ( 'NONE',  ( 54.03872891708841308, 6.856755485862130937E-15, 0.000000000000000000 ) ) ;
#31050 = AXIS2_PLACEMENT_3D ( 'NONE', #28204, #11964, #62150 ) ;
#31051 = CARTESIAN_POINT ( 'NONE',  ( -24.32060867053207076, 25.57659486167563756, 31.28716424263922846 ) ) ;
#31052 = ORIENTED_EDGE ( 'NONE', *, *, #2102, .T. ) ;
#31053 = EDGE_CURVE ( 'NONE', #62342, #17301, #71288, .T. ) ;
#31054 = EDGE_CURVE ( 'NONE', #28006, #52756, #5578, .T. ) ;
#31055 = UNCERTAINTY_MEASURE_WITH_UNIT (LENGTH_MEASURE( 1.000000000000000082E-05 ), #3067, 'distance_accuracy_value', 'NONE');
#31056 = B_SPLINE_CURVE_WITH_KNOTS ( 'NONE', 3,
 ( #60438, #53389, #27019, #101923, #60959, #67970, #100327, #10255, #2693, #4299, #93843, #37234, #26490, #35643, #2150, #59363, #92225, #84156, #76049, #43167 ),
 .UNSPECIFIED., .F., .F.,
 ( 4, 2, 2, 2, 2, 2, 2, 2, 2, 4 ),
 ( 0.003111094938513713805, 0.003615343640734996339, 0.004119592342956278005, 0.004623841045177561407, 0.005128089747398843073, 0.005380214098509484774, 0.005632338449620125607, 0.006136587151841411611, 0.006640835854062701084, 0.007145084556283989689 ),
 .UNSPECIFIED. ) ;
#31057 = VERTEX_POINT ( 'NONE', #104384 ) ;
#31059 = FACE_OUTER_BOUND ( 'NONE', #87700, .T. ) ;
#31058 = CARTESIAN_POINT ( 'NONE',  ( 43.71297783477844234, 485.1278128289774827, -1.116606130290200172 ) ) ;
#31060 = CARTESIAN_POINT ( 'NONE',  ( 15.17407431220850533, -5.000000000000000000, 0.000000000000000000 ) ) ;
#31061 = CARTESIAN_POINT ( 'NONE',  ( -43.68737779332776228, 464.3703856682102469, 8.648249337457524888 ) ) ;
#31062 = CARTESIAN_POINT ( 'NONE',  ( 40.59999999999999432, -3.309499999999999886, 0.000000000000000000 ) ) ;
#31063 = LINE ( 'NONE', #91393, #51749 ) ;
#31064 = CARTESIAN_POINT ( 'NONE',  ( 80.40000000000000568, 4.172000000000019249, 0.000000000000000000 ) ) ;
#31065 = ORIENTED_EDGE ( 'NONE', *, *, #38903, .T. ) ;
#31066 = CARTESIAN_POINT ( 'NONE',  ( 49.46860733447498149, -59.99999999999999289, -38.00840947334077669 ) ) ;
#31067 = CARTESIAN_POINT ( 'NONE',  ( 87.31629069312508307, -29.99999999999992184, 184.8944350655740720 ) ) ;
#31068 = CARTESIAN_POINT ( 'NONE',  ( -0.000000000000000000, 60.76237703744687479, -11.80995232570204045 ) ) ;
#31069 = CARTESIAN_POINT ( 'NONE',  ( -7.360438360694240956, -5.000000000000000000, -94.60993813356640203 ) ) ;
#31070 = EDGE_CURVE ( 'NONE', #39760, #43850, #12720, .T. ) ;
#31071 = CARTESIAN_POINT ( 'NONE',  ( 46.77673112620454532, 13.57592939483829220, -15.58267473267858350 ) ) ;
#31072 = EDGE_LOOP ( 'NONE', ( #75949, #88971 ) ) ;
#31073 = VECTOR ( 'NONE', #99707, 1000.000000000000114 ) ;
#31074 = VERTEX_POINT ( 'NONE', #45122 ) ;
#31075 = VERTEX_POINT ( 'NONE', #54762 ) ;
#31076 = CARTESIAN_POINT ( 'NONE',  ( 48.44486421332393178, 38.95340677879040925, -41.63464694080630579 ) ) ;
#31077 = CARTESIAN_POINT ( 'NONE',  ( -34.82215666917964825, 439.1572798958988528, 24.08424788675419848 ) ) ;
#31078 = CARTESIAN_POINT ( 'NONE',  ( 32.88833697125316746, 356.1062394740008017, 21.81815766810190027 ) ) ;
#31079 = CARTESIAN_POINT ( 'NONE',  ( -44.17677142954600100, 334.0173847572560817, -0.5134196407643211169 ) ) ;
#31080 = CARTESIAN_POINT ( 'NONE',  ( 32.39813942120852630, 439.6661968104010043, 24.00603005215503316 ) ) ;
#31081 = CARTESIAN_POINT ( 'NONE',  ( -44.05377772243112844, 485.6975038926928505, 3.984329897971015111 ) ) ;
#31082 = CARTESIAN_POINT ( 'NONE',  ( 48.02835407290544367, -1.200000000000000030E-05, 16.85535821593427386 ) ) ;
#31084 = ORIENTED_EDGE ( 'NONE', *, *, #106243, .T. ) ;
#31083 = CIRCLE ( 'NONE', #67237, 4.000000000000000888 ) ;
#31085 = DIRECTION ( 'NONE',  ( 0.000000000000000000, 1.000000000000000000, 0.000000000000000000 ) ) ;
#31086 = ORIENTED_EDGE ( 'NONE', *, *, #78702, .T. ) ;
#31087 = DIRECTION ( 'NONE',  ( 0.000000000000000000, 1.000000000000000000, 0.000000000000000000 ) ) ;
#31088 = DIRECTION ( 'NONE',  ( -1.000000000000000000, -1.224606353822377258E-16, -0.000000000000000000 ) ) ;
#31089 = CARTESIAN_POINT ( 'NONE',  ( -38.47428897412150661, 485.7788508071988076, -4.770630528146577731 ) ) ;
#31090 = EDGE_CURVE ( 'NONE', #79890, #16749, #82473, .T. ) ;
#31091 = FACE_OUTER_BOUND ( 'NONE', #2692, .T. ) ;
#31092 = CARTESIAN_POINT ( 'NONE',  ( 63.09060442939562563, -32.53182640883167664, 77.17087058294897872 ) ) ;
#31093 = ORIENTED_EDGE ( 'NONE', *, *, #65219, .F. ) ;
#31094 = STYLED_ITEM ( 'NONE', ( #13500 ), #80288 ) ;
#31095 = DIRECTION ( 'NONE',  ( -0.000000000000000000, 1.000000000000000000, 0.000000000000000000 ) ) ;
#31096 = LINE ( 'NONE', #56363, #74701 ) ;
#31097 = AXIS2_PLACEMENT_3D ( 'NONE', #26565, #27094, #99873 ) ;
#31098 = LINE ( 'NONE', #81182, #10215 ) ;
#31099 = ORIENTED_EDGE ( 'NONE', *, *, #11140, .F. ) ;
#31100 = STYLED_ITEM ( 'NONE', ( #7439 ), #78669 ) ;
#31101 = CARTESIAN_POINT ( 'NONE',  ( 0.000000000000000000, 0.000000000000000000, -2.342872917771300578 ) ) ;
#31102 = CARTESIAN_POINT ( 'NONE',  ( 7.500000000000006217, 39.99999999999942446, -59.88032989331673406 ) ) ;
#31103 = CARTESIAN_POINT ( 'NONE',  ( 3.313708498984762052, -27.40625000409676915, -8.000000000000000000 ) ) ;
#31104 = CARTESIAN_POINT ( 'NONE',  ( 7.137815226410160641, -3.000000000000000000, -4.175893272574602300 ) ) ;
#31105 = CARTESIAN_POINT ( 'NONE',  ( 86.80239051670210415, -28.05175165373529822, 186.1822811582222812 ) ) ;
#31106 = CARTESIAN_POINT ( 'NONE',  ( 75.30000000000001137, 0.000000000000000000, 3.309499999999999886 ) ) ;
#31107 = COLOUR_RGB ( '', 0.31764706, 0.68627451, 0.89019608) ;
#31108 = CARTESIAN_POINT ( 'NONE',  ( -4.659683500038751980, 8.173702696792386035, 5.000000000000000000 ) ) ;
#31109 = CARTESIAN_POINT ( 'NONE',  ( 93.97977184163765685, 1.030564683017419500E-14, 0.000000000000000000 ) ) ;
#31110 = CARTESIAN_POINT ( 'NONE',  ( 18.93091876528353623, 304.6959338034921529, 9.903868442296822394 ) ) ;
#31111 = ORIENTED_EDGE ( 'NONE', *, *, #106328, .T. ) ;
#31112 = SURFACE_STYLE_FILL_AREA ( #81716 ) ;
#31113 = DIRECTION ( 'NONE',  ( -1.000000000000000000, -1.224606353822377258E-16, -0.000000000000000000 ) ) ;
#31114 = CARTESIAN_POINT ( 'NONE',  ( 20.63737383274147419, -60.00000000000001421, 40.30261454582264236 ) ) ;
#31115 = CARTESIAN_POINT ( 'NONE',  ( -99.81090197708762446, -30.00000000000000000, 186.3697714946532358 ) ) ;
#31116 = EDGE_CURVE ( 'NONE', #11237, #7939, #22512, .T. ) ;
#31117 = CARTESIAN_POINT ( 'NONE',  ( 20.19615384615384457, -4.171999999999999709, 0.000000000000000000 ) ) ;
#31118 = CARTESIAN_POINT ( 'NONE',  ( 44.03287093842978805, -57.68433743212944620, 63.10718159453834630 ) ) ;
#31119 = STYLED_ITEM ( 'NONE', ( #89050 ), #91858 ) ;
#31121 = SURFACE_STYLE_FILL_AREA ( #87742 ) ;
#31120 = CARTESIAN_POINT ( 'NONE',  ( -0.4140831102887818638, 26.05273726750685981, -38.31762812124991058 ) ) ;
#31122 = EDGE_CURVE ( 'NONE', #99083, #73940, #63432, .T. ) ;
#31123 = ADVANCED_FACE ( 'NONE', ( #70447 ), #27407, .T. ) ;
#31124 = CARTESIAN_POINT ( 'NONE',  ( -52.56491209535032993, 39.42572890908717653, -38.23519342730720183 ) ) ;
#31125 = VECTOR ( 'NONE', #7405, 1000.000000000000000 ) ;
#31126 = CARTESIAN_POINT ( 'NONE',  ( -30.00000000000000355, 461.9311049912134877, 11.83317730145777702 ) ) ;
#31127 = CARTESIAN_POINT ( 'NONE',  ( -9.999999999999998224, 15.23416508905887490, 0.7060372491548249085 ) ) ;
#31128 = CARTESIAN_POINT ( 'NONE',  ( -21.11529628636797540, -60.00000000000000000, 40.37737908323012448 ) ) ;
#31129 = CARTESIAN_POINT ( 'NONE',  ( 0.3289898188424446035, -69.52447499062914460, 12.72735422194733879 ) ) ;
#31130 = ORIENTED_EDGE ( 'NONE', *, *, #80811, .F. ) ;
#31131 =( NAMED_UNIT ( * ) SI_UNIT ( $, .STERADIAN. ) SOLID_ANGLE_UNIT ( ) );
#31132 = CARTESIAN_POINT ( 'NONE',  ( -13.42288265799313685, -35.99464357137680537, 29.96928068455888905 ) ) ;
#31133 = EDGE_CURVE ( 'NONE', #89868, #30746, #46171, .T. ) ;
#31135 = FILL_AREA_STYLE_COLOUR ( '', #16394 ) ;
#31134 = CARTESIAN_POINT ( 'NONE',  ( -86.20182090415494258, -60.00000000000003553, 6.671171230388342366 ) ) ;
#31136 = ORIENTED_EDGE ( 'NONE', *, *, #73474, .F. ) ;
#31137 = CIRCLE ( 'NONE', #79298, 4.000000000000000888 ) ;
#31138 = CARTESIAN_POINT ( 'NONE',  ( 25.85214958460326429, 35.07651433957570930, 8.662971501749767711 ) ) ;
#31139 = CARTESIAN_POINT ( 'NONE',  ( -5.073014709117809495, -4.333232302193168906, -17.09748285339908946 ) ) ;
#31140 = CARTESIAN_POINT ( 'NONE',  ( 21.84999999999999787, 1.533819458162526451E-15, 0.000000000000000000 ) ) ;
#31141 = CARTESIAN_POINT ( 'NONE',  ( -10.50000000000000711, -5.000000000000000000, -77.33514508527181874 ) ) ;
#31142 = DIRECTION ( 'NONE',  ( 0.000000000000000000, -1.000000000000000000, 0.000000000000000000 ) ) ;
#31143 = CARTESIAN_POINT ( 'NONE',  ( 73.72526574475637062, -60.00000000000001421, 169.4364817653470539 ) ) ;
#31144 = CARTESIAN_POINT ( 'NONE',  ( -0.8386384795610041243, 54.17551965392264179, -8.069541871738774574 ) ) ;
#31145 = ORIENTED_EDGE ( 'NONE', *, *, #91225, .F. ) ;
#31146 = CARTESIAN_POINT ( 'NONE',  ( 0.000000000000000000, 0.000000000000000000, -0.02540000000000007530 ) ) ;
#31147 = DIRECTION ( 'NONE',  ( -1.000000000000000000, -0.000000000000000000, -0.000000000000000000 ) ) ;
#31149 = DIRECTION ( 'NONE',  ( -1.000000000000000000, -1.224606353822377258E-16, -0.000000000000000000 ) ) ;
#31148 = CARTESIAN_POINT ( 'NONE',  ( 4.277780656302746287, -59.99999999999995737, 41.98959578111988122 ) ) ;
#31150 = DIRECTION ( 'NONE',  ( 0.000000000000000000, -0.000000000000000000, 1.000000000000000000 ) ) ;
#31151 = EDGE_LOOP ( 'NONE', ( #25461, #29393, #40198 ) ) ;
#31152 = AXIS2_PLACEMENT_3D ( 'NONE', #88094, #32531, #31473 ) ;
#31153 = CARTESIAN_POINT ( 'NONE',  ( -30.19359820436435626, 332.6063179250270991, 15.69166344793225853 ) ) ;
#31154 = ORIENTED_EDGE ( 'NONE', *, *, #41725, .F. ) ;
#31155 = DIRECTION ( 'NONE',  ( -0.000000000000000000, -1.000000000000000000, -0.000000000000000000 ) ) ;
#31156 = CIRCLE ( 'NONE', #93183, 4.000000000000000888 ) ;
#31157 = DIRECTION ( 'NONE',  ( 0.000000000000000000, 0.000000000000000000, 1.000000000000000000 ) ) ;
#31158 = DIRECTION ( 'NONE',  ( 0.000000000000000000, -1.000000000000000000, 0.000000000000000000 ) ) ;
#31159 = ORIENTED_EDGE ( 'NONE', *, *, #13378, .T. ) ;
#31160 = DIRECTION ( 'NONE',  ( -0.000000000000000000, 1.000000000000000000, 0.000000000000000000 ) ) ;
#31161 = CARTESIAN_POINT ( 'NONE',  ( -9.896734177125578569, 7.425145793380092840, -1.133793817387026337 ) ) ;
#31162 = CARTESIAN_POINT ( 'NONE',  ( -112.6191437711416796, -60.00000000000245848, 190.6377985708280676 ) ) ;
#31163 = CIRCLE ( 'NONE', #86281, 5.000000000000000000 ) ;
#31164 = CARTESIAN_POINT ( 'NONE',  ( 6.291746522141163922, 1.386194408032345615, -6.829127798246563685 ) ) ;
#31165 = CARTESIAN_POINT ( 'NONE',  ( 48.53038198857916541, -59.99999999999997868, 68.24634254656791654 ) ) ;
#31166 = CARTESIAN_POINT ( 'NONE',  ( 30.00000000000000000, 0.000000000000000000, 8.000000000000007105 ) ) ;
#31167 = CARTESIAN_POINT ( 'NONE',  ( 0.1687358743861622490, 25.16821295365203071, -40.75000000000001421 ) ) ;
#31168 = AXIS2_PLACEMENT_3D ( 'NONE', #73277, #24249, #98098 ) ;
#31170 = CARTESIAN_POINT ( 'NONE',  ( 12.13045461104100298, -18.58664849654226359, 27.03410863527348695 ) ) ;
#31169 = CARTESIAN_POINT ( 'NONE',  ( -114.5724197576058714, -60.00000000000000000, 174.9505165961822684 ) ) ;
#31171 = CARTESIAN_POINT ( 'NONE',  ( 97.88801951303621252, -38.00000000000009237, 192.5957827294996321 ) ) ;
#31172 = CARTESIAN_POINT ( 'NONE',  ( 29.68315524077034340, 18.29184282782460969, 39.60535821593451544 ) ) ;
#31173 = EDGE_CURVE ( 'NONE', #95054, #92720, #21916, .T. ) ;
#31174 = CARTESIAN_POINT ( 'NONE',  ( -44.14030560050159835, -49.89427143720936186, 45.35222468316599986 ) ) ;
#31175 = AXIS2_PLACEMENT_3D ( 'NONE', #77085, #33460, #66334 ) ;
#31176 = CARTESIAN_POINT ( 'NONE',  ( 6.079546931269272925, -62.81856771641567150, 14.38824559419034799 ) ) ;
#31177 = VERTEX_POINT ( 'NONE', #22452 ) ;
#31178 = DIRECTION ( 'NONE',  ( 1.000000000000000000, -0.000000000000000000, -0.000000000000000000 ) ) ;
#31179 = CARTESIAN_POINT ( 'NONE',  ( -0.6188199107750348427, 18.48321454451371082, 49.41007108123974945 ) ) ;
#31180 = CARTESIAN_POINT ( 'NONE',  ( 2.500000000000003109, -19.94872423595276700, -28.09930031681329154 ) ) ;
#31181 = CARTESIAN_POINT ( 'NONE',  ( 6.812123203431564633, 304.7372914378963173, -10.02434013685850012 ) ) ;
#31182 = CARTESIAN_POINT ( 'NONE',  ( 31.00389226642222340, 485.8187364282109115, 14.27494812388583512 ) ) ;
#31183 = ORIENTED_EDGE ( 'NONE', *, *, #18444, .T. ) ;
#31184 = CARTESIAN_POINT ( 'NONE',  ( -9.283512820355584338, -2.882884900155469943, 14.75241131180710319 ) ) ;
#31185 = ORIENTED_EDGE ( 'NONE', *, *, #2232, .T. ) ;
#31186 = CARTESIAN_POINT ( 'NONE',  ( 104.6012708058323994, -30.00000000000270362, 195.8924596499454651 ) ) ;
#31187 = CARTESIAN_POINT ( 'NONE',  ( 46.00000000000000711, 461.5044003753988591, 9.500280912739080819 ) ) ;
#31188 = CARTESIAN_POINT ( 'NONE',  ( 6.417056588697860775, 41.92969932971389824, -59.44199684604556211 ) ) ;
#31189 = CARTESIAN_POINT ( 'NONE',  ( -3.673202536116901758E-15, 1.005902684993158047, -14.99698745252234566 ) ) ;
#31190 = CARTESIAN_POINT ( 'NONE',  ( 95.54465322637203428, -30.00000000000000355, 121.3526640118945892 ) ) ;
#31191 = EDGE_CURVE ( 'NONE', #85207, #98535, #104718, .T. ) ;
#31192 = CARTESIAN_POINT ( 'NONE',  ( -0.8413420114633378688, 36.41305800915415603, 29.42807188061774681 ) ) ;
#31193 = ORIENTED_EDGE ( 'NONE', *, *, #95616, .T. ) ;
#31194 = CIRCLE ( 'NONE', #12437, 1.000000000000000888 ) ;
#31195 = VERTEX_POINT ( 'NONE', #39150 ) ;
#31196 = ORIENTED_EDGE ( 'NONE', *, *, #84778, .F. ) ;
#31197 = CARTESIAN_POINT ( 'NONE',  ( -27.42501128590891568, 36.50037190240711737, 10.02642919151490553 ) ) ;
#31198 = DIRECTION ( 'NONE',  ( -1.000000000000000000, -1.224606353822377258E-16, -0.000000000000000000 ) ) ;
#31199 = CARTESIAN_POINT ( 'NONE',  ( -46.00000000000000000, 461.6622277975411635, 10.18145404766348783 ) ) ;
#31200 = VERTEX_POINT ( 'NONE', #102272 ) ;
#31201 = CARTESIAN_POINT ( 'NONE',  ( -16.05785784214673484, 4.775831776474317891, -3.710403933782548513 ) ) ;
#31202 = CIRCLE ( 'NONE', #32956, 8.000000000000000000 ) ;
#31203 = ORIENTED_EDGE ( 'NONE', *, *, #61722, .F. ) ;
#31204 = DIRECTION ( 'NONE',  ( 1.000000000000000000, 0.000000000000000000, 0.000000000000000000 ) ) ;
#31205 = CARTESIAN_POINT ( 'NONE',  ( 78.22497488676229693, -38.60204001542046370, 188.9231901909346618 ) ) ;
#31206 = FACE_OUTER_BOUND ( 'NONE', #44685, .T. ) ;
#31207 = CARTESIAN_POINT ( 'NONE',  ( 84.22446622427618479, -45.28768642902152664, -0.5874579490476177224 ) ) ;
#31208 = CARTESIAN_POINT ( 'NONE',  ( 85.73618404534279591, -38.00000000000005684, 185.6577708967697617 ) ) ;
#31209 = CARTESIAN_POINT ( 'NONE',  ( 35.11261897330833648, 305.4840936023398967, 12.42931627445148379 ) ) ;
#31210 = CARTESIAN_POINT ( 'NONE',  ( 42.18756898894605456, 484.4522853017719513, -2.425645685620597014 ) ) ;
#31211 = ADVANCED_FACE ( 'NONE', ( #95783 ), #103124, .T. ) ;
#31212 = CARTESIAN_POINT ( 'NONE',  ( -32.22503847990287795, 485.9064490506194716, 4.829857536089223302 ) ) ;
#31213 = DIRECTION ( 'NONE',  ( 0.000000000000000000, -1.000000000000000000, 0.000000000000000000 ) ) ;
#31214 = EDGE_LOOP ( 'NONE', ( #51126, #81635, #854, #10865 ) ) ;
#31215 = ADVANCED_FACE ( 'NONE', ( #90068 ), #55521, .F. ) ;
#31216 = FACE_OUTER_BOUND ( 'NONE', #59919, .T. ) ;
#31217 = CARTESIAN_POINT ( 'NONE',  ( -35.44533458431160255, 462.1326274906116964, 4.365931901573204321 ) ) ;
#31218 = AXIS2_PLACEMENT_3D ( 'NONE', #101334, #100258, #52773 ) ;
#31219 = CARTESIAN_POINT ( 'NONE',  ( -4.262243690392171658, 11.54664116576832988, 4.999999999999999112 ) ) ;
#31220 = EDGE_LOOP ( 'NONE', ( #89963, #55510 ) ) ;
#31221 = CARTESIAN_POINT ( 'NONE',  ( -35.53880766297544369, 395.9677348675359667, 6.885462253420658207 ) ) ;
#31222 = CARTESIAN_POINT ( 'NONE',  ( -25.74576498548020709, 305.2861965535228137, 10.48332055224852866 ) ) ;
#31223 = CARTESIAN_POINT ( 'NONE',  ( -12.18578101332841612, -4.618505902438846178, -76.80411978101685122 ) ) ;
#31224 = UNCERTAINTY_MEASURE_WITH_UNIT (LENGTH_MEASURE( 1.000000000000000082E-05 ), #21703, 'distance_accuracy_value', 'NONE');
#31225 = CARTESIAN_POINT ( 'NONE',  ( -89.99999999999997158, 500000.0000000000582, 188.5238439516623146 ) ) ;
#31226 = CARTESIAN_POINT ( 'NONE',  ( -5.656854249492381470, -14.56249999999999289, 5.656854249492379694 ) ) ;
#31227 = CARTESIAN_POINT ( 'NONE',  ( -3.250000000000002220, 5.629165124598849879, -5.592027715088708995 ) ) ;
#31228 = FACE_OUTER_BOUND ( 'NONE', #27547, .T. ) ;
#31229 = ORIENTED_EDGE ( 'NONE', *, *, #39756, .F. ) ;
#31230 = CARTESIAN_POINT ( 'NONE',  ( 85.48340152300438888, -35.70049165519398571, 183.4273707390578920 ) ) ;
#31231 = DIRECTION ( 'NONE',  ( 0.000000000000000000, -0.000000000000000000, 1.000000000000000000 ) ) ;
#31232 = ORIENTED_EDGE ( 'NONE', *, *, #68203, .F. ) ;
#31233 = CARTESIAN_POINT ( 'NONE',  ( 93.86032054255686319, -57.67368490835236372, 14.83889430886123151 ) ) ;
#31234 = AXIS2_PLACEMENT_3D ( 'NONE', #53976, #94473, #36792 ) ;
#31235 = CARTESIAN_POINT ( 'NONE',  ( 9.797174393178835518E-16, -100.0000000000000000, 8.000000000000007105 ) ) ;
#31236 = DIRECTION ( 'NONE',  ( 0.000000000000000000, 0.000000000000000000, -1.000000000000000000 ) ) ;
#31237 = CARTESIAN_POINT ( 'NONE',  ( 29.09375146990877070, 9.378808818926399837, 41.96648843557815667 ) ) ;
#31238 = CIRCLE ( 'NONE', #26093, 7.000000000000000000 ) ;
#31239 = VERTEX_POINT ( 'NONE', #5770 ) ;
#31240 = CIRCLE ( 'NONE', #45013, 5.000000000000000000 ) ;
#31241 = CARTESIAN_POINT ( 'NONE',  ( -56.97597412751945711, -38.00000000000000711, 64.03091273156307750 ) ) ;
#31242 = CARTESIAN_POINT ( 'NONE',  ( -2.094395098902536390, -3.000000000000000000, -8.000000000000000000 ) ) ;
#31243 = FACE_OUTER_BOUND ( 'NONE', #43015, .T. ) ;
#31245 = CARTESIAN_POINT ( 'NONE',  ( -12.37099948902435465, 9.735505124397592525, 9.467962123340013747 ) ) ;
#31244 = CARTESIAN_POINT ( 'NONE',  ( 2.459698528280936269, -7.240146430416073642, -0.09933465333851825008 ) ) ;
#31246 = AXIS2_PLACEMENT_3D ( 'NONE', #58114, #34944, #101251 ) ;
#31247 = CARTESIAN_POINT ( 'NONE',  ( 9.371250387798994552, 295.2890354897136262, -10.04040834969837448 ) ) ;
#31248 = CARTESIAN_POINT ( 'NONE',  ( -28.30696098233519820, 36.37587947255391896, -8.453513908488865525 ) ) ;
#31249 = B_SPLINE_CURVE_WITH_KNOTS ( 'NONE', 3,
 ( #8332, #22964, #40701, #14293, #7792, #73588 ),
 .UNSPECIFIED., .F., .F.,
 ( 4, 2, 4 ),
 ( 0.003990927807053575027, 0.005983070073873393568, 0.007975212340693212110 ),
 .UNSPECIFIED. ) ;
#31250 = CARTESIAN_POINT ( 'NONE',  ( 9.999999999999998224, 15.00000000000000000, -0.7768758660234752478 ) ) ;
#31251 = DIRECTION ( 'NONE',  ( 0.000000000000000000, 1.000000000000000000, 0.000000000000000000 ) ) ;
#31252 = CARTESIAN_POINT ( 'NONE',  ( -82.86548094586187574, -38.00000000000001421, 1.363017090156070532 ) ) ;
#31253 = ORIENTED_EDGE ( 'NONE', *, *, #87065, .F. ) ;
#31254 = CARTESIAN_POINT ( 'NONE',  ( 75.30000000000001137, 0.000000000000000000, 0.000000000000000000 ) ) ;
#31255 = PRESENTATION_STYLE_ASSIGNMENT (( #105114 ) ) ;
#31256 = ADVANCED_FACE ( 'NONE', ( #21989 ), #66578, .T. ) ;
#31257 = CARTESIAN_POINT ( 'NONE',  ( 4.503026011213025370, -64.45658137716682745, 3.965236350746919047 ) ) ;
#31258 = EDGE_CURVE ( 'NONE', #51023, #64324, #98216, .T. ) ;
#31260 = CARTESIAN_POINT ( 'NONE',  ( -41.46718496839501000, -47.40889074441435724, -31.47343794193032451 ) ) ;
#31259 = CARTESIAN_POINT ( 'NONE',  ( 45.94900261086841198, 5.000000000000003553, 0.000000000000000000 ) ) ;
#31261 = ORIENTED_EDGE ( 'NONE', *, *, #72290, .F. ) ;
#31262 = ORIENTED_EDGE ( 'NONE', *, *, #43425, .T. ) ;
#31263 = VECTOR ( 'NONE', #27737, 1000.000000000000000 ) ;
#31264 = CARTESIAN_POINT ( 'NONE',  ( 11.54066681168268715, 43.31748179290343614, -14.27987094040936178 ) ) ;
#31265 = AXIS2_PLACEMENT_3D ( 'NONE', #62021, #62534, #21560 ) ;
#31266 = LINE ( 'NONE', #15034, #90840 ) ;
#31267 = CARTESIAN_POINT ( 'NONE',  ( -92.03488671148051026, -60.00000000000000000, -13.80638005471863572 ) ) ;
#31268 = VERTEX_POINT ( 'NONE', #106304 ) ;
#31269 = CARTESIAN_POINT ( 'NONE',  ( -1.647285698089608230, 39.99999999999999289, -70.00000000000000000 ) ) ;
#31270 = DIRECTION ( 'NONE',  ( -0.000000000000000000, 1.000000000000000000, -0.000000000000000000 ) ) ;
#31271 = CARTESIAN_POINT ( 'NONE',  ( 98.78140442897466755, -45.26732928611253470, 193.4374649867567086 ) ) ;
#31273 = DIRECTION ( 'NONE',  ( 0.000000000000000000, -1.000000000000000000, 0.000000000000000000 ) ) ;
#31272 = CARTESIAN_POINT ( 'NONE',  ( 15.75384615384615294, 1.411358822780289120E-15, 0.000000000000000000 ) ) ;
#31274 = CARTESIAN_POINT ( 'NONE',  ( -81.96440918278869958, -42.97365977493816303, 165.6671748287174637 ) ) ;
#31275 = ORIENTED_EDGE ( 'NONE', *, *, #81833, .F. ) ;
#31276 = EDGE_LOOP ( 'NONE', ( #55176, #20284, #39911, #19259, #91932, #16105 ) ) ;
#31277 = ORIENTED_EDGE ( 'NONE', *, *, #67180, .F. ) ;
#31278 = CARTESIAN_POINT ( 'NONE',  ( 30.56153846153846132, 4.172000000000003261, 5.109226446042759579E-16 ) ) ;
#31279 = CARTESIAN_POINT ( 'NONE',  ( -6.386171959437410450, -11.88579060466480364, 10.72108492130440460 ) ) ;
#31280 = SURFACE_STYLE_FILL_AREA ( #95994 ) ;
#31281 = ORIENTED_EDGE ( 'NONE', *, *, #609, .F. ) ;
#31282 = CIRCLE ( 'NONE', #188, 66.00000000000000000 ) ;
#31283 = CARTESIAN_POINT ( 'NONE',  ( -9.500000000000000000, -5.000000000000000000, -20.99851272547259384 ) ) ;
#31284 =( LENGTH_UNIT ( ) NAMED_UNIT ( * ) SI_UNIT ( .MILLI., .METRE. ) );
#31285 = CARTESIAN_POINT ( 'NONE',  ( -73.23646197434321437, -57.64251361348243563, 182.9240549372742635 ) ) ;
#31286 = CARTESIAN_POINT ( 'NONE',  ( 2.723997317187916156, -49.63584449629185968, 102.8348549799726612 ) ) ;
#31287 = LINE ( 'NONE', #65212, #22086 ) ;
#31288 = CARTESIAN_POINT ( 'NONE',  ( -22.18906107735381283, 305.1406206946286943, -9.938500898754245583 ) ) ;
#31289 = CARTESIAN_POINT ( 'NONE',  ( 1.219859450172373405, 27.85995443672884875, -39.18316543001691343 ) ) ;
#31290 = CARTESIAN_POINT ( 'NONE',  ( -63.50642133866089978, -59.99999999999999289, -37.13819210229684842 ) ) ;
#31291 = CARTESIAN_POINT ( 'NONE',  ( -39.73689531673777964, -14.21045842199425735, 43.02931800076370195 ) ) ;
#31292 = EDGE_CURVE ( 'NONE', #34186, #35664, #41063, .T. ) ;
#31293 = CARTESIAN_POINT ( 'NONE',  ( -52.74279523840890960, -29.10740770686958712, 51.85141972818043143 ) ) ;
#31294 = EDGE_LOOP ( 'NONE', ( #3514, #75984, #95786, #19747, #42106 ) ) ;
#31295 = CARTESIAN_POINT ( 'NONE',  ( 43.31389755119118945, 487.3431498771903989, 8.040475431002054307 ) ) ;
#31296 = VERTEX_POINT ( 'NONE', #67477 ) ;
#31297 = CARTESIAN_POINT ( 'NONE',  ( -97.15103619198865204, -52.80984743541710458, 195.3003251582881319 ) ) ;
#31298 = CARTESIAN_POINT ( 'NONE',  ( -0.1689405702170302670, 52.17923068443690937, 7.749999999999985789 ) ) ;
#31299 = ORIENTED_EDGE ( 'NONE', *, *, #84641, .F. ) ;
#31300 = CARTESIAN_POINT ( 'NONE',  ( 19.38208173889043806, 49.92621484804256227, 61.05284527896436941 ) ) ;
#31302 = AXIS2_PLACEMENT_3D ( 'NONE', #83611, #92231, #34583 ) ;
#31301 = CARTESIAN_POINT ( 'NONE',  ( 90.70342993949924448, -38.35092529657300275, 17.86702295203266999 ) ) ;
#31303 = DIRECTION ( 'NONE',  ( -0.000000000000000000, -1.000000000000000000, -0.000000000000000000 ) ) ;
#31304 = CARTESIAN_POINT ( 'NONE',  ( -2.977408999572650039, -11.56250000204838635, -7.188101187500001821 ) ) ;
#31305 = CIRCLE ( 'NONE', #12324, 22.55262289886175964 ) ;
#31306 = CARTESIAN_POINT ( 'NONE',  ( -2.477041358201104604, 294.8392925341222508, 1.934412764169636034 ) ) ;
#31307 =( BOUNDED_CURVE ( )  B_SPLINE_CURVE ( 2, ( #103928, #30608, #39223, #72097, #64035, #26258, #67214, #822, #50993 ),
 .UNSPECIFIED., .F., .F. ) 
 B_SPLINE_CURVE_WITH_KNOTS ( ( 3, 2, 2, 2, 3 ),
 ( 0.4852941176470589313, 0.4926470588235295489, 0.5000000000000001110, 0.5073529411764706731, 0.5147058823529412352 ),
 .UNSPECIFIED. ) 
 CURVE ( )  GEOMETRIC_REPRESENTATION_ITEM ( )  RATIONAL_B_SPLINE_CURVE ( ( 0.9999999999999988898, 0.9238795325112878487, 1.000000000000000000, 0.9238795325112867385, 1.000000000000000000, 0.9238795325112867385, 1.000000000000000000, 0.9238795325112856283, 1.000000000000001110 ) ) 
 REPRESENTATION_ITEM ( '' )  );
#31308 = CARTESIAN_POINT ( 'NONE',  ( 29.98176661990081371, -5.000000000000000000, 0.000000000000000000 ) ) ;
#31310 = CARTESIAN_POINT ( 'NONE',  ( 85.86921380053233577, -29.99999999999999645, 177.6924406031379817 ) ) ;
#31309 = UNCERTAINTY_MEASURE_WITH_UNIT (LENGTH_MEASURE( 1.000000000000000082E-05 ), #15740, 'distance_accuracy_value', 'NONE');
#31311 = COLOUR_RGB ( '', 0.40784314, 0.44705882, 0.49803922) ;
#31312 = CARTESIAN_POINT ( 'NONE',  ( 19.53022819233322949, 303.7299160955794264, -10.02590801686515043 ) ) ;
#31313 = CARTESIAN_POINT ( 'NONE',  ( 4.181459352178379163, 52.13185942279471874, -6.680504396420412050 ) ) ;
#31314 = EDGE_CURVE ( 'NONE', #68586, #23322, #73765, .T. ) ;
#31315 = CARTESIAN_POINT ( 'NONE',  ( -0.1697973226534593427, 35.07848417048374046, 27.25873575795114334 ) ) ;
#31316 = LINE ( 'NONE', #29724, #62089 ) ;
#31317 = B_SPLINE_CURVE_WITH_KNOTS ( 'NONE', 3,
 ( #91913, #24557, #75181, #8330, #59026, #82757, #90859, #74120, #25079, #50903, #32647, #18044, #16975, #56872, #9923, #74649, #42831, #32102, #48777, #25631 ),
 .UNSPECIFIED., .F., .F.,
 ( 4, 2, 2, 2, 2, 2, 2, 2, 2, 4 ),
 ( 0.0009508909574247033456, 0.001455760884198638739, 0.001960630810972573915, 0.002465500737746509526, 0.002970370664520444702, 0.003475240591294379879, 0.003980110518068315055, 0.004232545481455281776, 0.004484980444842248497, 0.004989850371616175000 ),
 .UNSPECIFIED. ) ;
#31318 = VERTEX_POINT ( 'NONE', #33000 ) ;
#31319 = ORIENTED_EDGE ( 'NONE', *, *, #47652, .T. ) ;
#31320 = CARTESIAN_POINT ( 'NONE',  ( 49.55649468912712763, -42.97651784452486368, 51.16379761201464049 ) ) ;
#31321 = CARTESIAN_POINT ( 'NONE',  ( -0.1553312384537495483, 13.68574913102198742, 49.25766246113545321 ) ) ;
#31322 = CARTESIAN_POINT ( 'NONE',  ( -6.481071417163346560, 16.00509389820063078, -2.652271756153595561 ) ) ;
#31323 = CONICAL_SURFACE ( 'NONE', #74312, 4.000000000000001776, 0.9599310885968808105 ) ;
#31324 = CARTESIAN_POINT ( 'NONE',  ( -108.8742740125438075, -38.35654636151372188, 190.5310075001649466 ) ) ;
#31325 = ORIENTED_EDGE ( 'NONE', *, *, #33297, .T. ) ;
#31326 = CARTESIAN_POINT ( 'NONE',  ( 91.33800103527501335, -38.39896688930978996, -9.982889340764455000 ) ) ;
#31327 = CARTESIAN_POINT ( 'NONE',  ( 10.60657896622984175, 9.978945271511751258, -10.25335130518080007 ) ) ;
#31328 = CARTESIAN_POINT ( 'NONE',  ( -19.49484304323879513, 50.00000000000004974, 60.04171137605378306 ) ) ;
#31329 = CARTESIAN_POINT ( 'NONE',  ( 30.00000000000000355, 464.1078291054766964, 11.04693782968297100 ) ) ;
#31330 = CARTESIAN_POINT ( 'NONE',  ( 102.9432490270377514, -45.28273091632402725, 153.9878045269907432 ) ) ;
#31331 = LINE ( 'NONE', #55017, #46087 ) ;
#31332 = FILL_AREA_STYLE ('',( #90060 ) ) ;
#31333 = CARTESIAN_POINT ( 'NONE',  ( -35.42573747137001305, 370.6060757378968447, 4.789908646769843514 ) ) ;
#31334 = DIRECTION ( 'NONE',  ( 0.000000000000000000, 0.000000000000000000, 1.000000000000000000 ) ) ;
#31335 = CARTESIAN_POINT ( 'NONE',  ( 78.36952841773975820, -60.00000000000000000, 193.5507905296401532 ) ) ;
#31336 = EDGE_CURVE ( 'NONE', #63670, #105753, #54900, .T. ) ;
#31337 = CARTESIAN_POINT ( 'NONE',  ( 18.32078204077888373, 45.00000000000000711, 62.39758222047188951 ) ) ;
#31339 = VERTEX_POINT ( 'NONE', #554 ) ;
#31338 =( BOUNDED_SURFACE ( )  B_SPLINE_SURFACE ( 3, 2, ( 
 ( #7503, #6983, #14008 ),
 ( #71711, #104625, #31306 ),
 ( #16141, #40421, #88981 ),
 ( #63661, #47442, #96549 ),
 ( #64191, #24273, #22683 ),
 ( #97060, #40957, #64704 ),
 ( #80335, #47964, #6448 ),
 ( #81926, #73301, #49029 ),
 ( #106197, #23206, #32361 ),
 ( #73848, #97576, #80874 ),
 ( #39902, #72775, #30230 ),
 ( #105681, #31820, #23742 ),
 ( #65233, #56593, #98125 ),
 ( #42542, #10174, #43090 ),
 ( #100250, #32891, #18301 ),
 ( #50614, #17233, #74372 ),
 ( #65766, #74897, #99723 ),
 ( #51696, #58750, #84613 ),
 ( #91646, #24796, #449 ),
 ( #33419, #66292, #9633 ) ),
 .UNSPECIFIED., .F., .F., .F. ) 
 B_SPLINE_SURFACE_WITH_KNOTS ( ( 4, 2, 2, 2, 2, 2, 2, 2, 2, 4 ),
 ( 3, 3 ),
 ( 0.02263415075989269262, 0.02743304099212479086, 0.02983248610824084171, 0.03103220866629886887, 0.03223193122435689256, 0.03703082145658899427, 0.03763068273561800958, 0.03823054401464701796, 0.03943026657270504165, 0.04182971168882109597 ),
 ( 0.000000000000000000, 1.000000000000000000 ),
 .UNSPECIFIED. ) 
 GEOMETRIC_REPRESENTATION_ITEM ( )  RATIONAL_B_SPLINE_SURFACE ( (
 ( 1.000000000000000000, 0.7071075261727414185, 1.000000000000000000),
 ( 1.000000000000000000, 0.7071101665684027537, 1.000000000000000000),
 ( 1.000000000000000000, 0.7071141823836638585, 1.000000000000000000),
 ( 1.000000000000000000, 0.7071130896034428792, 1.000000000000000000),
 ( 1.000000000000000000, 0.7071116449877591359, 1.000000000000000000),
 ( 1.000000000000000000, 0.7071091580431273504, 1.000000000000000000),
 ( 1.000000000000000000, 0.7071082982894895119, 1.000000000000000000),
 ( 1.000000000000000000, 0.7071070358518728449, 1.000000000000000000),
 ( 1.000000000000000000, 0.7071066027193460002, 1.000000000000000000),
 ( 1.000000000000000000, 0.7071078298307942323, 1.000000000000000000),
 ( 1.000000000000000000, 0.7071068905341975075, 1.000000000000000000),
 ( 1.000000000000000000, 0.7071067685343632725, 1.000000000000000000),
 ( 1.000000000000000000, 0.7071080607249466965, 1.000000000000000000),
 ( 1.000000000000000000, 0.7071121120183785358, 1.000000000000000000),
 ( 1.000000000000000000, 0.7071147527875665251, 1.000000000000000000),
 ( 1.000000000000000000, 0.7071223063742563264, 1.000000000000000000),
 ( 1.000000000000000000, 0.7071265710165801632, 1.000000000000000000),
 ( 1.000000000000000000, 0.7071280425582433526, 1.000000000000000000),
 ( 1.000000000000000000, 0.7071102348506560498, 1.000000000000000000),
 ( 1.000000000000000000, 0.7071067811865472397, 1.000000000000000000) ) ) 
 REPRESENTATION_ITEM ( '' )  SURFACE ( )  );
#31340 = CARTESIAN_POINT ( 'NONE',  ( 55.06123850360377503, -53.37751811208404007, 66.16048837899118951 ) ) ;
#31341 = EDGE_CURVE ( 'NONE', #6815, #88199, #53156, .T. ) ;
#31342 = CARTESIAN_POINT ( 'NONE',  ( -28.00030505598783037, 305.7606182409026019, -9.353795520816204245 ) ) ;
#31343 = FACE_OUTER_BOUND ( 'NONE', #21298, .T. ) ;
#31344 = MECHANICAL_DESIGN_GEOMETRIC_PRESENTATION_REPRESENTATION (  '', ( #64047 ), #100207 ) ;
#31345 = FACE_OUTER_BOUND ( 'NONE', #82559, .T. ) ;
#31346 = ORIENTED_EDGE ( 'NONE', *, *, #92666, .F. ) ;
#31348 = CARTESIAN_POINT ( 'NONE',  ( -14.62302398986549967, 22.28582220554202920, -3.922348837399933341 ) ) ;
#31347 = CARTESIAN_POINT ( 'NONE',  ( -102.8054511067312973, -38.43301377309627753, 199.2360175344277309 ) ) ;
#31349 = DIRECTION ( 'NONE',  ( -1.000000000000000000, 0.000000000000000000, 0.000000000000000000 ) ) ;
#31350 = CARTESIAN_POINT ( 'NONE',  ( 31.36487079234788311, 435.2129478716335598, 22.89275833565512386 ) ) ;
#31351 = CARTESIAN_POINT ( 'NONE',  ( 34.35000000000000142, 1.533819458162526451E-15, 0.000000000000000000 ) ) ;
#31352 = CARTESIAN_POINT ( 'NONE',  ( -8.000000000000000000, -31.24999999999999645, -9.797174393178825657E-16 ) ) ;
#31353 = PRESENTATION_LAYER_ASSIGNMENT (  '', '', ( #22726 ) ) ;
#31354 = CARTESIAN_POINT ( 'NONE',  ( -1.570796324980114456, -5.000000000000002665, -73.00000000000001421 ) ) ;
#31355 =( GEOMETRIC_REPRESENTATION_CONTEXT ( 3 ) GLOBAL_UNCERTAINTY_ASSIGNED_CONTEXT ( ( #7322 ) ) GLOBAL_UNIT_ASSIGNED_CONTEXT ( ( #97941, #59631, #27830 ) ) REPRESENTATION_CONTEXT ( 'NONE', 'WORKASPACE' ) );
#31356 = EDGE_CURVE ( 'NONE', #64937, #28602, #98747, .T. ) ;
#31357 = CARTESIAN_POINT ( 'NONE',  ( 7.897850199329718990, -1.533397866934080422, -7.634054012537970557 ) ) ;
#31358 = ORIENTED_EDGE ( 'NONE', *, *, #58254, .F. ) ;
#31359 = CARTESIAN_POINT ( 'NONE',  ( 82.41388130231072751, -50.00333596804200909, 179.9547445588053733 ) ) ;
#31360 = DIRECTION ( 'NONE',  ( 0.000000000000000000, 0.000000000000000000, 1.000000000000000000 ) ) ;
#31361 = CARTESIAN_POINT ( 'NONE',  ( 36.35715703853927039, 28.12785541995608085, 12.56221659471220242 ) ) ;
#31362 = ORIENTED_EDGE ( 'NONE', *, *, #13042, .F. ) ;
#31363 = CARTESIAN_POINT ( 'NONE',  ( 0.000000000000000000, 47.29617335651134624, 0.000000000000000000 ) ) ;
#31364 = EDGE_CURVE ( 'NONE', #53134, #78006, #68723, .T. ) ;
#31365 =( NAMED_UNIT ( * ) PLANE_ANGLE_UNIT ( ) SI_UNIT ( $, .RADIAN. ) );
#31366 = CARTESIAN_POINT ( 'NONE',  ( 41.47568061452221144, 477.4151321979921363, -1.107586631990791437 ) ) ;
#31367 = CARTESIAN_POINT ( 'NONE',  ( 27.33349330513380337, -7.703719777548943412E-31, 4.000000000000001776 ) ) ;
#31368 =( NAMED_UNIT ( * ) SI_UNIT ( $, .STERADIAN. ) SOLID_ANGLE_UNIT ( ) );
#31369 = CARTESIAN_POINT ( 'NONE',  ( -28.53023071193248583, 11.34323491540338580, -41.35403323942997389 ) ) ;
#31370 = ORIENTED_EDGE ( 'NONE', *, *, #96592, .F. ) ;
#31371 = FILL_AREA_STYLE ('',( #105742 ) ) ;
#31372 = CARTESIAN_POINT ( 'NONE',  ( 37.56673239365841255, 27.60449318992554169, -13.45617127781092215 ) ) ;
#31373 = CARTESIAN_POINT ( 'NONE',  ( 0.9531491022388255407, 25.91474801773795633, 38.68721158006705707 ) ) ;
#31375 = CARTESIAN_POINT ( 'NONE',  ( -11.23306095913861213, 17.71175306491347712, -8.845014664451463560 ) ) ;
#31374 = CARTESIAN_POINT ( 'NONE',  ( 7.493949260784499522, 40.57568730855774675, -68.91429205858018747 ) ) ;
#31376 = CARTESIAN_POINT ( 'NONE',  ( -2.977408999572650039, -18.68750000204838102, -7.188101187500001821 ) ) ;
#31377 = CARTESIAN_POINT ( 'NONE',  ( 20.00100000000000477, 12.99999999999999289, 0.000000000000000000 ) ) ;
#31378 = LINE ( 'NONE', #55068, #43170 ) ;
#31379 = VERTEX_POINT ( 'NONE', #99825 ) ;
#31380 = STYLED_ITEM ( 'NONE', ( #96072 ), #82778 ) ;
#31381 = PRESENTATION_STYLE_ASSIGNMENT (( #104164 ) ) ;
#31382 = CARTESIAN_POINT ( 'NONE',  ( 7.500000000000000000, 3.882635837267457202, -7.781684861376771067 ) ) ;
#31383 = STYLED_ITEM ( 'NONE', ( #41148 ), #51627 ) ;
#31384 = CARTESIAN_POINT ( 'NONE',  ( -8.340816975826685464, 120.4114851256039600, 2.540892575254900838E-12 ) ) ;
#31385 = CARTESIAN_POINT ( 'NONE',  ( -7.230783190337165323, -5.000000000001424638, -70.90935357141312068 ) ) ;
#31386 = EDGE_CURVE ( 'NONE', #15028, #54088, #80686, .T. ) ;
#31387 = DIRECTION ( 'NONE',  ( -1.000000000000000000, -0.000000000000000000, -0.000000000000000000 ) ) ;
#31388 = EDGE_LOOP ( 'NONE', ( #102873, #86124, #22582, #12198, #13554, #94552 ) ) ;
#31389 = CARTESIAN_POINT ( 'NONE',  ( 47.40949999999999420, 0.000000000000000000, 4.000000000000000000 ) ) ;
#31390 = CARTESIAN_POINT ( 'NONE',  ( 0.000000000000000000, 0.000000000000000000, 0.000000000000000000 ) ) ;
#31392 = ORIENTED_EDGE ( 'NONE', *, *, #24170, .T. ) ;
#31391 = AXIS2_PLACEMENT_3D ( 'NONE', #103701, #29324, #62215 ) ;
#31393 = EDGE_CURVE ( 'NONE', #5108, #66410, #95765, .T. ) ;
#31395 = CARTESIAN_POINT ( 'NONE',  ( 0.000000000000000000, -100.0000000000000000, -8.000000000000000000 ) ) ;
#31394 = TOROIDAL_SURFACE ( 'NONE', #58939, 57.21727615095610275, 0.5000000000000000000 ) ;
#31396 = CARTESIAN_POINT ( 'NONE',  ( -43.88602474737083980, 39.35463593402870686, -47.77194135894280436 ) ) ;
#31397 = FILL_AREA_STYLE_COLOUR ( '', #23814 ) ;
#31398 = CARTESIAN_POINT ( 'NONE',  ( -110.9407563509171553, -60.00000000000000000, 151.5418352708265957 ) ) ;
#31399 = PRODUCT_DEFINITION_SHAPE ( 'NONE', 'NONE',  #106809 ) ;
#31400 = CARTESIAN_POINT ( 'NONE',  ( -15.00099999999999767, 12.99999999999999289, 0.000000000000000000 ) ) ;
#31401 = CARTESIAN_POINT ( 'NONE',  ( 30.87955015324946828, 351.7733141111877444, 20.67482462247657082 ) ) ;
#31402 = CARTESIAN_POINT ( 'NONE',  ( -32.17646412119409405, 464.6980787822278671, 10.84896803612746474 ) ) ;
#31403 = CARTESIAN_POINT ( 'NONE',  ( -7.996668422917848851, -4.999999999991826094, -91.14546720082944375 ) ) ;
#31404 = CARTESIAN_POINT ( 'NONE',  ( -82.48518652320663591, -50.01571124582150674, 180.4131216091861063 ) ) ;
#31405 = EDGE_LOOP ( 'NONE', ( #61621, #45841, #106475, #86722, #31997 ) ) ;
#31406 = VERTEX_POINT ( 'NONE', #76078 ) ;
#31407 = DIRECTION ( 'NONE',  ( -1.000000000000000000, -0.000000000000000000, -0.000000000000000000 ) ) ;
#31408 = ADVANCED_FACE ( 'NONE', ( #49677 ), #39377, .T. ) ;
#31409 = CARTESIAN_POINT ( 'NONE',  ( 33.49051768644739013, 464.3918346588610007, 8.532988796831755707 ) ) ;
#31410 = CIRCLE ( 'NONE', #50306, 0.5000000000000004441 ) ;
#31411 = FACE_BOUND ( 'NONE', #101169, .T. ) ;
#31412 = AXIS2_PLACEMENT_3D ( 'NONE', #19130, #86505, #12566 ) ;
#31413 = CARTESIAN_POINT ( 'NONE',  ( 9.240146679118391049, 12.02903014930353010, 0.000000000000000000 ) ) ;
#31414 = CARTESIAN_POINT ( 'NONE',  ( 40.59999999999999432, 1.533819458162526451E-15, 0.000000000000000000 ) ) ;
#31415 = CARTESIAN_POINT ( 'NONE',  ( 0.01688885742776662438, 6.535341423375591319, -4.680456609903973941 ) ) ;
#31416 = CARTESIAN_POINT ( 'NONE',  ( 85.76531507393636389, -14.21045842199426801, 195.9085670305863118 ) ) ;
#31417 = CARTESIAN_POINT ( 'NONE',  ( -101.4323841882945771, -14.21045842199443499, 121.1831906623697677 ) ) ;
#31418 = CONICAL_SURFACE ( 'NONE', #50313, 3.309500000000001663, 0.9599310885968770357 ) ;
#31419 = ADVANCED_FACE ( 'NONE', ( #92799 ), #18960, .T. ) ;
#31420 = CARTESIAN_POINT ( 'NONE',  ( -64.22233557390354974, -25.57930763091898640, 76.82107432232744770 ) ) ;
#31421 = VERTEX_POINT ( 'NONE', #84714 ) ;
#31422 = CARTESIAN_POINT ( 'NONE',  ( 42.77536428084039954, 38.95206598861494740, 47.52331724725532780 ) ) ;
#31423 = CARTESIAN_POINT ( 'NONE',  ( 98.39731940781094011, -60.00000000000247979, 204.7396733380437581 ) ) ;
#31424 = EDGE_LOOP ( 'NONE', ( #71591, #101299, #56423, #14956 ) ) ;
#31425 = CARTESIAN_POINT ( 'NONE',  ( 13.77155591953703961, -57.01367568605869707, 24.47427385584959225 ) ) ;
#31426 = CARTESIAN_POINT ( 'NONE',  ( 2.977408999572650927, -22.25000000204839523, -7.188101187500000933 ) ) ;
#31427 = CIRCLE ( 'NONE', #95159, 7.000000000000000000 ) ;
#31428 = CARTESIAN_POINT ( 'NONE',  ( -4.497472161260651191, -9.457774533740545664, -3.972129482042463522 ) ) ;
#31429 = VERTEX_POINT ( 'NONE', #66395 ) ;
#31430 = DIRECTION ( 'NONE',  ( 0.000000000000000000, -1.000000000000000000, 0.000000000000000000 ) ) ;
#31431 = ORIENTED_EDGE ( 'NONE', *, *, #16782, .T. ) ;
#31432 = CARTESIAN_POINT ( 'NONE',  ( 11.50618969897577948, 45.40753567543398361, -14.44225189481717031 ) ) ;
#31433 = CARTESIAN_POINT ( 'NONE',  ( -7.922281120364393914, 4.573931137438267847, -8.047472243342932430 ) ) ;
#31434 = CARTESIAN_POINT ( 'NONE',  ( -99.92409395513189452, -60.00000000000000000, 80.58707614375684614 ) ) ;
#31435 = CARTESIAN_POINT ( 'NONE',  ( 16.13647630347087514, 6.334953579828610515, 5.738861489051994447 ) ) ;
#31436 = CARTESIAN_POINT ( 'NONE',  ( -2.977408999572650039, -28.06250000204838813, -7.188101187500001821 ) ) ;
#31437 = CARTESIAN_POINT ( 'NONE',  ( 46.00000000000000000, 461.6622277975423003, 10.18145404766882933 ) ) ;
#31438 = CARTESIAN_POINT ( 'NONE',  ( -4.000000000000000000, 17.85270131633358659, -5.744562646538044604 ) ) ;
#31439 = CARTESIAN_POINT ( 'NONE',  ( 9.739726766104286781, 48.00000000000000000, -82.38252115500969808 ) ) ;
#31440 = CARTESIAN_POINT ( 'NONE',  ( 12.98335800805550022, -9.687644989897647108, 11.46374983418961691 ) ) ;
#31441 = EDGE_CURVE ( 'NONE', #62805, #54759, #82755, .T. ) ;
#31442 = CARTESIAN_POINT ( 'NONE',  ( 31.90579019990244447, 311.1086333623303517, -8.069066494172007609 ) ) ;
#31443 = CARTESIAN_POINT ( 'NONE',  ( -32.00796974007340623, -18.67729007039406497, 30.02893240338449488 ) ) ;
#31444 = VERTEX_POINT ( 'NONE', #52335 ) ;
#31445 = CARTESIAN_POINT ( 'NONE',  ( -14.75116209839012527, 43.55504285526384933, -90.22050492866908655 ) ) ;
#31446 = CARTESIAN_POINT ( 'NONE',  ( 41.77872314523253294, -29.15662253184162722, 37.78149640197655401 ) ) ;
#31447 = CARTESIAN_POINT ( 'NONE',  ( 2.723397405354400211E-15, -8.673617379884035472E-16, 22.23822744035697241 ) ) ;
#31448 = EDGE_LOOP ( 'NONE', ( #65103, #56021 ) ) ;
#31449 = CARTESIAN_POINT ( 'NONE',  ( 33.85195725564123848, 465.2464970902066739, 17.18122764674258462 ) ) ;
#31450 = CARTESIAN_POINT ( 'NONE',  ( -73.25624440150409100, -38.32611741607561839, 154.3746391340933144 ) ) ;
#31451 = EDGE_LOOP ( 'NONE', ( #105694, #33577, #7712 ) ) ;
#31453 = CARTESIAN_POINT ( 'NONE',  ( 29.07128654445882887, 296.9339959557834163, -9.548856946221640385 ) ) ;
#31452 = CARTESIAN_POINT ( 'NONE',  ( 16.84999999999999787, 1.533819458162526451E-15, 0.000000000000000000 ) ) ;
#31454 = DIRECTION ( 'NONE',  ( -0.000000000000000000, -0.000000000000000000, -1.000000000000000000 ) ) ;
#31455 = CARTESIAN_POINT ( 'NONE',  ( -33.77559172535808329, 464.7834715296605737, 7.192701217093241617 ) ) ;
#31456 = DIRECTION ( 'NONE',  ( 0.000000000000000000, 0.000000000000000000, 1.000000000000000000 ) ) ;
#31457 = CARTESIAN_POINT ( 'NONE',  ( -38.55706197334059482, 437.0914394628632635, 4.833655886046459571 ) ) ;
#31458 = CARTESIAN_POINT ( 'NONE',  ( -49.25998992636563401, 12.93544608831240161, -15.83190612885685589 ) ) ;
#31459 = CARTESIAN_POINT ( 'NONE',  ( 30.00000000000000000, 6.123233995736765296E-16, -4.999999999999999112 ) ) ;
#31460 = CARTESIAN_POINT ( 'NONE',  ( 93.34302217634724741, -59.99999999999998579, 35.60011999643739244 ) ) ;
#31461 = B_SPLINE_CURVE_WITH_KNOTS ( 'NONE', 3,
 ( #63783, #20718, #14659, #86487, #98252, #72899, #16813, #82604, #106323, #49700, #98769, #57244, #8708, #99297, #56718, #105809, #32490, #41616, #31949, #64830, #33021, #48094, #90164, #7110, #24922, #40026, #16268, #42136, #1120, #75022, #23874, #74500, #48623, #8178 ),
 .UNSPECIFIED., .F., .F.,
 ( 4, 2, 2, 2, 2, 2, 2, 2, 2, 2, 2, 2, 2, 2, 2, 2, 4 ),
 ( 0.01263964810480761557, 0.01342907106096845327, 0.01421849401712929097, 0.01500791697329012866, 0.01579733992945096810, 0.01658676288561180406, 0.01737618584177264350, 0.01816560879793347946, 0.01895503175409431890, 0.01974445471025515486, 0.02053387766641599430, 0.02132330062257683373, 0.02211272357873766969, 0.02290214653489850566, 0.02369156949105934509, 0.02448099244722018453, 0.02527041540338102049 ),
 .UNSPECIFIED. ) ;
#31463 = CARTESIAN_POINT ( 'NONE',  ( -1.722054852581828306E-15, 24.73290587908618932, -14.06164498842270483 ) ) ;
#31462 = AXIS2_PLACEMENT_3D ( 'NONE', #68488, #101377, #27530 ) ;
#31464 = CARTESIAN_POINT ( 'NONE',  ( -5.200782296141404082E-16, -0.6346842323187715795, 6.499999999999998224 ) ) ;
#31465 = DIRECTION ( 'NONE',  ( 0.000000000000000000, -0.000000000000000000, 1.000000000000000000 ) ) ;
#31466 = ORIENTED_EDGE ( 'NONE', *, *, #2571, .T. ) ;
#31467 = ADVANCED_FACE ( 'NONE', ( #11332 ), #49746, .T. ) ;
#31468 = CARTESIAN_POINT ( 'NONE',  ( -89.12256709102487662, -30.00000000000086686, -14.43968776839223800 ) ) ;
#31469 = ORIENTED_EDGE ( 'NONE', *, *, #3866, .F. ) ;
#31470 = CARTESIAN_POINT ( 'NONE',  ( -9.113097280746996987, -54.00000000000000711, 31.11721482942554928 ) ) ;
#31471 = CARTESIAN_POINT ( 'NONE',  ( -15.13304769501037050, 3.593526408006888939, 4.245863293369651181 ) ) ;
#31472 = CARTESIAN_POINT ( 'NONE',  ( 9.075061003897785028, 14.05394893824808555, 4.999999999999385381 ) ) ;
#31473 = DIRECTION ( 'NONE',  ( 0.000000000000000000, 0.000000000000000000, 1.000000000000000000 ) ) ;
#31474 = CARTESIAN_POINT ( 'NONE',  ( -22.11477862515238968, 27.78277355752724631, -32.62539941293130852 ) ) ;
#31475 = VECTOR ( 'NONE', #44569, 1000.000000000000000 ) ;
#31476 = CARTESIAN_POINT ( 'NONE',  ( 7.188101187500000044, -22.53125000204838457, 0.000000000000000000 ) ) ;
#31477 = LINE ( 'NONE', #62763, #12250 ) ;
#31479 = EDGE_CURVE ( 'NONE', #36519, #28856, #29110, .T. ) ;
#31478 = CARTESIAN_POINT ( 'NONE',  ( 7.320748848010288690, 41.41789156490656154, -68.91429206068630720 ) ) ;
#31480 = VERTEX_POINT ( 'NONE', #29189 ) ;
#31482 = ORIENTED_EDGE ( 'NONE', *, *, #96237, .T. ) ;
#31481 = DIRECTION ( 'NONE',  ( 3.469446951953614189E-16, -1.000000000000000000, 0.000000000000000000 ) ) ;
#31483 = CARTESIAN_POINT ( 'NONE',  ( 81.27861452902187978, -42.96768989124994675, 159.4987958060827111 ) ) ;
#31484 = B_SPLINE_CURVE_WITH_KNOTS ( 'NONE', 3,
 ( #20422, #3114, #93725, #85644, #69454, #75937, #11182, #2036, #36589, #102340 ),
 .UNSPECIFIED., .F., .F.,
 ( 4, 2, 2, 2, 4 ),
 ( 0.000000000000000000, 0.2500000000000000000, 0.5000000000000000000, 0.7500000000000000000, 1.000000000000000000 ),
 .UNSPECIFIED. ) ;
#31485 = CYLINDRICAL_SURFACE ( 'NONE', #98811, 7.000000000000000000 ) ;
#31486 = VERTEX_POINT ( 'NONE', #101952 ) ;
#31487 = EDGE_CURVE ( 'NONE', #28267, #99675, #36577, .T. ) ;
#31488 = CARTESIAN_POINT ( 'NONE',  ( 4.250000000000000000, 0.000000000000000000, -10.00000000000000000 ) ) ;
#31489 = CARTESIAN_POINT ( 'NONE',  ( -14.11595029532502643, 2.410436752314748521, -5.024000119269296682 ) ) ;
#31490 = CARTESIAN_POINT ( 'NONE',  ( 2.977408999572652260, -10.43750000204838457, 7.188101187500000044 ) ) ;
#31491 = LINE ( 'NONE', #49216, #41665 ) ;
#31493 = CARTESIAN_POINT ( 'NONE',  ( -24.14082041284044422, -57.67406494483144286, 42.97874410022470215 ) ) ;
#31492 = STYLED_ITEM ( 'NONE', ( #6371 ), #95952 ) ;
#31494 = CARTESIAN_POINT ( 'NONE',  ( 29.00000000000001066, 0.000000000000000000, 0.000000000000000000 ) ) ;
#31495 = EDGE_LOOP ( 'NONE', ( #101335, #33855, #99181, #15705, #21613, #16636 ) ) ;
#31496 = CARTESIAN_POINT ( 'NONE',  ( 2.849088492170980924, 81.66462479025911136, 5.000000000000000000 ) ) ;
#31497 = DIRECTION ( 'NONE',  ( 0.5735764363510557073, -0.8191520442889850262, 1.003171929053516612E-16 ) ) ;
#31498 = CARTESIAN_POINT ( 'NONE',  ( 22.61650669486618526, 1.474610560812782335E-15, 0.000000000000000000 ) ) ;
#31499 = ORIENTED_EDGE ( 'NONE', *, *, #18949, .F. ) ;
#31500 = CARTESIAN_POINT ( 'NONE',  ( 7.999999999999998224, -9.781250004096770923, 3.313708498984766493 ) ) ;
#31501 = CARTESIAN_POINT ( 'NONE',  ( -34.10647007375028039, -23.64402837878609986, 33.18254751217250487 ) ) ;
#31502 = FACE_OUTER_BOUND ( 'NONE', #64024, .T. ) ;
#31503 = CARTESIAN_POINT ( 'NONE',  ( -1.000000000000000000, -10.50453238069492912, -12.19598953690579535 ) ) ;
#31504 = CARTESIAN_POINT ( 'NONE',  ( -9.999945253488242258, 88.99986313370533253, -0.2662901834230884113 ) ) ;
#31505 = DIRECTION ( 'NONE',  ( 0.000000000000000000, -0.3420201433256725987, -0.9396926207859068736 ) ) ;
#31506 = PRODUCT_CONTEXT ( 'NONE', #89333, 'mechanical' ) ;
#31507 = CARTESIAN_POINT ( 'NONE',  ( 38.18741658151765250, 27.41008188141410074, 13.30318076387803572 ) ) ;
#31508 = ORIENTED_EDGE ( 'NONE', *, *, #100761, .F. ) ;
#31509 = CARTESIAN_POINT ( 'NONE',  ( -6.999999999318260890, -46.53316735177592278, 39.12435565337574417 ) ) ;
#31510 = CARTESIAN_POINT ( 'NONE',  ( -4.034557488803550918, 15.07443463110242199, 9.151133496028460712 ) ) ;
#31511 = CARTESIAN_POINT ( 'NONE',  ( 29.83349330513380693, 1.593028355512270962E-15, 0.000000000000000000 ) ) ;
#31512 = CARTESIAN_POINT ( 'NONE',  ( -44.13343456913869289, 464.3829732007670259, 9.622105740874530966 ) ) ;
#31513 = CARTESIAN_POINT ( 'NONE',  ( 0.000000000000000000, 0.000000000000000000, -0.5505556536572887572 ) ) ;
#31514 = SURFACE_SIDE_STYLE ('',( #33102 ) ) ;
#31515 = ADVANCED_FACE ( 'NONE', ( #37798 ), #25703, .F. ) ;
#31516 = EDGE_LOOP ( 'NONE', ( #90305, #65500, #87172, #30828, #5005, #30038, #58149, #18397 ) ) ;
#31517 = DIRECTION ( 'NONE',  ( 0.000000000000000000, -1.224646799147353700E-16, 1.000000000000000000 ) ) ;
#31518 = CARTESIAN_POINT ( 'NONE',  ( 93.70983742795966975, -57.61862147648758992, 204.5155149370983452 ) ) ;
#31519 = EDGE_CURVE ( 'NONE', #12676, #91673, #55795, .T. ) ;
#31520 = CARTESIAN_POINT ( 'NONE',  ( 34.88900972249024335, 464.6206820656014429, 18.69027339340525629 ) ) ;
#31521 = CARTESIAN_POINT ( 'NONE',  ( -16.14595037822608958, 20.23371447308013771, 4.922994507609250725 ) ) ;
#31522 = CARTESIAN_POINT ( 'NONE',  ( -5.616399669216317392, 54.12011764772116607, 6.063970369565759633 ) ) ;
#31523 = CARTESIAN_POINT ( 'NONE',  ( -74.81432347301979746, -60.00000000000002132, 179.8222036999654563 ) ) ;
#31524 = VECTOR ( 'NONE', #11752, 1000.000000000000227 ) ;
#31525 = CARTESIAN_POINT ( 'NONE',  ( -32.35336999986095208, 300.6590557721156642, 11.25190399080426751 ) ) ;
#31526 = DIRECTION ( 'NONE',  ( -0.1269898409407502204, 0.9919025243773941236, -0.001721171576547747550 ) ) ;
#31527 = CARTESIAN_POINT ( 'NONE',  ( -45.17824257314219949, 354.4244853104167987, 3.762393652172960845 ) ) ;
#31528 = CARTESIAN_POINT ( 'NONE',  ( -86.09903236225166268, -24.81206519315382764, 180.1009231137148561 ) ) ;
#31529 = VECTOR ( 'NONE', #82403, 1000.000000000000000 ) ;
#31530 = EDGE_LOOP ( 'NONE', ( #106093, #83569, #69342, #61532, #16264, #82023 ) ) ;
#31531 = CARTESIAN_POINT ( 'NONE',  ( 21.68456034400251653, 305.0468853612085240, -9.958482390678179641 ) ) ;
#31532 = AXIS2_PLACEMENT_3D ( 'NONE', #87496, #13041, #78849 ) ;
#31533 = ORIENTED_EDGE ( 'NONE', *, *, #105868, .T. ) ;
#31534 = CARTESIAN_POINT ( 'NONE',  ( 16.84999999999999787, -3.309499999999999886, 0.000000000000000000 ) ) ;
#31535 = B_SPLINE_CURVE_WITH_KNOTS ( 'NONE', 3,
 ( #55314, #56903, #89302, #88762, #88241, #14859, #89826, #40201, #90350, #24584, #5715, #15397, #73078, #7823, #105985, #30552, #97904, #48809, #81698, #40733, #74153, #25664, #90892, #50403, #17007, #34810, #67147, #42322, #9957, #18617, #76285, #50934, #42863, #66073, #84394, #49884, #67678, #17542, #83317, #2394, #1854, #10485, #75215, #43403, #25110, #98951, #82248, #35341, #75756, #1309, #9407, #68202, #93009, #101102, #41265, #83849, #92469, #18076, #51479, #58525, #26723, #19173, #100562, #59594, #57971, #27261, #236, #60145, #41795, #91944, #8364, #34270, #33203, #82790, #8891, #74682, #91431, #100029, #59057, #762, #33728, #66608, #26198, #99486, #46060, #20241, #52537, #102161, #86009, #62263, #69285, #4527, #61187, #78943, #45011, #36416, #4005, #87060, #61733, #2926, #70333, #60667, #35879, #85456, #103231, #86544, #29893, #70863, #103754, #94073, #3474, #54118, #28310, #62780, #11542, #53087, #45540, #5065, #43927, #12080, #93554, #77894, #19703, #37473, #36935, #69801, #12602, #95148, #37999, #20773, #78413, #68760, #13131, #44466, #29374, #102697, #28860, #95668, #21282, #52007, #53609, #84924, #101639, #27796, #11010, #76815, #77361, #94629, #55702, #89700, #32549, #15802, #87581, #97246, #32009, #64372, #97769, #104815, #72959, #88634, #105348, #40080, #71375, #15271, #13669, #64883, #14724, #23391, #105866, #106387, #81566, #48682, #47622, #48154, #7696, #63313, #47095, #22337, #65421, #81055, #56228, #96209, #72444, #80525, #63840, #23935, #89167, #31493, #96734, #46577, #56778, #40606, #7168, #6107, #73490, #30964, #55184, #21807, #6642, #104277 ),
 .UNSPECIFIED., .F., .F.,
 ( 4, 2, 2, 2, 2, 2, 2, 2, 2, 2, 2, 2, 2, 2, 2, 2, 2, 2, 2, 2, 2, 2, 2, 2, 2, 2, 2, 2, 2, 2, 2, 2, 2, 2, 2, 2, 2, 2, 2, 2, 2, 2, 2, 2, 2, 2, 2, 2, 2, 2, 2, 2, 2, 2, 2, 2, 2, 2, 2, 2, 2, 2, 2, 2, 2, 2, 2, 2, 2, 2, 2, 2, 2, 2, 2, 2, 2, 2, 2, 2, 2, 2, 2, 2, 2, 2, 2, 2, 2, 2, 2, 2, 2, 2, 2, 2, 2, 2, 2, 4 ),
 ( 1.408790152747874003E-05, 0.008346361953628917210, 0.01669272390725783442, 0.03338544781451566884, 0.04173180976814458432, 0.05007817172177350673, 0.05425135269858796794, 0.05842453367540242221, 0.06677089562903133768, 0.07511725758266024622, 0.07929043855947470743, 0.08346361953628916863, 0.08555021002469639924, 0.08763680051310362984, 0.09180998148991809105, 0.09389657197832532165, 0.09493986722252893695, 0.09598316246673255225, 0.09806975295513978286, 0.1001563434435470135, 0.1011996386877506288, 0.1022429339319542441, 0.1043295244203614747, 0.1085027053971759359, 0.1126758863739903971, 0.1168490673508048444, 0.1210222483276192917, 0.1251954293044337529, 0.1335417912580626754, 0.1418881532116915700, 0.1502345151653204924, 0.1669272390725783373, 0.1836199629798361821, 0.2003126868870940269, 0.2336981347016096888, 0.2503908586088675059, 0.2670835825161253507, 0.2754299444697542176, 0.2837763064233831400, 0.2921226683770120625, 0.2962958493538265237, 0.3004690303306409849, 0.3025556208190481877, 0.3046422113074554461, 0.3088153922842699073, 0.3109019827726771101, 0.3119452780168807671, 0.3129885732610843685, 0.3150751637494916269, 0.3161184589936952283, 0.3171617542378988297, 0.3192483447263060325, 0.3202916399705096895, 0.3213349352147132909, 0.3255081161915277521, 0.3265514114357313535, 0.3275947066799349550, 0.3296812971683422133, 0.3317678876567494717, 0.3338544781451566745, 0.3359410686335638774, 0.3380276591219711357, 0.3390709543661747372, 0.3401142496103783941, 0.3422008400987855969, 0.3442874305871927998, 0.3453307258313964567, 0.3463740210756000582, 0.3505472020524145194, 0.3547203830292289806, 0.3588935640060434418, 0.3630667449828579030, 0.3672399259596723642, 0.3755862879133012866, 0.3839326498669302090, 0.3922790118205591314, 0.4006253737741880538, 0.4173180976814458987, 0.4340108215887037435, 0.4507035454959615883, 0.4590499074495905107, 0.4673962694032193776, 0.4757426313568481890, 0.4799158123336627613, 0.4840889933104772225, 0.4882621742872916282, 0.4924353552641060894, 0.4945219457525132922, 0.4966085362409205506, 0.5007817172177350118, 0.5028683077061422146, 0.5039116029503458716, 0.5049548981945495285, 0.5091280791713639342, 0.5112146696597711371, 0.5133012601481783399, 0.5174744411249928566, 0.5216476221018073733, 0.5258208030786217790, 0.5341671650322507015 ),
 .UNSPECIFIED. ) ;
#31536 = ADVANCED_FACE ( 'NONE', ( #49951 ), #88633, .F. ) ;
#31537 = FACE_OUTER_BOUND ( 'NONE', #83926, .T. ) ;
#31538 = CARTESIAN_POINT ( 'NONE',  ( 42.99999999999992184, 487.9285348210859752, 8.903916466042419486 ) ) ;
#31539 = DIRECTION ( 'NONE',  ( 0.000000000000000000, 1.000000000000000000, 0.000000000000000000 ) ) ;
#31540 = CARTESIAN_POINT ( 'NONE',  ( 0.000000000000000000, -14.49999999999999822, 0.000000000000000000 ) ) ;
#31541 = ORIENTED_EDGE ( 'NONE', *, *, #99147, .F. ) ;
#31542 = CIRCLE ( 'NONE', #93510, 5.000000000000001776 ) ;
#31543 = CARTESIAN_POINT ( 'NONE',  ( 18.77149637936522097, 50.00000000000000000, 60.89551101287860746 ) ) ;
#31544 = FILL_AREA_STYLE_COLOUR ( '', #48454 ) ;
#31545 = CARTESIAN_POINT ( 'NONE',  ( 22.23822744035697241, -8.673617379884035472E-16, 2.910977163136220014 ) ) ;
#31546 = DIRECTION ( 'NONE',  ( 0.000000000000000000, -1.000000000000000000, 0.000000000000000000 ) ) ;
#31547 = CARTESIAN_POINT ( 'NONE',  ( 87.60230161701383622, -14.21045842199431064, -3.802929300262678947 ) ) ;
#31548 = CARTESIAN_POINT ( 'NONE',  ( -76.51940332190571326, -56.84804871597534515, 142.3230989425833855 ) ) ;
#31549 = VERTEX_POINT ( 'NONE', #42393 ) ;
#31550 = CARTESIAN_POINT ( 'NONE',  ( 82.31973535306708811, -57.52566952622508012, 200.7289113873300437 ) ) ;
#31551 = CARTESIAN_POINT ( 'NONE',  ( 28.31477239889190756, 34.24506016859675128, 8.451634719143738650 ) ) ;
#31552 = CARTESIAN_POINT ( 'NONE',  ( 31.44871638334648267, 310.1705813142233978, -8.300853151410109376 ) ) ;
#31553 = DIRECTION ( 'NONE',  ( -0.5735764363510494901, -0.8191520442889894671, 0.000000000000000000 ) ) ;
#31554 = ORIENTED_EDGE ( 'NONE', *, *, #2378, .T. ) ;
#31555 = PLANE ( 'NONE',  #104346 ) ;
#31556 = CARTESIAN_POINT ( 'NONE',  ( -12.49999999999999822, 0.4010732622483518806, -18.19005086670230398 ) ) ;
#31558 = CARTESIAN_POINT ( 'NONE',  ( -105.1817855895727263, -52.71030988280897134, 168.1451182041190293 ) ) ;
#31557 = DIRECTION ( 'NONE',  ( 0.000000000000000000, 0.000000000000000000, -1.000000000000000000 ) ) ;
#31559 = CARTESIAN_POINT ( 'NONE',  ( -2.977408999572650039, -17.18750000204838813, -7.188101187500001821 ) ) ;
#31560 = DIRECTION ( 'NONE',  ( -1.000000000000000000, 0.000000000000000000, 0.000000000000000000 ) ) ;
#31561 = TOROIDAL_SURFACE ( 'NONE', #22938, 12.00000000000000711, 3.000000000000000000 ) ;
#31562 = FILL_AREA_STYLE_COLOUR ( '', #67012 ) ;
#31563 = CARTESIAN_POINT ( 'NONE',  ( 3.337162542380456721E-15, 35.08181111624585213, 27.25000000000000000 ) ) ;
#31564 = PLANE ( 'NONE',  #6589 ) ;
#31565 = SURFACE_STYLE_FILL_AREA ( #80601 ) ;
#31566 = MECHANICAL_DESIGN_GEOMETRIC_PRESENTATION_REPRESENTATION (  '', ( #33246 ), #84969 ) ;
#31567 = ORIENTED_EDGE ( 'NONE', *, *, #48889, .T. ) ;
#31568 = CARTESIAN_POINT ( 'NONE',  ( -6.849721783289899335, 41.84384191736015168, -59.83401399873645232 ) ) ;
#31569 = MECHANICAL_DESIGN_GEOMETRIC_PRESENTATION_REPRESENTATION (  '', ( #17771 ), #12656 ) ;
#31571 = CARTESIAN_POINT ( 'NONE',  ( 28.68725023401711738, -29.05854980118881059, 30.85773263594263938 ) ) ;
#31570 = CARTESIAN_POINT ( 'NONE',  ( 0.3173508448886549482, 8.480771745766404024, 1.310872448937998813 ) ) ;
#31572 = DIRECTION ( 'NONE',  ( 0.000000000000000000, 1.000000000000000000, 0.000000000000000000 ) ) ;
#31573 = ORIENTED_EDGE ( 'NONE', *, *, #106064, .F. ) ;
#31574 = EDGE_LOOP ( 'NONE', ( #90495, #73478, #76843, #71080, #48950 ) ) ;
#31576 = CARTESIAN_POINT ( 'NONE',  ( -0.7866107806117342838, 43.26603872651622851, -18.48505893840705383 ) ) ;
#31575 = CARTESIAN_POINT ( 'NONE',  ( 29.66054107240687543, 6.123233995736772199E-16, -5.000000000000001776 ) ) ;
#31577 = PLANE ( 'NONE',  #92145 ) ;
#31578 = CARTESIAN_POINT ( 'NONE',  ( -44.29288495125481973, 463.9154455111743118, 8.171315969396212964 ) ) ;
#31579 = CARTESIAN_POINT ( 'NONE',  ( 14.29190075645216851, 12.99999999999999289, -10.00000000000000178 ) ) ;
#31580 = LINE ( 'NONE', #80089, #55129 ) ;
#31581 = ORIENTED_EDGE ( 'NONE', *, *, #75675, .F. ) ;
#31582 = CARTESIAN_POINT ( 'NONE',  ( 33.58349330513380693, -4.000000000000000888, 4.898587196589416773E-16 ) ) ;
#31583 = CARTESIAN_POINT ( 'NONE',  ( 85.04705102683632845, -29.99999999999995026, 170.8080372376007006 ) ) ;
#31584 = CARTESIAN_POINT ( 'NONE',  ( 0.000000000000000000, 0.000000000000000000, -5.000000000000000000 ) ) ;
#31585 = CARTESIAN_POINT ( 'NONE',  ( 0.000000000000000000, -3.331654917651224235, 0.000000000000000000 ) ) ;
#31586 = DIRECTION ( 'NONE',  ( 0.000000000000000000, 0.000000000000000000, 1.000000000000000000 ) ) ;
#31587 = EDGE_LOOP ( 'NONE', ( #46479, #33168, #49986, #35985, #38093 ) ) ;
#31588 = EDGE_CURVE ( 'NONE', #50186, #102336, #82547, .T. ) ;
#31589 = EDGE_CURVE ( 'NONE', #41440, #5773, #6709, .T. ) ;
#31590 = ORIENTED_EDGE ( 'NONE', *, *, #53506, .T. ) ;
#31591 = ORIENTED_EDGE ( 'NONE', *, *, #76974, .F. ) ;
#31592 = PRESENTATION_STYLE_ASSIGNMENT (( #25089 ) ) ;
#31593 = SURFACE_STYLE_FILL_AREA ( #7271 ) ;
#31594 = CARTESIAN_POINT ( 'NONE',  ( -40.31745201298756598, 437.2080480237208917, 22.20101732755830426 ) ) ;
#31595 = CARTESIAN_POINT ( 'NONE',  ( 21.79648701958511836, 303.1339518336154697, 9.997617627940190488 ) ) ;
#31596 = CARTESIAN_POINT ( 'NONE',  ( -43.46274389541398619, 361.0170833077261818, 12.68963403053921368 ) ) ;
#31597 = CARTESIAN_POINT ( 'NONE',  ( -2.752434797705083369, -69.16112139175940854, 12.98102957303667182 ) ) ;
#31598 = SURFACE_SIDE_STYLE ('',( #97352 ) ) ;
#31599 = LINE ( 'NONE', #46691, #20877 ) ;
#31600 = EDGE_LOOP ( 'NONE', ( #65355, #76169, #87779, #38502, #4935, #43953 ) ) ;
#31602 = ADVANCED_FACE ( 'NONE', ( #60215 ), #26793, .T. ) ;
#31601 = CARTESIAN_POINT ( 'NONE',  ( 30.00061906993038363, 12.59382690271831251, 39.64398720750875071 ) ) ;
#31603 = EDGE_LOOP ( 'NONE', ( #46807, #93864, #52139, #77457, #85576, #63803 ) ) ;
#31604 = DIRECTION ( 'NONE',  ( 0.000000000000000000, -1.000000000000000000, 0.000000000000000000 ) ) ;
#31605 = CARTESIAN_POINT ( 'NONE',  ( -6.837824896291513355, -3.947820044545450102, -6.564402953523720718 ) ) ;
#31606 = CARTESIAN_POINT ( 'NONE',  ( -39.23335254075706047, 485.6839217479342778, -4.505383133713231736 ) ) ;
#31607 = CARTESIAN_POINT ( 'NONE',  ( -2.087134204587958841, -60.00000000000000000, 33.88964995960240145 ) ) ;
#31608 = CARTESIAN_POINT ( 'NONE',  ( 64.47874323931745266, -42.95807119333815649, 86.48291114592055351 ) ) ;
#31609 = MECHANICAL_DESIGN_GEOMETRIC_PRESENTATION_REPRESENTATION (  '', ( #74595 ), #5709 ) ;
#31610 = ORIENTED_EDGE ( 'NONE', *, *, #89656, .F. ) ;
#31611 = EDGE_CURVE ( 'NONE', #27489, #100791, #101176, .T. ) ;
#31612 = CONICAL_SURFACE ( 'NONE', #52280, 5.000000000000001776, 0.9599310885968803664 ) ;
#31613 = CARTESIAN_POINT ( 'NONE',  ( -5.082755093536325042, -29.09375000204838813, -5.082755093536325930 ) ) ;
#31614 =( NAMED_UNIT ( * ) PLANE_ANGLE_UNIT ( ) SI_UNIT ( $, .RADIAN. ) );
#31615 = EDGE_LOOP ( 'NONE', ( #68307, #94407, #55805, #20426, #58670 ) ) ;
#31616 = CARTESIAN_POINT ( 'NONE',  ( 47.36618468514978986, 18.16301677597534336, 14.54218830158920639 ) ) ;
#31617 = VECTOR ( 'NONE', #79719, 1000.000000000000000 ) ;
#31618 = CARTESIAN_POINT ( 'NONE',  ( -37.49684268402597809, 491.2987049188604942, 12.22740886044745245 ) ) ;
#31619 = CARTESIAN_POINT ( 'NONE',  ( -5.656854249492381470, -32.75000000409677625, 5.656854249492379694 ) ) ;
#31620 = CARTESIAN_POINT ( 'NONE',  ( 19.34999999999999787, -3.309499999999999886, 0.000000000000000000 ) ) ;
#31621 =( LENGTH_UNIT ( ) NAMED_UNIT ( * ) SI_UNIT ( .MILLI., .METRE. ) );
#31622 = CARTESIAN_POINT ( 'NONE',  ( -10.01627249115706775, 7.476760474189255490, 5.000000000000000888 ) ) ;
#31623 = CARTESIAN_POINT ( 'NONE',  ( 12.50000000000000000, -4.999999999999997335, -14.04024970282782547 ) ) ;
#31624 = SURFACE_SIDE_STYLE ('',( #48297 ) ) ;
#31625 = ORIENTED_EDGE ( 'NONE', *, *, #28962, .F. ) ;
#31626 = DIRECTION ( 'NONE',  ( 0.000000000000000000, 1.000000000000000000, 0.000000000000000000 ) ) ;
#31627 = CARTESIAN_POINT ( 'NONE',  ( 4.898587196589412829E-16, -10.62499999999999289, -8.000000000000000000 ) ) ;
#31629 =( BOUNDED_SURFACE ( )  B_SPLINE_SURFACE ( 3, 2, ( 
 ( #13962, #63073, #12899 ),
 ( #22096, #71151, #14484 ),
 ( #104044, #6403, #70630 ),
 ( #87881, #47397, #39338 ),
 ( #103521, #80290, #79243 ),
 ( #46871, #95432, #29674 ),
 ( #62544, #21571, #71669 ),
 ( #87354, #105121, #13431 ) ),
 .UNSPECIFIED., .F., .F., .F. ) 
 B_SPLINE_SURFACE_WITH_KNOTS ( ( 4, 2, 2, 4 ),
 ( 3, 3 ),
 ( 0.03861844051980969916, 0.04325213341840641879, 0.04556897986770477860, 0.04788582631700313841 ),
 ( 0.000000000000000000, 1.000000000000000000 ),
 .UNSPECIFIED. ) 
 GEOMETRIC_REPRESENTATION_ITEM ( )  RATIONAL_B_SPLINE_SURFACE ( (
 ( 1.000000000000000000, 0.8047781759831917903, 1.000000000000000000),
 ( 1.000000000000000000, 0.8123762462806505269, 1.000000000000000000),
 ( 1.000000000000000000, 0.8190659850614816495, 1.000000000000000000),
 ( 1.000000000000000000, 0.8191937571014599184, 1.000000000000000000),
 ( 1.000000000000000000, 0.8176092952779866474, 1.000000000000000000),
 ( 1.000000000000000000, 0.8122962088597071029, 1.000000000000000000),
 ( 1.000000000000000000, 0.8086311330827505861, 1.000000000000000000),
 ( 1.000000000000000000, 0.8047712282214324331, 1.000000000000000000) ) ) 
 REPRESENTATION_ITEM ( '' )  SURFACE ( )  );
#31628 = CARTESIAN_POINT ( 'NONE',  ( 21.36556348850374221, -60.00000000000001421, 40.41599463261538006 ) ) ;
#31630 = AXIS2_PLACEMENT_3D ( 'NONE', #105074, #64099, #31213 ) ;
#31631 = CARTESIAN_POINT ( 'NONE',  ( -90.59850697782101747, -29.99999999999999289, 190.2918799463446931 ) ) ;
#31632 = EDGE_CURVE ( 'NONE', #82401, #61254, #68790, .T. ) ;
#31633 = B_SPLINE_CURVE_WITH_KNOTS ( 'NONE', 3,
 ( #17354, #105803, #23869, #56713, #64825, #32485, #31942, #80988, #49695, #41612, #50228, #89634 ),
 .UNSPECIFIED., .F., .F.,
 ( 4, 2, 2, 2, 2, 4 ),
 ( 9.300487239283920478E-15, 0.0007788392030127789254, 0.001557678406016257348, 0.001947098007517979049, 0.002336517609019700750, 0.003115356812023144586 ),
 .UNSPECIFIED. ) ;
#31634 = COLOUR_RGB ( '', 0.31764706, 0.68627451, 0.89019608) ;
#31635 = LINE ( 'NONE', #31117, #50295 ) ;
#31636 = CARTESIAN_POINT ( 'NONE',  ( 36.78581192191307281, -57.69605431621219793, 51.12723935542062037 ) ) ;
#31637 = CARTESIAN_POINT ( 'NONE',  ( -1.131308492565942458, 25.42167126197779936, -40.03766171172649280 ) ) ;
#31638 = EDGE_CURVE ( 'NONE', #59296, #60348, #15333, .T. ) ;
#31639 = ADVANCED_FACE ( 'NONE', ( #51550 ), #84463, .T. ) ;
#31640 = CARTESIAN_POINT ( 'NONE',  ( 5.199577819732106754, -21.67934222354764628, -38.54735607716909840 ) ) ;
#31641 = CARTESIAN_POINT ( 'NONE',  ( -32.31275654990349722, 464.7713635351630046, 15.30476493091208212 ) ) ;
#31642 = CARTESIAN_POINT ( 'NONE',  ( -9.216463528758735535, 15.13241195026071928, 3.884543032213891411 ) ) ;
#31643 = DIRECTION ( 'NONE',  ( 0.000000000000000000, 0.000000000000000000, -1.000000000000000000 ) ) ;
#31644 = B_SPLINE_CURVE_WITH_KNOTS ( 'NONE', 3,
 ( #92535, #18139, #74214, #67217 ),
 .UNSPECIFIED., .F., .F.,
 ( 4, 4 ),
 ( 1.734723475976807094E-18, 0.001668351617186183012 ),
 .UNSPECIFIED. ) ;
#31645 = CARTESIAN_POINT ( 'NONE',  ( -25.26314279777532690, -60.00000000000000711, 41.24176291422744356 ) ) ;
#31646 = PRESENTATION_STYLE_ASSIGNMENT (( #14887 ) ) ;
#31647 = CARTESIAN_POINT ( 'NONE',  ( -85.88498695457488452, -57.45118064709335925, 193.0270043969651397 ) ) ;
#31648 = ORIENTED_EDGE ( 'NONE', *, *, #57813, .F. ) ;
#31649 = CARTESIAN_POINT ( 'NONE',  ( 17.49999999999692690, 49.91179365273359991, 61.97298340135932193 ) ) ;
#31650 = FACE_OUTER_BOUND ( 'NONE', #97554, .T. ) ;
#31651 = CARTESIAN_POINT ( 'NONE',  ( -14.72005785463202621, -49.92084221828517343, 32.33953701706330008 ) ) ;
#31652 = DIRECTION ( 'NONE',  ( -1.000000000000000000, -0.000000000000000000, -0.000000000000000000 ) ) ;
#31653 = CYLINDRICAL_SURFACE ( 'NONE', #25940, 1.000000000000000000 ) ;
#31654 = ORIENTED_EDGE ( 'NONE', *, *, #26263, .T. ) ;
#31655 = EDGE_CURVE ( 'NONE', #44183, #88199, #71100, .T. ) ;
#31657 = CARTESIAN_POINT ( 'NONE',  ( -43.71273081481922418, 464.5191621324576658, 7.248379604737841930 ) ) ;
#31656 =( GEOMETRIC_REPRESENTATION_CONTEXT ( 3 ) GLOBAL_UNCERTAINTY_ASSIGNED_CONTEXT ( ( #56679 ) ) GLOBAL_UNIT_ASSIGNED_CONTEXT ( ( #58996, #19107, #51945 ) ) REPRESENTATION_CONTEXT ( 'NONE', 'WORKASPACE' ) );
#31658 = CARTESIAN_POINT ( 'NONE',  ( -7.270302578004622873, -3.659675574298181466, -18.03744543697015956 ) ) ;
#31659 = CARTESIAN_POINT ( 'NONE',  ( -7.550180524134850302, 33.00559247213185898, 2.651855549982496729 ) ) ;
#31660 = CARTESIAN_POINT ( 'NONE',  ( 0.000000000000000000, 0.000000000000000000, 14.00000000000000000 ) ) ;
#31661 = EDGE_CURVE ( 'NONE', #88306, #8828, #18844, .T. ) ;
#31662 = DIRECTION ( 'NONE',  ( 0.000000000000000000, 0.000000000000000000, -1.000000000000000000 ) ) ;
#31663 = CARTESIAN_POINT ( 'NONE',  ( 61.48198989113487301, -60.00000000000000000, 105.4918018471999517 ) ) ;
#31664 = CARTESIAN_POINT ( 'NONE',  ( -0.6401524832913686458, 54.23522517489366379, -7.923242704504276368 ) ) ;
#31665 = VERTEX_POINT ( 'NONE', #85536 ) ;
#31666 = CARTESIAN_POINT ( 'NONE',  ( -5.409176543609191867, -29.99999999999998934, 5.306317252530670991 ) ) ;
#31667 = CARTESIAN_POINT ( 'NONE',  ( 0.000000000000000000, 0.000000000000000000, -4.987924522925830217 ) ) ;
#31669 = CARTESIAN_POINT ( 'NONE',  ( -33.54350669342006341, 484.9999455485477142, -0.3061812613743876144 ) ) ;
#31668 = CARTESIAN_POINT ( 'NONE',  ( 21.36200998601213641, -60.00000000000005684, 42.72826288236584702 ) ) ;
#31670 = EDGE_CURVE ( 'NONE', #699, #79080, #18393, .T. ) ;
#31671 = CARTESIAN_POINT ( 'NONE',  ( 0.000000000000000000, 0.000000000000000000, -13.00000000000000000 ) ) ;
#31672 = ORIENTED_EDGE ( 'NONE', *, *, #44999, .T. ) ;
#31673 = CARTESIAN_POINT ( 'NONE',  ( -27.67545152213132909, 310.9892636312667378, 11.64432264744174184 ) ) ;
#31674 = VECTOR ( 'NONE', #70918, 1000.000000000000227 ) ;
#31675 = EDGE_LOOP ( 'NONE', ( #81009, #79863 ) ) ;
#31676 = CARTESIAN_POINT ( 'NONE',  ( 22.66207472693116642, 304.4407013690983490, 10.06416949456371768 ) ) ;
#31677 = CARTESIAN_POINT ( 'NONE',  ( -8.000000000000000000, 0.000000000000000000, -0.02540000000000007530 ) ) ;
#31678 = ORIENTED_EDGE ( 'NONE', *, *, #85079, .T. ) ;
#31679 = CARTESIAN_POINT ( 'NONE',  ( -114.6154627495407965, -59.99999999999028688, 172.5259999663634289 ) ) ;
#31681 = CARTESIAN_POINT ( 'NONE',  ( 5.974109059516062636, -2.735160444458186735, -6.500000000000002665 ) ) ;
#31680 = B_SPLINE_CURVE_WITH_KNOTS ( 'NONE', 3,
 ( #2207, #10827, #35155, #27079 ),
 .UNSPECIFIED., .F., .F.,
 ( 4, 4 ),
 ( 0.000000000000000000, 1.000000000000000000 ),
 .UNSPECIFIED. ) ;
#31682 = CARTESIAN_POINT ( 'NONE',  ( 47.97043484894224719, -59.99999999999998579, 66.94516856292635509 ) ) ;
#31683 = CARTESIAN_POINT ( 'NONE',  ( 6.281175601187038993, 3.752776749732559480, -6.500000000000007105 ) ) ;
#31684 = CARTESIAN_POINT ( 'NONE',  ( 0.5680201850460122603, 26.02808649538077646, -38.38338999498244419 ) ) ;
#31686 = CARTESIAN_POINT ( 'NONE',  ( 18.16438888712567490, -53.39614106568718910, 33.13417337925488226 ) ) ;
#31685 = CARTESIAN_POINT ( 'NONE',  ( -109.5584880022855998, -59.99999999999993605, 197.6571416747650574 ) ) ;
#31688 = CARTESIAN_POINT ( 'NONE',  ( 100.8551254251243563, -38.00000000000002842, 188.7646223632392264 ) ) ;
#31687 = PRODUCT_DEFINITION_CONTEXT ( 'detailed design', #95471, 'design' ) ;
#31689 = CARTESIAN_POINT ( 'NONE',  ( 1.097844465543542425, 54.05176034408437857, -8.381373465022610603 ) ) ;
#31690 = CARTESIAN_POINT ( 'NONE',  ( -45.52144803689373020, -39.53055252850298018, 44.31166116903103358 ) ) ;
#31691 = CARTESIAN_POINT ( 'NONE',  ( 85.59800593614014019, 1.016364837396684119E-14, 0.000000000000000000 ) ) ;
#31692 = VERTEX_POINT ( 'NONE', #75828 ) ;
#31693 = DIRECTION ( 'NONE',  ( 0.000000000000000000, -1.000000000000000000, 0.000000000000000000 ) ) ;
#31694 = DIRECTION ( 'NONE',  ( 0.000000000000000000, 0.000000000000000000, -1.000000000000000000 ) ) ;
#31695 = CARTESIAN_POINT ( 'NONE',  ( -1.451822140657068827, -69.63589226600636550, 12.81290273743130292 ) ) ;
#31696 = CARTESIAN_POINT ( 'NONE',  ( 0.000000000000000000, 15.00000000000000000, 0.000000000000000000 ) ) ;
#31697 = CARTESIAN_POINT ( 'NONE',  ( 34.06332199976886699, 330.0526646846329299, -3.810096259360388427 ) ) ;
#31698 = VERTEX_POINT ( 'NONE', #78484 ) ;
#31699 = ORIENTED_EDGE ( 'NONE', *, *, #53378, .T. ) ;
#31700 = CARTESIAN_POINT ( 'NONE',  ( 100.1372358933510327, -30.00000000002086509, 199.1046915188701405 ) ) ;
#31701 = DIRECTION ( 'NONE',  ( 0.000000000000000000, -1.000000000000000000, 0.000000000000000000 ) ) ;
#31702 = VECTOR ( 'NONE', #1857, 1000.000000000000000 ) ;
#31703 = CARTESIAN_POINT ( 'NONE',  ( 6.533698841377278299, 41.84235572472459097, -59.21169212581951058 ) ) ;
#31704 = FILL_AREA_STYLE ('',( #7390 ) ) ;
#31705 = CARTESIAN_POINT ( 'NONE',  ( 100.5523255717907745, -30.00000000000000355, 159.8787756642091153 ) ) ;
#31706 = CONICAL_SURFACE ( 'NONE', #26571, 4.250000000000000000, 0.9599310885968754814 ) ;
#31707 = CARTESIAN_POINT ( 'NONE',  ( 7.551437640244098581, 101.9912753747709075, -2.648272645923387625 ) ) ;
#31708 = ORIENTED_EDGE ( 'NONE', *, *, #44623, .T. ) ;
#31709 = ADVANCED_FACE ( 'NONE', ( #94701 ), #84248, .T. ) ;
#31710 = COLOUR_RGB ( '', 0.40784314, 0.44705882, 0.49803922) ;
#31711 = VERTEX_POINT ( 'NONE', #53163 ) ;
#31712 = EDGE_LOOP ( 'NONE', ( #106688, #38738, #7107, #3718 ) ) ;
#31713 = CARTESIAN_POINT ( 'NONE',  ( -33.86879232827779873, 484.1347737343850781, 1.564974661443849557 ) ) ;
#31714 = CARTESIAN_POINT ( 'NONE',  ( -6.195804093982627769, 41.59435685013754380, -70.65487364512668478 ) ) ;
#31715 = EDGE_CURVE ( 'NONE', #33833, #103460, #106643, .T. ) ;
#31716 = ORIENTED_EDGE ( 'NONE', *, *, #91719, .T. ) ;
#31718 = ADVANCED_FACE ( 'NONE', ( #20319 ), #53681, .F. ) ;
#31717 = CARTESIAN_POINT ( 'NONE',  ( 42.10086803841211633, 435.6552064019012960, 19.95582312411057302 ) ) ;
#31719 = ORIENTED_EDGE ( 'NONE', *, *, #16176, .F. ) ;
#31720 = CYLINDRICAL_SURFACE ( 'NONE', #62146, 4.250000000000000000 ) ;
#31721 = CARTESIAN_POINT ( 'NONE',  ( 80.57150957014567894, -38.81697432977912854, 193.9564742164324969 ) ) ;
#31722 = CARTESIAN_POINT ( 'NONE',  ( 15.78903373183817394, 4.458378530872352918, 5.229003202815950324 ) ) ;
#31723 = CARTESIAN_POINT ( 'NONE',  ( 101.2019940638598854, 6.123233995736568081E-16, -5.000000000000011546 ) ) ;
#31724 = CARTESIAN_POINT ( 'NONE',  ( 38.42690270509001493, 318.8932286035306447, 15.80036497839117793 ) ) ;
#31725 = LINE ( 'NONE', #91023, #78089 ) ;
#31726 = DIRECTION ( 'NONE',  ( -1.000000000000000000, -1.224606353822377258E-16, -0.000000000000000000 ) ) ;
#31727 = EDGE_CURVE ( 'NONE', #22950, #52196, #41204, .T. ) ;
#31728 = EDGE_CURVE ( 'NONE', #22025, #83401, #13634, .T. ) ;
#31729 = CARTESIAN_POINT ( 'NONE',  ( 0.000000000000000000, 48.50000000000000000, 0.000000000000000000 ) ) ;
#31730 = CARTESIAN_POINT ( 'NONE',  ( 42.77949383849493614, 391.0275278356816671, 19.62059687413802678 ) ) ;
#31731 = CARTESIAN_POINT ( 'NONE',  ( 32.78741055188847042, 485.3331003366707819, 5.977022408747033388 ) ) ;
#31732 = AXIS2_PLACEMENT_3D ( 'NONE', #55269, #105432, #88195 ) ;
#31733 = FILL_AREA_STYLE ('',( #74283 ) ) ;
#31734 = ORIENTED_EDGE ( 'NONE', *, *, #81070, .F. ) ;
#31735 = CARTESIAN_POINT ( 'NONE',  ( -42.55949806392435875, 435.1558328882642286, 18.91815692827004014 ) ) ;
#31737 = CARTESIAN_POINT ( 'NONE',  ( -27.07835102769082525, 307.1390153984987705, 10.92803387578435625 ) ) ;
#31736 =( NAMED_UNIT ( * ) PLANE_ANGLE_UNIT ( ) SI_UNIT ( $, .RADIAN. ) );
#31738 = CARTESIAN_POINT ( 'NONE',  ( 8.238701406685740025, 53.79503307339000173, -3.999633084520308302 ) ) ;
#31739 = DIRECTION ( 'NONE',  ( 0.000000000000000000, -1.000000000000000000, 0.000000000000000000 ) ) ;
#31740 = CARTESIAN_POINT ( 'NONE',  ( -8.000000000000000000, -13.24999999999999467, -9.797174393178825657E-16 ) ) ;
#31741 = CARTESIAN_POINT ( 'NONE',  ( -5.416666666666666075, 4.378239541354655984, -5.848636054922035754 ) ) ;
#31742 =( GEOMETRIC_REPRESENTATION_CONTEXT ( 3 ) GLOBAL_UNCERTAINTY_ASSIGNED_CONTEXT ( ( #92957 ) ) GLOBAL_UNIT_ASSIGNED_CONTEXT ( ( #44299, #45891, #61562 ) ) REPRESENTATION_CONTEXT ( 'NONE', 'WORKASPACE' ) );
#31743 = SURFACE_SIDE_STYLE ('',( #105602 ) ) ;
#31744 = CIRCLE ( 'NONE', #102324, 15.00000000000000000 ) ;
#31745 = ORIENTED_EDGE ( 'NONE', *, *, #19418, .T. ) ;
#31746 = CARTESIAN_POINT ( 'NONE',  ( 85.57898256585818331, -35.67946169813210133, 183.8354908636134724 ) ) ;
#31747 = PLANE ( 'NONE',  #80807 ) ;
#31748 = FILL_AREA_STYLE ('',( #91571 ) ) ;
#31749 = VERTEX_POINT ( 'NONE', #79023 ) ;
#31750 = CIRCLE ( 'NONE', #38610, 4.000000000000000000 ) ;
#31751 = CARTESIAN_POINT ( 'NONE',  ( 93.83684923425705904, -57.67470318766702064, 11.22057503938936129 ) ) ;
#31752 = LINE ( 'NONE', #97502, #86902 ) ;
#31753 = DIRECTION ( 'NONE',  ( -1.000000000000000000, -0.000000000000000000, -0.000000000000000000 ) ) ;
#31754 = B_SPLINE_CURVE_WITH_KNOTS ( 'NONE', 3,
 ( #93933, #28170, #35730, #102010, #68607, #61046 ),
 .UNSPECIFIED., .F., .F.,
 ( 4, 2, 4 ),
 ( 0.000000000000000000, 0.5000000000000000000, 1.000000000000000000 ),
 .UNSPECIFIED. ) ;
#31755 = CARTESIAN_POINT ( 'NONE',  ( -86.49015731118424810, -37.99999999999980105, 187.7658702032705378 ) ) ;
#31756 = CARTESIAN_POINT ( 'NONE',  ( -7.999999999999996447, -3.000000000000000000, 2.094395098902548824 ) ) ;
#31757 = DIRECTION ( 'NONE',  ( -1.000000000000000000, 0.000000000000000000, 0.000000000000000000 ) ) ;
#31758 = CARTESIAN_POINT ( 'NONE',  ( -11.67652068491833006, 8.895001519498853426, 9.142920084771974487 ) ) ;
#31759 = EDGE_CURVE ( 'NONE', #82593, #20391, #99648, .T. ) ;
#31760 = EDGE_LOOP ( 'NONE', ( #40946, #70928, #22844, #28119, #61898, #101341 ) ) ;
#31761 =( NAMED_UNIT ( * ) PLANE_ANGLE_UNIT ( ) SI_UNIT ( $, .RADIAN. ) );
#31762 = CARTESIAN_POINT ( 'NONE',  ( -10.50000000000000000, -5.000000000000000000, -11.21398294031087062 ) ) ;
#31763 = DIRECTION ( 'NONE',  ( 0.000000000000000000, 0.000000000000000000, 1.000000000000000000 ) ) ;
#31764 = CARTESIAN_POINT ( 'NONE',  ( 9.240220675753668900, 15.98931925350938243, -3.827754797006023058 ) ) ;
#31765 = CARTESIAN_POINT ( 'NONE',  ( 0.000000000000000000, 0.000000000000000000, 0.000000000000000000 ) ) ;
#31766 = CARTESIAN_POINT ( 'NONE',  ( 69.44037080505408710, -29.97022514493267309, -21.01289856691821001 ) ) ;
#31767 = ADVANCED_FACE ( 'NONE', ( #77963 ), #27473, .T. ) ;
#31768 = CONICAL_SURFACE ( 'NONE', #73072, 8.000000000000000000, 0.9599310885968911355 ) ;
#31769 = ORIENTED_EDGE ( 'NONE', *, *, #63025, .F. ) ;
#31770 =( NAMED_UNIT ( * ) SI_UNIT ( $, .STERADIAN. ) SOLID_ANGLE_UNIT ( ) );
#31771 = CARTESIAN_POINT ( 'NONE',  ( -10.82100110659969516, -16.37520694100678043, -34.74528928969461106 ) ) ;
#31772 = CONICAL_SURFACE ( 'NONE', #11108, 4.172000000000001485, 0.9599310885968750373 ) ;
#31774 = CARTESIAN_POINT ( 'NONE',  ( -31.96895277089044995, -47.40887110283673422, -32.79492523475107646 ) ) ;
#31773 = CARTESIAN_POINT ( 'NONE',  ( 0.000000000000000000, 67.05096163904791240, -10.02537308446411402 ) ) ;
#31775 = AXIS2_PLACEMENT_3D ( 'NONE', #28876, #5082, #86558 ) ;
#31776 = EDGE_LOOP ( 'NONE', ( #43775, #99550, #102629, #53067 ) ) ;
#31777 = ORIENTED_EDGE ( 'NONE', *, *, #67340, .F. ) ;
#31778 = FILL_AREA_STYLE_COLOUR ( '', #5479 ) ;
#31779 = CARTESIAN_POINT ( 'NONE',  ( -3.250000000000016431, 5.629165124598842773, 1.734723475976807094E-15 ) ) ;
#31780 = CARTESIAN_POINT ( 'NONE',  ( -92.59975610422581838, -60.00000000000001421, -2.780597702228391643 ) ) ;
#31781 = VERTEX_POINT ( 'NONE', #86615 ) ;
#31782 = CARTESIAN_POINT ( 'NONE',  ( 33.90317062511168444, -31.39243716251483107, -29.86178143371859051 ) ) ;
#31783 = CARTESIAN_POINT ( 'NONE',  ( -75.51516288543759003, -29.99999999999999289, -27.33247042156351725 ) ) ;
#31784 = CARTESIAN_POINT ( 'NONE',  ( 101.1766009655264895, -60.24913381348638097, 194.9937302242699673 ) ) ;
#31786 = CARTESIAN_POINT ( 'NONE',  ( -46.83547786243088495, 13.71028427728498045, 15.22387951581991672 ) ) ;
#31785 = FACE_OUTER_BOUND ( 'NONE', #67558, .T. ) ;
#31787 = EDGE_CURVE ( 'NONE', #68198, #80946, #46648, .T. ) ;
#31788 = CARTESIAN_POINT ( 'NONE',  ( -81.20415014607263515, -49.93051291868427199, 169.6414208886321262 ) ) ;
#31789 = VERTEX_POINT ( 'NONE', #4612 ) ;
#31790 = ORIENTED_EDGE ( 'NONE', *, *, #49238, .F. ) ;
#31791 = VERTEX_POINT ( 'NONE', #95743 ) ;
#31792 = LINE ( 'NONE', #64677, #65557 ) ;
#31793 = CARTESIAN_POINT ( 'NONE',  ( -4.999999999999960032, -14.45898243498580271, 13.52154848218615335 ) ) ;
#31794 = EDGE_LOOP ( 'NONE', ( #84913, #1216, #39794, #64674, #94932, #33216, #89032, #43478, #93542 ) ) ;
#31795 =( NAMED_UNIT ( * ) PLANE_ANGLE_UNIT ( ) SI_UNIT ( $, .RADIAN. ) );
#31796 = CARTESIAN_POINT ( 'NONE',  ( -6.949531687764044400E-15, 14.17434517210798184, 56.74723269274520021 ) ) ;
#31797 = CARTESIAN_POINT ( 'NONE',  ( -9.700350089084274430, 15.75268258782372754, -2.455962139888423490 ) ) ;
#31798 = CARTESIAN_POINT ( 'NONE',  ( -114.2271649293462445, -57.67113267762195505, 172.5270642037310722 ) ) ;
#31799 = CARTESIAN_POINT ( 'NONE',  ( -5.384233811324312668, -68.00217091344775611, 2.655407383564612811 ) ) ;
#31800 = DIRECTION ( 'NONE',  ( -0.000000000000000000, 0.000000000000000000, -1.000000000000000000 ) ) ;
#31801 = CARTESIAN_POINT ( 'NONE',  ( 7.500000000000000888, 1.224646799147353256E-15, 5.000000000000000000 ) ) ;
#31802 = DIRECTION ( 'NONE',  ( -1.000000000000000000, -1.224606353822377258E-16, -0.000000000000000000 ) ) ;
#31803 = CARTESIAN_POINT ( 'NONE',  ( 2.726837646490497757, -14.21045842199434794, -37.36840973699905533 ) ) ;
#31804 = LINE ( 'NONE', #41469, #25844 ) ;
#31805 = CARTESIAN_POINT ( 'NONE',  ( -54.29644833178524976, -29.09616009912803491, 54.75307643248039824 ) ) ;
#31806 = DIRECTION ( 'NONE',  ( 0.000000000000000000, 1.000000000000000000, 0.000000000000000000 ) ) ;
#31807 = PRODUCT_RELATED_PRODUCT_CATEGORY ( 'part', '', ( #104487 ) ) ;
#31808 = EDGE_LOOP ( 'NONE', ( #34228, #74633, #75974, #6348 ) ) ;
#31809 = AXIS2_PLACEMENT_3D ( 'NONE', #1251, #43348, #2871 ) ;
#31810 = CARTESIAN_POINT ( 'NONE',  ( -98.54215169052864098, -45.24992954469452400, 193.5376205676895722 ) ) ;
#31811 = STYLED_ITEM ( 'NONE', ( #49801 ), #55970 ) ;
#31812 = AXIS2_PLACEMENT_3D ( 'NONE', #6183, #5665, #71452 ) ;
#31813 = CARTESIAN_POINT ( 'NONE',  ( -5.433201317752814674, 294.7714280552114587, -8.410911388488676366 ) ) ;
#31814 = EDGE_LOOP ( 'NONE', ( #82807, #3464 ) ) ;
#31815 = CARTESIAN_POINT ( 'NONE',  ( -16.75187969033554936, 34.99134772383131065, -21.80698433968595751 ) ) ;
#31816 = VECTOR ( 'NONE', #105820, 1000.000000000000000 ) ;
#31817 = CARTESIAN_POINT ( 'NONE',  ( 89.38838440990150502, -38.38695707012075786, -17.36236548429767623 ) ) ;
#31818 = CARTESIAN_POINT ( 'NONE',  ( -9.000000000000001776, -4.000000000000003553, 42.58845726811989607 ) ) ;
#31819 = DIRECTION ( 'NONE',  ( 0.000000000000000000, -0.5000000000000013323, -0.8660254037844379305 ) ) ;
#31820 = CARTESIAN_POINT ( 'NONE',  ( -15.65218212520301755, 294.5588111923345878, 9.874722130675968046 ) ) ;
#31821 = AXIS2_PLACEMENT_3D ( 'NONE', #20381, #102836, #12214 ) ;
#31822 = DIRECTION ( 'NONE',  ( 0.000000000000000000, 0.000000000000000000, 1.000000000000000000 ) ) ;
#31823 = CARTESIAN_POINT ( 'NONE',  ( 84.03426563400070393, -30.00000000000000000, 161.3119413430846407 ) ) ;
#31824 = CARTESIAN_POINT ( 'NONE',  ( 18.68302636746854262, 303.6623007926234550, -10.04032342916666920 ) ) ;
#31825 = CARTESIAN_POINT ( 'NONE',  ( 36.90171438447441687, 490.9796882048100315, 12.46551445837898875 ) ) ;
#31826 = CARTESIAN_POINT ( 'NONE',  ( -28.43950163419759747, 12.73412882672193724, 40.70661530191370758 ) ) ;
#31827 = CARTESIAN_POINT ( 'NONE',  ( -6.837824896291514243, 3.947820044545419016, -6.564402953523714501 ) ) ;
#31828 = ADVANCED_BREP_SHAPE_REPRESENTATION ( '', ( #19858, #87588, #10728 ), #60740 ) ;
#31829 = B_SPLINE_CURVE_WITH_KNOTS ( 'NONE', 3,
 ( #92793, #69072, #101947, #17861 ),
 .UNSPECIFIED., .F., .F.,
 ( 4, 4 ),
 ( 8.835602482133882738E-17, 0.0007664883490338720738 ),
 .UNSPECIFIED. ) ;
#31830 = EDGE_LOOP ( 'NONE', ( #43264, #92378, #89406, #41202 ) ) ;
#31831 = ORIENTED_EDGE ( 'NONE', *, *, #50779, .T. ) ;
#31832 = CARTESIAN_POINT ( 'NONE',  ( 49.20253590315749648, -46.43899358245619169, 51.70391652283478834 ) ) ;
#31833 = CARTESIAN_POINT ( 'NONE',  ( 6.526057752884477203, 41.69808114003689070, -58.86835341771923424 ) ) ;
#31834 = DIRECTION ( 'NONE',  ( -1.000000000000000000, 0.000000000000000000, 0.000000000000000000 ) ) ;
#31835 = ADVANCED_FACE ( 'NONE', ( #38075 ), #12679, .T. ) ;
#31836 = ORIENTED_EDGE ( 'NONE', *, *, #18437, .T. ) ;
#31837 = CARTESIAN_POINT ( 'NONE',  ( -106.5422770149979357, -38.37230016228074447, 195.6026319719495064 ) ) ;
#31838 = EDGE_LOOP ( 'NONE', ( #18543, #91604, #93668, #49872 ) ) ;
#31839 = DIRECTION ( 'NONE',  ( 0.000000000000000000, 0.000000000000000000, 1.000000000000000000 ) ) ;
#31840 = CARTESIAN_POINT ( 'NONE',  ( 110.3060959018607576, -38.35604839215716311, 158.1135554324671944 ) ) ;
#31841 = CARTESIAN_POINT ( 'NONE',  ( 10.06039080892654169, 12.97763442506446907, -10.57343087305293317 ) ) ;
#31842 = CARTESIAN_POINT ( 'NONE',  ( -19.47057824336637211, 49.99002094786000328, 60.40962004294379284 ) ) ;
#31843 = CARTESIAN_POINT ( 'NONE',  ( -42.76758846428410976, 409.7905884173310369, 19.95987282388911765 ) ) ;
#31844 = CARTESIAN_POINT ( 'NONE',  ( 101.5801647266594046, -60.15125686205630018, 125.0291127044086892 ) ) ;
#31845 = B_SPLINE_CURVE_WITH_KNOTS ( 'NONE', 3,
 ( #57582, #90505, #84009, #99656 ),
 .UNSPECIFIED., .F., .F.,
 ( 4, 4 ),
 ( 0.000000000000000000, 0.0004300933845558184399 ),
 .UNSPECIFIED. ) ;
#31846 = CARTESIAN_POINT ( 'NONE',  ( 22.81472563493030492, 27.48372958372127783, 33.14224123365016794 ) ) ;
#31847 = CARTESIAN_POINT ( 'NONE',  ( -27.39853812899586671, 307.9048118753939320, -9.316184934693556130 ) ) ;
#31848 = DIRECTION ( 'NONE',  ( 0.000000000000000000, 0.000000000000000000, -1.000000000000000000 ) ) ;
#31849 = CARTESIAN_POINT ( 'NONE',  ( 78.07448996005189201, -60.00000000000000000, 192.9802269763975744 ) ) ;
#31850 = EDGE_CURVE ( 'NONE', #67654, #53206, #29173, .T. ) ;
#31851 = VECTOR ( 'NONE', #82260, 1000.000000000000000 ) ;
#31852 = ORIENTED_EDGE ( 'NONE', *, *, #82812, .F. ) ;
#31853 = CARTESIAN_POINT ( 'NONE',  ( 57.85089049392932026, -60.32948186521389289, 76.30787142766249076 ) ) ;
#31854 = ADVANCED_FACE ( 'NONE', ( #29454 ), #104347, .T. ) ;
#31855 = CARTESIAN_POINT ( 'NONE',  ( -30.25140696341276580, 297.9349684876631272, -1.321983318591468670 ) ) ;
#31856 = CARTESIAN_POINT ( 'NONE',  ( 9.378256585906134646, -52.21653903096282789, 23.52725134406122720 ) ) ;
#31857 = EDGE_CURVE ( 'NONE', #13534, #24651, #48362, .T. ) ;
#31858 = CARTESIAN_POINT ( 'NONE',  ( 51.01037695545453232, 450.0000000000002274, 18.20242257375371153 ) ) ;
#31859 = ORIENTED_EDGE ( 'NONE', *, *, #31632, .F. ) ;
#31861 = CARTESIAN_POINT ( 'NONE',  ( -14.82216446135968901, 22.90771190644582234, 1.995522466596231226 ) ) ;
#31860 = CARTESIAN_POINT ( 'NONE',  ( -81.38022930017784518, -38.35629332861885388, -25.64663872047383819 ) ) ;
#31862 = CARTESIAN_POINT ( 'NONE',  ( 0.000000000000000000, 0.000000000000000000, -0.02540000000000007530 ) ) ;
#31863 = DIRECTION ( 'NONE',  ( 0.000000000000000000, 1.000000000000000000, 0.000000000000000000 ) ) ;
#31864 = DIRECTION ( 'NONE',  ( 1.000000000000000000, 0.000000000000000000, 0.000000000000000000 ) ) ;
#31865 = CARTESIAN_POINT ( 'NONE',  ( 8.000000000000000000, -31.99999999999999289, 0.000000000000000000 ) ) ;
#31866 = SURFACE_SIDE_STYLE ('',( #74413 ) ) ;
#31867 = EDGE_CURVE ( 'NONE', #53571, #35344, #21353, .T. ) ;
#31868 = CARTESIAN_POINT ( 'NONE',  ( 62.06337123375777765, 48.00000000000000711, -19.99347512944438421 ) ) ;
#31869 = EDGE_LOOP ( 'NONE', ( #2186, #24582, #82370, #18950 ) ) ;
#31870 = CARTESIAN_POINT ( 'NONE',  ( 82.76193996168436229, -46.48728455946643834, 178.0629670417869761 ) ) ;
#31871 = CARTESIAN_POINT ( 'NONE',  ( 30.00000000000000355, 490.2060126478330631, 6.957942417092681353 ) ) ;
#31872 = FACE_OUTER_BOUND ( 'NONE', #50886, .T. ) ;
#31873 = ORIENTED_EDGE ( 'NONE', *, *, #6941, .F. ) ;
#31874 = DIRECTION ( 'NONE',  ( -1.000000000000000000, -1.224606353822377258E-16, -0.000000000000000000 ) ) ;
#31875 = CARTESIAN_POINT ( 'NONE',  ( 7.466456039914962872, -3.088347863567613150, -19.53079660665969541 ) ) ;
#31876 = CARTESIAN_POINT ( 'NONE',  ( 25.91508385773364154, 35.08289675578968314, -8.415194575045109815 ) ) ;
#31877 = FILL_AREA_STYLE_COLOUR ( '', #43440 ) ;
#31878 = DIRECTION ( 'NONE',  ( 0.000000000000000000, 0.000000000000000000, -1.000000000000000000 ) ) ;
#31879 = CARTESIAN_POINT ( 'NONE',  ( 43.30868969682389036, 0.000000000000000000, 5.000000000000002665 ) ) ;
#31880 = ORIENTED_EDGE ( 'NONE', *, *, #105270, .F. ) ;
#31881 = CONICAL_SURFACE ( 'NONE', #92132, 3.400000000000000355, 0.9599310885968748153 ) ;
#31882 = CARTESIAN_POINT ( 'NONE',  ( 6.944031699373470090, 105.5346065455613171, 3.972913591453824278 ) ) ;
#31883 = FACE_OUTER_BOUND ( 'NONE', #87286, .T. ) ;
#31885 = CARTESIAN_POINT ( 'NONE',  ( -10.18585140722862192, 16.00067669882299271, -10.17614714549901578 ) ) ;
#31884 = CARTESIAN_POINT ( 'NONE',  ( -12.53202292880966873, -21.38207867075475477, 35.62331039717147974 ) ) ;
#31886 = EDGE_CURVE ( 'NONE', #55601, #58295, #8483, .T. ) ;
#31887 = CIRCLE ( 'NONE', #2531, 3.309500000000001663 ) ;
#31888 = CARTESIAN_POINT ( 'NONE',  ( 2.977408999572650927, -15.87500000204838635, -7.188101187500001821 ) ) ;
#31889 = CARTESIAN_POINT ( 'NONE',  ( -28.71549002648981030, 15.67055689680110753, -41.65541077617267973 ) ) ;
#31890 =( GEOMETRIC_REPRESENTATION_CONTEXT ( 3 ) GLOBAL_UNCERTAINTY_ASSIGNED_CONTEXT ( ( #37371 ) ) GLOBAL_UNIT_ASSIGNED_CONTEXT ( ( #63636, #3798, #36735 ) ) REPRESENTATION_CONTEXT ( 'NONE', 'WORKASPACE' ) );
#31891 =( LENGTH_UNIT ( ) NAMED_UNIT ( * ) SI_UNIT ( .MILLI., .METRE. ) );
#31892 = AXIS2_PLACEMENT_3D ( 'NONE', #54161, #79518, #47671 ) ;
#31893 = AXIS2_PLACEMENT_3D ( 'NONE', #66291, #66832, #67890 ) ;
#31894 = ORIENTED_EDGE ( 'NONE', *, *, #77233, .T. ) ;
#31895 = DIRECTION ( 'NONE',  ( -0.5735764363510512664, 0.8191520442889881348, 1.003171929053520309E-16 ) ) ;
#31896 = CARTESIAN_POINT ( 'NONE',  ( 19.50000000000000000, 12.99999999999999289, 7.500000000000000000 ) ) ;
#31897 = CONICAL_SURFACE ( 'NONE', #83532, 5.000000000000010658, 0.9599310885968697082 ) ;
#31898 = CARTESIAN_POINT ( 'NONE',  ( -4.468886067276133467, 142.4736706807960616, -5.000000000000000888 ) ) ;
#31899 = EDGE_CURVE ( 'NONE', #66070, #106756, #5661, .T. ) ;
#31900 = DIRECTION ( 'NONE',  ( 0.000000000000000000, 0.000000000000000000, 1.000000000000000000 ) ) ;
#31901 = CARTESIAN_POINT ( 'NONE',  ( -15.29749241880924338, 3.521433830184460767, 3.946287723054361152 ) ) ;
#31902 = ORIENTED_EDGE ( 'NONE', *, *, #64902, .T. ) ;
#31903 = CARTESIAN_POINT ( 'NONE',  ( 19.34999999999999787, -3.309499999999999886, 4.475777889183790779E-16 ) ) ;
#31904 = FACE_OUTER_BOUND ( 'NONE', #50778, .T. ) ;
#31905 = ORIENTED_EDGE ( 'NONE', *, *, #103451, .T. ) ;
#31906 = DIRECTION ( 'NONE',  ( 0.000000000000000000, 0.000000000000000000, -1.000000000000000000 ) ) ;
#31907 = DIRECTION ( 'NONE',  ( 0.000000000000000000, 0.000000000000000000, -1.000000000000000000 ) ) ;
#31908 = CARTESIAN_POINT ( 'NONE',  ( -20.52361948052543639, 41.82532680694352223, -79.00191459447381703 ) ) ;
#31909 = CARTESIAN_POINT ( 'NONE',  ( -109.3749600128534354, -60.00000000000001421, 138.6821750997686422 ) ) ;
#31910 = CYLINDRICAL_SURFACE ( 'NONE', #56569, 4.000000000000000000 ) ;
#31911 = CARTESIAN_POINT ( 'NONE',  ( 1.714138721600513892E-15, 0.9999999999999943379, 13.99700487351915612 ) ) ;
#31912 = CARTESIAN_POINT ( 'NONE',  ( 30.00000000000000000, 4.000000000000000000, 18.57417562100670949 ) ) ;
#31913 = CARTESIAN_POINT ( 'NONE',  ( -14.64132442749376573, 0.3341158548789989191, 15.00000000000002132 ) ) ;
#31915 = CARTESIAN_POINT ( 'NONE',  ( 6.683837171061802529, 3.955946848495962787, 6.851900933636986935 ) ) ;
#31914 = CARTESIAN_POINT ( 'NONE',  ( -9.596002107494335576, -5.000000000000002665, -92.37456064099097830 ) ) ;
#31916 = EDGE_CURVE ( 'NONE', #93035, #29729, #37719, .T. ) ;
#31917 = CARTESIAN_POINT ( 'NONE',  ( -83.30516160954981331, -42.98134678973099199, 177.5882959578982252 ) ) ;
#31918 = VERTEX_POINT ( 'NONE', #65495 ) ;
#31919 = SURFACE_STYLE_USAGE ( .BOTH. , #90669 ) ;
#31920 = ORIENTED_EDGE ( 'NONE', *, *, #79256, .T. ) ;
#31921 =( BOUNDED_CURVE ( )  B_SPLINE_CURVE ( 2, ( #106196, #97575, #46914 ),
 .UNSPECIFIED., .F., .F. ) 
 B_SPLINE_CURVE_WITH_KNOTS ( ( 3, 3 ),
 ( 0.000000000000000000, 1.000000000000000000 ),
 .UNSPECIFIED. ) 
 CURVE ( )  GEOMETRIC_REPRESENTATION_ITEM ( )  RATIONAL_B_SPLINE_CURVE ( ( 1.000000000000000000, 1.857142857142858317, 1.000000000000000000 ) ) 
 REPRESENTATION_ITEM ( '' )  );
#31922 = ORIENTED_EDGE ( 'NONE', *, *, #68612, .F. ) ;
#31923 = FACE_BOUND ( 'NONE', #28440, .T. ) ;
#31924 = ADVANCED_FACE ( 'NONE', ( #98383 ), #15343, .F. ) ;
#31925 = CARTESIAN_POINT ( 'NONE',  ( 32.95589646111153570, 464.8957215206403930, 10.75300444715520953 ) ) ;
#31926 = FACE_OUTER_BOUND ( 'NONE', #63709, .T. ) ;
#31927 = CARTESIAN_POINT ( 'NONE',  ( -15.68120647348229468, 6.021684053265807357, -7.051923121162609220 ) ) ;
#31928 = CARTESIAN_POINT ( 'NONE',  ( 2.955800887866951943, 53.34171681442641955, -5.000000000000000000 ) ) ;
#31929 = CARTESIAN_POINT ( 'NONE',  ( -8.733111415123392618, -5.000000000000000000, -94.70106727903508670 ) ) ;
#31930 = LINE ( 'NONE', #48074, #76109 ) ;
#31931 = CARTESIAN_POINT ( 'NONE',  ( 113.0845476695725864, -59.99999999999993605, 149.3435440849930842 ) ) ;
#31932 = CARTESIAN_POINT ( 'NONE',  ( -109.2896413415886485, -29.99999999999996092, 180.5615511752786233 ) ) ;
#31933 = CARTESIAN_POINT ( 'NONE',  ( -61.87588688699417361, -29.06269388545054966, 72.16211123457625831 ) ) ;
#31934 = ORIENTED_EDGE ( 'NONE', *, *, #32278, .T. ) ;
#31935 = CARTESIAN_POINT ( 'NONE',  ( 58.05736968067268577, 38.95267796501454427, 26.29552882805327840 ) ) ;
#31936 = CARTESIAN_POINT ( 'NONE',  ( 107.2599453223138681, -60.00000000001746514, 200.4174002960321843 ) ) ;
#31937 = ORIENTED_EDGE ( 'NONE', *, *, #104526, .F. ) ;
#31938 = CARTESIAN_POINT ( 'NONE',  ( -8.046840872620296425E-06, -18.58625481980403649, 26.98735909623638207 ) ) ;
#31939 = CARTESIAN_POINT ( 'NONE',  ( -7.188101187500000044, -12.78125000204838635, -8.802885111219163269E-16 ) ) ;
#31940 = CARTESIAN_POINT ( 'NONE',  ( -9.500000025475724641, -4.999999999999997335, -69.85526497430338111 ) ) ;
#31941 = ORIENTED_EDGE ( 'NONE', *, *, #88968, .F. ) ;
#31942 = CARTESIAN_POINT ( 'NONE',  ( 36.29583367650112535, 464.0085854085123174, 19.58118771088512489 ) ) ;
#31943 = EDGE_LOOP ( 'NONE', ( #34493, #19963, #58391, #45988, #57215, #46872 ) ) ;
#31944 = CARTESIAN_POINT ( 'NONE',  ( 10.36871714652611054, 45.36883139708660906, -15.40779740156172295 ) ) ;
#31945 = VECTOR ( 'NONE', #68090, 1000.000000000000000 ) ;
#31946 = EDGE_CURVE ( 'NONE', #3450, #73270, #100698, .T. ) ;
#31947 = CARTESIAN_POINT ( 'NONE',  ( 4.401442555609581635E-16, -29.65625000204838813, -7.188101187500000044 ) ) ;
#31948 = CARTESIAN_POINT ( 'NONE',  ( -82.56557049406225701, -59.99999999999998579, 198.5083017901899893 ) ) ;
#31949 = CARTESIAN_POINT ( 'NONE',  ( 9.995361331467700339, -57.97514824717608661, 26.59863933490087362 ) ) ;
#31950 = CARTESIAN_POINT ( 'NONE',  ( -1.320432766682874540E-15, -28.90625000204838813, 7.188101187500000044 ) ) ;
#31951 = CARTESIAN_POINT ( 'NONE',  ( 33.54350669342029079, 484.9999455485476574, -0.3061812613748190470 ) ) ;
#31952 = CARTESIAN_POINT ( 'NONE',  ( -7.721181058141405096, -30.00000000000004263, -2.093648267354947912 ) ) ;
#31953 = CARTESIAN_POINT ( 'NONE',  ( 5.000000000000000888, -26.67919295183293116, -6.179716592092315608 ) ) ;
#31954 =( NAMED_UNIT ( * ) PLANE_ANGLE_UNIT ( ) SI_UNIT ( $, .RADIAN. ) );
#31955 = DIRECTION ( 'NONE',  ( 0.000000000000000000, 0.000000000000000000, 1.000000000000000000 ) ) ;
#31956 = DIRECTION ( 'NONE',  ( 0.000000000000000000, 1.000000000000000000, -0.000000000000000000 ) ) ;
#31957 = AXIS2_PLACEMENT_3D ( 'NONE', #71349, #6087, #54615 ) ;
#31958 = CARTESIAN_POINT ( 'NONE',  ( 104.1990965023338447, -60.00000000000000711, 190.2933881766849993 ) ) ;
#31959 = B_SPLINE_CURVE_WITH_KNOTS ( 'NONE', 3,
 ( #56757, #97749, #105331, #81549, #98810, #89684, #40063, #41655, #8218, #50272, #98294, #17397, #33581, #7671, #23916, #16860, #31474, #40590, #15782, #89150, #93, #48664, #73471, #90743, #57820, #97225 ),
 .UNSPECIFIED., .F., .F.,
 ( 4, 2, 2, 2, 2, 2, 2, 2, 2, 2, 2, 2, 4 ),
 ( 0.003090214743966922337, 0.003342416748342341183, 0.003594618752717760463, 0.003846820757093179308, 0.004099022761468598154, 0.004603426770219428907, 0.004855628774594835176, 0.005107830778970241445, 0.006116638796471930706, 0.006368840800847349118, 0.006621042805222767530, 0.006873244809598185075, 0.007125446813973602619 ),
 .UNSPECIFIED. ) ;
#31960 = CARTESIAN_POINT ( 'NONE',  ( -32.37223141510428093, -36.02462889410557523, 33.42066239552286078 ) ) ;
#31961 = LINE ( 'NONE', #49711, #31816 ) ;
#31962 = CARTESIAN_POINT ( 'NONE',  ( 38.79797393659272586, -53.34597881264516417, 40.67431443658261259 ) ) ;
#31963 = MECHANICAL_DESIGN_GEOMETRIC_PRESENTATION_REPRESENTATION (  '', ( #97371 ), #14673 ) ;
#31964 = VERTEX_POINT ( 'NONE', #105422 ) ;
#31965 = CYLINDRICAL_SURFACE ( 'NONE', #35787, 4.000000000000000888 ) ;
#31966 = CARTESIAN_POINT ( 'NONE',  ( -57.85136142586996755, -38.34423032919368524, 89.80014059173201701 ) ) ;
#31967 = PRESENTATION_LAYER_ASSIGNMENT (  '', '', ( #104232 ) ) ;
#31968 = ORIENTED_EDGE ( 'NONE', *, *, #94161, .F. ) ;
#31970 = CARTESIAN_POINT ( 'NONE',  ( 32.16694665535142406, 298.7751107022914425, -9.134474995491629556 ) ) ;
#31969 = PLANE ( 'NONE',  #26274 ) ;
#31971 = CARTESIAN_POINT ( 'NONE',  ( 19.83349330513380693, 4.000000000000002665, 0.000000000000000000 ) ) ;
#31972 = CARTESIAN_POINT ( 'NONE',  ( 6.326195795702099112, 1.326139502404654280, 6.831522767506993610 ) ) ;
#31973 = CONICAL_SURFACE ( 'NONE', #33742, 3.309500000000007880, 0.9599310885968770357 ) ;
#31974 = DIRECTION ( 'NONE',  ( -1.000000000000000000, -0.000000000000000000, -0.000000000000000000 ) ) ;
#31975 = CARTESIAN_POINT ( 'NONE',  ( -39.36202273480736835, 437.3280700035132895, 5.163426856676655241 ) ) ;
#31976 = CIRCLE ( 'NONE', #50871, 56.32976553137783782 ) ;
#31977 = CARTESIAN_POINT ( 'NONE',  ( -30.63800635041225817, 340.2357850014829523, 17.36489564963465781 ) ) ;
#31978 = FACE_OUTER_BOUND ( 'NONE', #38989, .T. ) ;
#31979 = CARTESIAN_POINT ( 'NONE',  ( 99.85406479428269222, -60.00000000000002132, 80.14550826570986430 ) ) ;
#31980 = VECTOR ( 'NONE', #36003, 1000.000000000000000 ) ;
#31981 = CARTESIAN_POINT ( 'NONE',  ( 0.4964154566687623005, -4.996589667937438861, -7.345652830558661250 ) ) ;
#31982 = CARTESIAN_POINT ( 'NONE',  ( 0.000000000000000000, 56.87938524157181774, 0.000000000000000000 ) ) ;
#31983 = CARTESIAN_POINT ( 'NONE',  ( 8.929771841637641927, 1.482358050883964840E-15, 0.000000000000000000 ) ) ;
#31984 = ORIENTED_EDGE ( 'NONE', *, *, #42330, .T. ) ;
#31985 = EDGE_CURVE ( 'NONE', #37787, #26262, #104891, .T. ) ;
#31986 = CARTESIAN_POINT ( 'NONE',  ( -79.59017023080539843, -30.00000000000330402, -25.12590073989853323 ) ) ;
#31987 = ORIENTED_EDGE ( 'NONE', *, *, #38730, .T. ) ;
#31988 = CARTESIAN_POINT ( 'NONE',  ( -9.286995370816610418, -55.77767719873747154, 30.70990524772856034 ) ) ;
#31989 =( NAMED_UNIT ( * ) SI_UNIT ( $, .STERADIAN. ) SOLID_ANGLE_UNIT ( ) );
#31990 = FACE_OUTER_BOUND ( 'NONE', #10085, .T. ) ;
#31991 = CARTESIAN_POINT ( 'NONE',  ( 9.333892298909262308, 28.21724268374966016, -3.590295303293458584 ) ) ;
#31992 = CARTESIAN_POINT ( 'NONE',  ( -2.977408999572650039, -25.06250000204838457, -7.188101187500001821 ) ) ;
#31994 = EDGE_CURVE ( 'NONE', #14702, #112, #58374, .T. ) ;
#31993 = DIRECTION ( 'NONE',  ( 0.000000000000000000, -1.000000000000000000, 0.000000000000000000 ) ) ;
#31995 = DIRECTION ( 'NONE',  ( 0.000000000000000000, 1.000000000000000000, -0.000000000000000000 ) ) ;
#31996 = CARTESIAN_POINT ( 'NONE',  ( 7.278899350266751611, 40.56071393749584075, -70.70219355279998297 ) ) ;
#31997 = ORIENTED_EDGE ( 'NONE', *, *, #46986, .T. ) ;
#31999 = EDGE_LOOP ( 'NONE', ( #26621, #53323, #104033, #51983 ) ) ;
#31998 = LINE ( 'NONE', #89690, #68432 ) ;
#32000 = CARTESIAN_POINT ( 'NONE',  ( 82.11076762983330468, -36.02623207226398705, 156.5626120355436512 ) ) ;
#32001 =( NAMED_UNIT ( * ) SI_UNIT ( $, .STERADIAN. ) SOLID_ANGLE_UNIT ( ) );
#32002 = CARTESIAN_POINT ( 'NONE',  ( 14.36577178754511763, 3.159923610463285293, -4.257245723725899822 ) ) ;
#32003 = ORIENTED_EDGE ( 'NONE', *, *, #34555, .F. ) ;
#32004 = CARTESIAN_POINT ( 'NONE',  ( -53.14306704977071405, 49.99999999999998579, 33.99800176510388638 ) ) ;
#32005 = CARTESIAN_POINT ( 'NONE',  ( -14.89763918506242213, 1.348991191048001692, -1.758109506422078638 ) ) ;
#32006 = CARTESIAN_POINT ( 'NONE',  ( 5.082755093536325930, -15.96875000204838635, -5.082755093536325042 ) ) ;
#32007 = CARTESIAN_POINT ( 'NONE',  ( 7.550180524134847637, 26.99440752786814102, 2.651855549982494953 ) ) ;
#32008 = CIRCLE ( 'NONE', #13020, 1.000000000000000888 ) ;
#32009 = CARTESIAN_POINT ( 'NONE',  ( -65.18805258578451856, -57.67964089302213893, 127.3758707571902846 ) ) ;
#32010 = DIRECTION ( 'NONE',  ( -1.000000000000000000, 0.000000000000000000, 0.000000000000000000 ) ) ;
#32011 = EDGE_CURVE ( 'NONE', #39800, #61594, #27196, .T. ) ;
#32012 = VERTEX_POINT ( 'NONE', #91889 ) ;
#32013 =( NAMED_UNIT ( * ) SI_UNIT ( $, .STERADIAN. ) SOLID_ANGLE_UNIT ( ) );
#32014 = CARTESIAN_POINT ( 'NONE',  ( 5.799999999999999822, 4.618802153517005848, 7.999999999999996447 ) ) ;
#32015 = CARTESIAN_POINT ( 'NONE',  ( -8.000000000000001776, -19.15624999999999289, 3.313708498984759387 ) ) ;
#32016 = ADVANCED_FACE ( 'NONE', ( #76761 ), #46445, .T. ) ;
#32017 = ORIENTED_EDGE ( 'NONE', *, *, #60565, .T. ) ;
#32018 = CARTESIAN_POINT ( 'NONE',  ( 5.656854249492378806, -9.875000004096769146, 5.656854249492381470 ) ) ;
#32019 = CARTESIAN_POINT ( 'NONE',  ( -27.84441264740780042, -20.64603143622934667, 31.82904849691709614 ) ) ;
#32020 = CARTESIAN_POINT ( 'NONE',  ( -39.36786586063794147, 490.3672761926048906, 11.50922959349409247 ) ) ;
#32021 = CARTESIAN_POINT ( 'NONE',  ( -1.000000000000000222, -15.98920185053290588, -10.19345919381858145 ) ) ;
#32022 = CARTESIAN_POINT ( 'NONE',  ( -9.918579450955563814, 88.79303912968688905, 1.297207292923873156 ) ) ;
#32023 = FACE_OUTER_BOUND ( 'NONE', #31603, .T. ) ;
#32024 = VECTOR ( 'NONE', #86714, 1000.000000000000000 ) ;
#32025 = SHAPE_DEFINITION_REPRESENTATION ( #100850, #49395 ) ;
#32026 = LINE ( 'NONE', #90242, #62620 ) ;
#32027 = ORIENTED_EDGE ( 'NONE', *, *, #34908, .F. ) ;
#32028 = DIRECTION ( 'NONE',  ( -1.000000000000000000, -1.224606353822377258E-16, -0.000000000000000000 ) ) ;
#32029 = CARTESIAN_POINT ( 'NONE',  ( 0.000000000000000000, 4.898587196589412829E-16, -4.000000000000000000 ) ) ;
#32030 = DIRECTION ( 'NONE',  ( 0.000000000000000000, -1.000000000000000000, 0.000000000000000000 ) ) ;
#32031 = CARTESIAN_POINT ( 'NONE',  ( -7.794767814137952833, -22.09678263551836253, -38.54438751446986089 ) ) ;
#32032 = CARTESIAN_POINT ( 'NONE',  ( 29.83349330513380693, 4.898587196589411843E-16, -4.000000000000001776 ) ) ;
#32033 = EDGE_CURVE ( 'NONE', #64161, #10296, #72437, .T. ) ;
#32034 = CARTESIAN_POINT ( 'NONE',  ( 0.000000000000000000, 0.000000000000000000, 3.469446951953614189E-15 ) ) ;
#32035 = ORIENTED_EDGE ( 'NONE', *, *, #31715, .F. ) ;
#32036 = CARTESIAN_POINT ( 'NONE',  ( 4.898587196589412829E-16, -9.312500004096769146, -8.000000000000000000 ) ) ;
#32037 = CIRCLE ( 'NONE', #66428, 5.000000000000010658 ) ;
#32038 = CARTESIAN_POINT ( 'NONE',  ( 96.42806518034892349, -57.62205372991940067, 204.4897109694943822 ) ) ;
#32039 = CARTESIAN_POINT ( 'NONE',  ( 35.04496600797013883, 464.5002996787647476, 18.88267410154261938 ) ) ;
#32040 = CARTESIAN_POINT ( 'NONE',  ( -9.500789678090530543, 51.30116685821661804, -3.607819160377707668 ) ) ;
#32041 = SURFACE_STYLE_USAGE ( .BOTH. , #38159 ) ;
#32042 = CARTESIAN_POINT ( 'NONE',  ( -6.536694770564420942, 53.53355194758169233, 7.404301873595124484 ) ) ;
#32043 = CARTESIAN_POINT ( 'NONE',  ( -74.42952615539968519, -60.00000000000000711, 176.4565370492489933 ) ) ;
#32044 = AXIS2_PLACEMENT_3D ( 'NONE', #70298, #77323, #3436 ) ;
#32045 = AXIS2_PLACEMENT_3D ( 'NONE', #28251, #94012, #20172 ) ;
#32046 = CIRCLE ( 'NONE', #23519, 4.000000000000007105 ) ;
#32047 = CARTESIAN_POINT ( 'NONE',  ( -40.85254446136673323, 441.7500193615117610, 25.53625856138344474 ) ) ;
#32048 = FILL_AREA_STYLE ('',( #56269 ) ) ;
#32049 = CARTESIAN_POINT ( 'NONE',  ( -39.13885763974980136, 324.4948203046521371, 17.18769520460729439 ) ) ;
#32050 = CARTESIAN_POINT ( 'NONE',  ( -85.50811847932432386, -39.29135958765198211, 185.4900395003674305 ) ) ;
#32051 = EDGE_LOOP ( 'NONE', ( #86513, #63721, #18805, #13066 ) ) ;
#32052 = CARTESIAN_POINT ( 'NONE',  ( 26.32888263779799587, 307.0379615089039476, -8.516298782527641720 ) ) ;
#32053 = AXIS2_PLACEMENT_3D ( 'NONE', #40368, #39857, #87874 ) ;
#32054 = ORIENTED_EDGE ( 'NONE', *, *, #84657, .F. ) ;
#32055 = CARTESIAN_POINT ( 'NONE',  ( -7.934914944860276265, -13.86845647200111920, -1.051261972695689551 ) ) ;
#32056 = ADVANCED_FACE ( 'NONE', ( #2335 ), #60086, .T. ) ;
#32057 = CARTESIAN_POINT ( 'NONE',  ( 0.000000000000000000, 0.000000000000000000, -2.716724522925831220 ) ) ;
#32058 = CARTESIAN_POINT ( 'NONE',  ( -82.06014707987355905, -37.79109599669338593, -13.64768699179697187 ) ) ;
#32059 = CARTESIAN_POINT ( 'NONE',  ( 0.000000000000000000, 0.000000000000000000, 0.000000000000000000 ) ) ;
#32061 = CIRCLE ( 'NONE', #45829, 15.00000000000000711 ) ;
#32060 = LINE ( 'NONE', #2170, #27573 ) ;
#32062 = VERTEX_POINT ( 'NONE', #52482 ) ;
#32063 = CARTESIAN_POINT ( 'NONE',  ( -33.13158811977432094, 464.8683774689862958, 15.82274808388414478 ) ) ;
#32064 = CARTESIAN_POINT ( 'NONE',  ( 12.86305608435086256, 23.43906773663930565, -4.864083290606698640 ) ) ;
#32065 = EDGE_CURVE ( 'NONE', #43945, #17545, #84324, .T. ) ;
#32066 = CARTESIAN_POINT ( 'NONE',  ( -22.88839214066252836, 27.45938914059933467, 33.17277703389353860 ) ) ;
#32067 = LINE ( 'NONE', #6160, #30819 ) ;
#32068 = CARTESIAN_POINT ( 'NONE',  ( 24.50706706878033359, -14.21045842199442077, -36.19515235953155496 ) ) ;
#32069 = CARTESIAN_POINT ( 'NONE',  ( -77.27742402748401673, -36.02507073553299222, 127.9111887702353840 ) ) ;
#32070 = ORIENTED_EDGE ( 'NONE', *, *, #807, .T. ) ;
#32071 = CARTESIAN_POINT ( 'NONE',  ( 48.80991865481109215, -14.21045842199436215, 55.83985330155353921 ) ) ;
#32072 = CARTESIAN_POINT ( 'NONE',  ( -10.00000000000000355, 15.00000000000000000, -10.00000000000000000 ) ) ;
#32073 = CARTESIAN_POINT ( 'NONE',  ( 92.56122130409121951, -57.65783127504731453, -18.25359173818277014 ) ) ;
#32074 = DIRECTION ( 'NONE',  ( 0.000000000000000000, 1.000000000000000000, 0.000000000000000000 ) ) ;
#32075 = CARTESIAN_POINT ( 'NONE',  ( 0.2565376335220204695, -2.516992571281984947, -6.499999999999999112 ) ) ;
#32076 = ORIENTED_EDGE ( 'NONE', *, *, #15158, .T. ) ;
#32077 = CARTESIAN_POINT ( 'NONE',  ( 43.58349330513380693, 1.593028355512270567E-15, 0.000000000000000000 ) ) ;
#32078 = DIRECTION ( 'NONE',  ( -0.5735764363510494901, -0.8191520442889894671, 0.000000000000000000 ) ) ;
#32079 = CARTESIAN_POINT ( 'NONE',  ( -7.188101187500002709, -21.31250000204838813, 2.977408999572648707 ) ) ;
#32080 = DIRECTION ( 'NONE',  ( -0.5735764363510494901, -0.8191520442889894671, 0.000000000000000000 ) ) ;
#32081 = CIRCLE ( 'NONE', #18302, 7.000000000000024869 ) ;
#32082 = CARTESIAN_POINT ( 'NONE',  ( 9.537909130738274399, 82.35385169036607067, -3.010726932293856795 ) ) ;
#32083 = CARTESIAN_POINT ( 'NONE',  ( -43.71217423904474231, 435.6632154632216043, 9.092528312227496912 ) ) ;
#32084 = FACE_OUTER_BOUND ( 'NONE', #57524, .T. ) ;
#32085 =( NAMED_UNIT ( * ) SI_UNIT ( $, .STERADIAN. ) SOLID_ANGLE_UNIT ( ) );
#32086 = ORIENTED_EDGE ( 'NONE', *, *, #93126, .F. ) ;
#32087 = CARTESIAN_POINT ( 'NONE',  ( -6.806778129255477872, 41.25019534346876782, -70.74215739106598733 ) ) ;
#32089 = CARTESIAN_POINT ( 'NONE',  ( 30.60635347677523299, -56.85241792156345042, 36.44043152735474678 ) ) ;
#32088 = DIRECTION ( 'NONE',  ( -1.000000000000000000, -1.224606353822377258E-16, -0.000000000000000000 ) ) ;
#32090 = CARTESIAN_POINT ( 'NONE',  ( 23.21751746555220564, 28.11705169068991950, -30.70617127781077116 ) ) ;
#32091 = ORIENTED_EDGE ( 'NONE', *, *, #3471, .F. ) ;
#32092 = ORIENTED_EDGE ( 'NONE', *, *, #69328, .F. ) ;
#32094 = FACE_BOUND ( 'NONE', #20044, .T. ) ;
#32093 = FILL_AREA_STYLE_COLOUR ( '', #2037 ) ;
#32095 = CARTESIAN_POINT ( 'NONE',  ( -16.36990510813551936, 294.5678840341198566, -2.060234697054666775 ) ) ;
#32096 = CYLINDRICAL_SURFACE ( 'NONE', #105171, 4.250000000000000000 ) ;
#32097 = CARTESIAN_POINT ( 'NONE',  ( 0.4142090692292615395, 46.18735664537236829, 16.31767936258320262 ) ) ;
#32098 = SURFACE_STYLE_FILL_AREA ( #55793 ) ;
#32099 = ORIENTED_EDGE ( 'NONE', *, *, #10849, .T. ) ;
#32100 = CARTESIAN_POINT ( 'NONE',  ( 8.295375291309756705, -59.99999999999999289, -42.48138218885826234 ) ) ;
#32101 = CONICAL_SURFACE ( 'NONE', #21801, 3.309500000000001663, 0.9599310885968770357 ) ;
#32102 = CARTESIAN_POINT ( 'NONE',  ( -9.953549941019272040, 46.18635266956800223, 12.94124874758487742 ) ) ;
#32103 = CARTESIAN_POINT ( 'NONE',  ( 0.000000000000000000, -1.550510257216834331, 112.0000000000000000 ) ) ;
#32104 = DIRECTION ( 'NONE',  ( 0.000000000000000000, -1.000000000000000000, 0.000000000000000000 ) ) ;
#32105 = LINE ( 'NONE', #48780, #1901 ) ;
#32106 = EDGE_LOOP ( 'NONE', ( #50372, #9779, #97309, #40042 ) ) ;
#32107 = EDGE_CURVE ( 'NONE', #58987, #96238, #106708, .T. ) ;
#32108 = EDGE_LOOP ( 'NONE', ( #36407, #17638, #23709, #49946 ) ) ;
#32109 = ORIENTED_EDGE ( 'NONE', *, *, #90040, .F. ) ;
#32110 = DIRECTION ( 'NONE',  ( 1.000000000000000000, 0.000000000000000000, 0.000000000000000000 ) ) ;
#32111 = CARTESIAN_POINT ( 'NONE',  ( -41.90771402882865715, 435.8631093490271269, 20.33118759140370102 ) ) ;
#32112 = CARTESIAN_POINT ( 'NONE',  ( 33.16841335515274380, 391.5752490215859325, 25.61045263980480158 ) ) ;
#32113 = CARTESIAN_POINT ( 'NONE',  ( -43.35589224434611566, 354.9930173192397547, 11.71192746841661148 ) ) ;
#32114 = CARTESIAN_POINT ( 'NONE',  ( -5.000000000001306510, -60.71953810597504742, 13.86359191440492467 ) ) ;
#32115 = CARTESIAN_POINT ( 'NONE',  ( 0.000000000000000000, 12.00000000000000000, 0.000000000000000000 ) ) ;
#32117 = ADVANCED_FACE ( 'NONE', ( #43868 ), #35821, .T. ) ;
#32116 = CARTESIAN_POINT ( 'NONE',  ( 23.86650669486618881, 1.474610560812782335E-15, 0.000000000000000000 ) ) ;
#32118 = EDGE_LOOP ( 'NONE', ( #101199, #67593, #33934, #9507, #23173 ) ) ;
#32119 = CARTESIAN_POINT ( 'NONE',  ( 30.06815944328944923, 12.45816842452745021, 39.66421731453360877 ) ) ;
#32120 = ORIENTED_EDGE ( 'NONE', *, *, #24647, .F. ) ;
#32121 = CARTESIAN_POINT ( 'NONE',  ( 22.33349330513380693, 1.593028355512270962E-15, 0.000000000000000000 ) ) ;
#32122 = FACE_OUTER_BOUND ( 'NONE', #47891, .T. ) ;
#32123 = LINE ( 'NONE', #50395, #100694 ) ;
#32124 = AXIS2_PLACEMENT_3D ( 'NONE', #69757, #44419, #36370 ) ;
#32125 = AXIS2_PLACEMENT_3D ( 'NONE', #92581, #10592, #43510 ) ;
#32126 = AXIS2_PLACEMENT_3D ( 'NONE', #38788, #86818, #103510 ) ;
#32127 = PRESENTATION_LAYER_ASSIGNMENT (  '', '', ( #78591 ) ) ;
#32128 =( BOUNDED_SURFACE ( )  B_SPLINE_SURFACE ( 3, 2, ( 
 ( #58786, #10211, #41522 ),
 ( #66330, #83049, #42052 ),
 ( #2109, #100812, #40995 ),
 ( #1022, #25929, #11261 ) ),
 .UNSPECIFIED., .F., .F., .F. ) 
 B_SPLINE_SURFACE_WITH_KNOTS ( ( 4, 4 ),
 ( 3, 3 ),
 ( 2.905661822261151883E-17, 0.0002890439564778435463 ),
 ( 0.000000000000000000, 1.000000000000000000 ),
 .UNSPECIFIED. ) 
 GEOMETRIC_REPRESENTATION_ITEM ( )  RATIONAL_B_SPLINE_SURFACE ( (
 ( 1.000000000000000000, 0.8001746426090936559, 1.000000000000000000),
 ( 1.000000000000000000, 0.7985501684305429393, 1.000000000000000000),
 ( 1.000000000000000000, 0.7968416491994178008, 1.000000000000000000),
 ( 1.000000000000000000, 0.7950530193019601510, 1.000000000000000000) ) ) 
 REPRESENTATION_ITEM ( '' )  SURFACE ( )  );
#32129 = CARTESIAN_POINT ( 'NONE',  ( -77.37933372540865662, -59.99999999999995737, 150.9740157483943506 ) ) ;
#32130 = CARTESIAN_POINT ( 'NONE',  ( 68.68987387269132228, -18.63274608647051878, 85.98930702359679401 ) ) ;
#32131 = CIRCLE ( 'NONE', #66519, 45.10524579772351217 ) ;
#32132 = EDGE_LOOP ( 'NONE', ( #1690, #37765 ) ) ;
#32133 = CARTESIAN_POINT ( 'NONE',  ( 17.50000000000002487, 48.88514111886252067, 64.06409622908613244 ) ) ;
#32134 = CIRCLE ( 'NONE', #35614, 3.000000000000012434 ) ;
#32135 = CARTESIAN_POINT ( 'NONE',  ( -6.321708934325914520, 10.35608347206918545, 3.012444762083620109 ) ) ;
#32136 = EDGE_CURVE ( 'NONE', #4466, #86580, #95553, .T. ) ;
#32137 = EDGE_LOOP ( 'NONE', ( #45288, #30540, #5084, #19515 ) ) ;
#32138 = FILL_AREA_STYLE ('',( #55832 ) ) ;
#32139 = FILL_AREA_STYLE ('',( #71506 ) ) ;
#32140 = AXIS2_PLACEMENT_3D ( 'NONE', #50269, #42176, #84241 ) ;
#32141 = CARTESIAN_POINT ( 'NONE',  ( -37.00151214922456688, 491.8254423329677252, 12.57683263657885497 ) ) ;
#32142 = CARTESIAN_POINT ( 'NONE',  ( -8.000000000000000000, -31.53125000409677270, -3.313708498984762496 ) ) ;
#32143 = CARTESIAN_POINT ( 'NONE',  ( -7.137815226409945701, -4.999999999999998224, 4.175893272574815462 ) ) ;
#32144 = CARTESIAN_POINT ( 'NONE',  ( 0.000000000000000000, 6.123233995736770227E-16, -5.000000000000002665 ) ) ;
#32145 =( GEOMETRIC_REPRESENTATION_CONTEXT ( 3 ) GLOBAL_UNCERTAINTY_ASSIGNED_CONTEXT ( ( #38595 ) ) GLOBAL_UNIT_ASSIGNED_CONTEXT ( ( #3642, #61355, #61896 ) ) REPRESENTATION_CONTEXT ( 'NONE', 'WORKASPACE' ) );
#32146 = CARTESIAN_POINT ( 'NONE',  ( 9.699189539447125696, 33.17692228246711039, -2.444343703917216448 ) ) ;
#32147 = CARTESIAN_POINT ( 'NONE',  ( 18.58349330513380693, -3.851859888774471706E-31, 4.000000000000001776 ) ) ;
#32148 = CARTESIAN_POINT ( 'NONE',  ( 6.663820940124920433, 304.7444949031477677, 9.914190422159109062 ) ) ;
#32149 = ORIENTED_EDGE ( 'NONE', *, *, #30378, .T. ) ;
#32150 = CARTESIAN_POINT ( 'NONE',  ( 43.55054245096676624, 486.2288135416363275, 8.070792277557991667 ) ) ;
#32151 = DIRECTION ( 'NONE',  ( 0.000000000000000000, 0.000000000000000000, 1.000000000000000000 ) ) ;
#32152 = CARTESIAN_POINT ( 'NONE',  ( 8.550030583596393896, -60.00000000000000000, 39.63663732540850759 ) ) ;
#32153 = CARTESIAN_POINT ( 'NONE',  ( -98.86655644987608582, -30.00000000000000355, 189.1318155084324246 ) ) ;
#32154 = B_SPLINE_CURVE_WITH_KNOTS ( 'NONE', 3,
 ( #61491, #70625, #20544, #13426, #53382, #38283, #29669, #95425, #85210, #11301, #4295, #63068, #21564, #46348, #5365, #52301, #77120, #36176, #69045, #38794, #15024, #54947, #64145, #47393, #5870, #23691, #47914, #48449, #46868, #24224, #106690, #96498, #31257, #80822, #22092, #40906 ),
 .UNSPECIFIED., .F., .F.,
 ( 4, 2, 2, 2, 2, 2, 2, 2, 2, 2, 2, 2, 2, 2, 2, 2, 2, 4 ),
 ( 0.000000000000000000, 0.0008074604767267247983, 0.001614920953453449597, 0.002422381430180174395, 0.003229841906906899193, 0.004037302383633624425, 0.004844762860360348790, 0.005652223337087073154, 0.006459683813813798386, 0.007267144290540523618, 0.008074604767267248850, 0.008882065243993972348, 0.009689525720720697580, 0.01049698619744742281, 0.01130444667417414631, 0.01211190715090087154, 0.01251563738926423502, 0.01291936762762759677 ),
 .UNSPECIFIED. ) ;
#32155 = CARTESIAN_POINT ( 'NONE',  ( -89.99999999999997158, -52.00000000000000000, 196.0238439516549818 ) ) ;
#32156 = CARTESIAN_POINT ( 'NONE',  ( 54.56491434472576429, -57.67593140129608997, 90.07630786268572365 ) ) ;
#32158 = CARTESIAN_POINT ( 'NONE',  ( -9.686158086385539434, 53.40057947480783440, 3.329218293922611593 ) ) ;
#32157 = CARTESIAN_POINT ( 'NONE',  ( 8.000000000000000000, -15.68750000409677092, 0.000000000000000000 ) ) ;
#32159 = CARTESIAN_POINT ( 'NONE',  ( -39.68467815576735802, 459.8383127612378303, 1.879537633271044728 ) ) ;
#32160 = CARTESIAN_POINT ( 'NONE',  ( -7.500000000000000888, -3.640541674360523228, -0.7158139487964588765 ) ) ;
#32161 = CARTESIAN_POINT ( 'NONE',  ( 27.99999999999999645, 0.000000000000000000, 0.000000000000000000 ) ) ;
#32162 = CARTESIAN_POINT ( 'NONE',  ( -6.181622435106722158, -60.00000000000001421, 39.62780610759933353 ) ) ;
#32163 = CARTESIAN_POINT ( 'NONE',  ( 34.16642289233210050, 463.8422268500519863, 18.98106911353328385 ) ) ;
#32164 = VECTOR ( 'NONE', #53080, 1000.000000000000000 ) ;
#32165 = CARTESIAN_POINT ( 'NONE',  ( -86.00392355705747605, -61.04916185595598677, 194.3144374245121639 ) ) ;
#32166 = ORIENTED_EDGE ( 'NONE', *, *, #89921, .T. ) ;
#32167 = CARTESIAN_POINT ( 'NONE',  ( 17.49999999999876721, 50.01371676752351192, 60.25403804532950858 ) ) ;
#32168 = CARTESIAN_POINT ( 'NONE',  ( 10.99833518290787815, -10.49270544111268144, 18.32972597813727589 ) ) ;
#32169 = CARTESIAN_POINT ( 'NONE',  ( -9.217550163516040840, -39.47610853938331843, 30.47143711703355251 ) ) ;
#32170 = DIRECTION ( 'NONE',  ( 0.000000000000000000, 0.000000000000000000, 1.000000000000000000 ) ) ;
#32171 = CARTESIAN_POINT ( 'NONE',  ( -101.1267960657979756, -59.99999999999995737, 195.0049809712846525 ) ) ;
#32172 = EDGE_CURVE ( 'NONE', #20574, #83726, #37946, .T. ) ;
#32173 = ORIENTED_EDGE ( 'NONE', *, *, #70152, .T. ) ;
#32174 = DIRECTION ( 'NONE',  ( 1.000000000000000000, 0.000000000000000000, 0.000000000000000000 ) ) ;
#32175 = CARTESIAN_POINT ( 'NONE',  ( -6.016266904914970404, -5.000000000005825562, -16.21640811047240049 ) ) ;
#32176 = CARTESIAN_POINT ( 'NONE',  ( -30.10565283232759981, 7.858405490276831884, -42.03377155531590148 ) ) ;
#32177 = AXIS2_PLACEMENT_3D ( 'NONE', #98360, #48204, #90273 ) ;
#32178 = CARTESIAN_POINT ( 'NONE',  ( 32.21125840474181956, 298.9095371842905138, -9.102426614015140416 ) ) ;
#32179 = CARTESIAN_POINT ( 'NONE',  ( 20.00000000000000000, 12.99999999999999289, -6.999999999999999112 ) ) ;
#32180 = EDGE_CURVE ( 'NONE', #48676, #83974, #103267, .T. ) ;
#32181 = CARTESIAN_POINT ( 'NONE',  ( -7.744329845603314944, -81.53711769846545110, -2.018701143083234673 ) ) ;
#32182 = CARTESIAN_POINT ( 'NONE',  ( 73.53860074992563511, -59.99999999999999289, 167.5715982711623440 ) ) ;
#32183 = CARTESIAN_POINT ( 'NONE',  ( -32.54922218626916930, 319.8023524069591303, -6.363686095274232457 ) ) ;
#32184 = EDGE_LOOP ( 'NONE', ( #70944, #100793, #97342 ) ) ;
#32185 = CARTESIAN_POINT ( 'NONE',  ( -7.093569395281086543, -30.00000000000000355, 3.069303058423363151 ) ) ;
#32186 = CARTESIAN_POINT ( 'NONE',  ( -9.253500431420452088, 251.2977154991770590, 3.792688295761950101 ) ) ;
#32187 =( GEOMETRIC_REPRESENTATION_CONTEXT ( 3 ) GLOBAL_UNCERTAINTY_ASSIGNED_CONTEXT ( ( #68839 ) ) GLOBAL_UNIT_ASSIGNED_CONTEXT ( ( #61167, #70842, #93534 ) ) REPRESENTATION_CONTEXT ( 'NONE', 'WORKASPACE' ) );
#32188 = AXIS2_PLACEMENT_3D ( 'NONE', #24089, #48839, #16492 ) ;
#32189 = VECTOR ( 'NONE', #48126, 1000.000000000000000 ) ;
#32190 = EDGE_CURVE ( 'NONE', #103730, #2640, #8038, .T. ) ;
#32192 = DIRECTION ( 'NONE',  ( -1.000000000000000000, -1.224606353822377258E-16, -0.000000000000000000 ) ) ;
#32191 = CARTESIAN_POINT ( 'NONE',  ( 12.46466094585187889, -29.99999999999991118, 37.03825901911487506 ) ) ;
#32193 = CYLINDRICAL_SURFACE ( 'NONE', #14852, 1.250000000000001110 ) ;
#32194 = FILL_AREA_STYLE ('',( #39748 ) ) ;
#32195 = ORIENTED_EDGE ( 'NONE', *, *, #76053, .F. ) ;
#32196 = B_SPLINE_CURVE_WITH_KNOTS ( 'NONE', 3,
 ( #85058, #28442, #1990, #67807 ),
 .UNSPECIFIED., .F., .F.,
 ( 4, 4 ),
 ( 0.000000000000000000, 0.0004475792522134993041 ),
 .UNSPECIFIED. ) ;
#32197 = AXIS2_PLACEMENT_3D ( 'NONE', #24119, #72627, #47806 ) ;
#32198 = EDGE_CURVE ( 'NONE', #52930, #27869, #68878, .T. ) ;
#32199 = CARTESIAN_POINT ( 'NONE',  ( -22.76293769579003623, 305.5621053821230930, 10.09118165409745593 ) ) ;
#32200 = EDGE_LOOP ( 'NONE', ( #68730, #47911, #37171, #71567 ) ) ;
#32201 = CARTESIAN_POINT ( 'NONE',  ( 33.88237199998279436, 485.0486819176492759, 1.241522336454514264 ) ) ;
#32202 = CARTESIAN_POINT ( 'NONE',  ( 31.91891815526927445, 439.7370520509067546, 23.87859572923007434 ) ) ;
#32203 = PRESENTATION_STYLE_ASSIGNMENT (( #88826 ) ) ;
#32204 = ORIENTED_EDGE ( 'NONE', *, *, #97255, .T. ) ;
#32205 =( NAMED_UNIT ( * ) PLANE_ANGLE_UNIT ( ) SI_UNIT ( $, .RADIAN. ) );
#32206 = CARTESIAN_POINT ( 'NONE',  ( -21.44411787121075363, -60.00000000000489564, 42.81394995815333715 ) ) ;
#32207 = CARTESIAN_POINT ( 'NONE',  ( 44.29544435252744705, 435.1888869815376779, 13.53377863749212828 ) ) ;
#32208 = CARTESIAN_POINT ( 'NONE',  ( 67.29303862372746892, -60.00000000000000000, 127.0361366969463859 ) ) ;
#32209 = CARTESIAN_POINT ( 'NONE',  ( -1.484885661199817548E-13, 25.16821295365152622, -40.75000000000150635 ) ) ;
#32211 = CARTESIAN_POINT ( 'NONE',  ( 15.72127475791274342, -42.95378344181465025, 31.23277305341622778 ) ) ;
#32210 = CARTESIAN_POINT ( 'NONE',  ( -106.9310521912263710, -14.21045842199434794, 169.9232300575910131 ) ) ;
#32212 = CARTESIAN_POINT ( 'NONE',  ( 82.81422886519544591, -37.99999999999996447, 23.20150160915743243 ) ) ;
#32213 = CARTESIAN_POINT ( 'NONE',  ( 28.09999999999999787, 1.533819458162526451E-15, 0.000000000000000000 ) ) ;
#32214 = CARTESIAN_POINT ( 'NONE',  ( -47.78472977372928909, -18.76678906305324901, 41.09994231454981417 ) ) ;
#32215 = CARTESIAN_POINT ( 'NONE',  ( -1.250481436861478945, 34.56029847975127467, -28.65557344373550563 ) ) ;
#32216 = ORIENTED_EDGE ( 'NONE', *, *, #73533, .T. ) ;
#32217 = CARTESIAN_POINT ( 'NONE',  ( 52.81650669486619165, -1.232595164407830946E-29, 4.000000000000007105 ) ) ;
#32218 = DIRECTION ( 'NONE',  ( 1.000000000000000000, -0.000000000000000000, -0.000000000000000000 ) ) ;
#32219 = DIRECTION ( 'NONE',  ( -0.000000000000000000, 1.000000000000000000, -0.000000000000000000 ) ) ;
#32220 = DIRECTION ( 'NONE',  ( 0.000000000000000000, 0.000000000000000000, 1.000000000000000000 ) ) ;
#32221 = PRESENTATION_STYLE_ASSIGNMENT (( #103959 ) ) ;
#32222 = CARTESIAN_POINT ( 'NONE',  ( 31.19792890532719198, 414.2215770364159084, 25.44228638033458623 ) ) ;
#32224 = ORIENTED_EDGE ( 'NONE', *, *, #35503, .T. ) ;
#32223 = AXIS2_PLACEMENT_3D ( 'NONE', #63387, #95734, #56298 ) ;
#32225 = CARTESIAN_POINT ( 'NONE',  ( -16.58646281676584522, 37.15392203743714816, -21.81520449073906320 ) ) ;
#32226 = VERTEX_POINT ( 'NONE', #20721 ) ;
#32227 = CARTESIAN_POINT ( 'NONE',  ( 88.50590120176012476, -30.00000000000198597, 198.8119346494863464 ) ) ;
#32228 = CARTESIAN_POINT ( 'NONE',  ( 19.43524536873321651, 41.87218652733789526, -80.47567652358424084 ) ) ;
#32229 = CARTESIAN_POINT ( 'NONE',  ( 5.744147429006506655, 41.99823327698700837, -59.60979843494948938 ) ) ;
#32230 = AXIS2_PLACEMENT_3D ( 'NONE', #105461, #9394, #67667 ) ;
#32231 = CARTESIAN_POINT ( 'NONE',  ( -3.444109705163657007E-15, 24.73290587908618932, -14.06164498842270483 ) ) ;
#32232 = CARTESIAN_POINT ( 'NONE',  ( 92.46214547348466795, -30.00000000000000000, 102.8783225717633627 ) ) ;
#32233 = CARTESIAN_POINT ( 'NONE',  ( 7.896571385775231100, 101.2100200065424787, 1.305932416347435732 ) ) ;
#32234 = ORIENTED_EDGE ( 'NONE', *, *, #9459, .F. ) ;
#32235 = ADVANCED_FACE ( 'NONE', ( #69232 ), #46006, .T. ) ;
#32236 = ORIENTED_EDGE ( 'NONE', *, *, #62548, .F. ) ;
#32237 = VERTEX_POINT ( 'NONE', #103699 ) ;
#32238 = CARTESIAN_POINT ( 'NONE',  ( -13.50000000000000000, 7.794228634059933825, -13.00000000000000000 ) ) ;
#32239 = CARTESIAN_POINT ( 'NONE',  ( 22.59000000144133935, 25.42954125889399819, 33.04937649237353980 ) ) ;
#32240 = ADVANCED_FACE ( 'NONE', ( #53559 ), #39537, .F. ) ;
#32241 = ADVANCED_FACE ( 'NONE', ( #28260 ), #6784, .F. ) ;
#32242 = EDGE_LOOP ( 'NONE', ( #20457, #72733, #41119, #69128, #62464 ) ) ;
#32243 = CARTESIAN_POINT ( 'NONE',  ( 9.537927238823508347, 107.6462685711817926, -3.010735687602429600 ) ) ;
#32244 = ORIENTED_EDGE ( 'NONE', *, *, #7200, .T. ) ;
#32245 = DIRECTION ( 'NONE',  ( -1.000000000000000000, 0.000000000000000000, 0.000000000000000000 ) ) ;
#32246 = CARTESIAN_POINT ( 'NONE',  ( 85.83366297925716992, -38.65129167634649576, 198.9702531129130421 ) ) ;
#32247 = CARTESIAN_POINT ( 'NONE',  ( 14.23326139838831494, 6.534605160808406588, 7.647391678231034717 ) ) ;
#32248 = CARTESIAN_POINT ( 'NONE',  ( 0.000000000000000000, 0.000000000000000000, -3.432199999999999918 ) ) ;
#32249 = CARTESIAN_POINT ( 'NONE',  ( 40.04056949100335316, 318.9660535511408739, 7.801086534252953619 ) ) ;
#32250 = CONICAL_SURFACE ( 'NONE', #40851, 4.172000000000001485, 0.9599310885968750373 ) ;
#32251 = FACE_OUTER_BOUND ( 'NONE', #80810, .T. ) ;
#32252 = CONICAL_SURFACE ( 'NONE', #92505, 5.000000000000001776, 0.9599310885968803664 ) ;
#32253 = CARTESIAN_POINT ( 'NONE',  ( 11.36650669486618881, 1.474610560812782335E-15, 0.000000000000000000 ) ) ;
#32254 = CARTESIAN_POINT ( 'NONE',  ( -4.973317752991197160, -46.53140123174669895, 102.2736751349651456 ) ) ;
#32255 =( BOUNDED_SURFACE ( )  B_SPLINE_SURFACE ( 3, 2, ( 
 ( #20206, #12052, #79837 ),
 ( #43895, #105188, #55020 ),
 ( #22170, #22707, #14557 ),
 ( #30799, #14033, #23228 ) ),
 .UNSPECIFIED., .F., .F., .F. ) 
 B_SPLINE_SURFACE_WITH_KNOTS ( ( 4, 4 ),
 ( 3, 3 ),
 ( 8.673617379884035472E-19, 0.003511371752238591840 ),
 ( 0.000000000000000000, 1.000000000000000000 ),
 .UNSPECIFIED. ) 
 GEOMETRIC_REPRESENTATION_ITEM ( )  RATIONAL_B_SPLINE_SURFACE ( (
 ( 1.000000000000000000, 0.7409272757993143887, 1.000000000000000000),
 ( 1.000000000000000000, 0.7572402302192213774, 1.000000000000000000),
 ( 1.000000000000000000, 0.7731133056332801790, 1.000000000000000000),
 ( 1.000000000000000000, 0.7888522786295014688, 1.000000000000000000) ) ) 
 REPRESENTATION_ITEM ( '' )  SURFACE ( )  );
#32256 = CARTESIAN_POINT ( 'NONE',  ( 1.810361544441083977E-15, 0.5000000000000000000, -14.78272384904389192 ) ) ;
#32257 = EDGE_CURVE ( 'NONE', #105650, #94111, #51598, .T. ) ;
#32258 = CARTESIAN_POINT ( 'NONE',  ( -5.000000000000000000, -14.21727251091160404, 9.320362779991915758 ) ) ;
#32259 = VERTEX_POINT ( 'NONE', #31952 ) ;
#32260 = CARTESIAN_POINT ( 'NONE',  ( -42.43166099484149356, 436.1632441641000355, 19.16791492761042903 ) ) ;
#32262 = CARTESIAN_POINT ( 'NONE',  ( -24.91217021099775764, 295.6308500594226985, 2.104243703054258674 ) ) ;
#32261 =( NAMED_UNIT ( * ) SI_UNIT ( $, .STERADIAN. ) SOLID_ANGLE_UNIT ( ) );
#32263 = CARTESIAN_POINT ( 'NONE',  ( -12.36633005457817802, -4.301166014002332894, -76.75180828602299243 ) ) ;
#32264 = UNCERTAINTY_MEASURE_WITH_UNIT (LENGTH_MEASURE( 1.000000000000000082E-05 ), #74122, 'distance_accuracy_value', 'NONE');
#32265 = DIRECTION ( 'NONE',  ( 0.000000000000000000, 0.000000000000000000, 1.000000000000000000 ) ) ;
#32266 = CARTESIAN_POINT ( 'NONE',  ( -1.469576158976823947E-15, -17.37499999999999289, 8.000000000000000000 ) ) ;
#32267 = TOROIDAL_SURFACE ( 'NONE', #56312, 6.999999999999999112, 0.5000000000000000000 ) ;
#32269 = CARTESIAN_POINT ( 'NONE',  ( -2.352990130084491319E-16, 7.505553499465148271, -6.064240316920404439 ) ) ;
#32268 = COLOUR_RGB ( '', 0.08235294, 0.09019608, 0.10196078) ;
#32270 = EDGE_CURVE ( 'NONE', #29313, #98120, #47572, .T. ) ;
#32271 = CARTESIAN_POINT ( 'NONE',  ( -7.934203308536663890, 101.1329965998220217, 1.057099537198549655 ) ) ;
#32272 = CIRCLE ( 'NONE', #73574, 3.309500000000001663 ) ;
#32273 = CIRCLE ( 'NONE', #63301, 4.000000000000001776 ) ;
#32274 = STYLED_ITEM ( 'NONE', ( #101421 ), #3855 ) ;
#32275 = CARTESIAN_POINT ( 'NONE',  ( 6.615539890938310741, 303.7455199599310731, 9.914405304616634496 ) ) ;
#32276 = ORIENTED_EDGE ( 'NONE', *, *, #48991, .T. ) ;
#32277 = CARTESIAN_POINT ( 'NONE',  ( 84.23888984516474920, -53.80018453417523716, 189.3803214424800672 ) ) ;
#32278 = EDGE_CURVE ( 'NONE', #89827, #79740, #10246, .T. ) ;
#32279 = CARTESIAN_POINT ( 'NONE',  ( 1.128238012697730275, 300.0000000000000000, 9.936150108905557943 ) ) ;
#32280 =( NAMED_UNIT ( * ) PLANE_ANGLE_UNIT ( ) SI_UNIT ( $, .RADIAN. ) );
#32281 = VERTEX_POINT ( 'NONE', #24410 ) ;
#32282 = CARTESIAN_POINT ( 'NONE',  ( 82.96216422859413342, -57.67107778185281575, -28.42881364454757076 ) ) ;
#32283 = CARTESIAN_POINT ( 'NONE',  ( 36.57768354961403645, 437.5705742298895302, 4.260889744331655571 ) ) ;
#32284 = DIRECTION ( 'NONE',  ( 0.000000000000000000, 0.000000000000000000, 1.000000000000000000 ) ) ;
#32285 = AXIS2_PLACEMENT_3D ( 'NONE', #53522, #12511, #82016 ) ;
#32286 = DIRECTION ( 'NONE',  ( -0.000000000000000000, 1.000000000000000000, -0.000000000000000000 ) ) ;
#32287 = AXIS2_PLACEMENT_3D ( 'NONE', #68803, #61236, #62304 ) ;
#32288 = CARTESIAN_POINT ( 'NONE',  ( -81.59242062888966984, -30.00000000000000355, -7.123010226814199264 ) ) ;
#32289 = CARTESIAN_POINT ( 'NONE',  ( 28.49053509030336073, 18.29756676117402492, 40.46890581211940940 ) ) ;
#32290 = CARTESIAN_POINT ( 'NONE',  ( -2.094395098902661623, -3.000000000000000000, 8.000000000000000000 ) ) ;
#32291 = DIRECTION ( 'NONE',  ( -1.000000000000000000, -1.224606353822377258E-16, -0.000000000000000000 ) ) ;
#32293 = DIRECTION ( 'NONE',  ( 0.5735764363510491570, -0.8191520442889895781, 1.003171929053522035E-16 ) ) ;
#32292 = CARTESIAN_POINT ( 'NONE',  ( 3.991107381396987730, -48.94960763643569379, 104.5611067885112959 ) ) ;
#32294 = CIRCLE ( 'NONE', #51197, 4.172000000000009479 ) ;
#32295 = CARTESIAN_POINT ( 'NONE',  ( 1.530808498934196254E-15, 3.999999999999996447, -12.00000000000003908 ) ) ;
#32296 = CARTESIAN_POINT ( 'NONE',  ( -31.95313894478998051, 438.9705935198780935, 23.61757669276694571 ) ) ;
#32297 = DIRECTION ( 'NONE',  ( -1.000000000000000000, -1.224606353822377258E-16, -0.000000000000000000 ) ) ;
#32298 = CARTESIAN_POINT ( 'NONE',  ( 0.000000000000000000, -5.000000000000000888, -73.00000000000001421 ) ) ;
#32299 = CARTESIAN_POINT ( 'NONE',  ( 14.83349330513380693, 4.000000000000002665, 0.000000000000000000 ) ) ;
#32300 = LINE ( 'NONE', #65171, #95855 ) ;
#32301 = CARTESIAN_POINT ( 'NONE',  ( -97.88527447864335329, -38.00000000000000000, 192.5969185656728371 ) ) ;
#32302 = STYLED_ITEM ( 'NONE', ( #75567 ), #29483 ) ;
#32303 = ORIENTED_EDGE ( 'NONE', *, *, #45812, .F. ) ;
#32304 = DIRECTION ( 'NONE',  ( -1.000000000000000000, -1.224606353822377258E-16, -0.000000000000000000 ) ) ;
#32305 = DIRECTION ( 'NONE',  ( 0.000000000000000000, 0.000000000000000000, 1.000000000000000000 ) ) ;
#32306 = AXIS2_PLACEMENT_3D ( 'NONE', #54360, #87303, #13386 ) ;
#32307 = CARTESIAN_POINT ( 'NONE',  ( -20.54902761521100629, -18.70952130878982089, -33.64984671759549428 ) ) ;
#32309 = CARTESIAN_POINT ( 'NONE',  ( -28.41674959901979847, -34.58966139483771229, -31.03040257763374399 ) ) ;
#32308 = CYLINDRICAL_SURFACE ( 'NONE', #70866, 4.000000000000000000 ) ;
#32310 = EDGE_CURVE ( 'NONE', #55614, #21618, #69174, .T. ) ;
#32311 = VERTEX_POINT ( 'NONE', #48097 ) ;
#32312 = EDGE_CURVE ( 'NONE', #20227, #95973, #9924, .T. ) ;
#32313 = ORIENTED_EDGE ( 'NONE', *, *, #88401, .T. ) ;
#32314 = CARTESIAN_POINT ( 'NONE',  ( 42.19180677453717720, 462.2931784592651638, 3.389262873192018244 ) ) ;
#32315 = EDGE_CURVE ( 'NONE', #76425, #85977, #25441, .T. ) ;
#32316 = EDGE_CURVE ( 'NONE', #89487, #50732, #16427, .T. ) ;
#32317 = CARTESIAN_POINT ( 'NONE',  ( -3.979266480701241449, -30.00000000000000000, -6.940132439339151027 ) ) ;
#32318 = CARTESIAN_POINT ( 'NONE',  ( 3.400000000000000355, 0.000000000000000000, -2.716724522925831220 ) ) ;
#32319 = B_SPLINE_CURVE_WITH_KNOTS ( 'NONE', 3,
 ( #7705, #51753, #19978, #33092, #74040, #65957, #60416, #57846, #93825, #84135, #3218, #27537, #93294, #101904, #90772, #10233, #43669, #68494, #36160, #44214, #76557, #77101, #59877, #2668, #101383, #19450, #98326, #2127, #57317, #52285, #85196, #122, #43148, #84668, #76031, #69031, #28063, #60935, #35082, #67951, #92750, #10753, #81579, #73500, #18909, #106399, #40616, #32560, #90235, #65432, #100833, #24482, #16340, #49226, #82128, #8245, #41157, #98836, #24993, #16890, #49770, #26998, #54387, #45281, #30708, #11821, #13409, #36690, #54931, #20526, #94900, #102443, #61472, #4279, #46853, #79221, #95953, #29139, #52823, #70610, #37207, #29653, #37748, #38781, #86283, #21042, #53876, #95410, #70076, #12882, #53363, #87333, #13942, #62525, #21552, #62008, #12355, #102977, #79749, #78160, #5856, #28588, #46334, #71647, #44754, #86809, #69553 ),
 .UNSPECIFIED., .F., .F.,
 ( 4, 2, 2, 2, 2, 1, 2, 2, 2, 1, 1, 2, 2, 1, 2, 2, 1, 1, 2, 2, 1, 1, 2, 2, 1, 2, 2, 2, 2, 2, 1, 2, 2, 2, 1, 2, 2, 1, 1, 2, 2, 2, 2, 1, 2, 2, 1, 1, 2, 2, 1, 2, 2, 1, 2, 2, 1, 2, 2, 1, 1, 2, 2, 4 ),
 ( 0.000000000000000000, 0.06202959713925935287, 0.1240591942785187057, 0.1279360440997223958, 0.1318128939209261274, 0.1395665935633337573, 0.1550739928481488783, 0.1860887914177792313, 0.1880272163283812359, 0.1899656412389832127, 0.1938424910601872775, 0.2015961907025952682, 0.2171035899874111386, 0.2180728024427120992, 0.2185574086703626628, 0.2190420148980131709, 0.2209804398086148702, 0.2248572896298183244, 0.2326109892722254824, 0.2481183885570396597, 0.2490876010123405093, 0.2495722072399910174, 0.2498145103538162159, 0.2500568134676414700, 0.2519952383782430583, 0.2558720881994462348, 0.2636257878418524769, 0.2791331871266647946, 0.2810716120372663274, 0.2820408244925671215, 0.2830100369478679156, 0.2868868867690712032, 0.2946405864114776119, 0.3101479856962904291, 0.3120864106068919619, 0.3123287137207171882, 0.3125710168345423590, 0.3130556230621926450, 0.3140248355174932171, 0.3179016853386955610, 0.3256553849811001378, 0.3411627842659093468, 0.3721775828355277094, 0.3741160077461288536, 0.3746006139737790841, 0.3750852202014293146, 0.3760544326567299422, 0.3799312824779323972, 0.3876849821203374180, 0.4031923814051473487, 0.4051308063157485484, 0.4061000187710491205, 0.4070692312263496926, 0.4109460810475520920, 0.4186997806899569463, 0.4342071799747664884, 0.4361456048853676881, 0.4371148173406683157, 0.4375994235683186018, 0.4380840297959688878, 0.4419608796171713982, 0.4497145792595763636, 0.4652219785443864053, 0.4962367771140062667 ),
 .UNSPECIFIED. ) ;
#32320 = CARTESIAN_POINT ( 'NONE',  ( -50.52133408753726229, -59.99999999999999289, -37.80162784956270627 ) ) ;
#32321 = VERTEX_POINT ( 'NONE', #50747 ) ;
#32322 = CARTESIAN_POINT ( 'NONE',  ( 14.20401263913925760, -24.37963745956056272, -30.50600035239884633 ) ) ;
#32323 = CARTESIAN_POINT ( 'NONE',  ( -3.348056043397916071, -1.092793117426783089, 104.4613933532584440 ) ) ;
#32325 = CARTESIAN_POINT ( 'NONE',  ( -47.50581258546153407, 12.72782412601323720, 14.46700746232338908 ) ) ;
#32324 = DIRECTION ( 'NONE',  ( 0.000000000000000000, 0.000000000000000000, 1.000000000000000000 ) ) ;
#32326 = EDGE_CURVE ( 'NONE', #63501, #38791, #64018, .T. ) ;
#32327 = CARTESIAN_POINT ( 'NONE',  ( -80.25168178368869576, -53.38897274610327770, 165.9826718664497776 ) ) ;
#32328 =( GEOMETRIC_REPRESENTATION_CONTEXT ( 3 ) GLOBAL_UNCERTAINTY_ASSIGNED_CONTEXT ( ( #58036 ) ) GLOBAL_UNIT_ASSIGNED_CONTEXT ( ( #61330, #59732, #68894 ) ) REPRESENTATION_CONTEXT ( 'NONE', 'WORKASPACE' ) );
#32329 = ORIENTED_EDGE ( 'NONE', *, *, #25561, .F. ) ;
#32330 = EDGE_CURVE ( 'NONE', #63739, #94695, #86042, .T. ) ;
#32331 = VERTEX_POINT ( 'NONE', #27609 ) ;
#32332 = VERTEX_POINT ( 'NONE', #27074 ) ;
#32333 = CARTESIAN_POINT ( 'NONE',  ( 31.19344562713908431, 380.6578681173627956, 24.42638549347173793 ) ) ;
#32334 = CARTESIAN_POINT ( 'NONE',  ( -5.000000000000000000, -14.65803281199242036, 12.34559804589020260 ) ) ;
#32335 =( NAMED_UNIT ( * ) SI_UNIT ( $, .STERADIAN. ) SOLID_ANGLE_UNIT ( ) );
#32336 = ORIENTED_EDGE ( 'NONE', *, *, #70864, .T. ) ;
#32337 = DIRECTION ( 'NONE',  ( 0.000000000000000000, 0.000000000000000000, -1.000000000000000000 ) ) ;
#32338 = CARTESIAN_POINT ( 'NONE',  ( 6.499999999999999112, 3.752776749732559036, -6.064240316920397333 ) ) ;
#32339 = CARTESIAN_POINT ( 'NONE',  ( -10.00000000000000000, 15.00000000000000000, -2.701558353794502931 ) ) ;
#32340 = CARTESIAN_POINT ( 'NONE',  ( -104.5387911149144600, -57.64184148030879840, 201.9936694370400971 ) ) ;
#32341 = CARTESIAN_POINT ( 'NONE',  ( -7.188101187500000044, -30.40625000204838813, -8.802885111219163269E-16 ) ) ;
#32342 = CARTESIAN_POINT ( 'NONE',  ( -63.27102371193947761, 47.99999999999999289, 15.76003347376316377 ) ) ;
#32343 = CIRCLE ( 'NONE', #70203, 4.000000000000007105 ) ;
#32344 = CARTESIAN_POINT ( 'NONE',  ( -0.1695571859891748800, 26.07487066857262192, 38.25869140465272267 ) ) ;
#32345 = PLANE ( 'NONE',  #17546 ) ;
#32346 = CARTESIAN_POINT ( 'NONE',  ( -8.554898963428433589, -59.99999999999994316, -44.87740334038038270 ) ) ;
#32347 = DIRECTION ( 'NONE',  ( 1.000000000000000000, 1.224606353822377258E-16, 0.000000000000000000 ) ) ;
#32348 = CARTESIAN_POINT ( 'NONE',  ( -53.46773452942882443, -49.90981900733154220, 61.13492274314185693 ) ) ;
#32349 = DIRECTION ( 'NONE',  ( 0.000000000000000000, -1.000000000000000000, 0.000000000000000000 ) ) ;
#32351 = ORIENTED_EDGE ( 'NONE', *, *, #1542, .F. ) ;
#32350 = AXIS2_PLACEMENT_3D ( 'NONE', #67846, #76998, #85642 ) ;
#32352 = AXIS2_PLACEMENT_3D ( 'NONE', #47932, #22650, #64157 ) ;
#32353 = CARTESIAN_POINT ( 'NONE',  ( -100.6707438451295218, -52.74366064756212324, 193.6868164564221786 ) ) ;
#32354 = STYLED_ITEM ( 'NONE', ( #32676 ), #38990 ) ;
#32355 = CARTESIAN_POINT ( 'NONE',  ( 0.000000000000000000, 0.000000000000000000, 4.000000000000000000 ) ) ;
#32356 = ORIENTED_EDGE ( 'NONE', *, *, #7586, .F. ) ;
#32357 = CARTESIAN_POINT ( 'NONE',  ( -17.73845910361362499, 34.63644398513737599, -22.27319956676174684 ) ) ;
#32358 = CARTESIAN_POINT ( 'NONE',  ( 83.07532134950429281, -38.35702953817527572, -24.43146694555268539 ) ) ;
#32359 = DIRECTION ( 'NONE',  ( -0.000000000000000000, -1.000000000000000000, -0.000000000000000000 ) ) ;
#32360 = DIRECTION ( 'NONE',  ( -1.000000000000000000, -0.000000000000000000, -0.000000000000000000 ) ) ;
#32361 = CARTESIAN_POINT ( 'NONE',  ( -9.966015359215459668, 294.6437633021450893, 1.892774790111525496 ) ) ;
#32362 = CARTESIAN_POINT ( 'NONE',  ( 0.000000000000000000, 0.000000000000000000, -1.175078176076019387 ) ) ;
#32363 = CARTESIAN_POINT ( 'NONE',  ( 82.59595123229216540, -30.00000000000000000, 150.0044142168436849 ) ) ;
#32364 = CARTESIAN_POINT ( 'NONE',  ( 36.52797673977651982, 490.9928046865358624, 12.47113835539106041 ) ) ;
#32365 = CARTESIAN_POINT ( 'NONE',  ( -29.09616027395263416, 9.373446874598341694, 41.96755440745693022 ) ) ;
#32366 = DIRECTION ( 'NONE',  ( -0.000000000000000000, 1.000000000000000000, -0.000000000000000000 ) ) ;
#32367 = CIRCLE ( 'NONE', #70227, 13.00000000000000000 ) ;
#32368 = ORIENTED_EDGE ( 'NONE', *, *, #100828, .F. ) ;
#32369 = VERTEX_POINT ( 'NONE', #8713 ) ;
#32370 = CARTESIAN_POINT ( 'NONE',  ( 49.68469382639499088, -36.05181846547831270, 49.09954005784402398 ) ) ;
#32371 = CARTESIAN_POINT ( 'NONE',  ( -7.188580507048828672, 302.2771598081733941, -10.02656291412436751 ) ) ;
#32372 = LINE ( 'NONE', #66845, #1376 ) ;
#32373 = EDGE_CURVE ( 'NONE', #72949, #105278, #18920, .T. ) ;
#32374 = EDGE_LOOP ( 'NONE', ( #87481, #52563 ) ) ;
#32375 = CARTESIAN_POINT ( 'NONE',  ( -91.04146929460924298, -38.35192349718176530, 1.571303803682228439 ) ) ;
#32376 = VECTOR ( 'NONE', #11904, 1000.000000000000227 ) ;
#32377 = VERTEX_POINT ( 'NONE', #1124 ) ;
#32378 = DIRECTION ( 'NONE',  ( 0.000000000000000000, -1.000000000000000000, 0.000000000000000000 ) ) ;
#32379 = CARTESIAN_POINT ( 'NONE',  ( 90.88251751199774731, -38.35193396244151387, 21.04299878531615775 ) ) ;
#32380 = CARTESIAN_POINT ( 'NONE',  ( 11.66272034348327757, 8.929129883720431593, -9.157998212364818258 ) ) ;
#32381 = CARTESIAN_POINT ( 'NONE',  ( -37.40757794985528761, 25.81202373761992774, -10.96376234217055234 ) ) ;
#32382 = CARTESIAN_POINT ( 'NONE',  ( 103.5574493089503960, -45.28273134603495720, 161.0537541144917384 ) ) ;
#32383 = CARTESIAN_POINT ( 'NONE',  ( -31.67563778497622096, 439.7335944510184049, 23.71446993618755172 ) ) ;
#32384 = FILL_AREA_STYLE ('',( #64728 ) ) ;
#32385 = CARTESIAN_POINT ( 'NONE',  ( -35.53731096081859420, 361.9375032173327327, 2.592946827012501121 ) ) ;
#32386 = CARTESIAN_POINT ( 'NONE',  ( 6.463481858019715531, 7.246446802359423067, -1.128819432756289487 ) ) ;
#32387 = CIRCLE ( 'NONE', #23771, 3.309500000000007880 ) ;
#32388 = CARTESIAN_POINT ( 'NONE',  ( 75.01297031408984139, -59.99999999999999289, 181.3575635546025069 ) ) ;
#32389 = CYLINDRICAL_SURFACE ( 'NONE', #37205, 5.000000000000002665 ) ;
#32390 = ORIENTED_EDGE ( 'NONE', *, *, #3212, .T. ) ;
#32391 = CARTESIAN_POINT ( 'NONE',  ( 54.73609672033058615, -60.31833313769052296, 68.31609071314774440 ) ) ;
#32392 = CARTESIAN_POINT ( 'NONE',  ( -22.09288372273234202, 303.0838735200828182, -9.950444626390048342 ) ) ;
#32393 = DIRECTION ( 'NONE',  ( -3.700743415420800925E-15, 0.000000000000000000, 1.000000000000000000 ) ) ;
#32394 = ORIENTED_EDGE ( 'NONE', *, *, #85026, .F. ) ;
#32396 = CARTESIAN_POINT ( 'NONE',  ( 0.000000000000000000, 0.000000000000000000, 0.000000000000000000 ) ) ;
#32395 = CARTESIAN_POINT ( 'NONE',  ( -79.79561180674197374, -30.00000000001763212, 189.8119606060800209 ) ) ;
#32397 = VECTOR ( 'NONE', #106416, 1000.000000000000000 ) ;
#32398 = CARTESIAN_POINT ( 'NONE',  ( 7.791781413346524410, -2.999999999999999556, -2.093983074874241179 ) ) ;
#32399 = CARTESIAN_POINT ( 'NONE',  ( 24.48998408367273427, 306.7567165393634809, 9.364080809398716454 ) ) ;
#32400 = CARTESIAN_POINT ( 'NONE',  ( -39.97809621673793856, 463.9322724720692577, 18.76396717432225714 ) ) ;
#32401 = CARTESIAN_POINT ( 'NONE',  ( 4.898587196589412829E-16, -33.12499999999999289, -8.000000000000000000 ) ) ;
#32402 = CARTESIAN_POINT ( 'NONE',  ( 0.000000000000000000, -3.000000000000002665, -75.00000000000001421 ) ) ;
#32403 = CIRCLE ( 'NONE', #39248, 8.500000000000000000 ) ;
#32404 = CARTESIAN_POINT ( 'NONE',  ( 58.13370862442641140, 48.00000000000000711, -29.53088244907750237 ) ) ;
#32405 = AXIS2_PLACEMENT_3D ( 'NONE', #54436, #77154, #3270 ) ;
#32406 = ORIENTED_EDGE ( 'NONE', *, *, #41556, .T. ) ;
#32407 = CARTESIAN_POINT ( 'NONE',  ( 84.88381472203214173, -28.91780597334601310, 171.4463788976194394 ) ) ;
#32408 = EDGE_CURVE ( 'NONE', #49420, #5539, #31001, .T. ) ;
#32409 = DIRECTION ( 'NONE',  ( -0.4127509058099244066, 0.1524945595934079634, -0.8979878056229381178 ) ) ;
#32410 = AXIS2_PLACEMENT_3D ( 'NONE', #36817, #45417, #86419 ) ;
#32411 = DIRECTION ( 'NONE',  ( 0.000000000000000000, -1.000000000000000000, 0.000000000000000000 ) ) ;
#32412 = EDGE_LOOP ( 'NONE', ( #74155, #26952, #45541, #10018 ) ) ;
#32413 = LINE ( 'NONE', #74422, #97995 ) ;
#32414 = CARTESIAN_POINT ( 'NONE',  ( 5.318172249950410269, -4.999999999999983125, -15.46996282975494985 ) ) ;
#32415 = CARTESIAN_POINT ( 'NONE',  ( 27.10511071441176867, 34.75829513984540142, -7.556984339686343866 ) ) ;
#32416 = CARTESIAN_POINT ( 'NONE',  ( 14.99580413334056139, 1.250310433696042889, -0.8744943966827515291 ) ) ;
#32417 = DIRECTION ( 'NONE',  ( -1.000000000000000000, -0.000000000000000000, -0.000000000000000000 ) ) ;
#32418 = CYLINDRICAL_SURFACE ( 'NONE', #90476, 1.249999999999999334 ) ;
#32419 = SURFACE_SIDE_STYLE ('',( #106260 ) ) ;
#32420 = CIRCLE ( 'NONE', #6508, 5.000000000000002665 ) ;
#32421 = CIRCLE ( 'NONE', #87538, 3.309500000000001663 ) ;
#32422 = AXIS2_PLACEMENT_3D ( 'NONE', #17597, #49937, #82842 ) ;
#32423 = CARTESIAN_POINT ( 'NONE',  ( 6.928203230275509661, 105.0000000000000000, 4.000000000000001776 ) ) ;
#32424 = CARTESIAN_POINT ( 'NONE',  ( 0.000000000000000000, 0.000000000000000000, 5.000000000000000888 ) ) ;
#32426 = CARTESIAN_POINT ( 'NONE',  ( -12.36035296938143446, 9.759048222428928554, -9.476106837505529512 ) ) ;
#32425 = CARTESIAN_POINT ( 'NONE',  ( -27.41650441252286186, -30.69644322685219606, 39.25280176715715896 ) ) ;
#32427 = EDGE_CURVE ( 'NONE', #31964, #21035, #88458, .T. ) ;
#32428 = CARTESIAN_POINT ( 'NONE',  ( -7.188101187500001821, -11.00000000204838635, -2.977408999572651371 ) ) ;
#32429 = VECTOR ( 'NONE', #52714, 1000.000000000000000 ) ;
#32430 = CARTESIAN_POINT ( 'NONE',  ( -29.49550841906124887, 18.54274624009277161, -39.61427208276962375 ) ) ;
#32431 = AXIS2_PLACEMENT_3D ( 'NONE', #64495, #72045, #97366 ) ;
#32432 = CARTESIAN_POINT ( 'NONE',  ( 0.000000000000000000, 4.898587196589413815E-16, -4.000000000000000888 ) ) ;
#32433 = ORIENTED_EDGE ( 'NONE', *, *, #98877, .T. ) ;
#32434 = CARTESIAN_POINT ( 'NONE',  ( -17.50000000000008171, 49.99999999999968026, 59.91915230424517347 ) ) ;
#32435 = CARTESIAN_POINT ( 'NONE',  ( -46.00000000000000000, 450.0000000000002274, 13.20242257375370976 ) ) ;
#32436 = CARTESIAN_POINT ( 'NONE',  ( -8.972157809039631005, 136.3338258388681652, -2.602085213997499507E-15 ) ) ;
#32437 = CARTESIAN_POINT ( 'NONE',  ( -4.205882352941162416, -4.999999999999998224, -72.69916451482997388 ) ) ;
#32438 = CARTESIAN_POINT ( 'NONE',  ( 2.500000000000013767, -30.00000000000000355, -31.87333685190803223 ) ) ;
#32439 = VERTEX_POINT ( 'NONE', #53943 ) ;
#32440 = CARTESIAN_POINT ( 'NONE',  ( -4.521127550501229386, -85.67610240527663734, 3.944701057164354818 ) ) ;
#32441 = DIRECTION ( 'NONE',  ( -1.000000000000000000, -0.000000000000000000, -0.000000000000000000 ) ) ;
#32442 = ORIENTED_EDGE ( 'NONE', *, *, #94820, .T. ) ;
#32443 = ADVANCED_FACE ( 'NONE', ( #62083 ), #87797, .T. ) ;
#32444 =( NAMED_UNIT ( * ) PLANE_ANGLE_UNIT ( ) SI_UNIT ( $, .RADIAN. ) );
#32445 = ADVANCED_FACE ( 'NONE', ( #86878 ), #30932, .T. ) ;
#32446 = SURFACE_STYLE_FILL_AREA ( #82561 ) ;
#32447 = AXIS2_PLACEMENT_3D ( 'NONE', #96024, #71715, #95482 ) ;
#32448 = CARTESIAN_POINT ( 'NONE',  ( -33.19692928480100846, 40.68433407882878328, -62.00609778940272321 ) ) ;
#32449 = CARTESIAN_POINT ( 'NONE',  ( -100.8702866454455460, -60.00000000000000000, 86.13925423138952908 ) ) ;
#32450 = CARTESIAN_POINT ( 'NONE',  ( 28.46824965450711531, 18.16842165451063451, -40.55076743663480698 ) ) ;
#32451 = CARTESIAN_POINT ( 'NONE',  ( -6.953930663124324063, 304.7325910270068334, -10.02533923955978956 ) ) ;
#32452 = DIRECTION ( 'NONE',  ( 0.000000000000000000, -1.000000000000000000, 0.000000000000000000 ) ) ;
#32453 = CARTESIAN_POINT ( 'NONE',  ( -6.250885388987164504, 3.157894736842104866, 14.66382285868950675 ) ) ;
#32455 = DIRECTION ( 'NONE',  ( -1.000000000000000000, -0.000000000000000000, -0.000000000000000000 ) ) ;
#32454 = CARTESIAN_POINT ( 'NONE',  ( -9.739726766100238464, -5.000000000005447198, -87.61747884500121586 ) ) ;
#32456 = CIRCLE ( 'NONE', #92715, 4.172000000000001485 ) ;
#32457 = CARTESIAN_POINT ( 'NONE',  ( -83.83424416342712959, -39.45725404996229457, 177.1358821851452490 ) ) ;
#32458 = ORIENTED_EDGE ( 'NONE', *, *, #74896, .F. ) ;
#32459 = CARTESIAN_POINT ( 'NONE',  ( 7.500000000000005329, 42.83333333333329307, -71.71180648257555390 ) ) ;
#32460 = EDGE_CURVE ( 'NONE', #37464, #42449, #28133, .T. ) ;
#32461 = ORIENTED_EDGE ( 'NONE', *, *, #66784, .F. ) ;
#32462 = ORIENTED_EDGE ( 'NONE', *, *, #49598, .T. ) ;
#32463 = CARTESIAN_POINT ( 'NONE',  ( 89.64643850830432825, 1.030564683017419500E-14, 0.000000000000000000 ) ) ;
#32464 = EDGE_CURVE ( 'NONE', #86888, #34804, #104092, .T. ) ;
#32465 = CARTESIAN_POINT ( 'NONE',  ( 33.22740183697520422, 464.7219767738044425, 9.606361102772776661 ) ) ;
#32466 = CARTESIAN_POINT ( 'NONE',  ( 41.36650669486618881, -3.851859888774471706E-31, 4.000000000000000888 ) ) ;
#32467 = PRESENTATION_STYLE_ASSIGNMENT (( #14111 ) ) ;
#32468 = CARTESIAN_POINT ( 'NONE',  ( 8.763463954874010753, 19.59837311309268060, -5.000000000000613731 ) ) ;
#32469 = DIRECTION ( 'NONE',  ( -1.000000000000000000, -1.224606353822377258E-16, -0.000000000000000000 ) ) ;
#32470 = CARTESIAN_POINT ( 'NONE',  ( 8.000000000000000000, 9.797174393178825657E-16, -12.97459999999999525 ) ) ;
#32471 = PRESENTATION_LAYER_ASSIGNMENT (  '', '', ( #68655 ) ) ;
#32472 = CARTESIAN_POINT ( 'NONE',  ( 104.9451034742319706, -14.21045842199432663, 145.4709692194043669 ) ) ;
#32473 = CARTESIAN_POINT ( 'NONE',  ( -114.5930292407900879, -59.99999999999997868, 172.8116974628616163 ) ) ;
#32474 = CARTESIAN_POINT ( 'NONE',  ( -61.45978968603484560, -36.01376588712385995, 74.41489827584142347 ) ) ;
#32475 = EDGE_LOOP ( 'NONE', ( #93267, #97753, #80177, #93812 ) ) ;
#32476 = CARTESIAN_POINT ( 'NONE',  ( 50.75636146201753718, 38.95350866439012094, 38.88400008374063077 ) ) ;
#32477 = CARTESIAN_POINT ( 'NONE',  ( 113.8393408857289586, -60.00000000002444978, 184.8621818493575404 ) ) ;
#32478 = ORIENTED_EDGE ( 'NONE', *, *, #21150, .T. ) ;
#32479 = CARTESIAN_POINT ( 'NONE',  ( 1.003931843719813255, -39.47262783694441168, 30.46842126575976906 ) ) ;
#32480 = CARTESIAN_POINT ( 'NONE',  ( -5.082755093536326818, -11.09375000204838457, 5.082755093536325042 ) ) ;
#32481 = AXIS2_PLACEMENT_3D ( 'NONE', #53169, #86620, #102239 ) ;
#32482 = DIRECTION ( 'NONE',  ( 0.1270361284032164306, 0.9918980905719708696, 0.000000000000000000 ) ) ;
#32483 = EDGE_LOOP ( 'NONE', ( #69792, #82200, #67061, #28326, #26911 ) ) ;
#32485 = CARTESIAN_POINT ( 'NONE',  ( 36.16933211627106459, 464.0306822413344889, 19.55183272904454128 ) ) ;
#32484 = CIRCLE ( 'NONE', #63444, 3.309500000000001663 ) ;
#32486 = ORIENTED_EDGE ( 'NONE', *, *, #44781, .F. ) ;
#32487 = DIRECTION ( 'NONE',  ( -0.2277538186085105443, 0.3726643368266331913, 0.8995829534661088367 ) ) ;
#32488 = CARTESIAN_POINT ( 'NONE',  ( -48.02835407290516656, 9.771516447483513446, 16.85535821593516559 ) ) ;
#32489 = CARTESIAN_POINT ( 'NONE',  ( -96.32505468604630039, -59.99999999999997868, 58.36311956787620403 ) ) ;
#32490 = CARTESIAN_POINT ( 'NONE',  ( 9.995943316031024040, -57.99951415928671850, 27.38809334239569182 ) ) ;
#32491 = CARTESIAN_POINT ( 'NONE',  ( -5.082755093536325042, -27.96875000204838457, -5.082755093536325930 ) ) ;
#32492 = CARTESIAN_POINT ( 'NONE',  ( 46.00000000000004263, 463.6789860417705995, 9.766835940523808546 ) ) ;
#32493 = CARTESIAN_POINT ( 'NONE',  ( 81.26467260280679739, 5.000000000000023093, 6.123233995736781074E-16 ) ) ;
#32494 = CARTESIAN_POINT ( 'NONE',  ( -11.46409645960823021, 12.99999999999756994, 10.00000000000000178 ) ) ;
#32495 = DIRECTION ( 'NONE',  ( 0.000000000000000000, -1.000000000000000000, 0.000000000000000000 ) ) ;
#32496 = SURFACE_STYLE_FILL_AREA ( #23879 ) ;
#32497 = SURFACE_SIDE_STYLE ('',( #90711 ) ) ;
#32498 = CARTESIAN_POINT ( 'NONE',  ( -32.64609568143473695, 299.7802937897311040, -0.8989887599977948174 ) ) ;
#32499 = CARTESIAN_POINT ( 'NONE',  ( 94.52956274838354034, -59.99999999999999289, 83.18473151235357932 ) ) ;
#32500 = CARTESIAN_POINT ( 'NONE',  ( -33.05142072533534048, -42.96510174916534197, 35.01105748586546440 ) ) ;
#32501 = DIRECTION ( 'NONE',  ( 1.000000000000000000, 0.000000000000000000, 0.000000000000000000 ) ) ;
#32502 = CARTESIAN_POINT ( 'NONE',  ( 40.91608130519752962, -32.60971946095668983, 37.87311596600657992 ) ) ;
#32504 = COLOUR_RGB ( '', 0.72549020, 0.75294118, 0.79215686) ;
#32503 = FACE_OUTER_BOUND ( 'NONE', #71603, .T. ) ;
#32505 = ORIENTED_EDGE ( 'NONE', *, *, #8473, .F. ) ;
#32506 = CARTESIAN_POINT ( 'NONE',  ( 44.35819766388060259, 435.2221642642162465, 12.65712761108002837 ) ) ;
#32507 = EDGE_CURVE ( 'NONE', #31074, #45473, #104964, .T. ) ;
#32508 = CARTESIAN_POINT ( 'NONE',  ( -78.02821241015172404, -38.57756610151510301, 188.3064634691189099 ) ) ;
#32509 = ORIENTED_EDGE ( 'NONE', *, *, #52348, .T. ) ;
#32511 = CARTESIAN_POINT ( 'NONE',  ( 40.17205142263708240, 310.2804317922712016, -6.358608209523628929 ) ) ;
#32510 = CARTESIAN_POINT ( 'NONE',  ( 2.499999999999997780, -18.83380486180452706, 27.02532357426314036 ) ) ;
#32512 = CARTESIAN_POINT ( 'NONE',  ( -13.40797866535512028, 24.44206711738619475, -2.534967161872643260 ) ) ;
#32513 = CARTESIAN_POINT ( 'NONE',  ( -33.07276483573669168, 438.9325140356086195, 23.89537236861389147 ) ) ;
#32514 = CARTESIAN_POINT ( 'NONE',  ( 6.098403338275567798, 3.412123303362088578, 6.499999999999997335 ) ) ;
#32515 = CARTESIAN_POINT ( 'NONE',  ( 0.8398752165421072835, 43.96108724165920734, -16.57059267381174550 ) ) ;
#32516 = CARTESIAN_POINT ( 'NONE',  ( -38.90208975916836209, 437.7929390082023815, 4.481369775519661758 ) ) ;
#32517 = CARTESIAN_POINT ( 'NONE',  ( 5.383284837158154978, -88.00049343515779299, 2.657356347551699027 ) ) ;
#32518 = CARTESIAN_POINT ( 'NONE',  ( 17.40604945778712676, 45.37707562542234996, 6.412274061844262185 ) ) ;
#32519 = CARTESIAN_POINT ( 'NONE',  ( 99.00645613855532190, -60.00000000000000711, 75.09026749361882480 ) ) ;
#32520 = CARTESIAN_POINT ( 'NONE',  ( 14.58934900096756770, 5.487773041252724582, -6.668063844682254881 ) ) ;
#32521 =( NAMED_UNIT ( * ) SI_UNIT ( $, .STERADIAN. ) SOLID_ANGLE_UNIT ( ) );
#32522 = EDGE_CURVE ( 'NONE', #68449, #59572, #94667, .T. ) ;
#32523 = ORIENTED_EDGE ( 'NONE', *, *, #106268, .T. ) ;
#32524 = EDGE_CURVE ( 'NONE', #86309, #90844, #1605, .T. ) ;
#32525 = TOROIDAL_SURFACE ( 'NONE', #3238, 18.00000000000000355, 4.000000000000000000 ) ;
#32526 = CARTESIAN_POINT ( 'NONE',  ( -87.40951643045639230, -30.00000000000008171, 185.2141721731731820 ) ) ;
#32527 = VERTEX_POINT ( 'NONE', #64707 ) ;
#32528 = DIRECTION ( 'NONE',  ( -1.000000000000000000, 0.000000000000000000, 0.000000000000000000 ) ) ;
#32529 = CARTESIAN_POINT ( 'NONE',  ( -15.43760447746183928, 2.782577468885437000, -1.950845582978123938 ) ) ;
#32530 = CARTESIAN_POINT ( 'NONE',  ( 8.441095186762201052, 28.00979909688160063, 5.000000000003685052 ) ) ;
#32531 = DIRECTION ( 'NONE',  ( -0.000000000000000000, 1.000000000000000000, -0.000000000000000000 ) ) ;
#32532 = CARTESIAN_POINT ( 'NONE',  ( -32.94021323899823983, 485.0599191339510980, 5.361609822537303671 ) ) ;
#32533 = CARTESIAN_POINT ( 'NONE',  ( -2.977408999572650039, -26.56250000204838457, -7.188101187500001821 ) ) ;
#32534 = FACE_OUTER_BOUND ( 'NONE', #24447, .T. ) ;
#32535 = EDGE_LOOP ( 'NONE', ( #75413, #39346, #69543, #5420 ) ) ;
#32536 = AXIS2_PLACEMENT_3D ( 'NONE', #57857, #106409, #15292 ) ;
#32538 = VERTEX_POINT ( 'NONE', #56594 ) ;
#32537 = DIRECTION ( 'NONE',  ( 1.000000000000000000, -0.000000000000000000, -0.000000000000000000 ) ) ;
#32539 = CARTESIAN_POINT ( 'NONE',  ( 80.99391690137066746, -36.02900316038034134, 148.3428981197941425 ) ) ;
#32540 = ADVANCED_FACE ( 'NONE', ( #97061 ), #70620, .T. ) ;
#32541 = FACE_OUTER_BOUND ( 'NONE', #94514, .T. ) ;
#32542 = CARTESIAN_POINT ( 'NONE',  ( 9.165151389911683211, 85.26295510916339992, 3.999999999999999112 ) ) ;
#32543 = VERTEX_POINT ( 'NONE', #89516 ) ;
#32544 = CARTESIAN_POINT ( 'NONE',  ( -47.94005199002864259, 49.99999999999999289, 40.89453192823585681 ) ) ;
#32545 = CARTESIAN_POINT ( 'NONE',  ( -30.00000000000000000, 461.8887775513397855, 11.55279652844097171 ) ) ;
#32546 = CARTESIAN_POINT ( 'NONE',  ( 7.188101187499999156, -13.25000000204838280, 2.977408999572654924 ) ) ;
#32547 = CARTESIAN_POINT ( 'NONE',  ( 7.343637806710344940, 27.55636878099382869, 3.177475076494675310 ) ) ;
#32548 = CARTESIAN_POINT ( 'NONE',  ( -1.286415259407877265, -60.00000000000000711, -36.88577855157840446 ) ) ;
#32549 = CARTESIAN_POINT ( 'NONE',  ( -69.31411742845799040, -57.68241165371757262, 149.3509116208381329 ) ) ;
#32550 = EDGE_CURVE ( 'NONE', #26186, #93546, #105682, .T. ) ;
#32551 = DIRECTION ( 'NONE',  ( -1.000000000000000000, 0.000000000000000000, 0.000000000000000000 ) ) ;
#32552 = VERTEX_POINT ( 'NONE', #87927 ) ;
#32553 = AXIS2_PLACEMENT_3D ( 'NONE', #35196, #85317, #3871 ) ;
#32554 = DIRECTION ( 'NONE',  ( 0.000000000000000000, 0.000000000000000000, 1.000000000000000000 ) ) ;
#32555 = CLOSED_SHELL ( 'NONE', ( #62309, #88998, #21064, #15742, #104999, #4676, #30015, #104447, #98588, #1295, #88531, #12706, #106267, #57703, #39645, #91903, #80423, #57843, #96628, #99403, #98076, #97530, #30461, #97663, #15539, #51928, #29927, #35546, #85040, #32594, #74032, #88671, #73100, #83076, #105223, #103288, #57062, #90519, #66169, #45323, #75332, #71864, #4855, #85045, #11826, #20556, #73504, #57039, #51549, #54879, #80131, #101595, #68029, #104802, #74154, #46863, #52561, #52549, #24334, #28741, #83953, #62276, #97978, #61649, #3463, #43199, #35091, #64461, #30528, #40153, #11396, #52873 ) ) ;
#32556 = CARTESIAN_POINT ( 'NONE',  ( 20.60725157159463805, 18.64284798592509773, -32.43860525503979630 ) ) ;
#32557 = CARTESIAN_POINT ( 'NONE',  ( -0.6250000000000004441, 8.299410119600873159, -7.298562697733108173 ) ) ;
#32558 = ORIENTED_EDGE ( 'NONE', *, *, #5285, .T. ) ;
#32559 = CARTESIAN_POINT ( 'NONE',  ( -7.188101187500002709, -28.81250000204838457, 2.977408999572648707 ) ) ;
#32560 = CARTESIAN_POINT ( 'NONE',  ( 24.52173661427685758, -28.71376923063367315, 38.10928809281097784 ) ) ;
#32561 = CARTESIAN_POINT ( 'NONE',  ( 80.00000000000000000, -60.00000000000000000, -21.09707704303352926 ) ) ;
#32562 = AXIS2_PLACEMENT_3D ( 'NONE', #47653, #80020, #22366 ) ;
#32563 = CARTESIAN_POINT ( 'NONE',  ( 38.54364474655984907, 439.2805328589141709, 23.69816338776510989 ) ) ;
#32565 = EDGE_CURVE ( 'NONE', #49522, #99943, #99634, .T. ) ;
#32564 = APPLICATION_PROTOCOL_DEFINITION ( 'draft international standard', 'automotive_design', 1998, #43806 ) ;
#32566 = CARTESIAN_POINT ( 'NONE',  ( 48.48458519718480630, 8.810627846918919204, 16.77132102101048616 ) ) ;
#32567 = ORIENTED_EDGE ( 'NONE', *, *, #65521, .T. ) ;
#32568 = CARTESIAN_POINT ( 'NONE',  ( -36.31162387720043228, 438.2523736922216244, 3.875403351156469167 ) ) ;
#32570 = CARTESIAN_POINT ( 'NONE',  ( 27.33349330513380337, 4.898587196589405926E-16, -4.000000000000001776 ) ) ;
#32569 =( BOUNDED_SURFACE ( )  B_SPLINE_SURFACE ( 3, 2, ( 
 ( #45433, #37363, #103130 ),
 ( #27688, #4964, #29279 ),
 ( #37895, #10899, #76711 ),
 ( #68653, #11976, #44360 ) ),
 .UNSPECIFIED., .F., .F., .F. ) 
 B_SPLINE_SURFACE_WITH_KNOTS ( ( 4, 4 ),
 ( 3, 3 ),
 ( 3.686287386450715076E-17, 0.002123809863745970954 ),
 ( 0.000000000000000000, 1.000000000000000000 ),
 .UNSPECIFIED. ) 
 GEOMETRIC_REPRESENTATION_ITEM ( )  RATIONAL_B_SPLINE_SURFACE ( (
 ( 1.000000000000000000, 0.8347624811021843172, 1.000000000000000000),
 ( 1.000000000000000000, 0.8202629603801117053, 1.000000000000000000),
 ( 1.000000000000000000, 0.8052718258174581534, 1.000000000000000000),
 ( 1.000000000000000000, 0.7904469216846389257, 1.000000000000000000) ) ) 
 REPRESENTATION_ITEM ( '' )  SURFACE ( )  );
#32571 = CARTESIAN_POINT ( 'NONE',  ( 1.207272737710394672, -21.32703354115300698, -38.55255691456996914 ) ) ;
#32572 = CYLINDRICAL_SURFACE ( 'NONE', #11382, 4.000000000000000000 ) ;
#32573 = FILL_AREA_STYLE_COLOUR ( '', #1483 ) ;
#32574 = ORIENTED_EDGE ( 'NONE', *, *, #74261, .T. ) ;
#32575 = LINE ( 'NONE', #81598, #47897 ) ;
#32576 = CARTESIAN_POINT ( 'NONE',  ( 113.9480634309076379, -57.67139826047481677, 163.7752955952890659 ) ) ;
#32577 = CARTESIAN_POINT ( 'NONE',  ( 36.32791536946660926, 464.0041716472645135, 19.58704090454613223 ) ) ;
#32578 = CARTESIAN_POINT ( 'NONE',  ( 8.595526037062774425E-16, 13.85270131633358304, 7.000000000000011546 ) ) ;
#32579 = PLANE ( 'NONE',  #42632 ) ;
#32580 = DIRECTION ( 'NONE',  ( 0.000000000000000000, -1.000000000000000000, 0.000000000000000000 ) ) ;
#32581 = B_SPLINE_CURVE_WITH_KNOTS ( 'NONE', 3,
 ( #30233, #96551, #29211, #14011, #20601, #13482, #46406, #103055, #62597, #6450, #12952, #22685, #12424, #5923, #88462, #14536, #79292, #94975, #61549, #86359, #47445, #71197, #70150, #80337, #102520, #78234, #28663, #53438, #37821, #45356, #62084, #45872, #78752, #4885, #29721, #7505, #40424, #83014, #39904, #65235, #8048, #97578, #64708, #39386, #15081, #80876, #24275, #8584, #23210, #66295, #56595, #106744, #32893, #49574, #57127, #32363, #64193, #65768, #16145, #90036, #106200, #49032, #25337, #40962, #91126, #31823, #23745, #98127, #58200, #72262, #81929, #56048, #105164, #81394, #98649, #73305, #73850, #88983, #24798, #47966, #82483, #97063, #6985, #72777, #57653, #48501, #105683, #99177, #89518, #15612, #90574, #50107, #16683, #41484, #74374, #451, #31310, #17237, #33421, #984, #18853, #18304, #85140, #59818, #27483, #10701, #19929, #2615, #60360, #84076, #101850, #42544, #26944, #68977, #101331, #50616, #43615, #92695, #75447, #60881, #19398, #84615, #67372, #11233, #58753, #52230, #44158, #77046, #51698, #34507, #33964, #25895, #3162, #1540, #35564, #66835, #76507, #68438, #93235, #67893, #36106, #28011, #9107, #93771, #52772, #74900, #42015, #10176, #43092, #99725, #9636, #35030, #91647, #17760, #75980, #2077, #83533, #100254, #26417, #59282, #92158, #51158, #100781, #46282, #79165, #95897, #103448, #78624, #3707, #5296, #62470, #29599, #45748, #86232, #87278, #46805, #30110, #63002, #104503, #30651, #79697, #22570, #4758, #102384, #11766, #20992, #38215, #12827, #53826, #28537, #37697, #94309, #22022, #71077, #36633, #20471, #53312, #95361, #94847, #12304, #38729, #54878, #87808, #37160, #103968, #70562, #13886, #5805, #71598, #63538, #21498, #54335, #96433, #85689, #86759, #44700, #13355, #77587, #69498, #61417, #45232, #78107, #4225, #70022, #102921, #29089, #61954, #105566, #40834, #31705, #80753, #98007, #73722, #24680, #24159, #89401, #96950, #23085, #90453, #65110, #16565, #6323, #7391, #40304, #88864, #48384, #99052, #57006, #89920, #106084, #56472, #31190, #57531, #16026, #15496, #55921, #73177, #6868, #81276, #39791, #48907, #14953, #8463, #47846, #72665, #39265, #66170, #64593, #32232, #81800, #97463, #88341, #41365, #7927, #47324, #106625, #32775, #49448, #333, #65648, #80220, #55407, #98533, #82357, #23620, #74257, #33300, #14413, #72139, #105049, #64075, #59695, #1957, #91528, #76924, #35440, #60243, #75320, #67775, #100133, #92574, #34910, #93111, #100661, #76381, #67254, #99593, #25218, #26822, #49984, #59161, #42971, #9515, #75862, #34381, #25770, #27364, #74783, #85022, #3035, #18725, #51578, #82891, #84494, #10586, #43502, #83952, #2491, #862, #33840, #68312, #1417, #58073, #58629, #101207, #66713, #35983, #10062, #19284, #90997, #52110, #92043, #18176, #8989, #11106, #44031, #68856, #26299, #17109, #17643, #41894, #51038, #50504, #83416, #42427, #86642, #45112, #11646, #62881, #45634, #70957, #103333, #95772, #46162, #79050, #13766, #46678, #21908, #28411, #62356, #20347, #60765, #93654, #102263, #29480, #94729, #52639, #95246, #61285, #12707, #77991, #54754, #78509, #103849, #4643, #87686, #21379, #79574, #94183, #86109, #20876, #5687, #38612, #53709, #44575, #27898, #37035, #54217, #28964, #69903, #77465, #87157, #102802, #36514, #37574, #53192, #61833, #12180, #13238, #101732, #19802, #70439, #5170, #29995, #4108, #38099, #85571, #3578, #69381, #106492, #56874, #7264, #63423, #81154 ),
 .UNSPECIFIED., .F., .F.,
 ( 4, 1, 1, 1, 1, 1, 1, 1, 1, 1, 2, 2, 1, 1, 1, 1, 1, 1, 2, 2, 1, 1, 1, 1, 1, 1, 2, 2, 1, 1, 1, 1, 1, 1, 1, 1, 2, 2, 1, 1, 1, 1, 1, 1, 2, 2, 1, 1, 1, 1, 1, 1, 1, 1, 2, 2, 1, 1, 1, 1, 1, 1, 1, 1, 2, 2, 1, 1, 1, 1, 1, 1, 1, 1, 1, 2, 2, 1, 1, 1, 1, 1, 1, 1, 1, 2, 2, 1, 1, 1, 1, 1, 1, 1, 2, 2, 1, 1, 1, 2, 2, 1, 1, 1, 1, 1, 1, 1, 1, 2, 2, 1, 1, 1, 2, 2, 1, 1, 1, 1, 1, 2, 2, 1, 1, 2, 2, 1, 1, 1, 1, 2, 2, 1, 1, 1, 1, 1, 2, 2, 1, 1, 1, 1, 1, 2, 2, 1, 1, 1, 2, 2, 1, 1, 1, 1, 1, 2, 2, 1, 1, 1, 1, 1, 1, 2, 2, 1, 1, 1, 1, 1, 1, 1, 1, 2, 2, 1, 1, 1, 1, 1, 1, 1, 1, 1, 1, 2, 2, 1, 1, 1, 1, 1, 1, 1, 1, 1, 1, 2, 2, 1, 1, 1, 1, 1, 1, 1, 1, 1, 1, 2, 2, 1, 1, 1, 1, 1, 1, 1, 1, 2, 2, 1, 1, 1, 1, 1, 1, 1, 1, 2, 2, 1, 1, 1, 1, 1, 1, 1, 1, 1, 1, 2, 2, 1, 1, 1, 1, 1, 1, 1, 1, 1, 2, 2, 1, 1, 1, 1, 1, 1, 1, 2, 2, 1, 1, 1, 1, 1, 1, 1, 2, 2, 1, 1, 1, 1, 1, 1, 2, 2, 1, 1, 1, 1, 1, 1, 1, 2, 2, 1, 1, 1, 1, 1, 1, 2, 2, 1, 1, 1, 1, 1, 1, 2, 2, 1, 1, 1, 1, 1, 1, 1, 1, 2, 2, 1, 1, 1, 1, 1, 1, 1, 2, 2, 1, 1, 1, 1, 1, 2, 2, 1, 1, 1, 1, 1, 1, 1, 1, 2, 2, 4 ),
 ( 0.000000000000000000, 0.03124999999957970426, 0.04687499999936961537, 0.05468749999926453276, 0.05859374999921199145, 0.06054687499918578325, 0.06152343749917271037, 0.06201171874916613230, 0.06225585937416285021, 0.06237792968666124732, 0.06243896484291044241, 0.06249999999915964444, 0.07812499999895176905, 0.08593749999884778279, 0.08984374999879572721, 0.09179687499876966472, 0.09277343749875666123, 0.09326171874875018031, 0.09350585937374693291, 0.09374999999874368550, 0.1093749999985339227, 0.1171874999984289789, 0.1210937499983765070, 0.1230468749983502086, 0.1240234374983369969, 0.1245117187483303772, 0.1247558593733270049, 0.1249999999983236187, 0.1874999999974600873, 0.2187499999970283215, 0.2343749999968123832, 0.2421874999967045528, 0.2460937499966507347, 0.2480468749966238118, 0.2490234374966104891, 0.2495117187466037167, 0.2497558593716003028, 0.2499999999965969166, 0.2656249999963781194, 0.2734374999962687069, 0.2773437499962139174, 0.2792968749961864949, 0.2802734374961726727, 0.2807617187461656783, 0.2810058593711620700, 0.2812499999961584618, 0.2968749999959144348, 0.3046874999957924213, 0.3085937499957315255, 0.3105468749957010499, 0.3115234374956858399, 0.3120117187456782348, 0.3122558593706744046, 0.3123779296831725172, 0.3124389648394215735, 0.3124999999956706298, 0.3203124999955406782, 0.3242187499954757302, 0.3261718749954432561, 0.3271484374954269914, 0.3276367187454188867, 0.3278808593704149454, 0.3280029296829130581, 0.3280639648391620034, 0.3280944824172863927, 0.3281249999954107821, 0.3359374999952490781, 0.3398437499951681984, 0.3417968749951277863, 0.3427734374951075802, 0.3432617187450975327, 0.3435058593700924812, 0.3436279296825899277, 0.3436889648388389840, 0.3437194824169632068, 0.3437347412060256513, 0.3437499999950880403, 0.3515624999950815455, 0.3554687499950783258, 0.3574218749950767715, 0.3583984374950760499, 0.3588867187450754948, 0.3591308593700751062, 0.3592529296825751062, 0.3593139648388249396, 0.3593444824169498841, 0.3593749999950747731, 0.3671874999950420770, 0.3710937499950257568, 0.3730468749950177076, 0.3740234374950136553, 0.3745117187450116569, 0.3747558593700106577, 0.3748779296825102691, 0.3749389648387601026, 0.3749999999950099361, 0.3789062499950078267, 0.3808593749950066609, 0.3811035156200064944, 0.3812255859325062723, 0.3813476562450061058, 0.3818359374950055507, 0.3828124999950045515, 0.3867187499950002216, 0.3886718749949980567, 0.3896484374949969465, 0.3901367187449965024, 0.3903808593699961693, 0.3905029296824958918, 0.3905639648387459473, 0.3906249999949959473, 0.3925781249949994445, 0.3935546874950012763, 0.3940429687450022200, 0.3942871093700026641, 0.3945312499950030527, 0.3964843749950062723, 0.3974609374950079377, 0.3979492187450087148, 0.3981933593700090479, 0.3983154296825091589, 0.3983764648387592144, 0.3984374999950092699, 0.4003906249950098251, 0.4013671874950099916, 0.4018554687450100471, 0.4023437499950101026, 0.4042968749950097695, 0.4052734374950096585, 0.4057617187450095475, 0.4060058593700094365, 0.4061279296825093255, 0.4062499999950091589, 0.4082031249950073826, 0.4091796874950064944, 0.4096679687450061058, 0.4099121093700058838, 0.4100341796825057727, 0.4100952148387557172, 0.4101562499950057172, 0.4121093749950055507, 0.4130859374950055507, 0.4135742187450055507, 0.4138183593700054397, 0.4139404296825054397, 0.4140014648387554397, 0.4140624999950054397, 0.4150390624950059393, 0.4155273437450061058, 0.4157714843700061058, 0.4158935546825060503, 0.4160156249950059393, 0.4169921874950046625, 0.4174804687450040519, 0.4177246093700036633, 0.4178466796825034413, 0.4179077148387534968, 0.4179382324168784413, 0.4179687499950034413, 0.4199218749950064944, 0.4208984374950079932, 0.4213867187450087703, 0.4216308593700091589, 0.4217529296825094365, 0.4218139648387596585, 0.4218444824168848251, 0.4218749999950099361, 0.4296874999950471286, 0.4335937499950655583, 0.4355468749950748841, 0.4365234374950796026, 0.4370117187450819896, 0.4372558593700832108, 0.4373779296825838769, 0.4374389648388341545, 0.4374694824169592100, 0.4374999999950843210, 0.4687499999954365948, 0.4843749999956128982, 0.4921874999957009944, 0.4960937499957450147, 0.4980468749957669417, 0.4990234374957779329, 0.4995117187457834840, 0.4997558593707862595, 0.4998779296832877028, 0.4999389648395383690, 0.4999694824176637575, 0.4999999999957892571, 0.5312499999960962338, 0.5468749999962496666, 0.5546874999963264941, 0.5585937499963649078, 0.5605468749963840036, 0.5615234374963936625, 0.5620117187463983255, 0.5622558593714006570, 0.5623779296839017672, 0.5624389648401522113, 0.5624694824182773223, 0.5624999999964025443, 0.5937499999967007502, 0.6093749999968498532, 0.6171874999969244602, 0.6210937499969616526, 0.6230468749969803044, 0.6240234374969896303, 0.6245117187469941822, 0.6247558593719966247, 0.6248779296844978459, 0.6249389648407485121, 0.6249694824188737341, 0.6249999999969989561, 0.6406249999970944353, 0.6484374999971422859, 0.6523437499971662668, 0.6542968749971781461, 0.6552734374971841413, 0.6557617187471871389, 0.6560058593721885822, 0.6561279296846893594, 0.6561889648409398035, 0.6562499999971902476, 0.6718749999972619680, 0.6796874999972977172, 0.6835937499973157028, 0.6855468749973245846, 0.6865234374973291365, 0.6870117187473313569, 0.6872558593723324671, 0.6873779296848331333, 0.6874389648410834663, 0.6874999999973339104, 0.7187499999975396348, 0.7343749999976424414, 0.7421874999976939558, 0.7460937499977197129, 0.7480468749977324805, 0.7490234374977389198, 0.7495117187477421394, 0.7497558593727436937, 0.7498779296852444709, 0.7499389648414949150, 0.7499694824196200260, 0.7499999999977451370, 0.7812499999980321297, 0.7968749999981755705, 0.8046874999982472909, 0.8085937499982830401, 0.8105468749983010257, 0.8115234374983099075, 0.8120117187483144594, 0.8122558593733167909, 0.8123779296858179011, 0.8124389648420684562, 0.8124999999983189003, 0.8281249999984525711, 0.8359374999985194066, 0.8398437499985528243, 0.8417968749985694776, 0.8427734374985778043, 0.8432617187485820232, 0.8435058593735840216, 0.8436279296860850208, 0.8437499999985860200, 0.8593749999987186916, 0.8671874999987848609, 0.8710937499988180566, 0.8730468749988345989, 0.8740234374988429256, 0.8745117187488470334, 0.8747558593738490318, 0.8748779296863501420, 0.8749999999988511412, 0.8906249999989839239, 0.8984374999990503152, 0.9023437499990835109, 0.9042968749991001642, 0.9052734374991083799, 0.9057617187491125987, 0.9060058593741147082, 0.9062499999991167066, 0.9140624999991834310, 0.9179687499992166266, 0.9199218749992333910, 0.9208984374992417177, 0.9213867187492458255, 0.9216308593742479349, 0.9217529296867489341, 0.9218139648429994892, 0.9218749999992499333, 0.9257812499992839061, 0.9277343749993007815, 0.9287109374993093303, 0.9291992187493135491, 0.9294433593743156585, 0.9295654296868167688, 0.9296264648430672128, 0.9296874999993177680, 0.9335937499993516298, 0.9355468749993685051, 0.9365234374993769428, 0.9370117187493811617, 0.9372558593743832711, 0.9373779296868842703, 0.9374389648431348254, 0.9374999999993852695, 0.9453124999994531041, 0.9492187499994869659, 0.9511718749995038413, 0.9521484374995123900, 0.9526367187495166089, 0.9528808593745187183, 0.9530029296870197175, 0.9530639648432702726, 0.9530944824213954947, 0.9531249999995208277, 0.9570312499995546895, 0.9589843749995717870, 0.9599609374995802247, 0.9604492187495844435, 0.9606933593745866640, 0.9608154296870876632, 0.9608764648433382183, 0.9609069824214634403, 0.9609374999995886624, 0.9648437499996247446, 0.9667968749996427302, 0.9677734374996518341, 0.9682617187496563860, 0.9685058593746586064, 0.9686279296871597166, 0.9687499999996609379, 0.9765624999997345457, 0.9804687499997714051, 0.9824218749997898348, 0.9833984374997990496, 0.9838867187498037126, 0.9841308593748060440, 0.9842529296873072653, 0.9843139648435577094, 0.9843444824216830424, 0.9843749999998082645, 1.000000000000000000 ),
 .UNSPECIFIED. ) ;
#32582 = CARTESIAN_POINT ( 'NONE',  ( -73.90092748813849255, -60.00000000000000000, 171.2155407444064110 ) ) ;
#32583 = AXIS2_PLACEMENT_3D ( 'NONE', #7038, #39954, #72827 ) ;
#32584 = FACE_OUTER_BOUND ( 'NONE', #24058, .T. ) ;
#32585 = SURFACE_STYLE_FILL_AREA ( #82155 ) ;
#32586 = CARTESIAN_POINT ( 'NONE',  ( -61.09659575455685143, 50.00000000000000000, -16.41787579824995902 ) ) ;
#32587 = B_SPLINE_CURVE_WITH_KNOTS ( 'NONE', 3,
 ( #8197, #41107, #42160, #106348 ),
 .UNSPECIFIED., .F., .F.,
 ( 4, 4 ),
 ( 0.000000000000000000, 1.000000000000000000 ),
 .UNSPECIFIED. ) ;
#32588 = CARTESIAN_POINT ( 'NONE',  ( -85.28664353795764441, -42.93378835376115887, 186.5457363852486310 ) ) ;
#32589 = VERTEX_POINT ( 'NONE', #6984 ) ;
#32590 = CARTESIAN_POINT ( 'NONE',  ( 26.59004530782534559, 307.2471289293887367, -8.468265503451595677 ) ) ;
#32591 = EDGE_CURVE ( 'NONE', #89804, #37408, #84162, .T. ) ;
#32592 = ORIENTED_EDGE ( 'NONE', *, *, #59032, .F. ) ;
#32593 = DIRECTION ( 'NONE',  ( -1.000000000000000000, -1.224606353822377258E-16, -0.000000000000000000 ) ) ;
#32594 = ADVANCED_FACE ( 'NONE', ( #72261 ), #15611, .F. ) ;
#32595 = DIRECTION ( 'NONE',  ( 0.000000000000000000, 0.000000000000000000, 1.000000000000000000 ) ) ;
#32596 = CARTESIAN_POINT ( 'NONE',  ( -84.46960190694564119, -45.27041167832899760, -5.142523808328494539 ) ) ;
#32597 = STYLED_ITEM ( 'NONE', ( #4183 ), #45279 ) ;
#32598 = CARTESIAN_POINT ( 'NONE',  ( -42.48722704179489540, 465.9004001135029398, 13.75636562493584414 ) ) ;
#32599 = FACE_OUTER_BOUND ( 'NONE', #51475, .T. ) ;
#32600 = ORIENTED_EDGE ( 'NONE', *, *, #87728, .T. ) ;
#32601 = EDGE_CURVE ( 'NONE', #21098, #89053, #34230, .T. ) ;
#32602 = CARTESIAN_POINT ( 'NONE',  ( 13.44467335266196528, 24.50761115066882212, -2.221713994527983793 ) ) ;
#32603 = CARTESIAN_POINT ( 'NONE',  ( 11.19959342722337681, 2.897043466792154898E-12, -19.43146043914873289 ) ) ;
#32604 = CIRCLE ( 'NONE', #80763, 5.000000000000002665 ) ;
#32605 = CARTESIAN_POINT ( 'NONE',  ( -35.31443409317565596, 437.2805527638894318, 5.244185069633918950 ) ) ;
#32606 = CARTESIAN_POINT ( 'NONE',  ( 33.15797435408901350, -29.99999999999994671, -37.92174772678599481 ) ) ;
#32607 = CARTESIAN_POINT ( 'NONE',  ( -78.84973396984698013, -32.55776669678326130, 132.6303212860630367 ) ) ;
#32608 = ORIENTED_EDGE ( 'NONE', *, *, #39839, .F. ) ;
#32609 = CARTESIAN_POINT ( 'NONE',  ( 55.31236231582965956, -60.00000000000003553, 93.46951393418744658 ) ) ;
#32610 = DIRECTION ( 'NONE',  ( 0.000000000000000000, -1.000000000000000000, 0.000000000000000000 ) ) ;
#32611 = CARTESIAN_POINT ( 'NONE',  ( 94.10923974253748270, -57.67266607662146782, 21.51150559826979602 ) ) ;
#32612 = EDGE_LOOP ( 'NONE', ( #86539, #85793, #105193, #92507 ) ) ;
#32613 = CARTESIAN_POINT ( 'NONE',  ( 27.86692020406142589, 34.24704128939396952, 9.812054281695964164 ) ) ;
#32614 = VECTOR ( 'NONE', #76349, 1000.000000000000000 ) ;
#32615 = FACE_OUTER_BOUND ( 'NONE', #41761, .T. ) ;
#32616 = VERTEX_POINT ( 'NONE', #30775 ) ;
#32617 = LINE ( 'NONE', #62207, #90644 ) ;
#32618 = CYLINDRICAL_SURFACE ( 'NONE', #35907, 4.000000000000000888 ) ;
#32619 = FACE_OUTER_BOUND ( 'NONE', #92007, .T. ) ;
#32620 = CARTESIAN_POINT ( 'NONE',  ( 7.188101187500001821, -17.56250000204838457, -2.977408999572650483 ) ) ;
#32621 = CARTESIAN_POINT ( 'NONE',  ( 44.19630675230467887, 485.6206890027685859, 3.558858865136342864 ) ) ;
#32622 = CARTESIAN_POINT ( 'NONE',  ( 9.165151389911679658, 85.00000000000000000, 4.000000000000000000 ) ) ;
#32623 = CARTESIAN_POINT ( 'NONE',  ( -12.13034742782427955, 48.00000000000000000, -93.82352941176471006 ) ) ;
#32624 = CARTESIAN_POINT ( 'NONE',  ( -17.25516560787559683, 45.65538004793684479, -4.306155947794052530 ) ) ;
#32625 = CARTESIAN_POINT ( 'NONE',  ( 42.68684796707852769, 436.2654864220232867, 7.155924889999337957 ) ) ;
#32626 = AXIS2_PLACEMENT_3D ( 'NONE', #26206, #42869, #99497 ) ;
#32627 = ORIENTED_EDGE ( 'NONE', *, *, #10077, .T. ) ;
#32628 = CARTESIAN_POINT ( 'NONE',  ( -7.493977375961165421, 40.56334907134074541, -69.29067413203748060 ) ) ;
#32630 = CARTESIAN_POINT ( 'NONE',  ( 29.54011214367963589, -22.11874979585171275, 29.86351015682103238 ) ) ;
#32629 = CARTESIAN_POINT ( 'NONE',  ( -20.75616973061526949, -30.00000000000004263, 37.60198765588109637 ) ) ;
#32631 = CARTESIAN_POINT ( 'NONE',  ( 24.76885996170685544, 306.0690732980165194, -8.735186880116588171 ) ) ;
#32632 = ORIENTED_EDGE ( 'NONE', *, *, #55946, .T. ) ;
#32633 = EDGE_CURVE ( 'NONE', #20907, #82359, #8047, .T. ) ;
#32634 = CIRCLE ( 'NONE', #68809, 4.000000000000007105 ) ;
#32635 = ORIENTED_EDGE ( 'NONE', *, *, #82466, .F. ) ;
#32637 = CARTESIAN_POINT ( 'NONE',  ( 1.103059070678794606, 51.47956408706726705, 9.609521617059924026 ) ) ;
#32636 = LINE ( 'NONE', #67105, #7198 ) ;
#32638 = CARTESIAN_POINT ( 'NONE',  ( -20.21880305278369150, 304.8280059657581660, -9.005058168222323189 ) ) ;
#32639 = CARTESIAN_POINT ( 'NONE',  ( 38.54515645702225868, 1.482358050883964840E-15, 0.000000000000000000 ) ) ;
#32640 = CARTESIAN_POINT ( 'NONE',  ( 7.048357505843847903, 41.75164249415616524, -68.91429206277067010 ) ) ;
#32641 = B_SPLINE_CURVE_WITH_KNOTS ( 'NONE', 3,
 ( #43282, #102041, #92889, #51891, #84807, #1742 ),
 .UNSPECIFIED., .F., .F.,
 ( 4, 2, 4 ),
 ( 0.000000000000000000, 0.002016319290324576803, 0.004032638580649153606 ),
 .UNSPECIFIED. ) ;
#32642 = CARTESIAN_POINT ( 'NONE',  ( 0.5675612687379431032, 46.16185839072779373, 16.38316274734319222 ) ) ;
#32643 = CARTESIAN_POINT ( 'NONE',  ( -36.20419914068695988, 464.0241112302327906, 19.56059989341670757 ) ) ;
#32644 = EDGE_LOOP ( 'NONE', ( #13220, #31984, #10219, #67468, #65262, #27969 ) ) ;
#32645 = EDGE_CURVE ( 'NONE', #34061, #2886, #61790, .T. ) ;
#32646 = CARTESIAN_POINT ( 'NONE',  ( 33.25680808871401695, -60.00000000000000000, -40.52559416211042276 ) ) ;
#32647 = CARTESIAN_POINT ( 'NONE',  ( -9.058657501722457539, 46.09928351899775123, 13.86902144048102059 ) ) ;
#32648 = CARTESIAN_POINT ( 'NONE',  ( 30.00000000000000355, 461.8802764867031669, 14.89328939272364316 ) ) ;
#32649 = DIRECTION ( 'NONE',  ( -1.000000000000000000, -1.224606353822377258E-16, -0.000000000000000000 ) ) ;
#32650 = CARTESIAN_POINT ( 'NONE',  ( 46.79755470960057551, 13.68519846643611260, -15.37381431200700810 ) ) ;
#32651 = EDGE_CURVE ( 'NONE', #82907, #99696, #94506, .T. ) ;
#32652 = ORIENTED_EDGE ( 'NONE', *, *, #14637, .F. ) ;
#32653 = CARTESIAN_POINT ( 'NONE',  ( -4.250000000000000000, 5.204748896376250699E-16, -2.342872917771300578 ) ) ;
#32654 = ORIENTED_EDGE ( 'NONE', *, *, #52312, .T. ) ;
#32655 = ORIENTED_EDGE ( 'NONE', *, *, #26221, .T. ) ;
#32656 = CARTESIAN_POINT ( 'NONE',  ( 20.34579289372440059, 303.8361034413807147, -9.003336996645794343 ) ) ;
#32657 =( LENGTH_UNIT ( ) NAMED_UNIT ( * ) SI_UNIT ( .MILLI., .METRE. ) );
#32658 = CARTESIAN_POINT ( 'NONE',  ( -27.10511071441183262, -1.200000000000000030E-05, 7.556984339686156460 ) ) ;
#32659 = DIRECTION ( 'NONE',  ( 0.000000000000000000, 0.000000000000000000, 1.000000000000000000 ) ) ;
#32660 = CARTESIAN_POINT ( 'NONE',  ( -44.11907783817835593, 333.2661371888331701, -0.6867057639839724281 ) ) ;
#32661 = CARTESIAN_POINT ( 'NONE',  ( -5.045023136152173571, -61.23904260837603175, 13.88549718443812964 ) ) ;
#32663 = FACE_OUTER_BOUND ( 'NONE', #48023, .T. ) ;
#32662 = AXIS2_PLACEMENT_3D ( 'NONE', #37617, #70480, #103375 ) ;
#32664 = PRESENTATION_STYLE_ASSIGNMENT (( #26184 ) ) ;
#32665 = VERTEX_POINT ( 'NONE', #40423 ) ;
#32666 = FACE_OUTER_BOUND ( 'NONE', #29763, .T. ) ;
#32667 = ORIENTED_EDGE ( 'NONE', *, *, #13119, .T. ) ;
#32668 = CARTESIAN_POINT ( 'NONE',  ( 9.647540759884607908, 51.27675344764688958, -3.402203074467008648 ) ) ;
#32669 = CARTESIAN_POINT ( 'NONE',  ( 9.250997389131581983, 1.340359594676612611E-15, 0.000000000000000000 ) ) ;
#32670 = CARTESIAN_POINT ( 'NONE',  ( 3.454253436624922013, -49.15858197120396511, 103.7259032015043090 ) ) ;
#32671 = AXIS2_PLACEMENT_3D ( 'NONE', #64782, #88006, #38926 ) ;
#32672 = CONICAL_SURFACE ( 'NONE', #42959, 3.309500000000001663, 0.9599310885968770357 ) ;
#32673 = FACE_BOUND ( 'NONE', #31072, .T. ) ;
#32674 = CARTESIAN_POINT ( 'NONE',  ( 68.29127775091039609, -42.95892816396526825, 98.34793835544786589 ) ) ;
#32675 = ORIENTED_EDGE ( 'NONE', *, *, #77849, .F. ) ;
#32676 = PRESENTATION_STYLE_ASSIGNMENT (( #17540 ) ) ;
#32677 = CARTESIAN_POINT ( 'NONE',  ( -6.481161585458341534, 9.994713615451841449, 2.652050489361055696 ) ) ;
#32678 = ADVANCED_FACE ( 'NONE', ( #57125 ), #73303, .T. ) ;
#32679 = ORIENTED_EDGE ( 'NONE', *, *, #96676, .T. ) ;
#32680 = AXIS2_PLACEMENT_3D ( 'NONE', #70396, #11601, #52596 ) ;
#32681 = SHAPE_REPRESENTATION_RELATIONSHIP ( 'NONE' , 'NONE' ,  #49395, #29376 ) ;
#32682 = AXIS2_PLACEMENT_3D ( 'NONE', #10105, #2001, #43016 ) ;
#32683 = CIRCLE ( 'NONE', #3328, 8.857142857142855874 ) ;
#32684 = CARTESIAN_POINT ( 'NONE',  ( -35.96015918321902660, 491.7728760210378596, 12.54260821243620505 ) ) ;
#32685 = CARTESIAN_POINT ( 'NONE',  ( 103.5111111111111057, 1.023464760207051730E-14, 0.000000000000000000 ) ) ;
#32686 = CARTESIAN_POINT ( 'NONE',  ( 7.999999999999998224, -23.28125000409677270, 3.313708498984766493 ) ) ;
#32687 = ADVANCED_FACE ( 'NONE', ( #22146 ), #10327, .T. ) ;
#32688 = PRESENTATION_STYLE_ASSIGNMENT (( #38648 ) ) ;
#32689 = CARTESIAN_POINT ( 'NONE',  ( 33.00540147335428287, 487.4196752801332195, 9.523982417622292473 ) ) ;
#32690 = SURFACE_STYLE_FILL_AREA ( #96869 ) ;
#32691 = CARTESIAN_POINT ( 'NONE',  ( -5.939670878927854503, 4.581516962870602505, 5.000000000000000888 ) ) ;
#32692 = CARTESIAN_POINT ( 'NONE',  ( 7.343637806710343163, -7.556368780993834910, 3.177475076494673978 ) ) ;
#32693 =( NAMED_UNIT ( * ) SI_UNIT ( $, .STERADIAN. ) SOLID_ANGLE_UNIT ( ) );
#32694 = CARTESIAN_POINT ( 'NONE',  ( -0.7408669144225156211, 15.11700796859873108, -9.999999999997889688 ) ) ;
#32695 = ORIENTED_EDGE ( 'NONE', *, *, #43376, .F. ) ;
#32696 = DIRECTION ( 'NONE',  ( 0.000000000000000000, 0.000000000000000000, -1.000000000000000000 ) ) ;
#32697 = DIRECTION ( 'NONE',  ( 0.000000000000000000, 1.000000000000000000, 0.000000000000000000 ) ) ;
#32698 = CARTESIAN_POINT ( 'NONE',  ( -98.12681787409746903, -29.99999999999999645, 190.3891223338559655 ) ) ;
#32699 = CIRCLE ( 'NONE', #32779, 5.000000000000002665 ) ;
#32700 = CARTESIAN_POINT ( 'NONE',  ( -40.42062918464028343, 485.1352466658498770, -4.233530644584298841 ) ) ;
#32701 = CARTESIAN_POINT ( 'NONE',  ( 63.30621635515526435, -57.67870488568929233, 119.7030265864528076 ) ) ;
#32703 = CARTESIAN_POINT ( 'NONE',  ( -6.486091964843609503, 4.943792391109567141, 4.959578321183684579 ) ) ;
#32702 = LINE ( 'NONE', #65571, #70777 ) ;
#32705 = CARTESIAN_POINT ( 'NONE',  ( 10.26328300195640963, -22.68956793900527913, -38.54249056527262951 ) ) ;
#32704 = CIRCLE ( 'NONE', #92965, 5.000000000000001776 ) ;
#32706 = CARTESIAN_POINT ( 'NONE',  ( -7.500000000000000888, 0.000000000000000000, 1.734723475976807094E-15 ) ) ;
#32707 = SURFACE_SIDE_STYLE ('',( #48312 ) ) ;
#32708 = CARTESIAN_POINT ( 'NONE',  ( -3.925451770789095463, -60.00000000000000711, 39.63159641071881367 ) ) ;
#32709 = CARTESIAN_POINT ( 'NONE',  ( -0.9330442100819067441, -70.05675763226155084, 13.03100537459362407 ) ) ;
#32710 = CIRCLE ( 'NONE', #65412, 5.000000000000001776 ) ;
#32711 = LINE ( 'NONE', #97943, #106137 ) ;
#32712 = CARTESIAN_POINT ( 'NONE',  ( -87.13321523403938329, -42.76517114182743029, 190.1424499742896330 ) ) ;
#32713 = EDGE_LOOP ( 'NONE', ( #53728, #28940, #42944, #66601 ) ) ;
#32714 = CARTESIAN_POINT ( 'NONE',  ( 17.50000000000001066, 51.54267222162374651, 62.45775632500005514 ) ) ;
#32715 = DIRECTION ( 'NONE',  ( 0.000000000000000000, 0.5000000000000013323, 0.8660254037844378194 ) ) ;
#32716 = CARTESIAN_POINT ( 'NONE',  ( -8.140123003886579056, -35.99444279251709844, 29.88182697456086601 ) ) ;
#32718 = CARTESIAN_POINT ( 'NONE',  ( 2.914316916059087603, -69.03253091208547687, 13.00441016735022437 ) ) ;
#32717 = CARTESIAN_POINT ( 'NONE',  ( -0.04050535873994216135, -7.919512791578273259, -6.573129608219107745 ) ) ;
#32719 = EDGE_CURVE ( 'NONE', #57174, #68586, #20312, .T. ) ;
#32720 = VERTEX_POINT ( 'NONE', #31308 ) ;
#32721 = CARTESIAN_POINT ( 'NONE',  ( 27.10511071441197117, 34.47735702144345282, 10.05698433968570704 ) ) ;
#32722 = CARTESIAN_POINT ( 'NONE',  ( -7.468840097763780328, -3.123202671101336314, -19.53083092318177805 ) ) ;
#32723 = CARTESIAN_POINT ( 'NONE',  ( -7.934914944860276265, 33.86845647200111387, -1.051261972695689106 ) ) ;
#32724 = AXIS2_PLACEMENT_3D ( 'NONE', #7835, #40213, #48293 ) ;
#32725 = CARTESIAN_POINT ( 'NONE',  ( 34.89096242599858044, 301.3136321141124085, -8.544899998089542592 ) ) ;
#32726 = ADVANCED_FACE ( 'NONE', ( #106743 ), #25989, .F. ) ;
#32727 = CARTESIAN_POINT ( 'NONE',  ( 51.01037695545453232, 500.0000000000002274, 5.000000000000001776 ) ) ;
#32729 = CARTESIAN_POINT ( 'NONE',  ( -7.619753052866895970, -81.82548497192826176, -2.447276542590447246 ) ) ;
#32728 = B_SPLINE_CURVE_WITH_KNOTS ( 'NONE', 3,
 ( #106266, #97129, #32430, #97646, #6517, #22750, #56113, #16209, #55588, #14601, #89584, #5990, #30846, #41025, #49092, #48035, #15150, #32958, #98706, #65827, #38916, #71783, #72329, #31889, #96615, #80942, #89049, #47513, #80404, #39452 ),
 .UNSPECIFIED., .F., .F.,
 ( 4, 2, 2, 2, 2, 2, 2, 2, 2, 2, 2, 2, 2, 2, 4 ),
 ( 0.006732386592399363864, 0.007201418480221516427, 0.007435934424132591841, 0.007670450368043668123, 0.007904966311954744404, 0.008139482255865821553, 0.008373998199776896967, 0.008608514143687972381, 0.009077546031510112801, 0.009546577919332253220, 0.01048464169497652365, 0.01142270547062079582, 0.01236076924626506798, 0.01329883302190933841, 0.01423689679755360885 ),
 .UNSPECIFIED. ) ;
#32730 = DIRECTION ( 'NONE',  ( -6.104959157215355576E-15, -0.3964176948853179727, -0.9180702648391412257 ) ) ;
#32731 = CARTESIAN_POINT ( 'NONE',  ( 112.5893299866519897, -60.00000000000007105, 145.0945492492805045 ) ) ;
#32732 = LINE ( 'NONE', #97962, #87153 ) ;
#32733 = ORIENTED_EDGE ( 'NONE', *, *, #23728, .F. ) ;
#32734 = CARTESIAN_POINT ( 'NONE',  ( -3.323053273850956835, -29.99999999999999289, 6.657831141027028110 ) ) ;
#32735 = CARTESIAN_POINT ( 'NONE',  ( -9.797936955406333581, 253.4667168977047709, -2.012343231877574468 ) ) ;
#32736 = CARTESIAN_POINT ( 'NONE',  ( 102.6464385083043283, 5.000000000000020428, 0.000000000000000000 ) ) ;
#32737 = CARTESIAN_POINT ( 'NONE',  ( -1.843253007570911225E-16, -9.147862274876562338, -8.047472243342939535 ) ) ;
#32738 = CARTESIAN_POINT ( 'NONE',  ( 37.70204294583037807, 409.1425458642764852, 6.512462526010587283 ) ) ;
#32739 = CARTESIAN_POINT ( 'NONE',  ( 43.36987996225059305, 463.6266071988662247, 5.362859980318074982 ) ) ;
#32740 = EDGE_LOOP ( 'NONE', ( #36755, #89387, #85169, #98596, #11772, #22987 ) ) ;
#32741 = CARTESIAN_POINT ( 'NONE',  ( -23.40846030801418820, 305.8699098592260270, 9.159741819081197889 ) ) ;
#32742 = ORIENTED_EDGE ( 'NONE', *, *, #6380, .T. ) ;
#32743 = CARTESIAN_POINT ( 'NONE',  ( 37.69644952591121978, 484.8922498457696406, -3.621330182635625228 ) ) ;
#32744 =( LENGTH_UNIT ( ) NAMED_UNIT ( * ) SI_UNIT ( .MILLI., .METRE. ) );
#32745 = CARTESIAN_POINT ( 'NONE',  ( 9.443351513663944985, 46.21199249391290920, 13.23092383815001760 ) ) ;
#32746 = ORIENTED_EDGE ( 'NONE', *, *, #91786, .T. ) ;
#32747 = EDGE_CURVE ( 'NONE', #102845, #38992, #26943, .T. ) ;
#32748 =( LENGTH_UNIT ( ) NAMED_UNIT ( * ) SI_UNIT ( .MILLI., .METRE. ) );
#32749 = CARTESIAN_POINT ( 'NONE',  ( 4.999999999999843681, -12.25926108426882166, 9.485372419963775670 ) ) ;
#32750 = CARTESIAN_POINT ( 'NONE',  ( -15.38582294317437338, -60.00000000000488853, 42.16893985326622385 ) ) ;
#32751 = DIRECTION ( 'NONE',  ( 0.000000000000000000, 1.000000000000000000, 0.000000000000000000 ) ) ;
#32752 = CARTESIAN_POINT ( 'NONE',  ( 92.13933835806670913, -59.99999999999998579, 21.62654867099170275 ) ) ;
#32754 = CARTESIAN_POINT ( 'NONE',  ( 15.60252081763109544, -35.99201029456901324, 30.06430533318423670 ) ) ;
#32753 = CARTESIAN_POINT ( 'NONE',  ( -112.2649012439172793, -59.99999999999995026, 191.8495178741738130 ) ) ;
#32755 = UNCERTAINTY_MEASURE_WITH_UNIT (LENGTH_MEASURE( 1.000000000000000082E-05 ), #55581, 'distance_accuracy_value', 'NONE');
#32756 = CARTESIAN_POINT ( 'NONE',  ( 0.08494585571554005843, 54.30758622938873259, -7.750000000000002665 ) ) ;
#32757 = AXIS2_PLACEMENT_3D ( 'NONE', #2014, #81857, #7980 ) ;
#32758 = CARTESIAN_POINT ( 'NONE',  ( -47.76393914926944717, -25.68763306169221394, 43.13152166428435663 ) ) ;
#32759 = ADVANCED_FACE ( 'NONE', ( #59817 ), #37008, .T. ) ;
#32760 = CARTESIAN_POINT ( 'NONE',  ( 19.83463548332445825, 303.8035096162420245, 9.926734387303332241 ) ) ;
#32761 = ORIENTED_EDGE ( 'NONE', *, *, #46459, .T. ) ;
#32762 = CARTESIAN_POINT ( 'NONE',  ( -52.56483885390523625, 48.00000000000000000, -38.23529411764706509 ) ) ;
#32763 = CARTESIAN_POINT ( 'NONE',  ( 1.224646799147353651E-15, 0.000000000000000000, 10.00000000000000355 ) ) ;
#32764 = CARTESIAN_POINT ( 'NONE',  ( 31.02212611900126760, 360.5725590293961318, 22.12937154125974715 ) ) ;
#32765 = CARTESIAN_POINT ( 'NONE',  ( 2.500000000000002220, -8.000000000000000000, -17.89626171146327138 ) ) ;
#32766 = DIRECTION ( 'NONE',  ( 0.000000000000000000, 1.000000000000000000, 0.000000000000000000 ) ) ;
#32767 = CARTESIAN_POINT ( 'NONE',  ( 30.87955015324946828, 351.7733141111877444, 20.67482462247657082 ) ) ;
#32768 = EDGE_LOOP ( 'NONE', ( #101724, #49105, #13200, #93683 ) ) ;
#32769 = DIRECTION ( 'NONE',  ( -1.000000000000000000, 0.000000000000000000, 0.000000000000000000 ) ) ;
#32770 = VERTEX_POINT ( 'NONE', #55920 ) ;
#32771 = CARTESIAN_POINT ( 'NONE',  ( 73.12653570793921176, -29.99999999999997868, 143.9247086217570768 ) ) ;
#32772 = CARTESIAN_POINT ( 'NONE',  ( 23.93147354620797529, 41.62439615674134075, -74.39855162740241212 ) ) ;
#32773 = DIRECTION ( 'NONE',  ( 0.000000000000000000, 1.000000000000000000, 0.000000000000000000 ) ) ;
#32774 = CARTESIAN_POINT ( 'NONE',  ( 0.000000000000000000, 36.79151656018385097, 0.000000000000000000 ) ) ;
#32775 = CARTESIAN_POINT ( 'NONE',  ( 91.56652514123703668, -30.00000000000000355, 97.63639661058265062 ) ) ;
#32776 = CARTESIAN_POINT ( 'NONE',  ( -46.00000000000000000, 500.0000000000002274, 5.000000000000001776 ) ) ;
#32777 = ADVANCED_FACE ( 'NONE', ( #23619 ), #1700, .T. ) ;
#32778 = ORIENTED_EDGE ( 'NONE', *, *, #79709, .T. ) ;
#32779 = AXIS2_PLACEMENT_3D ( 'NONE', #11958, #28726, #85333 ) ;
#32780 = ORIENTED_EDGE ( 'NONE', *, *, #60152, .T. ) ;
#32781 = VERTEX_POINT ( 'NONE', #39790 ) ;
#32782 = DIRECTION ( 'NONE',  ( -0.000000000000000000, -1.000000000000000000, -0.000000000000000000 ) ) ;
#32783 = CARTESIAN_POINT ( 'NONE',  ( 44.03654441205471670, 435.3114017552815085, 15.42721916007442751 ) ) ;
#32784 = CARTESIAN_POINT ( 'NONE',  ( -39.21606699811488994, 464.6169417331591944, 18.47934099087227366 ) ) ;
#32785 = ORIENTED_EDGE ( 'NONE', *, *, #63900, .T. ) ;
#32786 = CARTESIAN_POINT ( 'NONE',  ( 10.00004721872059754, 109.0001180468114939, -0.2617599822266517551 ) ) ;
#32787 = VECTOR ( 'NONE', #6603, 1000.000000000000000 ) ;
#32788 = ORIENTED_EDGE ( 'NONE', *, *, #3398, .F. ) ;
#32789 = CARTESIAN_POINT ( 'NONE',  ( 0.000000000000000000, 304.8518027762758038, 9.936999415352289589 ) ) ;
#32790 = CARTESIAN_POINT ( 'NONE',  ( 81.63480950427671701, -38.84194040926732328, 195.4446013772895583 ) ) ;
#32791 = DIRECTION ( 'NONE',  ( 0.000000000000000000, 1.000000000000000000, 0.000000000000000000 ) ) ;
#32792 = CARTESIAN_POINT ( 'NONE',  ( 37.78940342756484938, 315.0498657100115452, 14.83808658025191995 ) ) ;
#32793 = DIRECTION ( 'NONE',  ( -0.2281669654643559142, 0.2206132685150330730, 0.9482982767177750016 ) ) ;
#32794 = AXIS2_PLACEMENT_3D ( 'NONE', #19753, #36465, #68806 ) ;
#32795 = CARTESIAN_POINT ( 'NONE',  ( 29.98176661990081371, 1.340359594676612611E-15, 0.000000000000000000 ) ) ;
#32796 = CARTESIAN_POINT ( 'NONE',  ( -27.72576971702810411, 34.28420696235267684, -9.904009874722952134 ) ) ;
#32797 = CARTESIAN_POINT ( 'NONE',  ( -5.833333333391548692, -46.26205164321604002, 103.8776713793676834 ) ) ;
#32798 = CARTESIAN_POINT ( 'NONE',  ( 0.000000000000000000, 0.000000000000000000, -5.710657142857142432 ) ) ;
#32799 = ADVANCED_FACE ( 'NONE', ( #88340, #14952 ), #70044, .F. ) ;
#32800 = CARTESIAN_POINT ( 'NONE',  ( 0.000000000000000000, -1.200000000000000030E-05, -9.000000000000000000 ) ) ;
#32801 = EDGE_LOOP ( 'NONE', ( #36247, #27387, #105533, #56456 ) ) ;
#32802 = CARTESIAN_POINT ( 'NONE',  ( 3.352941176470589646, -48.79941684889505638, 104.5794940929807524 ) ) ;
#32803 = CARTESIAN_POINT ( 'NONE',  ( -25.12288893236338794, 295.6917592701588546, 2.117418662238229832 ) ) ;
#32804 = CARTESIAN_POINT ( 'NONE',  ( 14.75116209840774495, 43.55504285524111907, -90.22050492864485705 ) ) ;
#32805 = CARTESIAN_POINT ( 'NONE',  ( -7.847095227763523084, -4.129731495738496960, -7.493596212620242447 ) ) ;
#32806 = CARTESIAN_POINT ( 'NONE',  ( 4.433434719022584680, -18.46178206518997911, 35.06931429451628901 ) ) ;
#32807 = AXIS2_PLACEMENT_3D ( 'NONE', #91315, #17424, #2267 ) ;
#32808 = ADVANCED_FACE ( 'NONE', ( #40303 ), #6866, .F. ) ;
#32809 = LINE ( 'NONE', #83450, #73555 ) ;
#32810 = FACE_OUTER_BOUND ( 'NONE', #16039, .T. ) ;
#32811 = ORIENTED_EDGE ( 'NONE', *, *, #82955, .F. ) ;
#32812 = CARTESIAN_POINT ( 'NONE',  ( 85.91493313960407363, -31.99806336651779404, 183.3893818021954019 ) ) ;
#32813 = B_SPLINE_CURVE_WITH_KNOTS ( 'NONE', 3,
 ( #4054, #6155, #38049, #78465 ),
 .UNSPECIFIED., .F., .F.,
 ( 4, 4 ),
 ( 0.0007620286332983192655, 0.02097007980334730098 ),
 .UNSPECIFIED. ) ;
#32814 = ORIENTED_EDGE ( 'NONE', *, *, #16480, .F. ) ;
#32815 = CARTESIAN_POINT ( 'NONE',  ( 77.65333090421673035, -57.67122462496276825, -31.42556703637626470 ) ) ;
#32816 = ADVANCED_FACE ( 'NONE', ( #1416 ), #53376, .F. ) ;
#32817 = FACE_OUTER_BOUND ( 'NONE', #63817, .T. ) ;
#32818 = FACE_OUTER_BOUND ( 'NONE', #98939, .T. ) ;
#32819 = SURFACE_STYLE_USAGE ( .BOTH. , #55454 ) ;
#32820 = CARTESIAN_POINT ( 'NONE',  ( -80.86820734843506386, -30.00000000000000711, 18.00287957002532835 ) ) ;
#32821 = AXIS2_PLACEMENT_3D ( 'NONE', #14015, #21629, #72267 ) ;
#32822 = CARTESIAN_POINT ( 'NONE',  ( -81.12287823873506909, -38.00000000000000711, 151.5567027523417778 ) ) ;
#32823 = CARTESIAN_POINT ( 'NONE',  ( -7.137815226411302838, -3.000000000000000000, -4.175893272573455661 ) ) ;
#32824 = DIRECTION ( 'NONE',  ( -0.5735764363510497121, 0.8191520442889892450, 1.003171929053521665E-16 ) ) ;
#32826 = CARTESIAN_POINT ( 'NONE',  ( 0.000000000000000000, 0.000000000000000000, 0.000000000000000000 ) ) ;
#32825 = CARTESIAN_POINT ( 'NONE',  ( 4.225130582364226228, -48.93881382677318470, 104.4756880579354998 ) ) ;
#32827 = CARTESIAN_POINT ( 'NONE',  ( 15.59999999999999787, 1.533819458162526451E-15, 0.000000000000000000 ) ) ;
#32828 = CARTESIAN_POINT ( 'NONE',  ( -29.14598918812196615, 18.82621124954751224, 39.72463063980541875 ) ) ;
#32829 = FILL_AREA_STYLE ('',( #56527 ) ) ;
#32830 = CARTESIAN_POINT ( 'NONE',  ( -34.13947300040292276, 489.1610961117067404, 11.38003656226515581 ) ) ;
#32831 = CARTESIAN_POINT ( 'NONE',  ( -22.22732789360396666, 25.59821783804387607, 32.73558766513509255 ) ) ;
#32832 = DIRECTION ( 'NONE',  ( 0.000000000000000000, 0.8660254037844380415, -0.5000000000000009992 ) ) ;
#32833 = CARTESIAN_POINT ( 'NONE',  ( -98.63393505101123537, -37.99999999999995737, 192.2163830362448493 ) ) ;
#32834 = AXIS2_PLACEMENT_3D ( 'NONE', #65531, #98418, #57413 ) ;
#32835 = ORIENTED_EDGE ( 'NONE', *, *, #71127, .T. ) ;
#32836 = CARTESIAN_POINT ( 'NONE',  ( 6.585468679846623985, -3.617797563910821079, -6.733790807807558565 ) ) ;
#32837 = CARTESIAN_POINT ( 'NONE',  ( 7.000000000000000000, 0.000000000000000000, -13.00000000000000000 ) ) ;
#32838 = CARTESIAN_POINT ( 'NONE',  ( -7.896254658894416245, 81.21070817245799844, 1.307282859663297714 ) ) ;
#32839 = CARTESIAN_POINT ( 'NONE',  ( -19.15334754509612125, -18.31105778728934297, -33.83673051268581133 ) ) ;
#32840 = AXIS2_PLACEMENT_3D ( 'NONE', #82212, #73043, #98915 ) ;
#32842 = CARTESIAN_POINT ( 'NONE',  ( -65.77390279226092673, -47.40885602207553262, -25.69725042524944669 ) ) ;
#32841 = CARTESIAN_POINT ( 'NONE',  ( 28.09999999999999787, 3.309500000000003439, 4.052968581778167743E-16 ) ) ;
#32843 = EDGE_CURVE ( 'NONE', #54417, #68926, #37708, .T. ) ;
#32844 = ORIENTED_EDGE ( 'NONE', *, *, #92693, .F. ) ;
#32845 = AXIS2_PLACEMENT_3D ( 'NONE', #21428, #22499, #37093 ) ;
#32846 = VERTEX_POINT ( 'NONE', #67253 ) ;
#32847 = CARTESIAN_POINT ( 'NONE',  ( 41.94726657796896063, 461.2497493224228720, 3.266452559854905235 ) ) ;
#32848 = ADVANCED_FACE ( 'NONE', ( #66712 ), #18765, .T. ) ;
#32849 = CARTESIAN_POINT ( 'NONE',  ( 11.53059725919837497, 43.41062336697758184, -13.95763859544337215 ) ) ;
#32850 = PRESENTATION_LAYER_ASSIGNMENT (  '', '', ( #79332 ) ) ;
#32851 = DIRECTION ( 'NONE',  ( 0.000000000000000000, 0.2105263157894738946, -0.9775881905793005755 ) ) ;
#32852 = CARTESIAN_POINT ( 'NONE',  ( -34.63102061609615845, -60.00000000000000000, -40.35545487002439558 ) ) ;
#32853 = VERTEX_POINT ( 'NONE', #1956 ) ;
#32854 = CARTESIAN_POINT ( 'NONE',  ( 52.55293351040379690, -36.28902381433119473, -27.45765431991302563 ) ) ;
#32855 = LINE ( 'NONE', #65732, #60926 ) ;
#32856 = CARTESIAN_POINT ( 'NONE',  ( 95.90148991104773302, -45.27101873155104528, 194.1444148739948332 ) ) ;
#32858 = DIRECTION ( 'NONE',  ( -0.000000000000000000, -0.000000000000000000, -1.000000000000000000 ) ) ;
#32857 = DIRECTION ( 'NONE',  ( -1.000000000000000000, -1.224606353822377258E-16, -0.000000000000000000 ) ) ;
#32859 = AXIS2_PLACEMENT_3D ( 'NONE', #37665, #64042, #89367 ) ;
#32860 = ORIENTED_EDGE ( 'NONE', *, *, #76700, .T. ) ;
#32861 = VERTEX_POINT ( 'NONE', #41893 ) ;
#32862 = ORIENTED_EDGE ( 'NONE', *, *, #79102, .T. ) ;
#32863 = CARTESIAN_POINT ( 'NONE',  ( 31.19215877409873627, 416.1752359029570130, 25.29151037147646974 ) ) ;
#32864 = CARTESIAN_POINT ( 'NONE',  ( -6.187404903417438540, -12.10572765818576357, 11.71902858906391032 ) ) ;
#32865 = LINE ( 'NONE', #100750, #100109 ) ;
#32866 = ORIENTED_EDGE ( 'NONE', *, *, #71525, .T. ) ;
#32867 = CARTESIAN_POINT ( 'NONE',  ( -42.61340452791774425, 486.8925439250689919, 7.464118458850297344 ) ) ;
#32868 = CARTESIAN_POINT ( 'NONE',  ( -119.0671996398097008, 7.666536031838888654, 59.53359981990485039 ) ) ;
#32869 = CARTESIAN_POINT ( 'NONE',  ( 2.500000000000003109, -8.000000000000000000, -9.184850993605154600E-17 ) ) ;
#32870 = CARTESIAN_POINT ( 'NONE',  ( -36.61061158941262761, -57.69633519219438966, 50.91350493295865931 ) ) ;
#32871 = CARTESIAN_POINT ( 'NONE',  ( -2.977408999572650039, -32.18750000204838813, -7.188101187500001821 ) ) ;
#32872 = CARTESIAN_POINT ( 'NONE',  ( 12.33349330513380337, 1.593028355512270567E-15, 0.000000000000000000 ) ) ;
#32873 = CARTESIAN_POINT ( 'NONE',  ( 95.42421628608209971, 5.000000000000021316, 0.000000000000000000 ) ) ;
#32874 = CARTESIAN_POINT ( 'NONE',  ( 0.6444865106606342264, 28.14418859657819283, -38.41607911672674902 ) ) ;
#32875 = CIRCLE ( 'NONE', #105146, 2.000000000000000000 ) ;
#32876 = CARTESIAN_POINT ( 'NONE',  ( -49.63234380517151578, -59.99999999999993605, -40.41886796471348475 ) ) ;
#32877 = ADVANCED_FACE ( 'NONE', ( #74782 ), #48193, .T. ) ;
#32878 = CARTESIAN_POINT ( 'NONE',  ( -43.53995238963259595, 465.2530981678407898, 9.299505628812474001 ) ) ;
#32879 = CARTESIAN_POINT ( 'NONE',  ( -52.19514852257324122, -29.11169795166002316, 50.88471273071843370 ) ) ;
#32880 = CARTESIAN_POINT ( 'NONE',  ( 1.056274524463007403, 21.71983277640987353, -6.924796165863814856 ) ) ;
#32881 = ORIENTED_EDGE ( 'NONE', *, *, #43057, .T. ) ;
#32882 = CARTESIAN_POINT ( 'NONE',  ( -99.71322838326179294, -52.76976600324411493, 194.3808308585486770 ) ) ;
#32883 = CARTESIAN_POINT ( 'NONE',  ( -6.549255471957041941, 294.7416366638757381, -7.570647764150726822 ) ) ;
#32884 = CARTESIAN_POINT ( 'NONE',  ( 12.08709333886138459, -2.335920665582410294, 20.67766530190866447 ) ) ;
#32885 = ORIENTED_EDGE ( 'NONE', *, *, #21854, .F. ) ;
#32886 = DIRECTION ( 'NONE',  ( -0.000000000000000000, -0.000000000000000000, -1.000000000000000000 ) ) ;
#32887 = EDGE_CURVE ( 'NONE', #57077, #86773, #75771, .T. ) ;
#32888 = CARTESIAN_POINT ( 'NONE',  ( 73.36361653136737004, -38.32548766739345325, 155.0768100110214789 ) ) ;
#32889 = DIRECTION ( 'NONE',  ( -1.000000000000000000, -1.224606353822377258E-16, -0.000000000000000000 ) ) ;
#32890 = CARTESIAN_POINT ( 'NONE',  ( 0.000000000000000000, -30.00000000000000000, 8.000000000000000000 ) ) ;
#32891 = CARTESIAN_POINT ( 'NONE',  ( -16.52205554056997272, 294.5714208180984315, 9.877401598617169043 ) ) ;
#32892 = DIRECTION ( 'NONE',  ( 0.5735764363510466035, -0.8191520442889914655, 1.003171929053524500E-16 ) ) ;
#32893 = CARTESIAN_POINT ( 'NONE',  ( 82.57022881561088923, -29.99999999999999645, 149.8254230277452450 ) ) ;
#32894 =( BOUNDED_CURVE ( )  B_SPLINE_CURVE ( 2, ( #68627, #34679, #67551 ),
 .UNSPECIFIED., .F., .F. ) 
 B_SPLINE_CURVE_WITH_KNOTS ( ( 3, 3 ),
 ( 0.000000000000000000, 1.000000000000000000 ),
 .UNSPECIFIED. ) 
 CURVE ( )  GEOMETRIC_REPRESENTATION_ITEM ( )  RATIONAL_B_SPLINE_CURVE ( ( 1.428571428571429047, 1.428571428571428381, 1.000000000000000000 ) ) 
 REPRESENTATION_ITEM ( '' )  );
#32895 = CARTESIAN_POINT ( 'NONE',  ( -11.07168871570084079, 43.17206246446114903, -15.14491642044191977 ) ) ;
#32896 = DIRECTION ( 'NONE',  ( -1.000000000000000000, -1.224606353822377258E-16, -0.000000000000000000 ) ) ;
#32897 = DIRECTION ( 'NONE',  ( 1.000000000000000000, 0.000000000000000000, 0.000000000000000000 ) ) ;
#32898 = AXIS2_PLACEMENT_3D ( 'NONE', #29090, #54337, #87279 ) ;
#32899 = ORIENTED_EDGE ( 'NONE', *, *, #32408, .F. ) ;
#32900 = ORIENTED_EDGE ( 'NONE', *, *, #48232, .T. ) ;
#32901 = CARTESIAN_POINT ( 'NONE',  ( 49.21559585471668896, -60.28730590752689267, 56.32551750424051562 ) ) ;
#32902 = CARTESIAN_POINT ( 'NONE',  ( -9.404050855906653794, 302.6623156739180445, -10.04027337526763120 ) ) ;
#32903 = CARTESIAN_POINT ( 'NONE',  ( 9.553684976492661463, 51.29138652321832836, 3.543474137435660420 ) ) ;
#32904 = ORIENTED_EDGE ( 'NONE', *, *, #45581, .F. ) ;
#32905 = CARTESIAN_POINT ( 'NONE',  ( -92.91729557026953046, -38.35493114579749374, 42.71798821936229729 ) ) ;
#32906 = VERTEX_POINT ( 'NONE', #49447 ) ;
#32907 = SURFACE_SIDE_STYLE ('',( #29870 ) ) ;
#32908 = CARTESIAN_POINT ( 'NONE',  ( 92.01162595420805701, -38.35403553970205337, 34.85480957562649706 ) ) ;
#32909 = CARTESIAN_POINT ( 'NONE',  ( 14.52361579593611296, 21.59610066891373137, -5.116830242441418264 ) ) ;
#32910 = CARTESIAN_POINT ( 'NONE',  ( 106.0485595022860394, -60.15138397827151806, 161.1432654068886166 ) ) ;
#32911 = CARTESIAN_POINT ( 'NONE',  ( -30.99883150094105133, 438.8494022061962028, 22.05589272262757916 ) ) ;
#32912 = CARTESIAN_POINT ( 'NONE',  ( -1.469576158976823947E-15, -20.56250000409676915, 8.000000000000000000 ) ) ;
#32913 = CARTESIAN_POINT ( 'NONE',  ( -35.18713100599366328, 355.9408742645140364, 2.597692190029098125 ) ) ;
#32914 = CARTESIAN_POINT ( 'NONE',  ( 74.30875725675150534, -60.00000000000000711, 175.2953947742391279 ) ) ;
#32915 = AXIS2_PLACEMENT_3D ( 'NONE', #27690, #102057, #28218 ) ;
#32916 = CIRCLE ( 'NONE', #93178, 4.000000000000000888 ) ;
#32917 = CARTESIAN_POINT ( 'NONE',  ( 89.99999999999997158, 500000.0000000000582, 196.0238439516549818 ) ) ;
#32918 = AXIS2_PLACEMENT_3D ( 'NONE', #97353, #30537, #13249 ) ;
#32919 = ORIENTED_EDGE ( 'NONE', *, *, #58343, .F. ) ;
#32920 = CARTESIAN_POINT ( 'NONE',  ( 62.29079176448218647, -22.11117550964195644, 69.90653633777594678 ) ) ;
#32921 = CARTESIAN_POINT ( 'NONE',  ( -21.51569398614849504, 294.9107018935608266, -9.987480606144570672 ) ) ;
#32922 = CARTESIAN_POINT ( 'NONE',  ( 10.00248409573528896, -49.99966751047049485, 26.85804522429446095 ) ) ;
#32923 = ADVANCED_FACE ( 'NONE', ( #28278 ), #98018, .T. ) ;
#32924 = CARTESIAN_POINT ( 'NONE',  ( -9.375019126488638221, -5.000000000000000888, -18.75059979026688595 ) ) ;
#32925 = EDGE_CURVE ( 'NONE', #37873, #67790, #7333, .T. ) ;
#32927 = CARTESIAN_POINT ( 'NONE',  ( -4.504779885944381057, 54.31184324146714459, 6.294090811699073029 ) ) ;
#32926 = CARTESIAN_POINT ( 'NONE',  ( -76.05260806692862730, -29.99999999983540633, 166.0217771130949131 ) ) ;
#32928 = CARTESIAN_POINT ( 'NONE',  ( -41.61767405872787862, 334.1594308673269325, 11.43720139602365293 ) ) ;
#32929 = CYLINDRICAL_SURFACE ( 'NONE', #26091, 5.000000000000002665 ) ;
#32930 = CARTESIAN_POINT ( 'NONE',  ( -42.72825394835516022, 464.8055660505491460, 15.62448665940029713 ) ) ;
#32931 = CARTESIAN_POINT ( 'NONE',  ( 5.656854249492378806, -29.18749999999999645, 5.656854249492381470 ) ) ;
#32932 = CARTESIAN_POINT ( 'NONE',  ( 0.000000000000000000, 4.898587196589412829E-16, -4.000000000000000000 ) ) ;
#32933 = CONICAL_SURFACE ( 'NONE', #93191, 4.172000000000009479, 0.9599310885968813656 ) ;
#32934 = ADVANCED_FACE ( 'NONE', ( #26298 ), #92042, .F. ) ;
#32935 = AXIS2_PLACEMENT_3D ( 'NONE', #70597, #3203, #103488 ) ;
#32936 = EDGE_CURVE ( 'NONE', #40695, #5888, #61868, .T. ) ;
#32937 = CARTESIAN_POINT ( 'NONE',  ( 59.99387666504468086, 48.00000000000000000, 25.54086645653093512 ) ) ;
#32938 = ORIENTED_EDGE ( 'NONE', *, *, #75852, .F. ) ;
#32939 = CARTESIAN_POINT ( 'NONE',  ( 82.34467536305523083, -49.99737630304606739, 179.4894546011980481 ) ) ;
#32940 = CARTESIAN_POINT ( 'NONE',  ( 3.730566219500684344, -11.49691612730111245, -10.68061658281946080 ) ) ;
#32941 = FACE_OUTER_BOUND ( 'NONE', #85643, .T. ) ;
#32942 = ORIENTED_EDGE ( 'NONE', *, *, #45393, .T. ) ;
#32943 = CARTESIAN_POINT ( 'NONE',  ( 6.326622418652845248, -1.327077765692999733, 6.831545684615177194 ) ) ;
#32944 = EDGE_CURVE ( 'NONE', #94655, #31429, #83950, .T. ) ;
#32945 = DIRECTION ( 'NONE',  ( 0.000000000000000000, -1.000000000000000000, 0.000000000000000000 ) ) ;
#32946 = SURFACE_SIDE_STYLE ('',( #58248 ) ) ;
#32947 = CARTESIAN_POINT ( 'NONE',  ( 14.68536286785138323, 1.589102881334510720, 3.051189359066827311 ) ) ;
#32948 = LINE ( 'NONE', #89568, #2410 ) ;
#32949 = CARTESIAN_POINT ( 'NONE',  ( -44.17836536378457168, 435.2619773020560956, 14.65562696767996087 ) ) ;
#32950 = AXIS2_PLACEMENT_3D ( 'NONE', #74732, #97410, #25166 ) ;
#32951 = CIRCLE ( 'NONE', #93216, 2.000000000000001776 ) ;
#32952 = CARTESIAN_POINT ( 'NONE',  ( 6.815765296784520366, 0.6502800852029971823, -6.170377922158429840 ) ) ;
#32953 = CARTESIAN_POINT ( 'NONE',  ( -4.022544416453469829, -48.63060458932351793, 103.0357414394655962 ) ) ;
#32955 = CARTESIAN_POINT ( 'NONE',  ( -13.61191251355394449, 22.69522632434492238, 2.525242973133198010 ) ) ;
#32954 = CARTESIAN_POINT ( 'NONE',  ( -27.44437592492746703, -30.71555339929342665, 39.26539023425417696 ) ) ;
#32956 = AXIS2_PLACEMENT_3D ( 'NONE', #64488, #13784, #56355 ) ;
#32957 = CARTESIAN_POINT ( 'NONE',  ( -2.977408999572650039, -14.18750000204838280, -7.188101187500001821 ) ) ;
#32958 = CARTESIAN_POINT ( 'NONE',  ( -28.43956359133921552, 17.90386495480483120, -40.70637206596309454 ) ) ;
#32959 = CARTESIAN_POINT ( 'NONE',  ( 4.506320246070899316, -1.182860540001308802, 104.3949652630312670 ) ) ;
#32960 = VERTEX_POINT ( 'NONE', #25769 ) ;
#32961 = CARTESIAN_POINT ( 'NONE',  ( -19.45524037106812543, 49.98193815142347773, 60.61134026580515410 ) ) ;
#32962 = CARTESIAN_POINT ( 'NONE',  ( 96.86866073052655679, 1.030564683017419500E-14, 0.000000000000000000 ) ) ;
#32963 = CARTESIAN_POINT ( 'NONE',  ( 23.21751746555220564, 28.11705169068991950, -30.70617127781077116 ) ) ;
#32964 = FACE_OUTER_BOUND ( 'NONE', #60229, .T. ) ;
#32966 = CARTESIAN_POINT ( 'NONE',  ( 70.42381680912748720, -34.58960566250176072, -21.61503493545830779 ) ) ;
#32965 = DIRECTION ( 'NONE',  ( -1.000000000000000000, -1.224606353822377258E-16, -0.000000000000000000 ) ) ;
#32967 = EDGE_CURVE ( 'NONE', #18381, #10075, #44720, .T. ) ;
#32968 = AXIS2_PLACEMENT_3D ( 'NONE', #90454, #24683, #57532 ) ;
#32969 = ORIENTED_EDGE ( 'NONE', *, *, #10190, .T. ) ;
#32970 = DIRECTION ( 'NONE',  ( 0.000000000000000000, 1.000000000000000000, 0.000000000000000000 ) ) ;
#32971 = CYLINDRICAL_SURFACE ( 'NONE', #99650, 4.000000000000000888 ) ;
#32972 = VERTEX_POINT ( 'NONE', #10061 ) ;
#32973 = EDGE_CURVE ( 'NONE', #91653, #492, #5028, .T. ) ;
#32974 = EDGE_CURVE ( 'NONE', #100346, #74421, #90452, .T. ) ;
#32975 = CARTESIAN_POINT ( 'NONE',  ( 4.699999999999999289, 6.499999999999999112, 0.000000000000000000 ) ) ;
#32976 = CARTESIAN_POINT ( 'NONE',  ( -25.87876790621018941, 41.47384575004832641, -71.78385368780867282 ) ) ;
#32977 = CARTESIAN_POINT ( 'NONE',  ( -98.09477537189171414, -59.99999999999999289, 69.51200655767426895 ) ) ;
#32978 = DIRECTION ( 'NONE',  ( -0.000000000000000000, -1.000000000000000000, -0.000000000000000000 ) ) ;
#32979 = CARTESIAN_POINT ( 'NONE',  ( -13.76424046522695122, 304.5457540960956067, -10.06505265514019243 ) ) ;
#32980 = CARTESIAN_POINT ( 'NONE',  ( 27.97565635352651015, 315.9216507687758053, 12.64980990155120999 ) ) ;
#32981 = CARTESIAN_POINT ( 'NONE',  ( -32.15961058743295808, 464.7082972388441817, 10.94058067631164022 ) ) ;
#32983 = CARTESIAN_POINT ( 'NONE',  ( 29.99999999999051070, 486.8910789110960309, 5.528145857006796504 ) ) ;
#32982 = CARTESIAN_POINT ( 'NONE',  ( 7.996668422914432028, -4.999999999991826094, -91.14546720080765851 ) ) ;
#32984 = CARTESIAN_POINT ( 'NONE',  ( -81.99888381046133645, -53.52207800286723227, 181.3765808315105801 ) ) ;
#32985 = ORIENTED_EDGE ( 'NONE', *, *, #55159, .F. ) ;
#32986 = CARTESIAN_POINT ( 'NONE',  ( 4.852941176470593199, 42.83333333333328596, -70.80672828634229177 ) ) ;
#32987 = AXIS2_PLACEMENT_3D ( 'NONE', #29631, #85176, #36667 ) ;
#32988 = VERTEX_POINT ( 'NONE', #13098 ) ;
#32989 = CIRCLE ( 'NONE', #43287, 0.9999999999999980016 ) ;
#32990 = ORIENTED_EDGE ( 'NONE', *, *, #79121, .T. ) ;
#32991 = CARTESIAN_POINT ( 'NONE',  ( -1.224646799147352665E-15, -3.000000000000002665, -75.00000000000001421 ) ) ;
#32992 = DIRECTION ( 'NONE',  ( 0.000000000000000000, -0.000000000000000000, 1.000000000000000000 ) ) ;
#32993 = VERTEX_POINT ( 'NONE', #37965 ) ;
#32994 = EDGE_CURVE ( 'NONE', #70408, #14645, #48032, .T. ) ;
#32995 = COLOUR_RGB ( '', 0.40784314, 0.44705882, 0.49803922) ;
#32996 = CYLINDRICAL_SURFACE ( 'NONE', #101246, 5.000000000000002665 ) ;
#32997 = CARTESIAN_POINT ( 'NONE',  ( -44.70137845890145911, -57.67116879762227910, -40.89012893473564958 ) ) ;
#32998 = DIRECTION ( 'NONE',  ( 0.000000000000000000, -1.000000000000000000, 0.000000000000000000 ) ) ;
#32999 = CARTESIAN_POINT ( 'NONE',  ( -7.934203308536663890, -61.13299659982202883, 1.057099537198546102 ) ) ;
#33000 = CARTESIAN_POINT ( 'NONE',  ( 20.11650669486618881, 4.000000000000003553, 4.898587196589414801E-16 ) ) ;
#33001 = CARTESIAN_POINT ( 'NONE',  ( 11.04978436692697308, -5.000000000000000000, -91.95127353814174853 ) ) ;
#33002 = CARTESIAN_POINT ( 'NONE',  ( -43.47770857297125957, 484.8227827122622102, 4.253339224813438513 ) ) ;
#33003 = CIRCLE ( 'NONE', #12258, 4.000000000000007105 ) ;
#33004 = CARTESIAN_POINT ( 'NONE',  ( 109.5128197388708031, -29.99999999999998934, 168.1051457340969932 ) ) ;
#33005 = CIRCLE ( 'NONE', #27884, 6.500000000000000000 ) ;
#33006 = CARTESIAN_POINT ( 'NONE',  ( -109.5811972119284690, -29.99999999999999289, 174.3366342583755113 ) ) ;
#33007 = CARTESIAN_POINT ( 'NONE',  ( -64.30537749630316569, -18.62720888008740161, 73.57097262722605535 ) ) ;
#33008 = ORIENTED_EDGE ( 'NONE', *, *, #40000, .F. ) ;
#33009 = CARTESIAN_POINT ( 'NONE',  ( -58.04881918066196533, 38.95268114429830320, 26.31400674393213635 ) ) ;
#33010 = CARTESIAN_POINT ( 'NONE',  ( 95.09347488121859726, -60.00000000001951150, -4.937967903116023294 ) ) ;
#33011 = VERTEX_POINT ( 'NONE', #88080 ) ;
#33012 = CARTESIAN_POINT ( 'NONE',  ( 3.214995758538034771E-05, -42.95368998299849750, 31.04859829010212380 ) ) ;
#33013 = CARTESIAN_POINT ( 'NONE',  ( -1.320432766682874540E-15, -10.90625000204838457, 7.188101187500000044 ) ) ;
#33014 = ADVANCED_FACE ( 'NONE', ( #38478 ), #70828, .F. ) ;
#33015 = CARTESIAN_POINT ( 'NONE',  ( -13.50000000000000000, -2.625659737069750754, -0.1132121849006608727 ) ) ;
#33016 = EDGE_LOOP ( 'NONE', ( #5175, #11271, #9702, #54968 ) ) ;
#33017 = CARTESIAN_POINT ( 'NONE',  ( 6.560701988338252910, -30.00000000000000000, 2.946301444182167106 ) ) ;
#33018 = ORIENTED_EDGE ( 'NONE', *, *, #8817, .F. ) ;
#33019 = SURFACE_STYLE_USAGE ( .BOTH. , #49150 ) ;
#33020 = CARTESIAN_POINT ( 'NONE',  ( -99.26889953123149724, -60.00000000000001421, 202.0842824767352681 ) ) ;
#33021 = CARTESIAN_POINT ( 'NONE',  ( 9.933618426942553370, -57.79423783648532265, 25.82409549033520690 ) ) ;
#33022 = CARTESIAN_POINT ( 'NONE',  ( 7.188101187500001821, -22.43750000204838813, -2.977408999572650483 ) ) ;
#33023 = CARTESIAN_POINT ( 'NONE',  ( 46.00000000000580513, 462.9210814260900406, 7.766178785318980538 ) ) ;
#33024 = CARTESIAN_POINT ( 'NONE',  ( -24.46190898409515313, 27.53854914924986730, -31.75601090834104312 ) ) ;
#33025 = CARTESIAN_POINT ( 'NONE',  ( -6.400492677076282000, 53.43410452881639827, -7.878742231350887693 ) ) ;
#33026 = CARTESIAN_POINT ( 'NONE',  ( 10.41054107240687188, 1.482358050883964840E-15, 0.000000000000000000 ) ) ;
#33027 = CARTESIAN_POINT ( 'NONE',  ( 5.799999999999999822, 1.502314598737159426E-15, -8.000000000000000000 ) ) ;
#33028 = CARTESIAN_POINT ( 'NONE',  ( 0.000000000000000000, 50.89575828009192549, 0.000000000000000000 ) ) ;
#33029 = CARTESIAN_POINT ( 'NONE',  ( 4.898587196589412829E-16, -22.62499999999999289, -8.000000000000000000 ) ) ;
#33030 = DIRECTION ( 'NONE',  ( -1.000000000000000000, -0.000000000000000000, -0.000000000000000000 ) ) ;
#33031 = CARTESIAN_POINT ( 'NONE',  ( -33.72753996741100480, -49.90232404750766904, 36.63834850608077431 ) ) ;
#33032 = AXIS2_PLACEMENT_3D ( 'NONE', #100886, #10283, #91752 ) ;
#33033 = CARTESIAN_POINT ( 'NONE',  ( -3.303250429861293469, -49.28697031698179387, 103.9470740044689308 ) ) ;
#33034 = CARTESIAN_POINT ( 'NONE',  ( 40.62329115609131236, -49.88684013868402900, 41.58757686396207731 ) ) ;
#33035 = CIRCLE ( 'NONE', #27822, 5.000000000000002665 ) ;
#33036 = FACE_OUTER_BOUND ( 'NONE', #17566, .T. ) ;
#33037 = VERTEX_POINT ( 'NONE', #44975 ) ;
#33038 = CARTESIAN_POINT ( 'NONE',  ( 44.19123973042410825, 435.3640897803218763, 10.85603094146364533 ) ) ;
#33039 = CIRCLE ( 'NONE', #91608, 5.000000000000010658 ) ;
#33040 = CARTESIAN_POINT ( 'NONE',  ( -76.67538504582743997, -38.42797185326705289, 182.7090895004452591 ) ) ;
#33041 = ORIENTED_EDGE ( 'NONE', *, *, #10109, .F. ) ;
#33043 = CARTESIAN_POINT ( 'NONE',  ( -43.51047069092275166, 435.7684321374283627, 8.546621873850019924 ) ) ;
#33042 = CARTESIAN_POINT ( 'NONE',  ( 2.499999999999998668, -12.75202509204646972, 21.42349226578282995 ) ) ;
#33044 = CARTESIAN_POINT ( 'NONE',  ( -12.19077546297355141, 22.10107656903681672, 6.639256695208207937 ) ) ;
#33045 = CARTESIAN_POINT ( 'NONE',  ( -49.28004588020300503, 7.871673175840900427, -15.62336800674829007 ) ) ;
#33046 = DIRECTION ( 'NONE',  ( 0.000000000000000000, 0.000000000000000000, -1.000000000000000000 ) ) ;
#33047 = CARTESIAN_POINT ( 'NONE',  ( 37.26669594562353893, 460.4728090823174966, 2.456107597708254708 ) ) ;
#33048 = CARTESIAN_POINT ( 'NONE',  ( -38.22195112133888983, 437.6732586221718293, 4.643349236000520186 ) ) ;
#33049 = CARTESIAN_POINT ( 'NONE',  ( 5.475947152006322760, -88.16217730109126194, 2.462898245435134470 ) ) ;
#33050 = CARTESIAN_POINT ( 'NONE',  ( -4.250000000000000000, 5.204748896376250699E-16, -0.5505556536572887572 ) ) ;
#33051 = CARTESIAN_POINT ( 'NONE',  ( 103.6141585822474411, -60.00000000000000711, 102.1783202260197925 ) ) ;
#33052 = CARTESIAN_POINT ( 'NONE',  ( 14.84266821126404423, 4.606643506680114797, -5.685020543968223095 ) ) ;
#33053 = CARTESIAN_POINT ( 'NONE',  ( -34.74668950323464145, 477.5735541584660382, -0.3049228838951520415 ) ) ;
#33054 = EDGE_LOOP ( 'NONE', ( #44775, #26324, #64305, #46029, #101959 ) ) ;
#33055 = EDGE_CURVE ( 'NONE', #85958, #87422, #102587, .T. ) ;
#33056 = CARTESIAN_POINT ( 'NONE',  ( -98.75918947158213257, -29.99999999999995026, 189.3635776327697897 ) ) ;
#33057 = ORIENTED_EDGE ( 'NONE', *, *, #19401, .F. ) ;
#33058 = DIRECTION ( 'NONE',  ( 0.000000000000000000, 0.000000000000000000, 1.000000000000000000 ) ) ;
#33059 = CARTESIAN_POINT ( 'NONE',  ( -16.05785784214732104, 4.775831776487164504, 3.710403933803105847 ) ) ;
#33060 = CARTESIAN_POINT ( 'NONE',  ( 4.474875413805487590, 142.5213423678850120, 5.000000000000000888 ) ) ;
#33061 = CARTESIAN_POINT ( 'NONE',  ( 25.12563779285825305, 306.0698335614371217, 10.43520451652393355 ) ) ;
#33062 = DIRECTION ( 'NONE',  ( 0.8308658609248572580, 0.5564727496918389082, 0.000000000000000000 ) ) ;
#33063 = CARTESIAN_POINT ( 'NONE',  ( -1.320432766682874540E-15, -25.90625000204838813, 7.188101187500000044 ) ) ;
#33064 = DIRECTION ( 'NONE',  ( 0.000000000000000000, 0.000000000000000000, -1.000000000000000000 ) ) ;
#33065 = CARTESIAN_POINT ( 'NONE',  ( 6.978962139004955212, 41.42610740536763103, -70.37780174659977206 ) ) ;
#33066 = ADVANCED_FACE ( 'NONE', ( #55150 ), #38998, .T. ) ;
#33067 = ORIENTED_EDGE ( 'NONE', *, *, #69560, .T. ) ;
#33068 = EDGE_CURVE ( 'NONE', #94772, #58831, #79962, .T. ) ;
#33070 = ORIENTED_EDGE ( 'NONE', *, *, #21567, .T. ) ;
#33069 = DIRECTION ( 'NONE',  ( 1.000000000000000000, -0.000000000000000000, -0.000000000000000000 ) ) ;
#33071 = CARTESIAN_POINT ( 'NONE',  ( 80.22144217257282151, -42.96589628622726309, 151.2297849153674463 ) ) ;
#33072 = CARTESIAN_POINT ( 'NONE',  ( -62.01418705508173446, 38.95383793066508815, -16.66584972140234910 ) ) ;
#33073 = CARTESIAN_POINT ( 'NONE',  ( 9.918325909156569864, 88.79235231707430387, 1.298699613733149683 ) ) ;
#33074 = ORIENTED_EDGE ( 'NONE', *, *, #86794, .F. ) ;
#33075 = CIRCLE ( 'NONE', #2074, 4.000000000000000888 ) ;
#33076 = DIRECTION ( 'NONE',  ( 0.000000000000000000, 0.000000000000000000, 1.000000000000000000 ) ) ;
#33077 = ADVANCED_FACE ( 'NONE', ( #61701 ), #29453, .F. ) ;
#33078 = CARTESIAN_POINT ( 'NONE',  ( -0.1547416878174255328, 12.93287229451991571, -51.74246760002737489 ) ) ;
#33079 = CARTESIAN_POINT ( 'NONE',  ( -5.082755093536325042, -11.09375000204838457, -5.082755093536325930 ) ) ;
#33080 = DIRECTION ( 'NONE',  ( 0.000000000000000000, 1.000000000000000000, 0.000000000000000000 ) ) ;
#33081 = MECHANICAL_DESIGN_GEOMETRIC_PRESENTATION_REPRESENTATION (  '', ( #60640 ), #88184 ) ;
#33082 = CARTESIAN_POINT ( 'NONE',  ( 48.10000000000000142, 0.000000000000000000, 0.000000000000000000 ) ) ;
#33083 = CARTESIAN_POINT ( 'NONE',  ( -32.13498246155330662, 335.5900755486186995, 17.83550542174494069 ) ) ;
#33084 = B_SPLINE_CURVE_WITH_KNOTS ( 'NONE', 3,
 ( #24093, #8398, #67189, #26232, #100066, #81734, #798, #73656, #98986, #17577, #82286, #49377, #89335, #17042, #33768, #32163 ),
 .UNSPECIFIED., .F., .F.,
 ( 4, 2, 2, 2, 2, 2, 2, 4 ),
 ( 1.851527828850887154E-16, 0.0005159648664366578213, 0.001031929732873130461, 0.001547894599309602992, 0.002063859465746075740, 0.002579824332182548054, 0.003095789198619020802, 0.004127718931491971069 ),
 .UNSPECIFIED. ) ;
#33085 = EDGE_LOOP ( 'NONE', ( #41102, #92789, #95085, #91083, #54866 ) ) ;
#33087 = DIRECTION ( 'NONE',  ( -1.000000000000000000, -0.000000000000000000, -0.000000000000000000 ) ) ;
#33086 = AXIS2_PLACEMENT_3D ( 'NONE', #7241, #73027, #105937 ) ;
#33088 = CARTESIAN_POINT ( 'NONE',  ( 7.274255167503934416, 41.49770586683256113, -59.52552407551726787 ) ) ;
#33089 = CARTESIAN_POINT ( 'NONE',  ( 86.12568212521020428, -61.03451969644774522, 194.3966504858508983 ) ) ;
#33090 = CARTESIAN_POINT ( 'NONE',  ( -7.980179952708205483E-13, 34.17188553057791722, -29.75000000000694911 ) ) ;
#33091 = CARTESIAN_POINT ( 'NONE',  ( 5.082755093536325930, -32.46875000204838813, -5.082755093536325042 ) ) ;
#33092 = CARTESIAN_POINT ( 'NONE',  ( 39.40329081872960160, -37.47882864960006088, 48.99327379398392424 ) ) ;
#33093 = CARTESIAN_POINT ( 'NONE',  ( -40.22495779148586337, 489.7644056528380929, 10.97694427318330668 ) ) ;
#33094 = CARTESIAN_POINT ( 'NONE',  ( 7.940845330314040496, 52.04497172380727932, 1.691901466013218780 ) ) ;
#33095 = FACE_OUTER_BOUND ( 'NONE', #73715, .T. ) ;
#33096 = PRODUCT_CONTEXT ( 'NONE', #47261, 'mechanical' ) ;
#33097 = CARTESIAN_POINT ( 'NONE',  ( -9.842473135306409660, 33.58931817113587925, 1.785129593756275224 ) ) ;
#33098 = VERTEX_POINT ( 'NONE', #89133 ) ;
#33099 = CARTESIAN_POINT ( 'NONE',  ( 0.3336880381504699900, 43.18998736639818503, 18.70756200222306020 ) ) ;
#33100 = DIRECTION ( 'NONE',  ( -1.000000000000000000, -1.224606353822377258E-16, -0.000000000000000000 ) ) ;
#33101 = SURFACE_STYLE_USAGE ( .BOTH. , #134 ) ;
#33102 = SURFACE_STYLE_FILL_AREA ( #83211 ) ;
#33103 = COLOUR_RGB ( '', 0.72549020, 0.75294118, 0.79215686) ;
#33104 = VERTEX_POINT ( 'NONE', #57805 ) ;
#33105 = FACE_OUTER_BOUND ( 'NONE', #60248, .T. ) ;
#33106 = CARTESIAN_POINT ( 'NONE',  ( 113.6035234506770024, -57.67119983476416678, 183.6741733121881737 ) ) ;
#33107 = AXIS2_PLACEMENT_3D ( 'NONE', #9912, #50894, #83277 ) ;
#33108 = EDGE_CURVE ( 'NONE', #12693, #82401, #63548, .T. ) ;
#33109 = CARTESIAN_POINT ( 'NONE',  ( 36.55533968308436243, 463.5207292468175524, 19.71490071751826179 ) ) ;
#33110 = CYLINDRICAL_SURFACE ( 'NONE', #22616, 1.000000000000000000 ) ;
#33111 = FACE_OUTER_BOUND ( 'NONE', #97077, .T. ) ;
#33112 = CARTESIAN_POINT ( 'NONE',  ( 37.40775037356466726, 25.53061312228623692, 13.45617127781006594 ) ) ;
#33113 = CARTESIAN_POINT ( 'NONE',  ( -76.26472227669087545, -60.00000000000000000, 188.0289714178661882 ) ) ;
#33114 = CARTESIAN_POINT ( 'NONE',  ( 0.000000000000000000, -80.00000000000000000, 27.00000000000000000 ) ) ;
#33115 = DIRECTION ( 'NONE',  ( 0.000000000000000000, 0.000000000000000000, 1.000000000000000000 ) ) ;
#33116 = CARTESIAN_POINT ( 'NONE',  ( -40.93435977689158989, 414.3154843149413296, 27.72243992809649527 ) ) ;
#33117 = CARTESIAN_POINT ( 'NONE',  ( -84.38815688596613995, -53.81528062727464601, 189.6626461044262442 ) ) ;
#33118 = ORIENTED_EDGE ( 'NONE', *, *, #52769, .F. ) ;
#33119 = CARTESIAN_POINT ( 'NONE',  ( 25.46344391298313781, 305.2723305331812185, -9.690526388420286352 ) ) ;
#33120 = ORIENTED_EDGE ( 'NONE', *, *, #5854, .F. ) ;
#33121 = CARTESIAN_POINT ( 'NONE',  ( 21.36650669486618881, 1.474610560812782335E-15, 0.000000000000000000 ) ) ;
#33122 = CARTESIAN_POINT ( 'NONE',  ( -5.683639242321874896, -2.934261738049319224, 103.9372442403038548 ) ) ;
#33123 = CARTESIAN_POINT ( 'NONE',  ( -86.93649315962268531, -60.22167703688511864, -9.633606967954129630 ) ) ;
#33124 = CARTESIAN_POINT ( 'NONE',  ( 37.46929538816834793, 50.00000000000000000, -55.58823529411764497 ) ) ;
#33125 = DIRECTION ( 'NONE',  ( -1.000000000000000000, 0.000000000000000000, 0.000000000000000000 ) ) ;
#33126 = VERTEX_POINT ( 'NONE', #97732 ) ;
#33127 = CARTESIAN_POINT ( 'NONE',  ( -43.00000000000000000, 500.0000000000002274, -12.00000000000000711 ) ) ;
#33128 = CARTESIAN_POINT ( 'NONE',  ( 10.35700060563541669, 16.95883745406678855, -9.900998136418390771 ) ) ;
#33129 = CARTESIAN_POINT ( 'NONE',  ( -10.45706415777455689, -1.734723475976807094E-15, -13.60704923275582701 ) ) ;
#33130 = FACE_OUTER_BOUND ( 'NONE', #25987, .T. ) ;
#33131 = CARTESIAN_POINT ( 'NONE',  ( 41.39111156191358276, -30.00000000000003908, -36.78675873448672462 ) ) ;
#33132 = CARTESIAN_POINT ( 'NONE',  ( -77.89137182638854995, -46.43782183837505073, 140.2357373465546004 ) ) ;
#33133 = ORIENTED_EDGE ( 'NONE', *, *, #11199, .F. ) ;
#33134 = CARTESIAN_POINT ( 'NONE',  ( 66.64731328016637235, -30.00000000000005684, 114.0820693445010363 ) ) ;
#33135 = CARTESIAN_POINT ( 'NONE',  ( 101.4868948250290259, 6.123233995736582872E-16, -5.000000000000011546 ) ) ;
#33136 = CARTESIAN_POINT ( 'NONE',  ( 113.2613034959341149, -57.67119509769668184, 154.8441214569275530 ) ) ;
#33137 = EDGE_LOOP ( 'NONE', ( #56889, #67668, #27814 ) ) ;
#33138 = FACE_OUTER_BOUND ( 'NONE', #62097, .T. ) ;
#33139 = EDGE_CURVE ( 'NONE', #90336, #57292, #73456, .T. ) ;
#33140 = EDGE_CURVE ( 'NONE', #79335, #66879, #34427, .T. ) ;
#33141 = CARTESIAN_POINT ( 'NONE',  ( 104.0908829527487711, 1.030564683017419500E-14, 0.000000000000000000 ) ) ;
#33142 = EDGE_LOOP ( 'NONE', ( #51653, #81459, #26526, #18525, #31086 ) ) ;
#33143 = CARTESIAN_POINT ( 'NONE',  ( 53.78349330513380266, 4.000000000000014211, 0.000000000000000000 ) ) ;
#33144 = SURFACE_SIDE_STYLE ('',( #25053 ) ) ;
#33145 = PLANE ( 'NONE',  #5371 ) ;
#33146 = CARTESIAN_POINT ( 'NONE',  ( 4.401442555609581635E-16, -20.28125000204838813, -7.188101187500000044 ) ) ;
#33147 = CARTESIAN_POINT ( 'NONE',  ( 43.69219460922279552, 484.4832989965491947, 2.442496667976668867 ) ) ;
#33148 = AXIS2_PLACEMENT_3D ( 'NONE', #95966, #22091, #54945 ) ;
#33149 = CARTESIAN_POINT ( 'NONE',  ( 9.843039827103241990, 81.40916497491664927, -1.781495459429541572 ) ) ;
#33150 = DIRECTION ( 'NONE',  ( 0.000000000000000000, 0.000000000000000000, 1.000000000000000000 ) ) ;
#33151 = CARTESIAN_POINT ( 'NONE',  ( -7.500000000000000000, -3.882691789159502971, -7.781695678276665973 ) ) ;
#33152 = CARTESIAN_POINT ( 'NONE',  ( 1.177401751624806314, 48.00000000000000711, -100.0000000000000284 ) ) ;
#33153 = ORIENTED_EDGE ( 'NONE', *, *, #51710, .F. ) ;
#33154 = CARTESIAN_POINT ( 'NONE',  ( -6.921856738059538827, 41.59435685020019235, -70.13580383255586526 ) ) ;
#33155 = CIRCLE ( 'NONE', #46899, 4.172000000000009479 ) ;
#33157 = CARTESIAN_POINT ( 'NONE',  ( 30.57601822009955228, -42.95894917474103636, 33.95501319845223520 ) ) ;
#33156 = CARTESIAN_POINT ( 'NONE',  ( -3.365451957726314447, -49.06858650466291749, 104.1992105446094001 ) ) ;
#33158 = CARTESIAN_POINT ( 'NONE',  ( 35.50524833579024886, 381.4531880784116993, 5.944804199580530302 ) ) ;
#33159 = VERTEX_POINT ( 'NONE', #105833 ) ;
#33160 = CARTESIAN_POINT ( 'NONE',  ( -0.9529166959714684415, 13.93637536997674786, 51.31279264900302195 ) ) ;
#33161 = ORIENTED_EDGE ( 'NONE', *, *, #77790, .F. ) ;
#33162 = CARTESIAN_POINT ( 'NONE',  ( 0.000000000000000000, -78.00000000000000000, 27.00000000000000000 ) ) ;
#33163 = CARTESIAN_POINT ( 'NONE',  ( 16.99873220396137796, 302.5765783365897619, -10.05837913125274952 ) ) ;
#33164 = DIRECTION ( 'NONE',  ( 0.000000000000000000, 0.000000000000000000, 1.000000000000000000 ) ) ;
#33165 = DIRECTION ( 'NONE',  ( 1.000000000000000000, 0.000000000000000000, 0.000000000000000000 ) ) ;
#33166 = CARTESIAN_POINT ( 'NONE',  ( 0.1694652132101762132, 46.21043659876566778, 16.25867386421069938 ) ) ;
#33167 = CARTESIAN_POINT ( 'NONE',  ( -36.69890166230307216, 463.9786769757894263, 19.62055820434390085 ) ) ;
#33168 = ORIENTED_EDGE ( 'NONE', *, *, #33450, .T. ) ;
#33169 = CARTESIAN_POINT ( 'NONE',  ( 91.96166712811336197, -60.00000000000000711, -14.13641865815662868 ) ) ;
#33170 = CARTESIAN_POINT ( 'NONE',  ( 22.88520313534120731, 26.05176548070731712, -30.73931513807078986 ) ) ;
#33171 = CARTESIAN_POINT ( 'NONE',  ( 32.21352700826018634, 464.7514164808271175, 11.12064077799058559 ) ) ;
#33172 = CARTESIAN_POINT ( 'NONE',  ( 69.67238219402268840, 4.000000000000014211, 0.000000000000000000 ) ) ;
#33173 = AXIS2_PLACEMENT_3D ( 'NONE', #18349, #68483, #84123 ) ;
#33174 = CARTESIAN_POINT ( 'NONE',  ( 46.86248696599233199, 13.70470512780037353, -15.14813956650342419 ) ) ;
#33175 = EDGE_LOOP ( 'NONE', ( #62795, #43582, #55590, #90601, #85007 ) ) ;
#33176 = DIRECTION ( 'NONE',  ( 0.000000000000000000, 0.000000000000000000, -1.000000000000000000 ) ) ;
#33177 = ORIENTED_EDGE ( 'NONE', *, *, #49773, .F. ) ;
#33178 = ORIENTED_EDGE ( 'NONE', *, *, #61734, .T. ) ;
#33179 = FACE_OUTER_BOUND ( 'NONE', #52447, .T. ) ;
#33180 =( NAMED_UNIT ( * ) SI_UNIT ( $, .STERADIAN. ) SOLID_ANGLE_UNIT ( ) );
#33181 = CARTESIAN_POINT ( 'NONE',  ( 38.58349330513380693, 1.593028355512270567E-15, 0.000000000000000000 ) ) ;
#33182 = CARTESIAN_POINT ( 'NONE',  ( 30.83690085618862398, 321.2017700030009451, 14.45204011326535998 ) ) ;
#33183 = CARTESIAN_POINT ( 'NONE',  ( 84.40376416015234895, -45.28787472347771370, -3.486817255051028130 ) ) ;
#33184 = CIRCLE ( 'NONE', #83052, 5.000000000000002665 ) ;
#33185 = CARTESIAN_POINT ( 'NONE',  ( -43.59476163150520733, 373.0867689854657669, 14.23677538628125561 ) ) ;
#33186 = CARTESIAN_POINT ( 'NONE',  ( -5.558262485387479579, -66.13834130795673616, 14.15003227941667241 ) ) ;
#33187 = FACE_OUTER_BOUND ( 'NONE', #2730, .T. ) ;
#33188 = CARTESIAN_POINT ( 'NONE',  ( 12.50000000000000533, 38.20397074648182212, -60.24274188675438779 ) ) ;
#33189 = ORIENTED_EDGE ( 'NONE', *, *, #84130, .F. ) ;
#33190 = CARTESIAN_POINT ( 'NONE',  ( 30.25697458664275530, 12.04847113665178071, 39.73669343589866543 ) ) ;
#33191 = ORIENTED_EDGE ( 'NONE', *, *, #84689, .T. ) ;
#33192 = CARTESIAN_POINT ( 'NONE',  ( 9.349999999999997868, 1.533819458162526451E-15, 0.000000000000000000 ) ) ;
#33193 = CARTESIAN_POINT ( 'NONE',  ( 11.93255308427328565, 294.5886021379643580, 9.881054392645332030 ) ) ;
#33195 = ORIENTED_EDGE ( 'NONE', *, *, #50250, .F. ) ;
#33194 = CARTESIAN_POINT ( 'NONE',  ( -39.59863853631028974, -59.99999999999997158, 42.73346896236057546 ) ) ;
#33196 = CARTESIAN_POINT ( 'NONE',  ( 67.53797569337646678, -36.00813603609307734, 91.97696651167636617 ) ) ;
#33197 = ORIENTED_EDGE ( 'NONE', *, *, #19382, .F. ) ;
#33198 = CARTESIAN_POINT ( 'NONE',  ( 32.06611684422574626, 38.95383793063784594, 55.63518754870414540 ) ) ;
#33199 = EDGE_CURVE ( 'NONE', #49522, #63698, #55666, .T. ) ;
#33200 = CARTESIAN_POINT ( 'NONE',  ( -5.835411572216779419, 11.94238963164415068, 3.866789010015637462 ) ) ;
#33201 =( BOUNDED_CURVE ( )  B_SPLINE_CURVE ( 2, ( #89344, #99534, #58573 ),
 .UNSPECIFIED., .F., .F. ) 
 B_SPLINE_CURVE_WITH_KNOTS ( ( 3, 3 ),
 ( 0.000000000000000000, 1.000000000000000000 ),
 .UNSPECIFIED. ) 
 CURVE ( )  GEOMETRIC_REPRESENTATION_ITEM ( )  RATIONAL_B_SPLINE_CURVE ( ( 1.000000000000000000, 1.857142857142858317, 1.000000000000000000 ) ) 
 REPRESENTATION_ITEM ( '' )  );
#33202 = EDGE_CURVE ( 'NONE', #29452, #2025, #32604, .T. ) ;
#33203 = CARTESIAN_POINT ( 'NONE',  ( -112.4702214903622490, -57.67117150189849895, 147.0458187677821797 ) ) ;
#33204 = ORIENTED_EDGE ( 'NONE', *, *, #63437, .T. ) ;
#33205 = DIRECTION ( 'NONE',  ( -0.000000000000000000, 1.000000000000000000, -0.000000000000000000 ) ) ;
#33206 = CARTESIAN_POINT ( 'NONE',  ( -34.84618260875192419, 489.9833681528629654, 11.97975507378832738 ) ) ;
#33207 = DIRECTION ( 'NONE',  ( -1.000000000000000000, -1.224606353822377258E-16, -0.000000000000000000 ) ) ;
#33208 = CARTESIAN_POINT ( 'NONE',  ( -5.656854249492381470, -26.75000000409677625, 5.656854249492379694 ) ) ;
#33209 = CARTESIAN_POINT ( 'NONE',  ( 0.5805565836007654523, 7.505553499465139389, 1.865978384307260116E-16 ) ) ;
#33210 =( GEOMETRIC_REPRESENTATION_CONTEXT ( 3 ) GLOBAL_UNCERTAINTY_ASSIGNED_CONTEXT ( ( #6009 ) ) GLOBAL_UNIT_ASSIGNED_CONTEXT ( ( #86345, #46906, #77701 ) ) REPRESENTATION_CONTEXT ( 'NONE', 'WORKASPACE' ) );
#33211 = DIRECTION ( 'NONE',  ( 0.5735764363510557073, -0.8191520442889850262, 1.003171929053516612E-16 ) ) ;
#33212 = CARTESIAN_POINT ( 'NONE',  ( -10.00002837220453600, 7.499959371249889983, 5.000000000000000888 ) ) ;
#33213 = FACE_OUTER_BOUND ( 'NONE', #2478, .T. ) ;
#33214 = COLOUR_RGB ( '', 0.66274510, 0.83137255, 0.94901961) ;
#33215 = CARTESIAN_POINT ( 'NONE',  ( -1.619566622897594232, -29.99999999999998579, -7.705259353042192672 ) ) ;
#33216 = ORIENTED_EDGE ( 'NONE', *, *, #79053, .F. ) ;
#33217 = DIRECTION ( 'NONE',  ( -1.000000000000000000, -1.224606353822377258E-16, -0.000000000000000000 ) ) ;
#33218 = DIRECTION ( 'NONE',  ( 0.000000000000000000, -1.000000000000000000, 0.000000000000000000 ) ) ;
#33219 = COLOUR_RGB ( '', 0.72549020, 0.75294118, 0.79215686) ;
#33220 = CARTESIAN_POINT ( 'NONE',  ( 0.000000000000000000, 16.00000000000000000, 0.000000000000000000 ) ) ;
#33221 = CARTESIAN_POINT ( 'NONE',  ( -97.10167131913696892, -30.00000000000000000, 191.0522010627015561 ) ) ;
#33222 = DIRECTION ( 'NONE',  ( -1.000000000000000000, -1.224606353822377258E-16, -0.000000000000000000 ) ) ;
#33223 = VECTOR ( 'NONE', #43365, 1000.000000000000000 ) ;
#33224 = CARTESIAN_POINT ( 'NONE',  ( 72.60991038965168798, -57.66267021765413148, 177.9523047781559910 ) ) ;
#33226 = CARTESIAN_POINT ( 'NONE',  ( -8.875443049772991699, 53.84837620808301750, 1.561318058200789505 ) ) ;
#33225 = CARTESIAN_POINT ( 'NONE',  ( 15.55105613542228404, -0.9527306383815096202, 14.97181131753247918 ) ) ;
#33227 = EDGE_CURVE ( 'NONE', #84887, #28086, #39450, .T. ) ;
#33228 = CARTESIAN_POINT ( 'NONE',  ( 14.67184194744775461, -23.97522478767837129, -38.53186082317327532 ) ) ;
#33229 = CARTESIAN_POINT ( 'NONE',  ( 0.000000000000000000, 0.000000000000000000, 0.000000000000000000 ) ) ;
#33230 = CARTESIAN_POINT ( 'NONE',  ( -40.96815392870907857, 488.3809129049190574, 10.59964723858178992 ) ) ;
#33231 = CARTESIAN_POINT ( 'NONE',  ( -46.99610915538814737, -59.99999999999999289, 64.77681108800881304 ) ) ;
#33232 = DIRECTION ( 'NONE',  ( 0.5735764363510466035, -0.8191520442889914655, 1.003171929053524500E-16 ) ) ;
#33233 = CARTESIAN_POINT ( 'NONE',  ( 0.1682126576532519957, 45.30391365246044444, -18.75000000000000711 ) ) ;
#33234 = CARTESIAN_POINT ( 'NONE',  ( -87.02199110510677826, -31.71018611468244686, 187.4638403878138604 ) ) ;
#33235 = ORIENTED_EDGE ( 'NONE', *, *, #70224, .F. ) ;
#33236 = CARTESIAN_POINT ( 'NONE',  ( 18.92590207683029035, 49.07586612980317398, 62.10725160223120866 ) ) ;
#33237 = CARTESIAN_POINT ( 'NONE',  ( 30.48515219902060736, 12.91670175270528098, 41.81704193310803674 ) ) ;
#33238 = CARTESIAN_POINT ( 'NONE',  ( -10.04926806037129161, -18.58639629729638543, 26.99593289150223185 ) ) ;
#33239 = CARTESIAN_POINT ( 'NONE',  ( 4.370690007832189750E-16, -5.309483803148808079, -3.803704290982246494 ) ) ;
#33240 = AXIS2_PLACEMENT_3D ( 'NONE', #66048, #100005, #42836 ) ;
#33243 = ADVANCED_FACE ( 'NONE', ( #74525, #602 ), #48120, .T. ) ;
#33242 = CARTESIAN_POINT ( 'NONE',  ( 4.177104036897216766, -67.05129264954501878, 13.14325999856157701 ) ) ;
#33241 = CARTESIAN_POINT ( 'NONE',  ( 5.727634848076907481, -4.575561887447414655, -6.326622577870443465 ) ) ;
#33244 = EDGE_LOOP ( 'NONE', ( #59175, #77767, #57504, #8477, #53504, #24754 ) ) ;
#33245 = CARTESIAN_POINT ( 'NONE',  ( 25.89618882946261991, 35.00184838547495048, 9.164364432303852226 ) ) ;
#33246 = STYLED_ITEM ( 'NONE', ( #86013 ), #92356 ) ;
#33247 = CARTESIAN_POINT ( 'NONE',  ( -7.499944090893143844, -3.043005460619030877, -20.23003913617138139 ) ) ;
#33248 = CARTESIAN_POINT ( 'NONE',  ( -7.151217271224854954, 31.78749400445714812, -3.587901469523285591 ) ) ;
#33249 = CARTESIAN_POINT ( 'NONE',  ( 30.86342090715118047, 298.3468162791613736, -1.228562068932849360 ) ) ;
#33250 = CARTESIAN_POINT ( 'NONE',  ( 4.999999999999993783, -46.00000000000000000, 102.2532056551910387 ) ) ;
#33251 = CARTESIAN_POINT ( 'NONE',  ( -7.414580834929599185, -82.35343719718518685, 3.010264818013836052 ) ) ;
#33252 = CARTESIAN_POINT ( 'NONE',  ( 107.9653405324804680, -30.00000000000002132, 188.7583403580863717 ) ) ;
#33253 = CARTESIAN_POINT ( 'NONE',  ( -35.76482652855951017, 405.2378813769876729, 6.148826621638260548 ) ) ;
#33254 = ORIENTED_EDGE ( 'NONE', *, *, #17686, .F. ) ;
#33255 = CARTESIAN_POINT ( 'NONE',  ( 40.02592568779148507, -5.000000000000000888, 6.123233995736769241E-16 ) ) ;
#33256 = CARTESIAN_POINT ( 'NONE',  ( 10.11650669486618881, 1.474610560812782335E-15, 0.000000000000000000 ) ) ;
#33257 = DIRECTION ( 'NONE',  ( 0.000000000000000000, -0.000000000000000000, 1.000000000000000000 ) ) ;
#33258 = CARTESIAN_POINT ( 'NONE',  ( -6.602753909532903087, -5.319290460493550476, -7.792447862505339273 ) ) ;
#33259 = DIRECTION ( 'NONE',  ( -1.000000000000000000, -0.000000000000000000, -0.000000000000000000 ) ) ;
#33260 = EDGE_CURVE ( 'NONE', #92310, #83331, #92858, .T. ) ;
#33261 = CARTESIAN_POINT ( 'NONE',  ( 17.23461538461538467, -4.171999999999999709, 5.616230220889763424E-16 ) ) ;
#33262 = ORIENTED_EDGE ( 'NONE', *, *, #92928, .T. ) ;
#33263 = UNCERTAINTY_MEASURE_WITH_UNIT (LENGTH_MEASURE( 1.000000000000000082E-05 ), #48945, 'distance_accuracy_value', 'NONE');
#33264 = CARTESIAN_POINT ( 'NONE',  ( -22.15956248098668269, 304.2723657570961677, 10.02744636126657163 ) ) ;
#33265 = VERTEX_POINT ( 'NONE', #56195 ) ;
#33266 = CARTESIAN_POINT ( 'NONE',  ( 38.23234611763021462, 485.0120663942624333, -3.939776079184425406 ) ) ;
#33268 = EDGE_CURVE ( 'NONE', #85394, #11109, #30843, .T. ) ;
#33267 = FILL_AREA_STYLE_COLOUR ( '', #98028 ) ;
#33269 = CARTESIAN_POINT ( 'NONE',  ( 10.12028333941264080, 45.42143084255511809, 15.39942097377729446 ) ) ;
#33270 = ORIENTED_EDGE ( 'NONE', *, *, #12358, .T. ) ;
#33271 = PRESENTATION_STYLE_ASSIGNMENT (( #105539 ) ) ;
#33272 = B_SPLINE_CURVE_WITH_KNOTS ( 'NONE', 3,
 ( #40828, #51034, #83412, #25766, #9510, #8460, #83947, #90449, #57002, #67250, #49444, #89916, #99590, #81798, #58624, #90994, #33294, #10059, #16560, #75316, #25215, #98004, #1414, #41361, #18173, #17640, #17104, #33835, #74254, #82888 ),
 .UNSPECIFIED., .F., .F.,
 ( 4, 2, 2, 2, 2, 2, 2, 2, 2, 2, 2, 2, 2, 2, 4 ),
 ( 0.004754800762794653829, 0.005690253947496240472, 0.006157980539847035528, 0.006625707132197830584, 0.006859570428373221174, 0.007093433724548612630, 0.007327297020724004087, 0.007561160316899394676, 0.007795023613074785265, 0.008028886909250175855, 0.008496613501600955298, 0.009432066686302517655, 0.01036751987100408001, 0.01130297305570564584, 0.01223842624040720820 ),
 .UNSPECIFIED. ) ;
#33273 = CARTESIAN_POINT ( 'NONE',  ( 6.187404903406283019, -12.10572765818970709, 11.71902858905958134 ) ) ;
#33274 = CARTESIAN_POINT ( 'NONE',  ( -70.09088371448167720, -59.99999999994136601, 157.7190277870289492 ) ) ;
#33275 = DIRECTION ( 'NONE',  ( -1.000000000000000000, 0.000000000000000000, 0.000000000000000000 ) ) ;
#33276 = ORIENTED_EDGE ( 'NONE', *, *, #30370, .F. ) ;
#33277 = CARTESIAN_POINT ( 'NONE',  ( 111.6827242965483151, -59.99999999999997868, 183.1303449405941706 ) ) ;
#33279 = CARTESIAN_POINT ( 'NONE',  ( 19.40890743283955899, -56.87623265366909919, 33.84337721544303434 ) ) ;
#33278 = CARTESIAN_POINT ( 'NONE',  ( -106.8727010878311745, -14.21045842199433373, 167.8788319932906461 ) ) ;
#33280 = CARTESIAN_POINT ( 'NONE',  ( 1.128592495958797404, 53.60018988584262445, -9.630884289430918344 ) ) ;
#33281 = CARTESIAN_POINT ( 'NONE',  ( -43.41331196749857924, -18.78938622932218649, 36.60976053377660833 ) ) ;
#33282 = CARTESIAN_POINT ( 'NONE',  ( -16.68184208835464233, 18.64284798593346082, -34.62135284426452131 ) ) ;
#33283 = ORIENTED_EDGE ( 'NONE', *, *, #71779, .F. ) ;
#33284 = FACE_OUTER_BOUND ( 'NONE', #41132, .T. ) ;
#33285 = CARTESIAN_POINT ( 'NONE',  ( 27.97565635352651015, 315.9216507687758053, 12.64980990155120999 ) ) ;
#33286 = CIRCLE ( 'NONE', #93565, 4.000000000000001776 ) ;
#33287 = SURFACE_SIDE_STYLE ('',( #323 ) ) ;
#33288 = CARTESIAN_POINT ( 'NONE',  ( 6.289572920342625828, 5.584521518880460889, 3.985288806461539046 ) ) ;
#33289 = CARTESIAN_POINT ( 'NONE',  ( -33.00000000000000000, 463.5362553048592531, 6.739467187734380360 ) ) ;
#33290 = ORIENTED_EDGE ( 'NONE', *, *, #32645, .T. ) ;
#33291 = CARTESIAN_POINT ( 'NONE',  ( 5.603804764709609643, -47.29776092513240826, 103.9691152301460022 ) ) ;
#33292 = ORIENTED_EDGE ( 'NONE', *, *, #84657, .T. ) ;
#33293 = CARTESIAN_POINT ( 'NONE',  ( 81.37391084052052292, -30.00000000000006040, -10.28767919861631164 ) ) ;
#33294 = CARTESIAN_POINT ( 'NONE',  ( 46.78712017075152829, 13.65728975790556454, 15.44288672244329419 ) ) ;
#33295 = VECTOR ( 'NONE', #7711, 1000.000000000000000 ) ;
#33296 = UNCERTAINTY_MEASURE_WITH_UNIT (LENGTH_MEASURE( 1.000000000000000082E-05 ), #73148, 'distance_accuracy_value', 'NONE');
#33297 = EDGE_CURVE ( 'NONE', #96464, #65523, #91109, .T. ) ;
#33298 = CARTESIAN_POINT ( 'NONE',  ( 24.29736616268256100, 25.57611167045289591, -31.30689180755234702 ) ) ;
#33299 = CARTESIAN_POINT ( 'NONE',  ( 40.92692307692308162, 1.411358822780289120E-15, 0.000000000000000000 ) ) ;
#33300 = CARTESIAN_POINT ( 'NONE',  ( 90.42490069223487126, -30.00000000000000000, 90.97836846167180624 ) ) ;
#33301 = COLOUR_RGB ( '', 0.66274510, 0.83137255, 0.94901961) ;
#33302 = DIRECTION ( 'NONE',  ( 0.000000000000000000, -1.000000000000000000, 0.000000000000000000 ) ) ;
#33303 = ORIENTED_EDGE ( 'NONE', *, *, #62580, .F. ) ;
#33304 = B_SPLINE_CURVE_WITH_KNOTS ( 'NONE', 3,
 ( #34716, #99935, #10909, #2289 ),
 .UNSPECIFIED., .F., .F.,
 ( 4, 4 ),
 ( 1.734723475976807094E-18, 0.001632242847434939390 ),
 .UNSPECIFIED. ) ;
#33305 = ORIENTED_EDGE ( 'NONE', *, *, #32994, .T. ) ;
#33306 = ORIENTED_EDGE ( 'NONE', *, *, #8991, .F. ) ;
#33307 = DIRECTION ( 'NONE',  ( 0.000000000000000000, 0.000000000000000000, 1.000000000000000000 ) ) ;
#33308 = CARTESIAN_POINT ( 'NONE',  ( -6.931098304924008247, -13.59560219465957154, -6.365424046575419048 ) ) ;
#33309 = VECTOR ( 'NONE', #17129, 1000.000000000000227 ) ;
#33310 = CARTESIAN_POINT ( 'NONE',  ( -41.74718156901468546, 464.4924520314310712, 17.10319308832293572 ) ) ;
#33311 = CARTESIAN_POINT ( 'NONE',  ( -31.35087655471889434, 439.7415908874936576, 22.35622233947958648 ) ) ;
#33312 = DIRECTION ( 'NONE',  ( -1.000000000000000000, -1.224606353822377258E-16, -0.000000000000000000 ) ) ;
#33313 = ORIENTED_EDGE ( 'NONE', *, *, #106495, .F. ) ;
#33314 = CARTESIAN_POINT ( 'NONE',  ( 9.334514330295428763, 106.7862273768178625, -3.588704711590612106 ) ) ;
#33315 = VERTEX_POINT ( 'NONE', #10324 ) ;
#33316 = CARTESIAN_POINT ( 'NONE',  ( -4.250000000000000000, 5.204748896376250699E-16, -10.00000000000000000 ) ) ;
#33317 = CARTESIAN_POINT ( 'NONE',  ( 77.69612501048428044, -38.53685538454406156, 187.1913476843784281 ) ) ;
#33318 = DIRECTION ( 'NONE',  ( 0.000000000000000000, -0.3420201433256733758, -0.9396926207859066515 ) ) ;
#33319 = CARTESIAN_POINT ( 'NONE',  ( 33.64205033492135044, 302.6176840280941178, 11.72452048251792078 ) ) ;
#33320 = CARTESIAN_POINT ( 'NONE',  ( 7.409113134841487507E-15, 49.50000000000000000, -60.50000000000000000 ) ) ;
#33321 = DIRECTION ( 'NONE',  ( -0.000000000000000000, -0.000000000000000000, -1.000000000000000000 ) ) ;
#33322 = CIRCLE ( 'NONE', #47298, 60.00000000000000000 ) ;
#33323 = DIRECTION ( 'NONE',  ( 0.000000000000000000, 0.000000000000000000, -1.000000000000000000 ) ) ;
#33324 = CARTESIAN_POINT ( 'NONE',  ( 42.71746488131647368, 428.6810652414584979, 19.02199747807395624 ) ) ;
#33325 = AXIS2_PLACEMENT_3D ( 'NONE', #44991, #70317, #54623 ) ;
#33326 = EDGE_CURVE ( 'NONE', #83184, #39611, #46356, .T. ) ;
#33327 = LINE ( 'NONE', #96461, #104852 ) ;
#33328 = SURFACE_SIDE_STYLE ('',( #82917 ) ) ;
#33330 = ORIENTED_EDGE ( 'NONE', *, *, #87196, .F. ) ;
#33329 = STYLED_ITEM ( 'NONE', ( #3846 ), #18983 ) ;
#33332 = CARTESIAN_POINT ( 'NONE',  ( -25.79311565262062089, 295.8993310619729868, 2.162649885535623540 ) ) ;
#33331 = DIRECTION ( 'NONE',  ( -1.000000000000000000, -0.000000000000000000, -0.000000000000000000 ) ) ;
#33333 = DIRECTION ( 'NONE',  ( -0.000000000000000000, -0.000000000000000000, 1.000000000000000000 ) ) ;
#33334 = UNCERTAINTY_MEASURE_WITH_UNIT (LENGTH_MEASURE( 1.000000000000000082E-05 ), #92893, 'distance_accuracy_value', 'NONE');
#33335 = SURFACE_SIDE_STYLE ('',( #11137 ) ) ;
#33336 = CARTESIAN_POINT ( 'NONE',  ( 5.656854249492378806, -11.18749999999999289, 5.656854249492381470 ) ) ;
#33337 = AXIS2_PLACEMENT_3D ( 'NONE', #94339, #43644, #93799 ) ;
#33338 = CARTESIAN_POINT ( 'NONE',  ( 39.35377274615763099, -37.46504824054412808, 48.92861146246112014 ) ) ;
#33339 = ADVANCED_FACE ( 'NONE', ( #68038 ), #68592, .T. ) ;
#33340 = CARTESIAN_POINT ( 'NONE',  ( -6.928203230275508773, 105.0000000000000000, 4.000000000000001776 ) ) ;
#33341 = DIRECTION ( 'NONE',  ( -1.000000000000000000, 0.000000000000000000, 0.000000000000000000 ) ) ;
#33342 = CARTESIAN_POINT ( 'NONE',  ( 86.09503755511013878, -28.33328412234302718, 182.5637252326066289 ) ) ;
#33343 = CARTESIAN_POINT ( 'NONE',  ( 82.70911704725124025, 1.016364837396684119E-14, 0.000000000000000000 ) ) ;
#33344 = EDGE_LOOP ( 'NONE', ( #50057, #97357, #227 ) ) ;
#33345 = CARTESIAN_POINT ( 'NONE',  ( 93.06064234306185767, -57.65576527925703232, -17.06971926439956277 ) ) ;
#33346 = DIRECTION ( 'NONE',  ( -0.000000000000000000, -1.000000000000000000, -0.000000000000000000 ) ) ;
#33347 = FILL_AREA_STYLE_COLOUR ( '', #42395 ) ;
#33348 = CARTESIAN_POINT ( 'NONE',  ( -81.03088382936273604, -30.00000000000000000, 21.51870931205188953 ) ) ;
#33349 = EDGE_CURVE ( 'NONE', #78599, #45114, #84230, .T. ) ;
#33350 = CARTESIAN_POINT ( 'NONE',  ( -83.15876612675486967, -37.99999999999995737, 169.0493242017684281 ) ) ;
#33351 = DIRECTION ( 'NONE',  ( -0.5735764363510497121, 0.8191520442889892450, 1.003171929053521665E-16 ) ) ;
#33352 = CARTESIAN_POINT ( 'NONE',  ( -6.486836893983013219, 4.915077010914094657, -7.231838333420560261 ) ) ;
#33354 = FACE_OUTER_BOUND ( 'NONE', #97836, .T. ) ;
#33353 = DIRECTION ( 'NONE',  ( -1.000000000000000000, -1.224606353822377258E-16, -0.000000000000000000 ) ) ;
#33355 = ADVANCED_FACE ( 'NONE', ( #100934 ), #11849, .T. ) ;
#33356 = FACE_OUTER_BOUND ( 'NONE', #26176, .T. ) ;
#33357 = CARTESIAN_POINT ( 'NONE',  ( -29.33036678664092278, 18.69950024370077202, 39.65481841613247838 ) ) ;
#33358 = CARTESIAN_POINT ( 'NONE',  ( -12.49999999999999822, -4.999999999999999112, -11.21398294031200393 ) ) ;
#33359 = CARTESIAN_POINT ( 'NONE',  ( 5.999511540169428336, -81.00073269114568575, -0.2833228702578375335 ) ) ;
#33360 = CARTESIAN_POINT ( 'NONE',  ( -22.00819901261985123, 25.77094897315768662, 32.31068855013590735 ) ) ;
#33361 = FACE_OUTER_BOUND ( 'NONE', #34617, .T. ) ;
#33362 = TOROIDAL_SURFACE ( 'NONE', #26454, 3.500000000000000000, 0.5000000000000000000 ) ;
#33363 = CARTESIAN_POINT ( 'NONE',  ( -99.26691377649297010, -38.00000000000004974, 191.6702388746358849 ) ) ;
#33364 = AXIS2_PLACEMENT_3D ( 'NONE', #28491, #11722, #45195 ) ;
#33365 = VERTEX_POINT ( 'NONE', #76125 ) ;
#33366 = CARTESIAN_POINT ( 'NONE',  ( 6.996281870428059158, 9.006495247806538984, 0.2643931112039918929 ) ) ;
#33367 = CARTESIAN_POINT ( 'NONE',  ( 32.62207953394533178, -5.000000000000000888, 6.123233995736769241E-16 ) ) ;
#33368 = CARTESIAN_POINT ( 'NONE',  ( -53.90143474190011830, -28.29133745413889756, -26.90304354338606174 ) ) ;
#33371 = ADVANCED_FACE ( 'NONE', ( #10842 ), #25696, .T. ) ;
#33370 = DIRECTION ( 'NONE',  ( -1.000000000000000000, -1.224606353822377258E-16, -0.000000000000000000 ) ) ;
#33369 = LINE ( 'NONE', #9056, #48433 ) ;
#33372 = ORIENTED_EDGE ( 'NONE', *, *, #17580, .T. ) ;
#33373 = DIRECTION ( 'NONE',  ( 0.000000000000000000, 0.000000000000000000, 1.000000000000000000 ) ) ;
#33374 = ORIENTED_EDGE ( 'NONE', *, *, #73816, .T. ) ;
#33375 = LINE ( 'NONE', #91079, #17296 ) ;
#33376 = CARTESIAN_POINT ( 'NONE',  ( 11.04658362184419218, 43.74827273734751998, -13.15312417557731628 ) ) ;
#33377 = CARTESIAN_POINT ( 'NONE',  ( -55.01636684413512768, -59.99999999999999289, -36.85708210959909792 ) ) ;
#33378 = EDGE_LOOP ( 'NONE', ( #89416, #66032, #106020, #64226, #90462 ) ) ;
#33379 = CARTESIAN_POINT ( 'NONE',  ( 2.499999999999984457, -21.99834388059804269, -30.53959902372158908 ) ) ;
#33380 = CARTESIAN_POINT ( 'NONE',  ( 15.05785784214677392, 3.824195276769925655, -4.604276673498363337 ) ) ;
#33381 = CARTESIAN_POINT ( 'NONE',  ( 102.6319757891835707, -60.18047993876283641, 193.3962675965070730 ) ) ;
#33383 = CARTESIAN_POINT ( 'NONE',  ( -46.77767549600498853, 13.52659353100013995, 15.64517449361655466 ) ) ;
#33382 = CARTESIAN_POINT ( 'NONE',  ( 21.93725470949543421, -26.33177549557095176, 28.96246740876147641 ) ) ;
#33384 = ORIENTED_EDGE ( 'NONE', *, *, #54369, .T. ) ;
#33385 = CIRCLE ( 'NONE', #57445, 15.00000000000001421 ) ;
#33386 = ORIENTED_EDGE ( 'NONE', *, *, #41183, .F. ) ;
#33387 = ORIENTED_EDGE ( 'NONE', *, *, #77992, .T. ) ;
#33388 = CARTESIAN_POINT ( 'NONE',  ( 31.21596591978341095, 336.6249549339077021, 17.82539080634884243 ) ) ;
#33389 = CIRCLE ( 'NONE', #33325, 3.309500000000001663 ) ;
#33390 = EDGE_CURVE ( 'NONE', #49420, #104803, #17385, .T. ) ;
#33391 = CARTESIAN_POINT ( 'NONE',  ( -5.000000000000000000, -14.08559933050952928, 11.75736354680345741 ) ) ;
#33392 = CARTESIAN_POINT ( 'NONE',  ( 8.880600455183216724, 53.58356968164088840, 4.000111768521608546 ) ) ;
#33393 = ORIENTED_EDGE ( 'NONE', *, *, #47214, .F. ) ;
#33394 =( GEOMETRIC_REPRESENTATION_CONTEXT ( 3 ) GLOBAL_UNCERTAINTY_ASSIGNED_CONTEXT ( ( #314 ) ) GLOBAL_UNIT_ASSIGNED_CONTEXT ( ( #86417, #52410, #93958 ) ) REPRESENTATION_CONTEXT ( 'NONE', 'WORKASPACE' ) );
#33395 = DIRECTION ( 'NONE',  ( -1.000000000000000000, 0.000000000000000000, 0.000000000000000000 ) ) ;
#33396 = CARTESIAN_POINT ( 'NONE',  ( 8.099999999999999645, -7.505553499465142053, -3.129864801432410934E-16 ) ) ;
#33397 = AXIS2_PLACEMENT_3D ( 'NONE', #89554, #80915, #48007 ) ;
#33398 = LINE ( 'NONE', #91100, #4834 ) ;
#33399 = CARTESIAN_POINT ( 'NONE',  ( -41.14701979708251400, -57.68941641447864299, 57.58229189354211286 ) ) ;
#33400 = CARTESIAN_POINT ( 'NONE',  ( 2.977408999572651815, -32.93750000204839523, 7.188101187500000933 ) ) ;
#33401 = CARTESIAN_POINT ( 'NONE',  ( -30.64177940627137531, 12.99790429510468570, 41.66010176663436937 ) ) ;
#33402 = AXIS2_PLACEMENT_3D ( 'NONE', #35741, #93946, #86926 ) ;
#33403 = CARTESIAN_POINT ( 'NONE',  ( 6.123233995736763324E-16, 48.00000000000000000, -75.00000000000001421 ) ) ;
#33404 = CARTESIAN_POINT ( 'NONE',  ( -6.738100187484505454, 41.71798639774085160, -59.05424569925489209 ) ) ;
#33405 = CARTESIAN_POINT ( 'NONE',  ( 2.851859124854637884, -60.00000000000000711, -45.00000000000000711 ) ) ;
#33406 = ADVANCED_FACE ( 'NONE', ( #100403 ), #85966, .F. ) ;
#33407 = CARTESIAN_POINT ( 'NONE',  ( -28.84153870763153904, -30.00000000000004619, 39.52238898731670247 ) ) ;
#33408 = CARTESIAN_POINT ( 'NONE',  ( -49.86947586418430234, -25.66521200955699555, 46.00621269778669387 ) ) ;
#33409 = CARTESIAN_POINT ( 'NONE',  ( 2.024297636968084735, 21.31243181164073874, -6.704763639156325006 ) ) ;
#33410 = ORIENTED_EDGE ( 'NONE', *, *, #57348, .F. ) ;
#33411 = CARTESIAN_POINT ( 'NONE',  ( -98.41647369420755354, -52.79632805706295784, 194.9882854070544340 ) ) ;
#33412 = CARTESIAN_POINT ( 'NONE',  ( 12.03234183921365563, 2.057523246211587775, 14.86059839350262912 ) ) ;
#33413 = ORIENTED_EDGE ( 'NONE', *, *, #53109, .T. ) ;
#33414 = CARTESIAN_POINT ( 'NONE',  ( -16.80382109351738862, 43.42138402310583700, 6.657797401561657225 ) ) ;
#33415 = CARTESIAN_POINT ( 'NONE',  ( 86.46411780683014570, -38.61740881457028962, 199.3064231678986005 ) ) ;
#33416 = CARTESIAN_POINT ( 'NONE',  ( 28.86650669486618881, 0.000000000000000000, 4.000000000000000888 ) ) ;
#33417 = CARTESIAN_POINT ( 'NONE',  ( -5.855287526011301757, 51.27353136529828959, -8.399225406922926851 ) ) ;
#33418 = ADVANCED_FACE ( 'NONE', ( #11378 ), #84246, .T. ) ;
#33419 = CARTESIAN_POINT ( 'NONE',  ( -19.96162532426518865, 302.8116070918645164, 9.928455558879852205 ) ) ;
#33420 = CARTESIAN_POINT ( 'NONE',  ( 45.60838156035057978, 42.00000000000004263, -79.13121736032620390 ) ) ;
#33421 = CARTESIAN_POINT ( 'NONE',  ( 85.94206644272870221, -30.00000000000000711, 178.2002489271057470 ) ) ;
#33422 = B_SPLINE_SURFACE_WITH_KNOTS ( 'NONE', 3, 3, ( 
 ( #40, #30893, #23319, #105799, #82047, #33012, #73959, #73420, #97699, #48084, #56158, #98242, #31938 ),
 ( #65879, #47026, #48615, #98758, #106315, #80985, #32479, #80454, #49144, #8169, #41075, #64820, #24397 ),
 ( #57236, #7101, #23863, #89630, #71836, #88045, #39499, #6565, #14125, #79928, #6037, #104742, #38962 ),
 ( #63773, #96661, #22796, #55631, #88568, #14649, #72373, #105279, #90694, #99835, #83125, #41607, #59403 ),
 ( #85671, #82594, #61397, #37139, #25465, #66956, #19906, #69481, #42665, #11746, #102366, #28514, #75014 ),
 ( #34618, #12286, #24912, #42128, #1108, #53293, #9749, #50733, #44682, #8699, #16802, #78091, #26007 ),
 ( #94286, #34084, #91760, #20453, #58870, #26530, #17350, #77569, #57766, #50224, #49688, #74490, #86214 ),
 ( #45216, #17879, #9220, #67487, #75564, #83643, #3685, #100366, #1659, #99288, #4209, #92264, #52748 ),
 ( #36616, #70005, #565, #33533, #66405, #58317, #91242, #78609, #87789, #13337, #103432, #47825, #4740 ),
 ( #46787, #23064, #80729, #14933, #22548, #38712, #30097, #38201, #6305, #13872, #55390, #6847, #94829 ),
 ( #20976, #29582, #88319, #62453, #95345, #46264, #21480, #39772, #79680, #63519, #80201, #70541, #47305 ),
 ( #12813, #5275, #87262, #54316, #29070, #71060, #22006, #45728, #103952, #39245, #37680, #5790, #54860 ),
 ( #64054, #62981, #79149, #72120, #61939, #95882, #71577, #104483, #30630, #96417, #14393, #53809, #31170 ),
 ( #105029, #96929, #55903, #88839, #102905, #86739, #8967, #74760, #16009, #82332, #8442, #58604, #72646 ),
 ( #89898, #99570, #57511, #98510, #90974, #56448, #64572, #17621, #40808, #17085, #33813, #49962, #81257 ),
 ( #73702, #66689, #7371, #56983, #7902, #32211, #97986, #32754, #91507, #82870, #49428, #23600, #25749 ),
 ( #40282, #81779, #106060, #50482, #58052, #24659, #83394, #48365, #48885, #65089, #9491, #106604, #105548 ),
 ( #66149, #65628, #31686, #313, #73159, #24140, #90434, #16538, #15471, #97439, #89381, #41343, #99031 ),
 ( #74236, #33279, #25195, #41872, #840, #10566, #68835, #59138, #26801, #28395, #43482, #92020, #75298 ),
 ( #59672, #51013, #27881, #44012, #61268, #60223, #85002, #52618, #85546, #19263, #35965, #1391, #60746 ),
 ( #93091, #92553, #10040, #34358, #67233, #76358, #18701, #42947, #36496, #83929, #20328, #75838, #101185 ),
 ( #2471, #93634, #67754, #69364, #102243, #94158, #52091, #101714, #3013, #19785, #35419, #68290, #27346 ),
 ( #51557, #84471, #100641, #100111, #11086, #76900, #18156, #11626, #44556, #1936, #77443, #3558, #53173 ),
 ( #34887, #86090, #42403, #26276, #79558, #61817, #5672, #96299, #70421, #62336, #30505, #31049, #95231 ),
 ( #38084, #14280, #46146, #29465, #12688, #96816, #95751, #38591, #22423, #86625, #63405, #78492, #80079 ),
 ( #63929, #87670, #71458, #77972, #4089, #29978, #45093, #39121, #103317, #94710, #22948, #13218, #6187 ),
 ( #20859, #70941, #28943, #103833, #104357, #53692, #55268, #88194, #21362, #54202, #47178, #55783, #87141 ),
 ( #62866, #71999, #79032, #45620, #5151, #21893, #4623, #37553, #54734, #104911, #12162, #13749, #69885 ),
 ( #37017, #46660, #102781, #15350, #8844, #74103, #7778, #82740, #64452, #73034, #48235, #49836, #56859 ),
 ( #97325, #82198, #24016, #99438, #16412, #56315, #89252, #40683, #40158, #31571, #41749, #66557, #65503 ),
 ( #106472, #32089, #49292, #23478, #74637, #8314, #89780, #41217, #105431, #105944, #715, #15884, #81139 ),
 ( #48760, #81653, #90303, #66026, #193, #33157, #7248, #73570, #64966, #97858, #33685, #32630, #98392 ),
 ( #25615, #88720, #14811, #98904, #24541, #57391, #25064, #57922, #90842, #16959, #47707, #80606, #6730 ),
 ( #39653, #72524, #76771, #83794, #75166, #100515, #35831, #1259, #43354, #10438, #68156, #19660, #67637 ),
 ( #2874, #17498, #26670, #9906, #34226, #92961, #84345, #10960, #9361, #93512, #69239, #59010, #59549 ),
 ( #101592, #76238, #43876, #27748, #60622, #1804, #101051, #27207, #44420, #58475, #75710, #34763, #85411 ),
 ( #2347, #68711, #42275, #50359, #3428, #92416, #52491, #11493, #77315, #67099, #91380, #18569, #36371 ),
 ( #51431, #102111, #19121, #26154, #91899, #35286, #42814, #99982, #83272, #18024, #60096, #51959, #84875 ),
 ( #50888, #36891, #22292, #62733, #103188, #54598, #44964, #12561, #14147, #29332, #77846, #61139, #12036 ),
 ( #69758, #13620, #29855, #47050, #46016, #70816, #38467, #71334, #5023, #21763, #94028, #46535, #28270 ),
 ( #45498, #102653, #20189, #53043, #62222, #78366, #28811, #55138, #61692, #6060, #94583, #87015, #85962 ),
 ( #79428, #53569, #88068, #79950, #38987, #37956, #87539, #95621, #5541, #95106, #21241, #54074, #3960 ),
 ( #4489, #86500, #20731, #37425, #13087, #104227, #78897, #30375, #70291, #71861, #103708, #63265, #96160 ),
 ( #65375, #90179, #31962, #64841, #72912, #14672, #7122, #89122, #23342, #30916, #40037, #23886, #47580 ),
 ( #82073, #80475, #89653, #56731, #7645, #65900, #105821, #56183, #49165, #63797, #97721, #15221, #6591 ),
 ( #15753, #57257, #55655, #33034, #8721, #105302, #48636, #98266, #41100, #81521, #16282, #73981, #63 ),
 ( #40561, #73444, #90717, #104767, #48106, #81007, #24939, #106339, #32502, #8190, #88592, #96683, #49712 ),
 ( #98783, #57790, #16827, #39522, #22821, #24421, #82619, #41629, #72397, #31446, #64327, #97198, #66978 ),
 ( #74513, #99859, #66427, #91261, #2751, #10829, #43750, #91782, #58890, #10311, #92286, #26552, #59967 ),
 ( #67508, #42152, #35703, #51297, #50756, #68581, #26031, #9774, #42689, #76112, #51834, #68026, #27082 ),
 ( #59423, #17903, #75035, #19529, #50245, #75585, #18441, #101464, #52366, #93379, #100918, #43228, #1684 ),
 ( #84216, #92828, #85277, #99311, #18991, #11364, #2210, #60497, #35160, #84748, #76642, #27617, #590 ),
 ( #33555, #25483, #58339, #17372, #83663, #1133, #83147, #9244, #34640, #100390, #34107, #38346, #85833 ),
 ( #52911, #103063, #69110, #44838, #103580, #77724, #3835, #61555, #36768, #22156, #21121, #4896, #21634 ),
 ( #95490, #69634, #5421, #94452, #63130, #12960, #29731, #3297, #36241, #62091, #77186, #71206, #102526 ),
 ( #55006, #45361, #104101, #28670, #93906, #70158, #61019, #29218, #37828, #20061, #70691, #54465, #20607 ),
 ( #62604, #96030, #53446, #87416, #94983, #46414, #78243, #11908, #86367, #12432, #4356, #37292, #53952 ),
 ( #13492, #86887, #101983, #30242, #28142, #45882, #78762, #79301, #87938, #44291, #39912, #8055, #96561 ),
 ( #47453, #81936, #88992, #40969, #22694, #7514, #56055, #24807, #48509, #88470, #14544, #72785, #72270 ),
 ( #73857, #98656, #97585, #40432, #31832, #64202, #81402, #55531, #106751, #73311, #15090, #106206, #30787 ),
 ( #32901, #47977, #63671, #46926, #104635, #31320, #80346, #32370, #97071, #65243, #6460, #65776, #98134 ),
 ( #6994, #39394, #49039, #23755, #23217, #57659, #105174, #80883, #105691, #15620, #24285, #57134, #90045 ),
 ( #64715, #56603, #89526, #14019, #16151, #79825, #5931, #38858, #71723, #2622, #10185, #26425, #17770 ),
 ( #100787, #1548, #43098, #101337, #82490, #84083, #27491, #75986, #50624, #2083, #9114, #84622, #10706 ),
 ( #67380, #51163, #67900, #58208, #35036, #50115, #51703, #33970, #35570, #59290, #26949, #49581, #8590 ),
 ( #16690, #43621, #42024, #33429, #68443, #91654, #76514, #91133, #66302, #9642, #459, #42550, #59825 ),
 ( #92701, #18860, #74907, #66843, #90582, #41493, #99733, #74380, #75453, #99183, #83541, #25345, #991 ),
 ( #83022, #25902, #34512, #17243, #58759, #100261, #92164, #18311, #19405, #68983, #44706, #101858, #78630 ),
 ( #102393, #45753, #77052, #19935, #28017, #4763, #77593, #37704, #3168, #4231, #3713, #29605, #78115 ),
 ( #36113, #61423, #52777, #44164, #70569, #103454, #20479, #37166, #94316, #61962, #11238, #53319, #86237 ),
 ( #62477, #36640, #93776, #29094, #93241, #69506, #85696, #60887, #70027, #28543, #102927, #85146, #86767 ),
 ( #94853, #12311, #12834, #45238, #11774, #20997, #53834, #60366, #52238, #106231, #40452, #56072, #72804 ),
 ( #32391, #97093, #31340, #23776, #96050, #104119, #57154, #80369, #56623, #73332, #89545, #14039, #5440 ),
 ( #65263, #88489, #72288, #98152, #14565, #7015, #104655, #64734, #38362, #30807, #30264, #22178, #24308 ),
 ( #81422, #22714, #96580, #47998, #23235, #64222, #97611, #80904, #105194, #79846, #90067, #89015, #47473 ),
 ( #63692, #6483, #39413, #39932, #15638, #105712, #48530, #87960, #15110, #55552, #5952, #16174, #46945 ),
 ( #31853, #49059, #71226, #63153, #7535, #55027, #38877, #71746, #92180, #99752, #1567, #94203, #73876 ),
 ( #20372, #34529, #9133, #100281, #479, #77488, #3602, #36537, #91674, #67402, #42574, #26442, #42045 ),
 ( #43116, #25369, #102285, #50640, #59309, #40986, #106771, #25922, #8081, #69403, #81955, #9660, #49601 ),
 ( #33995, #33448, #24826, #28432, #61315, #58779, #75473, #17790, #58226, #18330, #90602, #32920, #51185 ),
 ( #84104, #98672, #66321, #65797, #83041, #57679, #16713, #82509, #99204, #8611, #10203, #83561, #41514 ),
 ( #66864, #91154, #74399, #17261, #50133, #74927, #1011, #80120, #31092, #72042, #79597, #95798, #87180 ),
 ( #63443, #70980, #5708, #63970, #45135, #46701, #96858, #38633, #13260, #71497, #78534, #47219, #6225 ),
 ( #62902, #104397, #13788, #30546, #46181, #79073, #21399, #69928, #62379, #37597, #4664, #86133, #95270 ),
 ( #102826, #54237, #96339, #28988, #38124, #5192, #21928, #14316, #103867, #70461, #22464, #12206, #30017 ),
 ( #61855, #87708, #54778, #55308, #4129, #88236, #53213, #53734, #39161, #104951, #78014, #37059, #94751 ),
 ( #20900, #103358, #86663, #12732, #45655, #29505, #90345, #40195, #49879, #7817, #48803, #41261, #6770 ),
 ( #74674, #97899, #74148, #90887, #232, #31608, #22985, #24055, #17002, #105980, #89822, #89296, #82784 ),
 ( #41791, #98431, #82244, #88757, #14854, #40726, #55820, #8886, #81178, #72565, #756, #56895, #33723 ),
 ( #105468, #81692, #39689, #73613, #16450, #64492, #49338, #33196, #7289, #73071, #66068, #66602, #32130 ),
 ( #106517, #25106, #15926, #97362, #65009, #32674, #15391, #48277, #65542, #47747, #24581, #80646, #57424 ),
 ( #23522, #8359, #56360, #98945, #57965, #18612, #93550, #75209, #83842, #26194, #60663, #67673, #19698 ),
 ( #93004, #34805, #3468, #27253, #67142, #100023, #51473, #50928, #42317, #52532, #77356, #76280, #19166 ),
 ( #42857, #60139, #1305, #85451, #52002, #100554, #84918, #9400, #9951, #11536, #26716, #34265, #25657 ),
 ( #75751, #59053, #11004, #101095, #44461, #10477, #35334, #2918, #35874, #2388, #43921, #58520, #76809 ),
 ( #43397, #1847, #91937, #91424, #17538, #59588, #92460, #18070, #36411, #84389, #99481, #68195, #68752 ),
 ( #101634, #27789, #50398, #83311, #86537, #69796, #47089, #46052, #29888, #46571, #36930, #13661, #78937 ),
 ( #62773, #54640, #103225, #29369, #37465, #86003, #78408, #53603, #94622, #102156, #4520, #95143, #12075 ),
 ( #79465, #45004, #54112, #21275, #5058, #30412, #70328, #20767, #5577, #28306, #62257, #12597, #77890 ),
 ( #87054, #21800, #20235, #104268, #79989, #102691, #13125, #95662, #38503, #37994, #87575, #71368, #63305 ),
 ( #70855, #96202, #22330, #103746, #55177, #45533, #88103, #14185, #6100, #69281, #53082, #61181, #94068 ),
 ( #4001, #28855, #61729, #102, #7159, #33071, #47615, #32539, #81046, #49749, #73479, #6635, #39561 ),
 ( #97238, #88626, #98820, #16870, #15792, #65411, #56767, #89159, #106378, #80516, #65939, #98306, #40071 ),
 ( #55695, #23383, #24975, #72950, #14715, #71907, #22858, #56220, #72436, #24459, #40597, #57826, #89692 ),
 ( #49208, #82107, #48673, #57295, #104808, #90215, #39024, #81557, #15263, #105338, #30957, #63834, #105858 ),
 ( #7684, #16318, #82655, #96723, #8228, #31483, #41139, #32000, #74020, #64365, #90751, #48146, #64874 ),
 ( #97760, #23927, #26590, #67546, #100956, #51338, #1722, #83181, #43786, #92328, #91817, #76679, #67014 ),
 ( #50794, #10347, #92863, #2245, #68064, #91294, #100424, #26067, #9280, #60529, #17406, #83701, #59460 ),
 ( #93413, #27655, #35195, #84251, #42727, #9809, #19030, #18474, #27115, #19565, #624, #60006, #52398 ),
 ( #75619, #51868, #34140, #2789, #35737, #68619, #43262, #84782, #76144, #10866, #34674, #101500, #8757 ),
 ( #17937, #99894, #58922, #41661, #74550, #33591, #25523, #66466, #99342, #58377, #50277, #42188, #75073 ),
 ( #1165, #4392, #102016, #37331, #45920, #28177, #78799, #62641, #36800, #28708, #103616, #104138, #61590 ),
 ( #70190, #87450, #12465, #20098, #69665, #20640, #44869, #3870, #45398, #5457, #95019, #38378, #29248 ),
 ( #44326, #52942, #94486, #11942, #71241, #70723, #103099, #79336, #61051, #102562, #77758, #46448, #53480 ),
 ( #93943, #4932, #86402, #96064, #12995, #85870, #78276, #62128, #21154, #53983, #30283, #63170, #86924 ),
 ( #37864, #29764, #95527, #22196, #21672, #54505, #13531, #85316, #11401, #77222, #3334, #36278, #69149 ),
 ( #15129, #81973, #64754, #8094, #105726, #16188, #14057, #22730, #64236, #88505, #41004, #40467, #80923 ),
 ( #30825, #39432, #14581, #49075, #23250, #73891, #63710, #48549, #97108, #65809, #89560, #55568, #47491 ),
 ( #6496, #104673, #102441, #32939, #31870, #81438, #72822, #105212, #15656, #96597, #98687, #7553, #56092 ),
 ( #80387, #90084, #97626, #31359, #55047, #72306, #89029, #48013, #56641, #32407, #73349, #106247, #7034 ),
 ( #39949, #23792, #87976, #65279, #98170, #24324, #46961, #79859, #5967, #57172, #38897, #71761, #66880 ),
 ( #18896, #66336, #2654, #33462, #83570, #49617, #25384, #84121, #58241, #91172, #42058, #17276, #35605 ),
 ( #92193, #2116, #99220, #76017, #50151, #92738, #74944, #43655, #100294, #10220, #90622, #16727, #42588 ),
 ( #51739, #83058, #74418, #68480, #25936, #84656, #9149, #493, #50654, #41528, #9678, #18347, #1034 ),
 ( #35067, #34008, #82526, #51200, #24841, #43132, #58795, #67935, #99767, #10741, #76544, #57693, #34543 ),
 ( #100818, #26986, #91690, #17803, #75487, #1582, #67417, #26456, #59321, #8627, #59864, #20514, #11268 ),
 ( #78665, #44201, #86270, #53350, #4267, #62515, #3747, #19964, #45786, #60401, #69539, #52812, #77087 ),
 ( #12343, #53868, #52269, #29640, #5335, #101892, #36677, #94888, #37738, #45270, #86798, #70599, #103490 ),
 ( #37195, #95398, #21539, #78147, #61998, #11808, #54372, #70063, #102964, #12869, #85182, #93279, #46320 ),
 ( #4799, #87318, #13397, #3206, #101371, #102430, #79211, #77626, #61460, #38257, #28572, #29128, #93809 ),
 ( #27524, #85736, #19439, #36147, #69017, #28050, #60922, #44741, #94352, #21032, #88899, #23129, #56511 ),
 ( #87848, #55448, #57042, #72186, #13929, #104008, #54922, #88381, #79741, #89441, #72705, #89959, #14997 ),
 ( #14455, #71635, #16064, #46841, #39305, #47886, #98047, #48947, #81843, #97497, #6907, #105090, #6368 ),
 ( #80795, #23660, #7963, #80256, #47367, #96473, #30153, #31230, #96993, #5845, #64118, #48424, #38770 ),
 ( #55969, #39828, #32277, #105604, #22611, #15531, #63038, #31746, #64630, #104545, #81315, #7427, #40343 ),
 ( #106121, #71119, #30695, #73221, #65148, #24196, #95941, #22063, #63582, #43011, #91042, #50540, #34945 ),
 ( #91569, #1459, #58116, #67816, #25814, #66754, #59202, #24720, #32812, #92612, #9025, #92078, #1997 ),
 ( #49492, #40877, #41934, #100696, #17150, #901, #75900, #50023, #42464, #33342, #100172, #73764, #66210 ),
 ( #57567, #26866, #83994, #10099, #82928, #25255, #83455, #58668, #99639, #26341, #9556, #33876, #8501 ),
 ( #17677, #74820, #59734, #99092, #75359, #34422, #67294, #18221, #51073, #18770, #16601, #51617, #84538 ),
 ( #106662, #82396, #65684, #98572, #90492, #41404, #74295, #372, #53230, #44617, #52679, #20917, #28453 ),
 ( #95286, #19322, #69421, #35481, #11147, #69944, #44076, #76960, #27935, #3077, #21415, #94221, #78031 ),
 ( #85065, #61873, #36023, #78553, #61333, #37078, #54255, #2536, #4148, #10623, #102840, #77506, #29009 ),
 ( #4681, #37615, #70478, #20388, #94768, #53750, #86679, #3620, #36553, #85609, #27406, #19843, #101771 ),
 ( #43542, #11683, #102304, #60284, #86150, #12750, #93153, #12220, #45150, #45671, #103374, #29521, #68897 ),
 ( #76422, #62392, #60800, #52150, #68353, #101253, #93693, #38141, #16886, #99358, #87725, #22483, #80663 ),
 ( #21942, #71515, #55324, #46718, #5725, #47237, #8775, #96868, #41678, #31105, #49766, #46201, #54795 ),
 ( #13806, #74568, #72580, #6239, #82670, #62921, #104415, #79610, #641, #88251, #33608, #95815, #6783 ),
 ( #25540, #14868, #38649, #30560, #39175, #63459, #30032, #66481, #87195, #63989, #39703, #104962, #96352 ),
 ( #14331, #13273, #47759, #80137, #118, #103885, #72057, #79087, #23002, #55838, #5210, #70994, #88776 ),
 ( #33089, #65953, #98833, #24990, #57842, #90769, #101513, #35211, #51884, #91310, #76695, #58399, #2262 ),
 ( #84801, #100974, #92343, #100445, #68637, #19046, #1183, #10886, #35757, #9826, #1736, #2806, #77237 ),
 ( #27672, #84267, #60544, #18491, #99911, #42742, #26603, #17951, #83717, #51355, #85332, #68082, #11417 ),
 ( #19585, #17420, #26080, #67563, #91831, #44343, #43800, #10363, #52414, #34153, #75634, #50813, #3354 ) ),
 .UNSPECIFIED., .F., .F., .F.,
 ( 4, 3, 3, 3, 3, 3, 3, 3, 3, 3, 3, 3, 3, 3, 3, 3, 3, 3, 3, 3, 3, 3, 3, 3, 3, 3, 3, 3, 3, 3, 3, 3, 3, 3, 3, 3, 3, 3, 3, 3, 3, 3, 3, 3, 3, 3, 3, 3, 3, 3, 3, 4 ),
 ( 4, 3, 3, 3, 4 ),
 ( -1.110223024625156540E-16, 0.002843925521740953144, 0.005687851043482017310, 0.008531776565223081477, 0.01137570208696414564, 0.01421962760870520981, 0.01706355313044627398, 0.01990747865218733814, 0.02275140417392840231, 0.02417336693479893439, 0.02559532969566946647, 0.02701729245653999856, 0.02772827383697526460, 0.02843925521741053064, 0.03128318073915159481, 0.03412710626089265897, 0.03697103178263372314, 0.03981495730437478731, 0.04265888282611585147, 0.04408084558698638356, 0.04550280834785691564, 0.04834673386959797980, 0.05119065939133904397, 0.05403458491308010814, 0.05687851043482117230, 0.06256636147830330064, 0.06825421252178542897, 0.07394206356526755730, 0.07678598908700862147, 0.07962991460874968563, 0.09100561669571394230, 0.1137570208696424556, 0.1251327229566067123, 0.1365084250435709690, 0.1421962760870530973, 0.1478841271305352256, 0.1535719781740173540, 0.1592598292174994823, 0.1621037547392405465, 0.1635257175001110785, 0.1649476802609816106, 0.1677916057827226748, 0.1706355313044637390, 0.1720574940653342710, 0.1734794568262048031, 0.1749014195870753352, 0.1756124009675106012, 0.1763233823479458673, 0.1791673078696869315, 0.1798782892501221975, 0.1805892706305574635, 0.1820112333914279956 ),
 ( 0.03187303615303928306, 0.3799792527701029710, 0.7280854693871666727, 1.076191686004230430, 1.424297902621294076 ),
 .UNSPECIFIED. ) ;
#33423 = CARTESIAN_POINT ( 'NONE',  ( 34.58748436418837002, 491.1940522429740668, 12.14470207312156269 ) ) ;
#33424 = CARTESIAN_POINT ( 'NONE',  ( -29.14716730816305201, 13.65620768952807751, 39.72410719430370563 ) ) ;
#33425 = CARTESIAN_POINT ( 'NONE',  ( 0.000000000000000000, 4.898587196589412829E-16, -4.000000000000000000 ) ) ;
#33426 = AXIS2_PLACEMENT_3D ( 'NONE', #11341, #59946, #93884 ) ;
#33427 = ORIENTED_EDGE ( 'NONE', *, *, #73053, .T. ) ;
#33428 = EDGE_LOOP ( 'NONE', ( #5668, #39709, #2326, #91248, #10996 ) ) ;
#33429 = CARTESIAN_POINT ( 'NONE',  ( 52.04862490863282432, -49.90435108743835002, 58.16575394986750069 ) ) ;
#33430 = CARTESIAN_POINT ( 'NONE',  ( -1.954521441386776859, 298.2604977439763729, -10.00252169235627164 ) ) ;
#33431 = CARTESIAN_POINT ( 'NONE',  ( 9.797840486031143215, 51.31133413807796728, 2.591606615044619311 ) ) ;
#33432 = ORIENTED_EDGE ( 'NONE', *, *, #101380, .T. ) ;
#33433 = CARTESIAN_POINT ( 'NONE',  ( -90.63796294261014452, -38.34935958327475447, 15.74237372901285070 ) ) ;
#33434 = ORIENTED_EDGE ( 'NONE', *, *, #24853, .T. ) ;
#33435 = CARTESIAN_POINT ( 'NONE',  ( 15.68120647347719299, 6.021684053266091574, 7.051923121159668462 ) ) ;
#33436 = CARTESIAN_POINT ( 'NONE',  ( 92.51741348077821669, -38.35456167585839893, 39.42312903733464680 ) ) ;
#33437 = CARTESIAN_POINT ( 'NONE',  ( 12.94162442892976017, 23.58706790872225767, 4.602324725384438153 ) ) ;
#33438 = CARTESIAN_POINT ( 'NONE',  ( 87.71464298479139643, -60.14869002622434380, 36.80113247628132456 ) ) ;
#33439 = DIRECTION ( 'NONE',  ( 0.000000000000000000, 1.000000000000000000, 0.000000000000000000 ) ) ;
#33440 = FACE_BOUND ( 'NONE', #67697, .T. ) ;
#33441 = CARTESIAN_POINT ( 'NONE',  ( -35.02151964022808528, 330.0018426590012837, -3.593274941009661827 ) ) ;
#33442 = CIRCLE ( 'NONE', #74671, 3.000000000000023981 ) ;
#33443 = CARTESIAN_POINT ( 'NONE',  ( 3.634575668430249706, -68.17834049427936804, 13.10158581207672057 ) ) ;
#33444 = CARTESIAN_POINT ( 'NONE',  ( 75.19059096504483364, -59.99999999999999289, 182.6202054854667836 ) ) ;
#33445 =( GEOMETRIC_REPRESENTATION_CONTEXT ( 3 ) GLOBAL_UNCERTAINTY_ASSIGNED_CONTEXT ( ( #67095 ) ) GLOBAL_UNIT_ASSIGNED_CONTEXT ( ( #4598, #35401, #60725 ) ) REPRESENTATION_CONTEXT ( 'NONE', 'WORKASPACE' ) );
#33446 = DIRECTION ( 'NONE',  ( 0.000000000000000000, -1.000000000000000000, 0.000000000000000000 ) ) ;
#33447 = ORIENTED_EDGE ( 'NONE', *, *, #103458, .T. ) ;
#33448 = CARTESIAN_POINT ( 'NONE',  ( 60.20930824510026014, -56.86133611672916999, 81.16955359436684603 ) ) ;
#33449 = CARTESIAN_POINT ( 'NONE',  ( -26.51252764419330532, 296.0026311473873193, -9.752274705943550615 ) ) ;
#33450 = EDGE_CURVE ( 'NONE', #78409, #87161, #23992, .T. ) ;
#33451 = CARTESIAN_POINT ( 'NONE',  ( 9.864331116128868260, -50.40680126009896611, 25.34043079474438898 ) ) ;
#33453 = CARTESIAN_POINT ( 'NONE',  ( -5.290067270632215823, 53.47475093287481229, 8.531152949374556371 ) ) ;
#33452 = CARTESIAN_POINT ( 'NONE',  ( -90.13693044984590585, -38.39872991106614109, -15.64445292063840576 ) ) ;
#33454 = CARTESIAN_POINT ( 'NONE',  ( -33.08824659830909809, 433.9163703247937747, 24.51824011208189447 ) ) ;
#33455 = CARTESIAN_POINT ( 'NONE',  ( -38.66182218138258975, 25.17353944418798761, -12.83206308700384746 ) ) ;
#33456 = CARTESIAN_POINT ( 'NONE',  ( 0.000000000000000000, 61.50000000000000000, 0.000000000000000000 ) ) ;
#33457 = CARTESIAN_POINT ( 'NONE',  ( -5.656854249492379694, -28.43749999999999289, -5.656854249492380582 ) ) ;
#33458 = DIRECTION ( 'NONE',  ( -0.000000000000000000, -1.000000000000000000, -0.000000000000000000 ) ) ;
#33459 = EDGE_CURVE ( 'NONE', #25843, #84625, #46055, .T. ) ;
#33460 = DIRECTION ( 'NONE',  ( 0.000000000000000000, 0.000000000000000000, -1.000000000000000000 ) ) ;
#33461 = ORIENTED_EDGE ( 'NONE', *, *, #97343, .T. ) ;
#33462 = CARTESIAN_POINT ( 'NONE',  ( 82.63019022871336006, -50.02483195698248863, 181.3254256235556170 ) ) ;
#33463 = CARTESIAN_POINT ( 'NONE',  ( 5.000000000000000000, -15.93202192939576634, -5.930487099830193287 ) ) ;
#33464 = CARTESIAN_POINT ( 'NONE',  ( 19.61638200451619696, -5.000000000000000000, 0.000000000000000000 ) ) ;
#33465 = ORIENTED_EDGE ( 'NONE', *, *, #96715, .F. ) ;
#33466 = CARTESIAN_POINT ( 'NONE',  ( 13.50000000000000355, 7.794228634059978233, -11.79422863405993382 ) ) ;
#33467 = CIRCLE ( 'NONE', #52444, 8.000000000000000000 ) ;
#33468 = CARTESIAN_POINT ( 'NONE',  ( 42.52018344083600709, 435.0260445551345470, 8.239822296317143469 ) ) ;
#33469 = DIRECTION ( 'NONE',  ( 1.000000000000000000, 0.000000000000000000, 0.000000000000000000 ) ) ;
#33470 = CARTESIAN_POINT ( 'NONE',  ( -38.92110675614357973, 42.05584489377135782, -56.99232464755446870 ) ) ;
#33471 = EDGE_CURVE ( 'NONE', #77629, #55271, #87640, .T. ) ;
#33472 = B_SPLINE_CURVE_WITH_KNOTS ( 'NONE', 3,
 ( #75391, #81870, #7996, #51107 ),
 .UNSPECIFIED., .F., .F.,
 ( 4, 4 ),
 ( 0.000000000000000000, 1.000000000000000000 ),
 .UNSPECIFIED. ) ;
#33473 = STYLED_ITEM ( 'NONE', ( #105084 ), #16991 ) ;
#33474 = CARTESIAN_POINT ( 'NONE',  ( 55.93715591288651723, -60.00000000000000711, 87.98903091118835107 ) ) ;
#33475 = CYLINDRICAL_SURFACE ( 'NONE', #13421, 4.000000000000000000 ) ;
#33476 = CARTESIAN_POINT ( 'NONE',  ( 12.22201992443273966, -14.34686031290847907, 31.77896201686625943 ) ) ;
#33478 = CARTESIAN_POINT ( 'NONE',  ( -13.55912885999853579, 24.71192378330096773, -1.209952234050663211 ) ) ;
#33477 = CARTESIAN_POINT ( 'NONE',  ( -12.15630314080767960, -21.19743429706114313, 35.58279596609094853 ) ) ;
#33479 = CARTESIAN_POINT ( 'NONE',  ( -7.188101187500002709, -13.81250000204838280, 2.977408999572648707 ) ) ;
#33480 = DIRECTION ( 'NONE',  ( 0.000000000000000000, 0.000000000000000000, 1.000000000000000000 ) ) ;
#33481 = CARTESIAN_POINT ( 'NONE',  ( -4.613983237546153582, 6.452243898629807184, -7.591546097228403234 ) ) ;
#33482 = ORIENTED_EDGE ( 'NONE', *, *, #28138, .T. ) ;
#33483 = CARTESIAN_POINT ( 'NONE',  ( -17.49999999999737099, 50.00908096117626656, 61.65219700479646292 ) ) ;
#33484 = CARTESIAN_POINT ( 'NONE',  ( 23.83970809494289611, 25.80407537208032664, 30.86910450433977005 ) ) ;
#33485 = CARTESIAN_POINT ( 'NONE',  ( -40.97493796728242188, 465.3173804043414634, 16.74015881913296155 ) ) ;
#33487 = CARTESIAN_POINT ( 'NONE',  ( 47.71644133373404628, -47.40887823659345202, -30.35360365216715550 ) ) ;
#33486 = CARTESIAN_POINT ( 'NONE',  ( 5.206803358412888549, 53.49072178898849472, 8.531152949374478212 ) ) ;
#33488 = ADVANCED_FACE ( 'NONE', ( #34120 ), #68715, .T. ) ;
#33489 = B_SPLINE_CURVE_WITH_KNOTS ( 'NONE', 3,
 ( #55007, #70160, #31321, #47454, #104102, #39395, #103064, #29219, #87939, #71724, #94984, #14020, #21123, #78763, #53953, #46415, #13493, #46928, #29733, #71207, #37829, #12961, #30788, #70692, #103581, #95491, #63672, #21635 ),
 .UNSPECIFIED., .F., .F.,
 ( 4, 2, 2, 2, 2, 2, 2, 2, 2, 2, 2, 2, 2, 4 ),
 ( 0.007977619942176784537, 0.008210484177485675994, 0.008443348412794569186, 0.008909076883412357303, 0.009374805354030147156, 0.009840533824647937008, 0.01077199076588351845, 0.01170344770711909989, 0.01263490464835468133, 0.01356636158959026277, 0.01449781853082584421, 0.01496354700144363406, 0.01519641123675252725, 0.01542927547206142044 ),
 .UNSPECIFIED. ) ;
#33490 = VERTEX_POINT ( 'NONE', #51307 ) ;
#33491 = DIRECTION ( 'NONE',  ( -1.000000000000000000, -1.224606353822377258E-16, -0.000000000000000000 ) ) ;
#33492 = CARTESIAN_POINT ( 'NONE',  ( 17.23461538461538467, 4.172000000000003261, 5.109226446042759579E-16 ) ) ;
#33493 = ORIENTED_EDGE ( 'NONE', *, *, #69525, .F. ) ;
#33494 = DIRECTION ( 'NONE',  ( -1.000000000000000000, 0.000000000000000000, 0.000000000000000000 ) ) ;
#33495 = PRESENTATION_STYLE_ASSIGNMENT (( #49653 ) ) ;
#33496 = CARTESIAN_POINT ( 'NONE',  ( -19.45775703410437885, 41.87129219958859494, -80.44515592358796141 ) ) ;
#33497 =( GEOMETRIC_REPRESENTATION_CONTEXT ( 3 ) GLOBAL_UNCERTAINTY_ASSIGNED_CONTEXT ( ( #35826 ) ) GLOBAL_UNIT_ASSIGNED_CONTEXT ( ( #40720, #16448, #68747 ) ) REPRESENTATION_CONTEXT ( 'NONE', 'WORKASPACE' ) );
#33498 = CARTESIAN_POINT ( 'NONE',  ( -98.78051181877384579, -59.99999999999999289, 73.70903175910844141 ) ) ;
#33499 = FACE_OUTER_BOUND ( 'NONE', #69513, .T. ) ;
#33500 = PRESENTATION_LAYER_ASSIGNMENT (  '', '', ( #12847 ) ) ;
#33501 = CARTESIAN_POINT ( 'NONE',  ( -16.05785784214753775, 4.775831776487168945, 3.710403933803116949 ) ) ;
#33502 = MECHANICAL_DESIGN_GEOMETRIC_PRESENTATION_REPRESENTATION (  '', ( #61073 ), #62770 ) ;
#33503 = CARTESIAN_POINT ( 'NONE',  ( 39.45202195020148395, 464.6983304258686758, 18.31344484327332367 ) ) ;
#33504 = DIRECTION ( 'NONE',  ( 0.000000000000000000, 0.000000000000000000, 1.000000000000000000 ) ) ;
#33506 = CARTESIAN_POINT ( 'NONE',  ( -5.694238940269539917, 41.34481807419808064, -58.37580806326324989 ) ) ;
#33505 = CARTESIAN_POINT ( 'NONE',  ( 7.996668422910221175, -5.000000000000002665, -78.85453279918266389 ) ) ;
#33507 = CARTESIAN_POINT ( 'NONE',  ( -81.84813229431372861, -49.96181332713019430, 175.6604539455789222 ) ) ;
#33508 = ORIENTED_EDGE ( 'NONE', *, *, #62548, .T. ) ;
#33509 = MECHANICAL_DESIGN_GEOMETRIC_PRESENTATION_REPRESENTATION (  '', ( #52423 ), #93793 ) ;
#33510 = CARTESIAN_POINT ( 'NONE',  ( 7.500000000000005329, 44.25000000000000000, -68.91429205785459544 ) ) ;
#33511 = EDGE_LOOP ( 'NONE', ( #28527, #36703, #106737, #5915, #16569 ) ) ;
#33512 = ORIENTED_EDGE ( 'NONE', *, *, #31314, .F. ) ;
#33513 = DIRECTION ( 'NONE',  ( -1.000000000000000000, -0.000000000000000000, -0.000000000000000000 ) ) ;
#33514 =( BOUNDED_SURFACE ( )  B_SPLINE_SURFACE ( 2, 3, ( 
 ( #15105, #29743, #63688, #94997, #30801, #96574, #47467, #55022 ),
 ( #70170, #30258, #62618, #78775, #47992, #95504, #7009, #62105 ),
 ( #63147, #54484, #21133, #86900, #12973, #87430, #13505, #46428 ) ),
 .UNSPECIFIED., .F., .F., .F. ) 
 B_SPLINE_SURFACE_WITH_KNOTS ( ( 3, 3 ),
 ( 4, 2, 2, 4 ),
 ( 0.000000000000000000, 1.000000000000000000 ),
 ( -0.06656819121499020497, -0.06329489543879425473, 0.001517242213116295688, 0.005444315861320837488 ),
 .UNSPECIFIED. ) 
 GEOMETRIC_REPRESENTATION_ITEM ( )  RATIONAL_B_SPLINE_SURFACE ( (
 ( 1.000000000000000000, 1.000000000000000000, 1.000000000000000000, 1.000000000000000000, 1.000000000000000000, 1.000000000000000000, 1.000000000000000000, 1.000000000000000000),
 ( 1.857142857142858317, 1.857142857142858317, 1.857142857142858317, 1.857142857142858317, 1.857142857142858317, 1.857142857142858317, 1.857142857142858317, 1.857142857142858317),
 ( 1.000000000000000000, 1.000000000000000000, 1.000000000000000000, 1.000000000000000000, 1.000000000000000000, 1.000000000000000000, 1.000000000000000000, 1.000000000000000000) ) ) 
 REPRESENTATION_ITEM ( '' )  SURFACE ( )  );
#33515 = EDGE_CURVE ( 'NONE', #74576, #30465, #8390, .T. ) ;
#33516 = LINE ( 'NONE', #7606, #69769 ) ;
#33517 = EDGE_LOOP ( 'NONE', ( #17455, #26709, #93116, #91118, #74467, #18720 ) ) ;
#33518 = CARTESIAN_POINT ( 'NONE',  ( 0.000000000000000000, -1.500000000000000000, 10.00000000000000000 ) ) ;
#33519 = EDGE_CURVE ( 'NONE', #4042, #35042, #66992, .T. ) ;
#33520 = DIRECTION ( 'NONE',  ( 0.000000000000000000, 0.000000000000000000, 1.000000000000000000 ) ) ;
#33521 = CARTESIAN_POINT ( 'NONE',  ( 13.58349330513380515, 1.593028355512270962E-15, 0.000000000000000000 ) ) ;
#33522 = CARTESIAN_POINT ( 'NONE',  ( -1.249260851835055197, 53.88049993730678722, 8.835555377234499019 ) ) ;
#33523 = CARTESIAN_POINT ( 'NONE',  ( -7.814460424981007236, -5.000000000000000000, -95.45715767408282204 ) ) ;
#33524 = CARTESIAN_POINT ( 'NONE',  ( -43.33498512661116564, 464.9732568094945577, 13.98542553804671407 ) ) ;
#33525 = CARTESIAN_POINT ( 'NONE',  ( 109.4307067020638726, -30.00000000000001066, 166.0292171922573345 ) ) ;
#33526 = EDGE_CURVE ( 'NONE', #76134, #41710, #32683, .T. ) ;
#33527 = CARTESIAN_POINT ( 'NONE',  ( -106.9593936918335544, -14.21045842199438880, 171.9682640579732436 ) ) ;
#33528 = CARTESIAN_POINT ( 'NONE',  ( -58.81820099218335685, -42.96702668141021064, 70.77761850075783912 ) ) ;
#33529 = VERTEX_POINT ( 'NONE', #9786 ) ;
#33530 = CARTESIAN_POINT ( 'NONE',  ( -38.27578887202430025, 38.95432122817999954, 51.21386531492692029 ) ) ;
#33531 = CARTESIAN_POINT ( 'NONE',  ( 94.67678376100681703, -60.00000000000000000, 24.26864735211880486 ) ) ;
#33532 = ORIENTED_EDGE ( 'NONE', *, *, #18794, .F. ) ;
#33533 = CARTESIAN_POINT ( 'NONE',  ( 8.254048633541648528, -49.91580099947954352, 32.20254773541059024 ) ) ;
#33534 = CARTESIAN_POINT ( 'NONE',  ( -104.9716744181120305, -52.71025089284185583, 163.4601265114661715 ) ) ;
#33535 = CARTESIAN_POINT ( 'NONE',  ( -5.082755093536326818, -15.59375000204838635, 5.082755093536325042 ) ) ;
#33536 = CARTESIAN_POINT ( 'NONE',  ( 4.587132918264077652, -29.99999999999999289, 5.539110995917003066 ) ) ;
#33537 = VERTEX_POINT ( 'NONE', #101996 ) ;
#33538 = CARTESIAN_POINT ( 'NONE',  ( -46.00000000000000711, 488.1785408034348848, 2.468284771847338632 ) ) ;
#33539 = AXIS2_PLACEMENT_3D ( 'NONE', #39182, #31626, #7307 ) ;
#33540 = CARTESIAN_POINT ( 'NONE',  ( -75.93880995127246081, -59.99999999999997868, 186.8032436320886518 ) ) ;
#33541 = CARTESIAN_POINT ( 'NONE',  ( 5.082755093536325930, -17.84375000204838457, -5.082755093536325042 ) ) ;
#33542 = EDGE_CURVE ( 'NONE', #74736, #6290, #82541, .T. ) ;
#33543 = CARTESIAN_POINT ( 'NONE',  ( 46.00000000000000000, 460.6862940191787175, 7.630022560110487184 ) ) ;
#33544 = CARTESIAN_POINT ( 'NONE',  ( 102.6464385083043283, 6.123233995736568081E-16, -5.000000000000011546 ) ) ;
#33545 = AXIS2_PLACEMENT_3D ( 'NONE', #14588, #89566, #56100 ) ;
#33546 = DIRECTION ( 'NONE',  ( 0.000000000000000000, -1.000000000000000000, 0.000000000000000000 ) ) ;
#33547 = CARTESIAN_POINT ( 'NONE',  ( 13.50000000000000711, 6.533945317241104611, -12.15804109017022583 ) ) ;
#33548 = CARTESIAN_POINT ( 'NONE',  ( -30.00000000000000355, 464.1059074601055272, 11.21808947555541103 ) ) ;
#33549 = DIRECTION ( 'NONE',  ( 0.000000000000000000, 0.000000000000000000, 1.000000000000000000 ) ) ;
#33550 = CARTESIAN_POINT ( 'NONE',  ( -23.21751746555244722, 28.11705169068991594, 30.70617127781060418 ) ) ;
#33551 = CARTESIAN_POINT ( 'NONE',  ( 25.11650669486618881, 1.474610560812782335E-15, 0.000000000000000000 ) ) ;
#33552 = AXIS2_PLACEMENT_3D ( 'NONE', #9422, #60160, #19186 ) ;
#33553 = AXIS2_PLACEMENT_3D ( 'NONE', #30027, #19837, #62912 ) ;
#33554 = CARTESIAN_POINT ( 'NONE',  ( -33.65812250636221137, -42.96608556679607460, 35.30899569834211604 ) ) ;
#33555 = CARTESIAN_POINT ( 'NONE',  ( 46.36249026935708173, -60.26199203029697316, 51.31417678178487307 ) ) ;
#33556 = CARTESIAN_POINT ( 'NONE',  ( 0.000000000000000000, 0.000000000000000000, 0.000000000000000000 ) ) ;
#33557 = ORIENTED_EDGE ( 'NONE', *, *, #24415, .T. ) ;
#33558 = CARTESIAN_POINT ( 'NONE',  ( 43.79821706557852679, 434.9662578767633363, 12.22743114679940035 ) ) ;
#33559 = CARTESIAN_POINT ( 'NONE',  ( -78.45636384825381526, -38.62886288010908231, 189.5596485861315159 ) ) ;
#33560 = ORIENTED_EDGE ( 'NONE', *, *, #50545, .T. ) ;
#33562 = CARTESIAN_POINT ( 'NONE',  ( 40.61216075948964033, 351.1469683695276558, 22.89433108575548914 ) ) ;
#33561 = CARTESIAN_POINT ( 'NONE',  ( 0.000000000000000000, 3.000000000000002665, 0.000000000000000000 ) ) ;
#33563 = CARTESIAN_POINT ( 'NONE',  ( -9.417877086999621149E-14, 35.24549338070647764, 53.20147685480977628 ) ) ;
#33564 = CARTESIAN_POINT ( 'NONE',  ( 16.34886101041479378, 36.48569306717565297, 24.24298062968059853 ) ) ;
#33565 = CARTESIAN_POINT ( 'NONE',  ( -43.50250715914095423, 464.6389613228375879, 9.611700240010623730 ) ) ;
#33566 = CARTESIAN_POINT ( 'NONE',  ( 32.61650669486618881, 1.474610560812782335E-15, 0.000000000000000000 ) ) ;
#33567 = CARTESIAN_POINT ( 'NONE',  ( -38.19885457863131251, 25.52371017071349613, 11.08075699806225423 ) ) ;
#33568 = CARTESIAN_POINT ( 'NONE',  ( -31.18764089105624393, 357.3273780643992268, 20.56365793791859531 ) ) ;
#33569 = CARTESIAN_POINT ( 'NONE',  ( -3.313708498984741180, -25.71875000409677625, -8.000000000000019540 ) ) ;
#33570 = CARTESIAN_POINT ( 'NONE',  ( 111.0056519548954128, -60.00000000000002132, 152.1919057739970924 ) ) ;
#33571 = CARTESIAN_POINT ( 'NONE',  ( -3.354250471127029343E-15, -6.534749472788162983, -4.681481898396973484 ) ) ;
#33572 = CARTESIAN_POINT ( 'NONE',  ( -33.76223977132627141, 470.3516487496773948, 6.012963278766592978 ) ) ;
#33573 = EDGE_LOOP ( 'NONE', ( #30694, #38131, #59459, #14822 ) ) ;
#33574 = EDGE_CURVE ( 'NONE', #35576, #90586, #105935, .T. ) ;
#33575 = AXIS2_PLACEMENT_3D ( 'NONE', #37293, #38859, #63132 ) ;
#33576 = CARTESIAN_POINT ( 'NONE',  ( -99.06500401421689617, -29.99999999999995026, 188.7035041724194286 ) ) ;
#33577 = ORIENTED_EDGE ( 'NONE', *, *, #2172, .F. ) ;
#33578 = DIRECTION ( 'NONE',  ( -1.000000000000000000, -0.000000000000000000, -0.000000000000000000 ) ) ;
#33579 = SURFACE_STYLE_USAGE ( .BOTH. , #1157 ) ;
#33580 = CARTESIAN_POINT ( 'NONE',  ( 31.36136185978966040, 339.5482298604329685, 18.45068369565698418 ) ) ;
#33581 = CARTESIAN_POINT ( 'NONE',  ( -21.99817791066553951, 28.09376123749146714, -31.66916887880079301 ) ) ;
#33582 = CARTESIAN_POINT ( 'NONE',  ( -7.188101187500000044, -21.78125000204838457, -8.802885111219163269E-16 ) ) ;
#33583 = LINE ( 'NONE', #72943, #41583 ) ;
#33585 = ADVANCED_FACE ( 'NONE', ( #37305 ), #43271, .F. ) ;
#33584 = CARTESIAN_POINT ( 'NONE',  ( 7.398498005860211890, 40.00000000200842010, -70.41866429880424505 ) ) ;
#33586 = PRESENTATION_LAYER_ASSIGNMENT (  '', '', ( #35371 ) ) ;
#33587 = CONICAL_SURFACE ( 'NONE', #88697, 4.000000000000001776, 0.9599310885968774798 ) ;
#33588 = CIRCLE ( 'NONE', #90386, 5.000000000000000000 ) ;
#33589 = STYLED_ITEM ( 'NONE', ( #64448 ), #41857 ) ;
#33590 = VERTEX_POINT ( 'NONE', #3848 ) ;
#33591 = CARTESIAN_POINT ( 'NONE',  ( 82.39176465435255636, -42.97103400991685618, 169.7411559209277243 ) ) ;
#33592 = CARTESIAN_POINT ( 'NONE',  ( -8.334564508161101060, 38.95383793066860534, 63.67138272020815037 ) ) ;
#33593 = STYLED_ITEM ( 'NONE', ( #22567 ), #86480 ) ;
#33594 = ORIENTED_EDGE ( 'NONE', *, *, #94914, .F. ) ;
#33595 = CARTESIAN_POINT ( 'NONE',  ( -61.03778855244135571, 49.99999999999999289, -15.95112753556822760 ) ) ;
#33596 = FILL_AREA_STYLE_COLOUR ( '', #18495 ) ;
#33597 = DIRECTION ( 'NONE',  ( 1.000000000000000000, 0.000000000000000000, 0.000000000000000000 ) ) ;
#33598 = DIRECTION ( 'NONE',  ( -1.000000000000000000, -0.000000000000000000, -0.000000000000000000 ) ) ;
#33599 = AXIS2_PLACEMENT_3D ( 'NONE', #59580, #75196, #19685 ) ;
#33600 = CARTESIAN_POINT ( 'NONE',  ( -40.85164678844374464, -60.00000000000000000, -33.69328355261731645 ) ) ;
#33601 = CARTESIAN_POINT ( 'NONE',  ( -29.22284240011272161, 312.6584099927333682, 12.30496723460669273 ) ) ;
#33602 = CARTESIAN_POINT ( 'NONE',  ( 13.58349330513380515, 4.898587196589411843E-16, -4.000000000000001776 ) ) ;
#33603 = EDGE_CURVE ( 'NONE', #54759, #62805, #57467, .T. ) ;
#33604 = VERTEX_POINT ( 'NONE', #32912 ) ;
#33605 = FILL_AREA_STYLE_COLOUR ( '', #36813 ) ;
#33606 = CARTESIAN_POINT ( 'NONE',  ( -6.499999999999999112, -2.534234941938130703, -0.3584823952106149791 ) ) ;
#33607 = CARTESIAN_POINT ( 'NONE',  ( 7.439138809193584834, 41.00331669213974806, -59.84461289586582922 ) ) ;
#33609 = EDGE_CURVE ( 'NONE', #105779, #82223, #5098, .T. ) ;
#33608 = CARTESIAN_POINT ( 'NONE',  ( 86.79046891330465030, -24.35748604248244220, 185.5599931926667523 ) ) ;
#33610 = CARTESIAN_POINT ( 'NONE',  ( -7.500000000000000000, 4.330127018922188320, -7.422398894150033399 ) ) ;
#33611 = CARTESIAN_POINT ( 'NONE',  ( -3.999980918664427065, -8.688225714286829771, 6.928214246854706992 ) ) ;
#33612 = CARTESIAN_POINT ( 'NONE',  ( 16.08349330513380337, 4.000000000000003553, 0.000000000000000000 ) ) ;
#33613 = CARTESIAN_POINT ( 'NONE',  ( -15.05785784214257461, 3.824195276785042896, 4.604276673521232155 ) ) ;
#33614 = ADVANCED_FACE ( 'NONE', ( #56616 ), #104646, .F. ) ;
#33615 = CARTESIAN_POINT ( 'NONE',  ( 37.10858375827000089, 439.7067619725109466, 24.11495004416381960 ) ) ;
#33616 = CONTEXT_DEPENDENT_SHAPE_REPRESENTATION ( #103812, #23521 ) ;
#33617 = CARTESIAN_POINT ( 'NONE',  ( 48.15042790184239863, 11.33351092753205513, 14.35535821593427386 ) ) ;
#33618 = ORIENTED_EDGE ( 'NONE', *, *, #72780, .F. ) ;
#33619 = CARTESIAN_POINT ( 'NONE',  ( 0.4139731306290318491, 44.05904992622305372, 16.31755368115256033 ) ) ;
#33620 = FACE_OUTER_BOUND ( 'NONE', #31838, .T. ) ;
#33621 = CARTESIAN_POINT ( 'NONE',  ( -10.04799450895598412, 7.431456737699888571, -5.000000000000000888 ) ) ;
#33622 = CARTESIAN_POINT ( 'NONE',  ( 31.46253585067004721, 1.340359594676612611E-15, 0.000000000000000000 ) ) ;
#33623 = ORIENTED_EDGE ( 'NONE', *, *, #16598, .T. ) ;
#33624 = DIRECTION ( 'NONE',  ( -1.000000000000000000, -1.224606353822377258E-16, -0.000000000000000000 ) ) ;
#33625 = FACE_OUTER_BOUND ( 'NONE', #26633, .T. ) ;
#33626 = CARTESIAN_POINT ( 'NONE',  ( 0.000000000000000000, 0.000000000000000000, -2.296599999999999753 ) ) ;
#33627 = CARTESIAN_POINT ( 'NONE',  ( 99.73478044767607287, -57.67101520680783011, 67.37346591704599064 ) ) ;
#33628 = CARTESIAN_POINT ( 'NONE',  ( 36.12805158198114697, 463.5537319797338682, 19.64593688561118157 ) ) ;
#33629 = CARTESIAN_POINT ( 'NONE',  ( 3.013809335369860509, 15.21035869299223009, 6.321051127802831182 ) ) ;
#33630 = CARTESIAN_POINT ( 'NONE',  ( 98.31310517497099966, 5.000000000000020428, 0.000000000000000000 ) ) ;
#33631 = CARTESIAN_POINT ( 'NONE',  ( -19.50010530980351220, 50.00000000000000000, 59.90637122617393828 ) ) ;
#33632 = CARTESIAN_POINT ( 'NONE',  ( -76.16011686981150319, -60.00000000000001421, 187.6210859576851249 ) ) ;
#33633 = DIRECTION ( 'NONE',  ( 1.000000000000000000, 0.000000000000000000, 0.000000000000000000 ) ) ;
#33634 = CARTESIAN_POINT ( 'NONE',  ( -22.91651842568168362, 295.0901107613288445, -9.949346074078583513 ) ) ;
#33635 = CARTESIAN_POINT ( 'NONE',  ( -83.65499586678340904, -50.13462276898575709, 185.8592676192767783 ) ) ;
#33636 = AXIS2_PLACEMENT_3D ( 'NONE', #25132, #101119, #59616 ) ;
#33637 = ORIENTED_EDGE ( 'NONE', *, *, #64129, .T. ) ;
#33638 = CARTESIAN_POINT ( 'NONE',  ( 30.62685779490040261, 313.0583036694750945, -8.065315349801879918 ) ) ;
#33639 = ORIENTED_EDGE ( 'NONE', *, *, #21622, .F. ) ;
#33640 = CARTESIAN_POINT ( 'NONE',  ( -7.800703710507056243, -13.58595692657941711, 1.791736796405273058 ) ) ;
#33641 = ADVANCED_FACE ( 'NONE', ( #57671 ), #94945, .T. ) ;
#33643 = CARTESIAN_POINT ( 'NONE',  ( -47.33333333333330728, 59.99999999999999289, -23.66666666666666785 ) ) ;
#33642 = AXIS2_PLACEMENT_3D ( 'NONE', #1702, #66997, #34658 ) ;
#33644 = CARTESIAN_POINT ( 'NONE',  ( -84.48354631104164980, -45.26985310514864835, -5.680659070506059116 ) ) ;
#33645 = FILL_AREA_STYLE_COLOUR ( '', #32268 ) ;
#33646 = CARTESIAN_POINT ( 'NONE',  ( -15.39039450733990400, 44.07978680685108230, 5.266078492798498267 ) ) ;
#33647 = CIRCLE ( 'NONE', #2595, 4.000000000000001776 ) ;
#33648 = CARTESIAN_POINT ( 'NONE',  ( 92.53532739719321398, 6.123233995736568081E-16, -5.000000000000011546 ) ) ;
#33649 = CARTESIAN_POINT ( 'NONE',  ( 0.000000000000000000, 0.000000000000000000, 0.000000000000000000 ) ) ;
#33650 = CARTESIAN_POINT ( 'NONE',  ( 10.36976902195542749, 10.88984728681280778, -10.43162212896576335 ) ) ;
#33651 = ADVANCED_FACE ( 'NONE', ( #33440, #84096 ), #43634, .F. ) ;
#33652 = CARTESIAN_POINT ( 'NONE',  ( -6.949531687764044400E-15, 14.17434517210798184, 56.74723269274520021 ) ) ;
#33653 = CARTESIAN_POINT ( 'NONE',  ( -35.94513182849163258, 437.3829582663586848, 4.385777999725225307 ) ) ;
#33654 = EDGE_CURVE ( 'NONE', #26193, #80767, #67932, .T. ) ;
#33655 = CARTESIAN_POINT ( 'NONE',  ( 16.60915088697842990, -29.99999999999996092, -39.45628980158949162 ) ) ;
#33656 = CARTESIAN_POINT ( 'NONE',  ( -75.71675511854569152, -53.37976804700807776, 134.7001851824688856 ) ) ;
#33657 = VERTEX_POINT ( 'NONE', #17255 ) ;
#33658 = CARTESIAN_POINT ( 'NONE',  ( 71.28669324481667502, -60.00000000000002132, 168.6228882893990715 ) ) ;
#33659 = DIRECTION ( 'NONE',  ( 0.000000000000000000, -1.000000000000000000, 0.000000000000000000 ) ) ;
#33660 = CARTESIAN_POINT ( 'NONE',  ( 93.90460291926041236, -57.67583523855721950, 7.672568471264877843 ) ) ;
#33661 = CONICAL_SURFACE ( 'NONE', #47404, 4.000000000000001776, 0.9599310885968774798 ) ;
#33663 = VERTEX_POINT ( 'NONE', #42565 ) ;
#33662 = TOROIDAL_SURFACE ( 'NONE', #25046, 10.12668159690567826, 0.7733184030943209830 ) ;
#33664 = CARTESIAN_POINT ( 'NONE',  ( 7.299581481787712711, -12.47920354261283649, 8.323684855074615641 ) ) ;
#33665 = VECTOR ( 'NONE', #11052, 1000.000000000000000 ) ;
#33666 = EDGE_CURVE ( 'NONE', #90700, #22313, #96221, .T. ) ;
#33667 = CARTESIAN_POINT ( 'NONE',  ( -10.00000000000000178, 16.00000000000000000, 4.582575694955834500 ) ) ;
#33668 = ORIENTED_EDGE ( 'NONE', *, *, #98962, .F. ) ;
#33669 = AXIS2_PLACEMENT_3D ( 'NONE', #51053, #83970, #10081 ) ;
#33670 = DIRECTION ( 'NONE',  ( 0.000000000000000000, 0.000000000000000000, 1.000000000000000000 ) ) ;
#33671 = EDGE_CURVE ( 'NONE', #26189, #98844, #66855, .T. ) ;
#33672 = DIRECTION ( 'NONE',  ( 1.000000000000000000, 0.000000000000000000, 0.000000000000000000 ) ) ;
#33673 = FACE_OUTER_BOUND ( 'NONE', #52259, .T. ) ;
#33674 = CARTESIAN_POINT ( 'NONE',  ( 7.188101187500000044, -11.65625000204838635, 0.000000000000000000 ) ) ;
#33675 = EDGE_CURVE ( 'NONE', #89428, #69676, #91065, .T. ) ;
#33676 = LINE ( 'NONE', #66548, #106659 ) ;
#33677 = AXIS2_PLACEMENT_3D ( 'NONE', #6504, #65287, #39442 ) ;
#33678 = CARTESIAN_POINT ( 'NONE',  ( 6.683837171061805194, -3.955946848495972556, -6.851900933636989599 ) ) ;
#33679 = CARTESIAN_POINT ( 'NONE',  ( 6.394337469123802187, 3.776351736504755863, -6.540833074877207665 ) ) ;
#33680 = CARTESIAN_POINT ( 'NONE',  ( -7.500000000000000000, -3.105855721450334617, -7.659356991636312451 ) ) ;
#33681 = CARTESIAN_POINT ( 'NONE',  ( 63.56127108291158123, 6.975173280561618775E-15, 0.000000000000000000 ) ) ;
#33682 = VERTEX_POINT ( 'NONE', #51716 ) ;
#33683 = CARTESIAN_POINT ( 'NONE',  ( -7.414908815205982329, 40.55825190657662915, -70.34918218187874572 ) ) ;
#33685 = CARTESIAN_POINT ( 'NONE',  ( 29.71491464515361969, -25.59252497190302122, 30.54298176171112544 ) ) ;
#33684 = CARTESIAN_POINT ( 'NONE',  ( -3.454253436624944662, -49.15858197120394379, 103.7259032015042095 ) ) ;
#33686 = CARTESIAN_POINT ( 'NONE',  ( 25.72383541997187706, 306.6074583397111155, -8.614371337684147534 ) ) ;
#33687 = ORIENTED_EDGE ( 'NONE', *, *, #91651, .F. ) ;
#33688 = DIRECTION ( 'NONE',  ( 0.000000000000000000, -1.000000000000000000, 0.000000000000000000 ) ) ;
#33689 = ORIENTED_EDGE ( 'NONE', *, *, #90922, .T. ) ;
#33691 = CARTESIAN_POINT ( 'NONE',  ( -7.996316163937361665, -5.000000000000001776, -6.145999768515051365 ) ) ;
#33690 = DIRECTION ( 'NONE',  ( 0.000000000000000000, 0.000000000000000000, 1.000000000000000000 ) ) ;
#33692 = FACE_OUTER_BOUND ( 'NONE', #1892, .T. ) ;
#33693 = DIRECTION ( 'NONE',  ( 0.000000000000000000, -1.000000000000000000, 0.000000000000000000 ) ) ;
#33694 = CARTESIAN_POINT ( 'NONE',  ( 20.21880305278369150, 304.8280059657581660, -9.005058168222337400 ) ) ;
#33695 = CARTESIAN_POINT ( 'NONE',  ( 0.08412207463451333578, 46.21383923812597772, 16.25000000000000355 ) ) ;
#33696 = CARTESIAN_POINT ( 'NONE',  ( -35.47699217159583185, 463.6829005663038288, 19.36631617875508127 ) ) ;
#33697 = VERTEX_POINT ( 'NONE', #76523 ) ;
#33698 = CARTESIAN_POINT ( 'NONE',  ( 79.32333215263945192, -60.00000000000000711, -28.32974529982569578 ) ) ;
#33699 = CARTESIAN_POINT ( 'NONE',  ( -11.42604336269055487, 45.35830052782390709, -14.67759751612683417 ) ) ;
#33700 = SURFACE_STYLE_FILL_AREA ( #66575 ) ;
#33701 = CARTESIAN_POINT ( 'NONE',  ( 20.24579557674103469, 304.8297271373346575, -10.00469232190998703 ) ) ;
#33702 = CIRCLE ( 'NONE', #28555, 5.000000000000010658 ) ;
#33703 = CARTESIAN_POINT ( 'NONE',  ( -47.90217879170931781, 15.22462055664102465, -16.85535821593460781 ) ) ;
#33704 = ORIENTED_EDGE ( 'NONE', *, *, #27024, .T. ) ;
#33705 = CARTESIAN_POINT ( 'NONE',  ( -36.58660523126660280, 27.99651712798071657, 12.99820278958899067 ) ) ;
#33706 = ORIENTED_EDGE ( 'NONE', *, *, #82143, .F. ) ;
#33707 = VERTEX_POINT ( 'NONE', #27502 ) ;
#33708 = CARTESIAN_POINT ( 'NONE',  ( 6.928203230275510549, 85.00000000000000000, -4.000000000000000000 ) ) ;
#33709 = CARTESIAN_POINT ( 'NONE',  ( 43.71297783477844234, 485.1278128289774827, -1.116606130290200172 ) ) ;
#33710 = CARTESIAN_POINT ( 'NONE',  ( -33.00000000000000000, 461.8163627757383551, 11.11111419091028729 ) ) ;
#33711 = DIRECTION ( 'NONE',  ( 0.3144882010765461811, 0.9492613820142679071, 0.000000000000000000 ) ) ;
#33712 = CARTESIAN_POINT ( 'NONE',  ( 86.78697920443168812, -60.15489657647691502, -1.591601715208872836 ) ) ;
#33713 = CARTESIAN_POINT ( 'NONE',  ( -37.49627282300918552, 304.7695756402364395, -7.718605803013700140 ) ) ;
#33714 = FACE_OUTER_BOUND ( 'NONE', #81541, .T. ) ;
#33715 = CARTESIAN_POINT ( 'NONE',  ( 12.50000000000000711, 39.93267479482753401, -65.69976313914253296 ) ) ;
#33716 = ORIENTED_EDGE ( 'NONE', *, *, #42069, .F. ) ;
#33718 = EDGE_CURVE ( 'NONE', #28989, #48371, #87294, .T. ) ;
#33717 = CARTESIAN_POINT ( 'NONE',  ( -9.959852493538001283, 43.33480949895421475, 15.36720373720356747 ) ) ;
#33719 = EDGE_LOOP ( 'NONE', ( #51880, #105634, #17124, #102575 ) ) ;
#33720 = CARTESIAN_POINT ( 'NONE',  ( 9.635035931158675737, 51.40929392797971786, -2.123426622847617296 ) ) ;
#33722 = VERTEX_POINT ( 'NONE', #37177 ) ;
#33721 = CARTESIAN_POINT ( 'NONE',  ( 5.612821243144477279, 51.99076548715343193, 6.070840976756991303 ) ) ;
#33723 = CARTESIAN_POINT ( 'NONE',  ( 67.38364752544607938, -18.62895086270174616, 82.15773094806566235 ) ) ;
#33724 = B_SPLINE_CURVE_WITH_KNOTS ( 'NONE', 3,
 ( #55032, #63697, #62114, #72292, #53971, #97097 ),
 .UNSPECIFIED., .F., .F.,
 ( 4, 2, 4 ),
 ( 0.01390592816464532311, 0.01784842065628997054, 0.02179091314793462145 ),
 .UNSPECIFIED. ) ;
#33725 = VERTEX_POINT ( 'NONE', #61976 ) ;
#33726 = CARTESIAN_POINT ( 'NONE',  ( 50.91589357091642398, 38.95383793061586886, 39.12903940718169338 ) ) ;
#33727 = CARTESIAN_POINT ( 'NONE',  ( 7.188101187500000044, -25.15625000204838813, 0.000000000000000000 ) ) ;
#33728 = CARTESIAN_POINT ( 'NONE',  ( -113.8744714263418842, -57.67115484533559311, 181.1306260539751918 ) ) ;
#33729 = AXIS2_PLACEMENT_3D ( 'NONE', #104523, #22592, #96974 ) ;
#33730 = ORIENTED_EDGE ( 'NONE', *, *, #67896, .T. ) ;
#33731 =( NAMED_UNIT ( * ) PLANE_ANGLE_UNIT ( ) SI_UNIT ( $, .RADIAN. ) );
#33732 = CARTESIAN_POINT ( 'NONE',  ( 37.50059943756144776, 490.7879993827856993, 12.38039871356534505 ) ) ;
#33733 = COLOUR_RGB ( '', 0.08235294, 0.09019608, 0.10196078) ;
#33734 = CARTESIAN_POINT ( 'NONE',  ( 105.9254696489590089, -60.15131266928262477, 182.9954770859043833 ) ) ;
#33735 = CARTESIAN_POINT ( 'NONE',  ( 5.912699410789617360, 51.88565102575169874, -6.185454916783826640 ) ) ;
#33736 = ADVANCED_FACE ( 'NONE', ( #36125, #21008 ), #70038, .F. ) ;
#33737 = DIRECTION ( 'NONE',  ( 1.734723475976807094E-16, 0.000000000000000000, 1.000000000000000000 ) ) ;
#33738 = AXIS2_PLACEMENT_3D ( 'NONE', #83793, #74636, #8313 ) ;
#33739 = CARTESIAN_POINT ( 'NONE',  ( -5.656854249492379694, -22.62500000409676915, -5.656854249492380582 ) ) ;
#33740 = CONICAL_SURFACE ( 'NONE', #47486, 5.000000000000000000, 0.9599310885968913576 ) ;
#33741 = CARTESIAN_POINT ( 'NONE',  ( 43.32918576489185369, 484.9664181796746334, 4.870614540792619351 ) ) ;
#33742 = AXIS2_PLACEMENT_3D ( 'NONE', #19370, #100223, #50589 ) ;
#33743 =( NAMED_UNIT ( * ) PLANE_ANGLE_UNIT ( ) SI_UNIT ( $, .RADIAN. ) );
#33744 = VECTOR ( 'NONE', #23847, 1000.000000000000000 ) ;
#33745 = DIRECTION ( 'NONE',  ( -0.000000000000000000, 1.000000000000000000, -0.000000000000000000 ) ) ;
#33746 = ADVANCED_FACE ( 'NONE', ( #102405 ), #54263, .T. ) ;
#33747 = CARTESIAN_POINT ( 'NONE',  ( -9.999586304443505824, 7.500591597926683285, 5.000000000000000888 ) ) ;
#33748 = CARTESIAN_POINT ( 'NONE',  ( 19.29515645702225868, 6.123233995736772199E-16, -5.000000000000001776 ) ) ;
#33749 = CARTESIAN_POINT ( 'NONE',  ( 33.78291765283140791, 258.1183258647170646, 182.1969486012845891 ) ) ;
#33750 = ORIENTED_EDGE ( 'NONE', *, *, #84789, .T. ) ;
#33751 = CARTESIAN_POINT ( 'NONE',  ( 43.00000000000000000, 488.3725375423206287, 3.127739281036224117 ) ) ;
#33752 = DIRECTION ( 'NONE',  ( 0.000000000000000000, -1.000000000000000000, 0.000000000000000000 ) ) ;
#33753 = AXIS2_PLACEMENT_3D ( 'NONE', #80530, #6647, #64376 ) ;
#33754 = CARTESIAN_POINT ( 'NONE',  ( 7.961919226131998428, -60.00000000000000711, 39.63277225375871637 ) ) ;
#33755 = CARTESIAN_POINT ( 'NONE',  ( -95.56182489229684052, -29.99999999999999645, 191.3238752510769700 ) ) ;
#33756 = EDGE_LOOP ( 'NONE', ( #24243, #64907 ) ) ;
#33757 = ORIENTED_EDGE ( 'NONE', *, *, #11952, .F. ) ;
#33758 = DIRECTION ( 'NONE',  ( -0.8308658609248562588, -0.5564727496918402405, 0.000000000000000000 ) ) ;
#33759 = CARTESIAN_POINT ( 'NONE',  ( 69.93972929822530205, -57.68247516750832915, 153.7333845119171940 ) ) ;
#33761 = CARTESIAN_POINT ( 'NONE',  ( -9.172606077037439576, 6.899872791988882703, 3.046639664573870476 ) ) ;
#33760 =( NAMED_UNIT ( * ) PLANE_ANGLE_UNIT ( ) SI_UNIT ( $, .RADIAN. ) );
#33762 = CARTESIAN_POINT ( 'NONE',  ( 13.62955596626466992, -23.64027760696375324, -38.53637356313394946 ) ) ;
#33763 = PRODUCT_RELATED_PRODUCT_CATEGORY ( 'part', '', ( #14054 ) ) ;
#33764 = DIRECTION ( 'NONE',  ( 0.000000000000000000, 1.000000000000000000, -0.000000000000000000 ) ) ;
#33765 = CARTESIAN_POINT ( 'NONE',  ( -43.49728549343999617, -59.99999999999999289, 57.75799430402353352 ) ) ;
#33766 = B_SPLINE_CURVE_WITH_KNOTS ( 'NONE', 3,
 ( #25274, #32830, #90509, #16619 ),
 .UNSPECIFIED., .F., .F.,
 ( 4, 4 ),
 ( 0.000000000000000000, 0.001856568542221336254 ),
 .UNSPECIFIED. ) ;
#33767 = CARTESIAN_POINT ( 'NONE',  ( 11.42008614078136119, 13.49845512739828202, 9.994469747613118571 ) ) ;
#33768 = CARTESIAN_POINT ( 'NONE',  ( 34.38981283644013587, 463.7396323591540295, 19.22682496774580940 ) ) ;
#33769 = CARTESIAN_POINT ( 'NONE',  ( -86.58000157545598086, -16.99658149479392222, 184.8764613376573038 ) ) ;
#33770 = ORIENTED_EDGE ( 'NONE', *, *, #15801, .T. ) ;
#33771 = DIRECTION ( 'NONE',  ( 0.000000000000000000, 1.000000000000000000, 0.000000000000000000 ) ) ;
#33772 = CARTESIAN_POINT ( 'NONE',  ( -10.26648064962001605, -39.47613848608923348, 30.48065965013316969 ) ) ;
#33773 = CIRCLE ( 'NONE', #95742, 5.000000000000011546 ) ;
#33774 = SURFACE_SIDE_STYLE ('',( #49923 ) ) ;
#33775 = SURFACE_SIDE_STYLE ('',( #83357 ) ) ;
#33777 = CARTESIAN_POINT ( 'NONE',  ( 4.279808479562545287, -69.01068216744177164, 13.66703314698427363 ) ) ;
#33776 = DIRECTION ( 'NONE',  ( -1.000000000000000000, -0.000000000000000000, -0.000000000000000000 ) ) ;
#33778 = ORIENTED_EDGE ( 'NONE', *, *, #93960, .T. ) ;
#33779 = CARTESIAN_POINT ( 'NONE',  ( 26.35557460423923359, 34.76314064348615318, 9.820069159921292368 ) ) ;
#33780 = CARTESIAN_POINT ( 'NONE',  ( -3.594029361870008099, -9.531975552773349847, 6.225090491531444670 ) ) ;
#33781 = ADVANCED_FACE ( 'NONE', ( #25583 ), #15401, .T. ) ;
#33782 = CARTESIAN_POINT ( 'NONE',  ( -7.618844049274130725, 33.17235898929458671, 2.450177051822846064 ) ) ;
#33783 = CARTESIAN_POINT ( 'NONE',  ( 33.32676612059159282, 300.4738025130130836, -0.7366437868951274393 ) ) ;
#33784 = CARTESIAN_POINT ( 'NONE',  ( 4.628159615119683323, -47.68919827030615721, 102.5435725457685976 ) ) ;
#33785 = EDGE_CURVE ( 'NONE', #86867, #36517, #6779, .T. ) ;
#33786 = CARTESIAN_POINT ( 'NONE',  ( 0.000000000000000000, 0.000000000000000000, 11.27631144943088515 ) ) ;
#33787 = DIRECTION ( 'NONE',  ( 0.8191520442889884679, 0.000000000000000000, 0.5735764363510508224 ) ) ;
#33788 = CARTESIAN_POINT ( 'NONE',  ( 112.8608516834554649, -60.00000000000000000, 189.7942083920301855 ) ) ;
#33789 = VERTEX_POINT ( 'NONE', #26640 ) ;
#33790 = FACE_OUTER_BOUND ( 'NONE', #74808, .T. ) ;
#33791 = CARTESIAN_POINT ( 'NONE',  ( -33.00000000000000000, 450.0000000000002274, 13.20242257375370976 ) ) ;
#33792 = CARTESIAN_POINT ( 'NONE',  ( -7.922281120364393914, -4.573931137438282057, -8.047472243342934206 ) ) ;
#33793 = CARTESIAN_POINT ( 'NONE',  ( 45.50299341493403205, 391.6058417003721388, 8.004974616321380410 ) ) ;
#33794 = DIRECTION ( 'NONE',  ( 0.000000000000000000, -1.000000000000000000, 0.000000000000000000 ) ) ;
#33795 = ORIENTED_EDGE ( 'NONE', *, *, #38757, .T. ) ;
#33796 = PRESENTATION_LAYER_ASSIGNMENT (  '', '', ( #4436 ) ) ;
#33797 = FACE_BOUND ( 'NONE', #177, .T. ) ;
#33798 = ADVANCED_FACE ( 'NONE', ( #18532 ), #65379, .T. ) ;
#33799 = EDGE_LOOP ( 'NONE', ( #73172, #27725 ) ) ;
#33800 = CARTESIAN_POINT ( 'NONE',  ( 0.000000000000000000, 0.000000000000000000, 4.000000000000000888 ) ) ;
#33801 = ADVANCED_FACE ( 'NONE', ( #10922 ), #86037, .T. ) ;
#33802 = CARTESIAN_POINT ( 'NONE',  ( 31.70215989067338214, 439.7444121578560043, 23.75167943470401255 ) ) ;
#33803 = CARTESIAN_POINT ( 'NONE',  ( 9.040043340647704539, 46.05340506531722866, 14.03079106125270670 ) ) ;
#33804 = AXIS2_PLACEMENT_3D ( 'NONE', #77492, #59723, #1442 ) ;
#33805 = CARTESIAN_POINT ( 'NONE',  ( 63.03617022296134564, 48.00000000000000000, -16.93907820452146851 ) ) ;
#33806 = CARTESIAN_POINT ( 'NONE',  ( 6.124999999999992006, -15.62228920881126015, 14.41094225130410322 ) ) ;
#33808 = EDGE_CURVE ( 'NONE', #53428, #82494, #51097, .T. ) ;
#33807 = CARTESIAN_POINT ( 'NONE',  ( 46.00000000000003553, 436.0514809771110549, 12.15836796610173742 ) ) ;
#33809 = ORIENTED_EDGE ( 'NONE', *, *, #99330, .F. ) ;
#33810 = CARTESIAN_POINT ( 'NONE',  ( 108.1941172262546331, -60.00000000000000000, 195.3107487755136162 ) ) ;
#33811 = CIRCLE ( 'NONE', #47546, 0.5000000000000004441 ) ;
#33813 = CARTESIAN_POINT ( 'NONE',  ( 14.34223220226681050, -25.54896781464430688, 28.25844851971035965 ) ) ;
#33812 = CARTESIAN_POINT ( 'NONE',  ( -86.32002947858198638, -29.99999999999988987, 198.0868106477030892 ) ) ;
#33815 = FILL_AREA_STYLE ('',( #91508 ) ) ;
#33814 = PRODUCT_DEFINITION_CONTEXT ( 'detailed design', #58288, 'design' ) ;
#33816 = DIRECTION ( 'NONE',  ( -1.000000000000000000, 0.000000000000000000, 0.000000000000000000 ) ) ;
#33817 = CARTESIAN_POINT ( 'NONE',  ( -40.18246394402392951, -39.52194550917157301, 38.87972210423134101 ) ) ;
#33818 = DIRECTION ( 'NONE',  ( -1.000000000000000000, -0.000000000000000000, -0.000000000000000000 ) ) ;
#33819 = MECHANICAL_DESIGN_GEOMETRIC_PRESENTATION_REPRESENTATION (  '', ( #85466 ), #67139 ) ;
#33820 = ORIENTED_EDGE ( 'NONE', *, *, #65918, .F. ) ;
#33821 = CIRCLE ( 'NONE', #49334, 8.000000000000000000 ) ;
#33822 = CARTESIAN_POINT ( 'NONE',  ( 0.000000000000000000, -8.000000000000000000, 0.000000000000000000 ) ) ;
#33823 = CIRCLE ( 'NONE', #68217, 15.00000000000001243 ) ;
#33824 = CARTESIAN_POINT ( 'NONE',  ( 7.562131307723813478, 54.28093583783773823, 2.009306609246827691 ) ) ;
#33825 = CARTESIAN_POINT ( 'NONE',  ( 30.87955015324946828, 351.7733141111877444, 20.67482462247657082 ) ) ;
#33826 = AXIS2_PLACEMENT_3D ( 'NONE', #17860, #44254, #2169 ) ;
#33827 = FILL_AREA_STYLE ('',( #19792 ) ) ;
#33828 = DIRECTION ( 'NONE',  ( 0.000000000000000000, 0.000000000000000000, -1.000000000000000000 ) ) ;
#33829 = CARTESIAN_POINT ( 'NONE',  ( 21.36650669486618881, 4.000000000000003553, 4.898587196589414801E-16 ) ) ;
#33830 = VERTEX_POINT ( 'NONE', #60061 ) ;
#33831 = CARTESIAN_POINT ( 'NONE',  ( 4.980618096941788586, -46.46097021954796702, 103.2912570477108858 ) ) ;
#33832 = CARTESIAN_POINT ( 'NONE',  ( 0.000000000000000000, 0.1588408748199928722, 15.14825148316532832 ) ) ;
#33833 = VERTEX_POINT ( 'NONE', #60586 ) ;
#33834 = CARTESIAN_POINT ( 'NONE',  ( 47.39620038011970138, -30.00000000026522784, 59.33786523996079865 ) ) ;
#33835 = CARTESIAN_POINT ( 'NONE',  ( 47.78242936231066551, 10.33916499670818645, 16.83675847388925106 ) ) ;
#33836 = CIRCLE ( 'NONE', #69987, 4.000000000000000888 ) ;
#33837 = CARTESIAN_POINT ( 'NONE',  ( 24.46940115168818508, 25.33847118171375712, -31.99855969730282368 ) ) ;
#33838 = TOROIDAL_SURFACE ( 'NONE', #13076, 7.500000000000006217, 5.000000000000000000 ) ;
#33839 = DIRECTION ( 'NONE',  ( 0.000000000000000000, 0.000000000000000000, 1.000000000000000000 ) ) ;
#33840 = CARTESIAN_POINT ( 'NONE',  ( 81.10868664982288578, -29.99999999999999645, 22.89651086349327258 ) ) ;
#33841 =( BOUNDED_SURFACE ( )  B_SPLINE_SURFACE ( 3, 2, ( 
 ( #56621, #15636, #48528 ),
 ( #25920, #106769, #41511 ),
 ( #74397, #17259, #17788 ),
 ( #50638, #83559, #81420 ),
 ( #101874, #60382, #36657 ),
 ( #77609, #51182, #94332 ),
 ( #93257, #69521, #102413 ),
 ( #28556, #61440, #19420 ),
 ( #86252, #20495, #11252 ),
 ( #68998, #12326, #59848 ),
 ( #52253, #45251, #53334 ),
 ( #93794, #78129, #92717 ) ),
 .UNSPECIFIED., .F., .F., .T. ) 
 B_SPLINE_SURFACE_WITH_KNOTS ( ( 4, 2, 2, 2, 2, 4 ),
 ( 3, 3 ),
 ( 1.517883041479706208E-18, 0.001471464792626227692, 0.002942929585252453649, 0.003678661981565566844, 0.004414394377878680040, 0.005885859170504905563 ),
 ( 0.000000000000000000, 1.000000000000000000 ),
 .UNSPECIFIED. ) 
 GEOMETRIC_REPRESENTATION_ITEM ( )  RATIONAL_B_SPLINE_SURFACE ( (
 ( 1.000000000000000000, 0.8274249441183813003, 1.000000000000000000),
 ( 1.000000000000000000, 0.8369779515087686361, 1.000000000000000000),
 ( 1.000000000000000000, 0.8428664650350916610, 1.000000000000000000),
 ( 1.000000000000000000, 0.8506961607560086236, 1.000000000000000000),
 ( 1.000000000000000000, 0.8526029425209923351, 1.000000000000000000),
 ( 1.000000000000000000, 0.8531612821182233963, 1.000000000000000000),
 ( 1.000000000000000000, 0.8529462785849180051, 1.000000000000000000),
 ( 1.000000000000000000, 0.8517601151911999846, 1.000000000000000000),
 ( 1.000000000000000000, 0.8507906177106665524, 1.000000000000000000),
 ( 1.000000000000000000, 0.8467143344643495162, 1.000000000000000000),
 ( 1.000000000000000000, 0.8424736042941722847, 1.000000000000000000),
 ( 1.000000000000000000, 0.8360809698953560742, 1.000000000000000000) ) ) 
 REPRESENTATION_ITEM ( '' )  SURFACE ( )  );
#33842 = CARTESIAN_POINT ( 'NONE',  ( 7.986452802927059835, 101.0269024230811539, 0.5332468218996369025 ) ) ;
#33843 = EDGE_LOOP ( 'NONE', ( #40785, #19533 ) ) ;
#33844 = EDGE_LOOP ( 'NONE', ( #18933, #76907, #38125, #43561 ) ) ;
#33845 = VERTEX_POINT ( 'NONE', #16929 ) ;
#33846 = AXIS2_PLACEMENT_3D ( 'NONE', #96983, #73213, #30686 ) ;
#33847 = CARTESIAN_POINT ( 'NONE',  ( -46.79015243495860688, 13.37233443428283053, -15.81143384442421151 ) ) ;
#33848 = CARTESIAN_POINT ( 'NONE',  ( -6.912476948941361776, 40.56175638174910603, -71.08408186729455736 ) ) ;
#33849 = CARTESIAN_POINT ( 'NONE',  ( 19.83349330513380693, 1.593028355512270962E-15, 0.000000000000000000 ) ) ;
#33850 = FACE_OUTER_BOUND ( 'NONE', #71290, .T. ) ;
#33851 = DIRECTION ( 'NONE',  ( -1.000000000000000000, -1.224606353822377258E-16, -0.000000000000000000 ) ) ;
#33852 = VERTEX_POINT ( 'NONE', #33648 ) ;
#33854 = EDGE_CURVE ( 'NONE', #19188, #71499, #49806, .T. ) ;
#33853 = CARTESIAN_POINT ( 'NONE',  ( 23.58349330513380337, 1.593028355512270567E-15, 0.000000000000000000 ) ) ;
#33855 = ORIENTED_EDGE ( 'NONE', *, *, #7689, .T. ) ;
#33856 = CARTESIAN_POINT ( 'NONE',  ( 0.000000000000000000, 15.00000000000000000, 0.000000000000000000 ) ) ;
#33857 = CARTESIAN_POINT ( 'NONE',  ( 74.25335412531610757, -38.32804716266574019, 162.5607055868849500 ) ) ;
#33858 = CARTESIAN_POINT ( 'NONE',  ( 6.445370176742044599, 4.584736124524362744, -5.738941594274773905 ) ) ;
#33859 = CARTESIAN_POINT ( 'NONE',  ( 32.37165988990192744, 299.8773295831273344, 3.063193199593787330 ) ) ;
#33860 = CIRCLE ( 'NONE', #94109, 4.000000000000000888 ) ;
#33861 = CARTESIAN_POINT ( 'NONE',  ( -2.896852679609707160E-16, -5.309483803148803638, -3.803704290982251379 ) ) ;
#33862 = AXIS2_PLACEMENT_3D ( 'NONE', #25052, #99969, #91368 ) ;
#33863 = CARTESIAN_POINT ( 'NONE',  ( -27.86725909167721937, 34.24694088119783686, -9.811934799320198408 ) ) ;
#33864 = CARTESIAN_POINT ( 'NONE',  ( 42.69811214730273718, 434.9611672192513652, 18.34625614733210242 ) ) ;
#33865 = ADVANCED_FACE ( 'NONE', ( #8815 ), #73985, .T. ) ;
#33866 = CARTESIAN_POINT ( 'NONE',  ( 0.000000000000000000, 4.898587196589412829E-16, -4.000000000000000000 ) ) ;
#33867 = CYLINDRICAL_SURFACE ( 'NONE', #81468, 1.250000000000000222 ) ;
#33868 = EDGE_LOOP ( 'NONE', ( #25305, #51077 ) ) ;
#33870 = CARTESIAN_POINT ( 'NONE',  ( 4.684273348644264514E-15, 28.20649408426940141, 38.25000000000000000 ) ) ;
#33869 = PRESENTATION_STYLE_ASSIGNMENT (( #75889 ) ) ;
#33871 = CARTESIAN_POINT ( 'NONE',  ( 29.08076923076923137, 4.172000000000003261, 5.109226446042759579E-16 ) ) ;
#33872 = CARTESIAN_POINT ( 'NONE',  ( 94.26467260280679739, 6.123233995736582872E-16, -5.000000000000011546 ) ) ;
#33873 = CARTESIAN_POINT ( 'NONE',  ( 34.12349128637467999, 490.8027302422241860, 11.84948222508893068 ) ) ;
#33874 = CARTESIAN_POINT ( 'NONE',  ( 3.945802338410542731, 299.4462438666951698, 9.201290498665041895 ) ) ;
#33875 = CARTESIAN_POINT ( 'NONE',  ( 46.00000000000000000, 463.6369139993324211, 9.775485381103553806 ) ) ;
#33876 = CARTESIAN_POINT ( 'NONE',  ( 86.34082203149947077, -21.01137834141258409, 180.7326751960264630 ) ) ;
#33877 = DIRECTION ( 'NONE',  ( -1.000000000000000000, -1.224606353822377258E-16, -0.000000000000000000 ) ) ;
#33878 = EDGE_CURVE ( 'NONE', #46568, #104224, #72221, .T. ) ;
#33879 = AXIS2_PLACEMENT_3D ( 'NONE', #104821, #80002, #72448 ) ;
#33880 = CARTESIAN_POINT ( 'NONE',  ( 2.494577234427376227E-15, -18.92596047533412573, 20.36976895023282097 ) ) ;
#33881 = VERTEX_POINT ( 'NONE', #75130 ) ;
#33882 = CARTESIAN_POINT ( 'NONE',  ( 94.66746555106050209, -57.65776586346519395, -9.025452738816129639 ) ) ;
#33883 = FACE_OUTER_BOUND ( 'NONE', #8610, .T. ) ;
#33884 = CARTESIAN_POINT ( 'NONE',  ( 16.75187969033515145, 34.25544727262118982, -24.30698433968624883 ) ) ;
#33885 = CARTESIAN_POINT ( 'NONE',  ( 5.656854249492378806, -18.68749999999999289, 5.656854249492381470 ) ) ;
#33886 = EDGE_CURVE ( 'NONE', #13401, #90391, #105185, .T. ) ;
#33887 = CARTESIAN_POINT ( 'NONE',  ( -80.92579118157559037, -29.99999999999999645, 5.338923669854157339 ) ) ;
#33888 =( GEOMETRIC_REPRESENTATION_CONTEXT ( 3 ) GLOBAL_UNCERTAINTY_ASSIGNED_CONTEXT ( ( #18143 ) ) GLOBAL_UNIT_ASSIGNED_CONTEXT ( ( #43549, #99647, #76429 ) ) REPRESENTATION_CONTEXT ( 'NONE', 'WORKASPACE' ) );
#33889 = VECTOR ( 'NONE', #14489, 1000.000000000000114 ) ;
#33890 =( NAMED_UNIT ( * ) PLANE_ANGLE_UNIT ( ) SI_UNIT ( $, .RADIAN. ) );
#33891 = CARTESIAN_POINT ( 'NONE',  ( 0.000000000000000000, 0.000000000000000000, -5.703399999999999359 ) ) ;
#33892 = CARTESIAN_POINT ( 'NONE',  ( -7.298354728638307698, 4.926141412640832051, -7.913704048100022703 ) ) ;
#33894 =( NAMED_UNIT ( * ) SI_UNIT ( $, .STERADIAN. ) SOLID_ANGLE_UNIT ( ) );
#33893 =( NAMED_UNIT ( * ) SI_UNIT ( $, .STERADIAN. ) SOLID_ANGLE_UNIT ( ) );
#33895 = EDGE_CURVE ( 'NONE', #22182, #101681, #52961, .T. ) ;
#33896 =( NAMED_UNIT ( * ) PLANE_ANGLE_UNIT ( ) SI_UNIT ( $, .RADIAN. ) );
#33897 = CARTESIAN_POINT ( 'NONE',  ( -28.73029465396694349, 18.79238081053094334, 40.04376963015451452 ) ) ;
#33898 =( NAMED_UNIT ( * ) SI_UNIT ( $, .STERADIAN. ) SOLID_ANGLE_UNIT ( ) );
#33899 = CARTESIAN_POINT ( 'NONE',  ( 5.980543423763064581, -81.02903592498923047, -0.5500789318242851333 ) ) ;
#33900 = CARTESIAN_POINT ( 'NONE',  ( 0.000000000000000000, 0.000000000000000000, 0.000000000000000000 ) ) ;
#33901 = CARTESIAN_POINT ( 'NONE',  ( -43.03185303983481447, 485.3613526602391062, 6.073233449168579767 ) ) ;
#33902 = STYLED_ITEM ( 'NONE', ( #84773 ), #24056 ) ;
#33903 = AXIS2_PLACEMENT_3D ( 'NONE', #65711, #7988, #48445 ) ;
#33904 = AXIS2_PLACEMENT_3D ( 'NONE', #51313, #38746, #95915 ) ;
#33905 = VECTOR ( 'NONE', #89089, 1000.000000000000227 ) ;
#33906 = CARTESIAN_POINT ( 'NONE',  ( 69.77959388908855942, -29.97820759226561194, -20.83712817169497811 ) ) ;
#33907 = EDGE_CURVE ( 'NONE', #49140, #9363, #87720, .T. ) ;
#33908 = ORIENTED_EDGE ( 'NONE', *, *, #20768, .F. ) ;
#33909 = CARTESIAN_POINT ( 'NONE',  ( 6.560102024233679607, 9.829711121158393183, 2.452861370513718331 ) ) ;
#33910 = SURFACE_STYLE_FILL_AREA ( #9053 ) ;
#33911 = AXIS2_PLACEMENT_3D ( 'NONE', #104312, #55223, #70897 ) ;
#33912 = CARTESIAN_POINT ( 'NONE',  ( -7.413471587080149305, 82.35647840831674671, -3.013058070223552765 ) ) ;
#33913 = CARTESIAN_POINT ( 'NONE',  ( -61.99390519559347013, -29.47934043886439071, -24.25302986929749949 ) ) ;
#33915 = CARTESIAN_POINT ( 'NONE',  ( 37.50843704408828216, 482.0135999900019215, 15.15320708953895057 ) ) ;
#33914 = DIRECTION ( 'NONE',  ( -1.000000000000000000, -1.224606353822377258E-16, -0.000000000000000000 ) ) ;
#33916 = ORIENTED_EDGE ( 'NONE', *, *, #16474, .T. ) ;
#33917 = DIRECTION ( 'NONE',  ( 0.000000000000000000, 0.000000000000000000, 1.000000000000000000 ) ) ;
#33918 = ORIENTED_EDGE ( 'NONE', *, *, #46194, .T. ) ;
#33919 = CARTESIAN_POINT ( 'NONE',  ( -25.85870200593686263, 35.03474222141309724, 8.998851137906763498 ) ) ;
#33920 = CARTESIAN_POINT ( 'NONE',  ( 19.29515645702225868, 1.482358050883964840E-15, 0.000000000000000000 ) ) ;
#33921 = FACE_OUTER_BOUND ( 'NONE', #37019, .T. ) ;
#33922 = CARTESIAN_POINT ( 'NONE',  ( -88.11432633863014985, -59.99999999999999289, -21.44888580323229377 ) ) ;
#33923 = EDGE_LOOP ( 'NONE', ( #101404, #93639, #24786 ) ) ;
#33924 = PRESENTATION_STYLE_ASSIGNMENT (( #2576 ) ) ;
#33925 = CARTESIAN_POINT ( 'NONE',  ( -7.807718295557010357, 53.96912438917611610, -3.792492973880838836 ) ) ;
#33926 = CARTESIAN_POINT ( 'NONE',  ( 102.2338188462963871, -60.19688077974823415, 193.9243752497099536 ) ) ;
#33928 = CARTESIAN_POINT ( 'NONE',  ( 82.42421628608209971, -2.002967142162725287E-29, 5.000000000000011546 ) ) ;
#33927 = DIRECTION ( 'NONE',  ( -1.000000000000000000, -1.224606353822377258E-16, -0.000000000000000000 ) ) ;
#33929 = VECTOR ( 'NONE', #80062, 1000.000000000000000 ) ;
#33930 = EDGE_LOOP ( 'NONE', ( #12923, #102757, #99006, #1506 ) ) ;
#33931 = EDGE_LOOP ( 'NONE', ( #94351, #60635, #65397, #63388 ) ) ;
#33932 = CIRCLE ( 'NONE', #94206, 7.000000000000000000 ) ;
#33933 = EDGE_CURVE ( 'NONE', #27223, #28630, #103260, .T. ) ;
#33934 = ORIENTED_EDGE ( 'NONE', *, *, #1070, .T. ) ;
#33935 = CARTESIAN_POINT ( 'NONE',  ( 32.16709058540200772, 380.6344658977095605, 24.65337216308995139 ) ) ;
#33936 = EDGE_CURVE ( 'NONE', #35336, #8054, #73905, .T. ) ;
#33937 = CARTESIAN_POINT ( 'NONE',  ( -38.85446894546474539, 460.8903912184078422, 2.218456751110488678 ) ) ;
#33938 = CARTESIAN_POINT ( 'NONE',  ( 9.559166278073435663, 53.41734968321387100, 3.549940974394473425 ) ) ;
#33939 = EDGE_LOOP ( 'NONE', ( #52474, #35243, #41141, #60683, #80113 ) ) ;
#33940 = CARTESIAN_POINT ( 'NONE',  ( 15.88102029263265003, 46.13028405480692129, -4.403441971141990763 ) ) ;
#33941 = CARTESIAN_POINT ( 'NONE',  ( 70.41111111111112564, 3.309500000000014541, 4.052968581778174646E-16 ) ) ;
#33942 = CARTESIAN_POINT ( 'NONE',  ( -11.27550409577679247, -60.00000000000000000, -44.73582912082186169 ) ) ;
#33943 = CARTESIAN_POINT ( 'NONE',  ( -7.188101187500000044, -31.90625000204838813, -8.802885111219163269E-16 ) ) ;
#33944 = CARTESIAN_POINT ( 'NONE',  ( -29.87369781377633515, 13.22774345441025190, 42.09617408282262829 ) ) ;
#33945 = FACE_BOUND ( 'NONE', #105798, .T. ) ;
#33946 = CARTESIAN_POINT ( 'NONE',  ( 11.84999999999999787, 3.309500000000003439, 4.052968581778167743E-16 ) ) ;
#33947 = ADVANCED_FACE ( 'NONE', ( #61611 ), #85888, .T. ) ;
#33948 = CARTESIAN_POINT ( 'NONE',  ( -86.99605493950913626, -14.21045842199422005, 24.11595694609475160 ) ) ;
#33949 = ADVANCED_FACE ( 'NONE', ( #102580 ), #28201, .T. ) ;
#33950 = DIRECTION ( 'NONE',  ( 0.000000000000000000, 0.000000000000000000, 1.000000000000000000 ) ) ;
#33951 = CARTESIAN_POINT ( 'NONE',  ( -49.62087710221392456, -39.51757389364818351, 50.13317839744063065 ) ) ;
#33952 = DIRECTION ( 'NONE',  ( -0.000000000000000000, -1.000000000000000000, -0.000000000000000000 ) ) ;
#33953 = ORIENTED_EDGE ( 'NONE', *, *, #19524, .F. ) ;
#33954 = CARTESIAN_POINT ( 'NONE',  ( 12.50000000000000533, 9.372078270843420711, -27.37193597126559297 ) ) ;
#33955 = CARTESIAN_POINT ( 'NONE',  ( -4.913676358978594116, 296.1360674233372379, -10.01007018187696218 ) ) ;
#33956 = CARTESIAN_POINT ( 'NONE',  ( 12.28004307584039623, -2.771121092977573586, 20.68249676638044932 ) ) ;
#33957 = ORIENTED_EDGE ( 'NONE', *, *, #42907, .F. ) ;
#33958 = CARTESIAN_POINT ( 'NONE',  ( 4.589925132946512498, 248.9347398370747158, 3.864926970398271155 ) ) ;
#33959 = AXIS2_PLACEMENT_3D ( 'NONE', #63303, #5056, #12073 ) ;
#33960 = CARTESIAN_POINT ( 'NONE',  ( 104.6430114620182081, -38.40051020932904180, 197.8370924372202637 ) ) ;
#33961 = CARTESIAN_POINT ( 'NONE',  ( 48.02835407290545078, 16.78162100668605206, 14.35535821593427386 ) ) ;
#33962 = CARTESIAN_POINT ( 'NONE',  ( 22.25669491856071858, -5.000000000000000000, 6.123233995736768255E-16 ) ) ;
#33963 = CARTESIAN_POINT ( 'NONE',  ( 0.000000000000000000, 0.000000000000000000, -2.868028571428571372 ) ) ;
#33964 = CARTESIAN_POINT ( 'NONE',  ( 89.31065340740984482, -30.00000000000000000, 189.1380160600958789 ) ) ;
#33965 = CARTESIAN_POINT ( 'NONE',  ( 34.84618260875171103, 489.9833681528626244, 11.97975507378817994 ) ) ;
#33966 = SURFACE_STYLE_USAGE ( .BOTH. , #25341 ) ;
#33967 = CARTESIAN_POINT ( 'NONE',  ( 55.74444444444444713, 6.915964383211875250E-15, 0.000000000000000000 ) ) ;
#33968 = ORIENTED_EDGE ( 'NONE', *, *, #78143, .F. ) ;
#33969 = ORIENTED_EDGE ( 'NONE', *, *, #1262, .T. ) ;
#33970 = CARTESIAN_POINT ( 'NONE',  ( 51.98390228014496728, -36.04151142941384478, 52.98091492913632550 ) ) ;
#33971 = CARTESIAN_POINT ( 'NONE',  ( 5.902962692465450800, 41.87327339699977813, -59.02279353628207303 ) ) ;
#33972 = CIRCLE ( 'NONE', #94235, 4.000000000000000888 ) ;
#33973 = CARTESIAN_POINT ( 'NONE',  ( 9.539304943379745438, 51.45347982738971382, 1.988540865056009022 ) ) ;
#33974 = ORIENTED_EDGE ( 'NONE', *, *, #51604, .F. ) ;
#33976 = ADVANCED_FACE ( 'NONE', ( #86943 ), #10177, .F. ) ;
#33975 = CARTESIAN_POINT ( 'NONE',  ( -92.63712589027728939, -38.35495981404815069, 40.41764578554981568 ) ) ;
#33977 = ORIENTED_EDGE ( 'NONE', *, *, #67044, .T. ) ;
#33978 = CARTESIAN_POINT ( 'NONE',  ( 15.82318872385758546, 4.444012391148053354, 4.874853782833517002 ) ) ;
#33979 = CARTESIAN_POINT ( 'NONE',  ( 92.04444232229207046, -38.35407781392872550, 35.16507766400177815 ) ) ;
#33980 = CARTESIAN_POINT ( 'NONE',  ( 13.52808898108708568, 24.65652623284792000, 1.487090316686600744 ) ) ;
#33982 = CARTESIAN_POINT ( 'NONE',  ( 89.89243487226349316, -52.71666739316034977, 62.30352106449856109 ) ) ;
#33981 = VECTOR ( 'NONE', #2236, 1000.000000000000000 ) ;
#33983 = CARTESIAN_POINT ( 'NONE',  ( -17.89642918806200100, 43.18034132965723870, -5.550938134534490587 ) ) ;
#33984 = AXIS2_PLACEMENT_3D ( 'NONE', #5112, #11586, #44513 ) ;
#33985 = CARTESIAN_POINT ( 'NONE',  ( 32.66130572512987129, 465.7845731394320978, 12.51261058352552880 ) ) ;
#33987 = STYLED_ITEM ( 'NONE', ( #79273 ), #37228 ) ;
#33986 = CARTESIAN_POINT ( 'NONE',  ( -35.34007772701297512, 353.1885634555609954, 1.120430972263593672 ) ) ;
#33988 = PLANE ( 'NONE',  #74604 ) ;
#33989 = CARTESIAN_POINT ( 'NONE',  ( 76.53976976327565751, -60.00000000000000000, 189.0222597737091803 ) ) ;
#33990 = EDGE_CURVE ( 'NONE', #48389, #98734, #47904, .T. ) ;
#33991 = CARTESIAN_POINT ( 'NONE',  ( 12.79230769230769305, 1.411358822780289120E-15, 0.000000000000000000 ) ) ;
#33992 = AXIS2_PLACEMENT_3D ( 'NONE', #22771, #23839, #15172 ) ;
#33993 = CARTESIAN_POINT ( 'NONE',  ( 17.71556303271838928, 45.00000000000000711, 62.84553702592653224 ) ) ;
#33994 = EDGE_LOOP ( 'NONE', ( #23980, #77848, #20644, #97111, #91416, #16030 ) ) ;
#33995 = CARTESIAN_POINT ( 'NONE',  ( 60.00046932338042893, -60.33652138363083850, 82.29518702760771021 ) ) ;
#33996 = CARTESIAN_POINT ( 'NONE',  ( -23.61536189776495220, 303.4785653241179375, -9.865317176963937840 ) ) ;
#33997 = EDGE_CURVE ( 'NONE', #32226, #105963, #47282, .T. ) ;
#33998 = DIRECTION ( 'NONE',  ( -1.000000000000000000, -1.224606353822377258E-16, -0.000000000000000000 ) ) ;
#33999 = CARTESIAN_POINT ( 'NONE',  ( -9.434035901591116158, -5.000000000000000888, -19.23908757048410578 ) ) ;
#34000 = CARTESIAN_POINT ( 'NONE',  ( 6.249999999999998224, -4.618802153517012954, -8.000000000000001776 ) ) ;
#34001 = CARTESIAN_POINT ( 'NONE',  ( -40.94307380459559198, 409.3606216529898916, 27.70111150611745998 ) ) ;
#34002 = CARTESIAN_POINT ( 'NONE',  ( -38.81333125807601903, 25.21178128392378071, -12.01546574933351330 ) ) ;
#34003 = DIRECTION ( 'NONE',  ( -1.000000000000000000, -1.224606353822377258E-16, -0.000000000000000000 ) ) ;
#34004 = CARTESIAN_POINT ( 'NONE',  ( 4.898587196589412829E-16, -25.62499999999999645, -8.000000000000000000 ) ) ;
#34005 = CARTESIAN_POINT ( 'NONE',  ( -17.49999999999996447, 46.94999999999998153, 62.61746187599676716 ) ) ;
#34006 = CARTESIAN_POINT ( 'NONE',  ( 16.32476346754885554, 43.58736234942514898, -6.626941870814922808 ) ) ;
#34007 = ORIENTED_EDGE ( 'NONE', *, *, #23207, .T. ) ;
#34008 = CARTESIAN_POINT ( 'NONE',  ( 82.38523181566540643, -57.17260357990272723, 186.5832430736296885 ) ) ;
#34009 = EDGE_CURVE ( 'NONE', #31379, #38179, #39321, .T. ) ;
#34010 = DIRECTION ( 'NONE',  ( -1.000000000000000000, -0.000000000000000000, -0.000000000000000000 ) ) ;
#34011 = CARTESIAN_POINT ( 'NONE',  ( -39.82817075493480274, 438.7291009509302171, 23.10551559802240718 ) ) ;
#34012 = ORIENTED_EDGE ( 'NONE', *, *, #31850, .F. ) ;
#34013 = CARTESIAN_POINT ( 'NONE',  ( -3.313708498984760720, -33.21875000409677625, -8.000000000000000000 ) ) ;
#34014 = CARTESIAN_POINT ( 'NONE',  ( 42.89842744804999342, 435.5680593355373276, 8.824050052262007782 ) ) ;
#34015 = FILL_AREA_STYLE_COLOUR ( '', #36630 ) ;
#34016 = CARTESIAN_POINT ( 'NONE',  ( 14.33052326666366838, -3.000000000000002665, -89.63170281049063703 ) ) ;
#34017 = CARTESIAN_POINT ( 'NONE',  ( -18.64535684107481472, -25.34425824956045048, -38.50098957481070983 ) ) ;
#34018 =( NAMED_UNIT ( * ) PLANE_ANGLE_UNIT ( ) SI_UNIT ( $, .RADIAN. ) );
#34019 = EDGE_CURVE ( 'NONE', #45187, #42880, #7440, .T. ) ;
#34020 = FILL_AREA_STYLE_COLOUR ( '', #61039 ) ;
#34021 = CARTESIAN_POINT ( 'NONE',  ( 50.11026576053689752, -60.00000000000000000, 72.06894001542156047 ) ) ;
#34022 = DIRECTION ( 'NONE',  ( 0.000000000000000000, -1.000000000000000000, 0.000000000000000000 ) ) ;
#34023 = CARTESIAN_POINT ( 'NONE',  ( 19.18487022566833033, -16.76851763133264583, 31.49200998272180030 ) ) ;
#34024 = ADVANCED_FACE ( 'NONE', ( #38274 ), #71133, .F. ) ;
#34025 = CIRCLE ( 'NONE', #35799, 3.309500000000001663 ) ;
#34027 = CARTESIAN_POINT ( 'NONE',  ( -13.77345804302984789, 22.96215306780717924, -1.017947650526750181 ) ) ;
#34026 = CARTESIAN_POINT ( 'NONE',  ( -25.34519795292129629, -29.27581004272202136, 38.40335314319461446 ) ) ;
#34028 = CARTESIAN_POINT ( 'NONE',  ( -9.253583916535172094, 86.29803908005033009, 3.792462592445556169 ) ) ;
#34029 = CARTESIAN_POINT ( 'NONE',  ( -7.188101187500001821, -12.50000000204838990, -2.977408999572651371 ) ) ;
#34030 = CARTESIAN_POINT ( 'NONE',  ( 27.42790055916795566, 296.3899668198013160, -1.667331554639347013 ) ) ;
#34031 = CARTESIAN_POINT ( 'NONE',  ( 4.284822031654965890, -1.092833614412281218, 104.4267991316945086 ) ) ;
#34032 = ORIENTED_EDGE ( 'NONE', *, *, #63982, .T. ) ;
#34033 = COLOUR_RGB ( '', 0.66274510, 0.83137255, 0.94901961) ;
#34034 = CARTESIAN_POINT ( 'NONE',  ( -18.95009564030707949, 49.33583170005315566, 62.02326760999472555 ) ) ;
#34035 = ADVANCED_FACE ( 'NONE', ( #24211 ), #58132, .T. ) ;
#34036 = CARTESIAN_POINT ( 'NONE',  ( 0.000000000000000000, 70.00000000000000000, 0.000000000000000000 ) ) ;
#34037 = FILL_AREA_STYLE_COLOUR ( '', #30363 ) ;
#34039 = CARTESIAN_POINT ( 'NONE',  ( 50.18622294521377114, -34.58945973367626436, -27.70670043957319706 ) ) ;
#34038 = CARTESIAN_POINT ( 'NONE',  ( 4.278063764781172118, 54.28324999937112239, 6.542721817263923434 ) ) ;
#34040 = ORIENTED_EDGE ( 'NONE', *, *, #2395, .F. ) ;
#34041 = CARTESIAN_POINT ( 'NONE',  ( -5.982126593009819970, -88.97334227892930869, 0.5333292889181888707 ) ) ;
#34042 = VECTOR ( 'NONE', #67730, 1000.000000000000000 ) ;
#34043 = CIRCLE ( 'NONE', #66746, 1.000000000000003331 ) ;
#34044 = EDGE_LOOP ( 'NONE', ( #97639, #39035, #57099, #48398 ) ) ;
#34045 = DIRECTION ( 'NONE',  ( 1.000000000000000000, -0.000000000000000000, -0.000000000000000000 ) ) ;
#34046 = CARTESIAN_POINT ( 'NONE',  ( -6.641837642500876271, 41.74662713182689089, -59.04567091375639620 ) ) ;
#34047 = CARTESIAN_POINT ( 'NONE',  ( -19.68889612315570048, 41.86194541559208204, -80.13187903333529505 ) ) ;
#34048 = CARTESIAN_POINT ( 'NONE',  ( -103.7179628943768535, -60.00000000000000711, 102.7867851543608140 ) ) ;
#34049 = AXIS2_PLACEMENT_3D ( 'NONE', #24613, #74183, #49373 ) ;
#34050 = CARTESIAN_POINT ( 'NONE',  ( -30.00000000000000000, 0.000000000000000000, 0.000000000000000000 ) ) ;
#34051 = DIRECTION ( 'NONE',  ( -1.000000000000000000, -0.000000000000000000, -0.000000000000000000 ) ) ;
#34052 = VECTOR ( 'NONE', #57781, 1000.000000000000000 ) ;
#34053 = CARTESIAN_POINT ( 'NONE',  ( 20.24579557674108088, 304.8297271373347144, -10.00469232190996749 ) ) ;
#34054 = CARTESIAN_POINT ( 'NONE',  ( -4.051286199644062336, -48.60127012969241633, 103.8758286790404810 ) ) ;
#34056 = CARTESIAN_POINT ( 'NONE',  ( 5.299999999999999822, 7.505553499465139389, 0.000000000000000000 ) ) ;
#34055 = CARTESIAN_POINT ( 'NONE',  ( -7.996668422906947349, -3.000000000000002665, -91.14546720082398679 ) ) ;
#34057 = CARTESIAN_POINT ( 'NONE',  ( -83.14853206027666488, -39.48440948074397738, 171.2778937662942838 ) ) ;
#34058 = ORIENTED_EDGE ( 'NONE', *, *, #105684, .F. ) ;
#34059 = CARTESIAN_POINT ( 'NONE',  ( 6.457005528859116161, 41.52802923978755700, -70.63630686878374831 ) ) ;
#34060 = ORIENTED_EDGE ( 'NONE', *, *, #43950, .T. ) ;
#34061 = VERTEX_POINT ( 'NONE', #92093 ) ;
#34062 = CIRCLE ( 'NONE', #94334, 3.309500000000001663 ) ;
#34063 = DIRECTION ( 'NONE',  ( 0.000000000000000000, 0.000000000000000000, -1.000000000000000000 ) ) ;
#34064 = EDGE_CURVE ( 'NONE', #74993, #76425, #31845, .T. ) ;
#34065 = LINE ( 'NONE', #83106, #30193 ) ;
#34066 = VERTEX_POINT ( 'NONE', #74833 ) ;
#34067 = AXIS2_PLACEMENT_3D ( 'NONE', #99919, #50822, #19054 ) ;
#34068 = CARTESIAN_POINT ( 'NONE',  ( 0.000000000000000000, 0.000000000000000000, 0.000000000000000000 ) ) ;
#34069 =( NAMED_UNIT ( * ) PLANE_ANGLE_UNIT ( ) SI_UNIT ( $, .RADIAN. ) );
#34070 = CYLINDRICAL_SURFACE ( 'NONE', #24970, 5.000000000000000888 ) ;
#34071 = CARTESIAN_POINT ( 'NONE',  ( -3.010034769234505525, 15.20602481743756051, 6.322865676976533678 ) ) ;
#34072 = CARTESIAN_POINT ( 'NONE',  ( 43.55333112596303380, 465.2342844084865874, 9.238213423009675296 ) ) ;
#34073 = CARTESIAN_POINT ( 'NONE',  ( -13.93074145947618447, -50.20627081601409714, 28.41232622077120595 ) ) ;
#34074 = CARTESIAN_POINT ( 'NONE',  ( -5.000000000000000000, -14.08124958900141621, 11.76357069870068628 ) ) ;
#34075 = ADVANCED_FACE ( 'NONE', ( #33354 ), #15476, .T. ) ;
#34076 = CARTESIAN_POINT ( 'NONE',  ( 99.06540890750190442, -59.99999999999989342, 60.62284496578245552 ) ) ;
#34077 = CARTESIAN_POINT ( 'NONE',  ( -114.4520492995273315, -60.00000000000003553, 166.3968728284598342 ) ) ;
#34078 = CARTESIAN_POINT ( 'NONE',  ( -59.78161821688770061, -25.59841304440983478, 65.24320542831817704 ) ) ;
#34079 = AXIS2_PLACEMENT_3D ( 'NONE', #92980, #1823, #34783 ) ;
#34080 = ORIENTED_EDGE ( 'NONE', *, *, #67181, .T. ) ;
#34081 =( NAMED_UNIT ( * ) SI_UNIT ( $, .STERADIAN. ) SOLID_ANGLE_UNIT ( ) );
#34082 = CARTESIAN_POINT ( 'NONE',  ( 109.3871879777513669, -60.00000000001244871, 197.8688627231219073 ) ) ;
#34083 = ORIENTED_EDGE ( 'NONE', *, *, #90865, .F. ) ;
#34084 = CARTESIAN_POINT ( 'NONE',  ( 6.205941524835793643, -56.87779645166712328, 33.35922039782534654 ) ) ;
#34085 = CARTESIAN_POINT ( 'NONE',  ( -106.0491298257543775, -60.15510293424402732, 161.1420266926477325 ) ) ;
#34086 = CARTESIAN_POINT ( 'NONE',  ( -5.082755093536325042, -12.96875000204838280, -5.082755093536325930 ) ) ;
#34087 = CARTESIAN_POINT ( 'NONE',  ( 0.000000000000000000, -48.44948974278317877, 112.0000000000000000 ) ) ;
#34088 = CIRCLE ( 'NONE', #30611, 12.00000000000000711 ) ;
#34089 = DIRECTION ( 'NONE',  ( -0.000000000000000000, -1.000000000000000000, -0.000000000000000000 ) ) ;
#34090 = EDGE_LOOP ( 'NONE', ( #99751, #14018, #105368, #102199, #91711 ) ) ;
#34091 = CYLINDRICAL_SURFACE ( 'NONE', #4503, 4.000000000000000000 ) ;
#34092 = CARTESIAN_POINT ( 'NONE',  ( -75.18318468975571989, -59.99999999999997868, 182.6337824465098834 ) ) ;
#34093 = CARTESIAN_POINT ( 'NONE',  ( 36.37640517269390728, 26.07922816359034712, -11.81515425344730552 ) ) ;
#34094 = CARTESIAN_POINT ( 'NONE',  ( -7.188101187500001821, -18.87500000204838457, -2.977408999572651371 ) ) ;
#34095 = FACE_OUTER_BOUND ( 'NONE', #31495, .T. ) ;
#34096 = CIRCLE ( 'NONE', #63338, 0.5000000000000000000 ) ;
#34097 = SURFACE_STYLE_FILL_AREA ( #43217 ) ;
#34098 = CARTESIAN_POINT ( 'NONE',  ( 16.90652009647421394, -0.000000000000000000, 2.220657265755147325 ) ) ;
#34099 = CARTESIAN_POINT ( 'NONE',  ( 5.000000000000000000, -8.791602747472031965, -8.558960929452199551 ) ) ;
#34100 = CARTESIAN_POINT ( 'NONE',  ( -30.00000000000000355, 461.8423776372225689, 11.25810401088562607 ) ) ;
#34101 = CARTESIAN_POINT ( 'NONE',  ( -10.12089030649893395, 44.03014547783647004, -12.90779740156153643 ) ) ;
#34102 = CARTESIAN_POINT ( 'NONE',  ( -31.44127085143751188, 298.7743126848183692, -1.130929553568158052 ) ) ;
#34103 = CARTESIAN_POINT ( 'NONE',  ( -14.29190075645224844, 19.61368180394242700, -4.501023549838558679 ) ) ;
#34104 = CARTESIAN_POINT ( 'NONE',  ( -28.78195043134853037, -18.63874505867011777, 29.02999481432414797 ) ) ;
#34105 = B_SPLINE_CURVE_WITH_KNOTS ( 'NONE', 3,
 ( #77750, #2779, #28169, #54497, #3323 ),
 .UNSPECIFIED., .F., .F.,
 ( 4, 1, 4 ),
 ( 0.000000000000000000, 0.003752776749732570066, 0.007505553499465140131 ),
 .UNSPECIFIED. ) ;
#34106 = FACE_OUTER_BOUND ( 'NONE', #21982, .T. ) ;
#34107 = CARTESIAN_POINT ( 'NONE',  ( 46.21019612037324009, -25.69888004963982908, 41.24161030058627375 ) ) ;
#34108 = DIRECTION ( 'NONE',  ( -1.000000000000000000, -1.224606353822377258E-16, -0.000000000000000000 ) ) ;
#34109 = ORIENTED_EDGE ( 'NONE', *, *, #86587, .F. ) ;
#34111 = AXIS2_PLACEMENT_3D ( 'NONE', #58070, #26297, #66710 ) ;
#34110 = CARTESIAN_POINT ( 'NONE',  ( 43.22728423987868496, 434.6919775797230727, 9.646941480579668493 ) ) ;
#34112 = CARTESIAN_POINT ( 'NONE',  ( -76.71984652716008668, -38.43189599304911752, 182.9491387776208171 ) ) ;
#34113 = VERTEX_POINT ( 'NONE', #57060 ) ;
#34115 =( NAMED_UNIT ( * ) PLANE_ANGLE_UNIT ( ) SI_UNIT ( $, .RADIAN. ) );
#34114 = CARTESIAN_POINT ( 'NONE',  ( 0.000000000000000000, 0.000000000000000000, 0.000000000000000000 ) ) ;
#34116 = CARTESIAN_POINT ( 'NONE',  ( 55.18499737084820111, -59.99999999999997158, 69.25531299354273074 ) ) ;
#34117 = CARTESIAN_POINT ( 'NONE',  ( 15.51166181318966508, 36.90500793569743365, 23.41746243165347607 ) ) ;
#34118 = CARTESIAN_POINT ( 'NONE',  ( 6.222582369487715148, -4.088457415080688051, 6.499999999999999112 ) ) ;
#34119 = CARTESIAN_POINT ( 'NONE',  ( 34.05841483224278932, 462.4673622309109078, 4.856678830036404548 ) ) ;
#34120 = FACE_OUTER_BOUND ( 'NONE', #49580, .T. ) ;
#34121 = CARTESIAN_POINT ( 'NONE',  ( 5.094000037296078531, -87.44634123771227507, -3.174960020027664420 ) ) ;
#34122 = CARTESIAN_POINT ( 'NONE',  ( 108.8577760144673761, -60.00000000000000711, 134.9695025774865940 ) ) ;
#34123 = AXIS2_PLACEMENT_3D ( 'NONE', #77367, #2932, #3483 ) ;
#34124 = CARTESIAN_POINT ( 'NONE',  ( 22.61650669486618526, 0.000000000000000000, 4.000000000000000888 ) ) ;
#34125 = VERTEX_POINT ( 'NONE', #89976 ) ;
#34126 = EDGE_CURVE ( 'NONE', #826, #86797, #5183, .T. ) ;
#34127 = CARTESIAN_POINT ( 'NONE',  ( -86.67473478203353920, -30.00000000000003908, 182.4036165407476631 ) ) ;
#34128 = ORIENTED_EDGE ( 'NONE', *, *, #57441, .T. ) ;
#34129 = CARTESIAN_POINT ( 'NONE',  ( -5.075741750048029743, -4.332638003024074536, -17.09621982684887698 ) ) ;
#34130 = CARTESIAN_POINT ( 'NONE',  ( 27.95351751955323749, 311.8734759528393283, 11.86698417665069982 ) ) ;
#34132 = DIRECTION ( 'NONE',  ( 0.5735764363510491570, -0.8191520442889895781, 1.003171929053522035E-16 ) ) ;
#34131 = CIRCLE ( 'NONE', #59996, 4.000000000000001776 ) ;
#34133 = AXIS2_PLACEMENT_3D ( 'NONE', #103029, #62571, #84710 ) ;
#34134 = CARTESIAN_POINT ( 'NONE',  ( 7.188101187499999156, -21.12500000204838813, 2.977408999572654924 ) ) ;
#34135 = CARTESIAN_POINT ( 'NONE',  ( -7.000000000000000000, 8.572527594031471218E-16, -2.575493252495433261 ) ) ;
#34136 = AXIS2_PLACEMENT_3D ( 'NONE', #101803, #43047, #83489 ) ;
#34137 = CONICAL_SURFACE ( 'NONE', #65131, 18.72828050308589454, 0.7292773806962717931 ) ;
#34138 = DIRECTION ( 'NONE',  ( -0.000000000000000000, -1.000000000000000000, -0.000000000000000000 ) ) ;
#34139 = EDGE_LOOP ( 'NONE', ( #7534, #70689 ) ) ;
#34140 = CARTESIAN_POINT ( 'NONE',  ( 80.87394805517843110, -53.40757338515430774, 172.1382403962514331 ) ) ;
#34141 = VERTEX_POINT ( 'NONE', #83471 ) ;
#34142 = CARTESIAN_POINT ( 'NONE',  ( -0.9887154240794179261, 17.70149142468999770, -49.73206415546439985 ) ) ;
#34143 = CARTESIAN_POINT ( 'NONE',  ( 38.31542881513956189, 27.59987916515866857, -11.19254653711393566 ) ) ;
#34144 = CARTESIAN_POINT ( 'NONE',  ( 6.928203230275509661, 30.00000000000000000, 4.000000000000000000 ) ) ;
#34145 = CARTESIAN_POINT ( 'NONE',  ( -26.14413424799793262, 305.7334878758448440, 10.58890971036053941 ) ) ;
#34146 = FACE_OUTER_BOUND ( 'NONE', #79813, .T. ) ;
#34147 = ADVANCED_FACE ( 'NONE', ( #8515 ), #34460, .F. ) ;
#34148 = ORIENTED_EDGE ( 'NONE', *, *, #59518, .F. ) ;
#34149 = SURFACE_STYLE_FILL_AREA ( #66478 ) ;
#34150 = AXIS2_PLACEMENT_3D ( 'NONE', #59763, #50047, #9052 ) ;
#34151 = DIRECTION ( 'NONE',  ( 0.000000000000000000, 0.9900230405584208304, 0.1409055682485944594 ) ) ;
#34152 = FACE_OUTER_BOUND ( 'NONE', #58501, .T. ) ;
#34153 = CARTESIAN_POINT ( 'NONE',  ( 87.29183096894618643, -28.00114413134319946, 187.7157000835711642 ) ) ;
#34154 = EDGE_CURVE ( 'NONE', #98655, #34834, #66223, .T. ) ;
#34155 = CARTESIAN_POINT ( 'NONE',  ( 1.005674572306967995, 34.34876838514327346, -29.24676969006877769 ) ) ;
#34156 = CARTESIAN_POINT ( 'NONE',  ( 5.082755093536325930, -33.96875000204838813, -5.082755093536325042 ) ) ;
#34157 = DIRECTION ( 'NONE',  ( 0.000000000000000000, 0.000000000000000000, 1.000000000000000000 ) ) ;
#34158 = CARTESIAN_POINT ( 'NONE',  ( 0.000000000000000000, 34.19642918197134662, 0.000000000000000000 ) ) ;
#34159 = AXIS2_PLACEMENT_3D ( 'NONE', #6997, #47455, #80349 ) ;
#34160 = CARTESIAN_POINT ( 'NONE',  ( 41.97106272281727968, 437.4388437799331655, 21.41148611803419755 ) ) ;
#34161 = ORIENTED_EDGE ( 'NONE', *, *, #9492, .T. ) ;
#34162 = EDGE_CURVE ( 'NONE', #64324, #61408, #55042, .T. ) ;
#34163 = CARTESIAN_POINT ( 'NONE',  ( 1.218727205067523522, 43.73156354412988378, 17.17928489613208143 ) ) ;
#34164 = CARTESIAN_POINT ( 'NONE',  ( -10.01459525654357030, 7.479155813459358093, -4.999999999999987566 ) ) ;
#34165 =( BOUNDED_SURFACE ( )  B_SPLINE_SURFACE ( 3, 2, ( 
 ( #91160, #24832, #83563 ),
 ( #1020, #76007, #57686 ),
 ( #8617, #43122, #50139 ),
 ( #16718, #75477, #17266 ),
 ( #9665, #58784, #83047 ),
 ( #84109, #49607, #35057 ),
 ( #91679, #9139, #50645 ),
 ( #74407, #82514, #2107 ),
 ( #42050, #42578, #92185 ),
 ( #67925, #1571, #100284 ),
 ( #100810, #99211, #41520 ),
 ( #34534, #26446, #484 ) ),
 .UNSPECIFIED., .F., .F., .F. ) 
 B_SPLINE_SURFACE_WITH_KNOTS ( ( 4, 2, 2, 2, 2, 4 ),
 ( 3, 3 ),
 ( 1.840107927142398125E-15, 0.002111337082682424732, 0.003167005624022716827, 0.004222674165363008922, 0.006334011248043593112, 0.008445348330724177302 ),
 ( 0.000000000000000000, 1.000000000000000000 ),
 .UNSPECIFIED. ) 
 GEOMETRIC_REPRESENTATION_ITEM ( )  RATIONAL_B_SPLINE_SURFACE ( (
 ( 1.000000000000000000, 0.8812198548864098591, 1.000000000000000000),
 ( 1.000000000000000000, 0.8727984268039941096, 1.000000000000000000),
 ( 1.000000000000000000, 0.8622592014671073279, 1.000000000000000000),
 ( 1.000000000000000000, 0.8442704230973751001, 1.000000000000000000),
 ( 1.000000000000000000, 0.8379082757199421971, 1.000000000000000000),
 ( 1.000000000000000000, 0.8246032719432775382, 1.000000000000000000),
 ( 1.000000000000000000, 0.8177416415213525358, 1.000000000000000000),
 ( 1.000000000000000000, 0.7969800896719004824, 1.000000000000000000),
 ( 1.000000000000000000, 0.7828175013986581332, 1.000000000000000000),
 ( 1.000000000000000000, 0.7557468352507644704, 1.000000000000000000),
 ( 1.000000000000000000, 0.7431293883733521843, 1.000000000000000000),
 ( 1.000000000000000000, 0.7328671738315113426, 1.000000000000000000) ) ) 
 REPRESENTATION_ITEM ( '' )  SURFACE ( )  );
#34166 = EDGE_LOOP ( 'NONE', ( #102157, #11344, #67634, #151, #86407 ) ) ;
#34168 = B_SPLINE_CURVE_WITH_KNOTS ( 'NONE', 3,
 ( #39266, #87810, #96952, #78626, #37698, #79168, #104504, #22023 ),
 .UNSPECIFIED., .F., .F.,
 ( 4, 2, 2, 4 ),
 ( 0.01336725832182608306, 0.01453745201803765055, 0.01570764571424921457, 0.01804803310667234956 ),
 .UNSPECIFIED. ) ;
#34167 = CIRCLE ( 'NONE', #94450, 4.981862520314373377 ) ;
#34169 = FILL_AREA_STYLE_COLOUR ( '', #68687 ) ;
#34170 = CARTESIAN_POINT ( 'NONE',  ( 110.1281201688277918, -57.67139407212744118, 129.8419390022934294 ) ) ;
#34171 = VERTEX_POINT ( 'NONE', #66768 ) ;
#34172 = CIRCLE ( 'NONE', #99574, 4.000000000000000888 ) ;
#34173 = CARTESIAN_POINT ( 'NONE',  ( 33.92709525147887462, 435.0559456452658651, 11.89085117398059843 ) ) ;
#34174 = B_SPLINE_CURVE_WITH_KNOTS ( 'NONE', 3,
 ( #47523, #97656, #70751, #14612, #103646 ),
 .UNSPECIFIED., .F., .F.,
 ( 4, 1, 4 ),
 ( 0.000000000000000000, 0.003752776749732572234, 0.007505553499465144468 ),
 .UNSPECIFIED. ) ;
#34175 = CARTESIAN_POINT ( 'NONE',  ( -8.559508646656389885, 51.55638410492942825, -4.031152949374503081 ) ) ;
#34176 = DIRECTION ( 'NONE',  ( -0.000000000000000000, -1.000000000000000000, -0.000000000000000000 ) ) ;
#34177 = CARTESIAN_POINT ( 'NONE',  ( 19.18290667320985676, 302.7118746156783686, 9.907256564758082362 ) ) ;
#34178 = CARTESIAN_POINT ( 'NONE',  ( -79.65127760519116862, -60.00000000000001421, 195.5387530500997855 ) ) ;
#34179 = FACE_OUTER_BOUND ( 'NONE', #70504, .T. ) ;
#34181 = PRESENTATION_LAYER_ASSIGNMENT (  '', '', ( #41002 ) ) ;
#34180 = CARTESIAN_POINT ( 'NONE',  ( 0.000000000000000000, 0.000000000000000000, 0.000000000000000000 ) ) ;
#34182 = CARTESIAN_POINT ( 'NONE',  ( -45.29905483467455696, 497.0732240353902398, -8.041250874568902418 ) ) ;
#34183 = PRESENTATION_LAYER_ASSIGNMENT (  '', '', ( #103078 ) ) ;
#34184 = CARTESIAN_POINT ( 'NONE',  ( -86.22339662976257557, -21.27558923800543056, 177.9722882754944067 ) ) ;
#34185 = ORIENTED_EDGE ( 'NONE', *, *, #10240, .F. ) ;
#34186 = VERTEX_POINT ( 'NONE', #41418 ) ;
#34187 = CARTESIAN_POINT ( 'NONE',  ( 16.01235146068399473, 3.721755040408527115, 0.3223148954820237444 ) ) ;
#34188 = EDGE_CURVE ( 'NONE', #75560, #99927, #3564, .T. ) ;
#34189 =( NAMED_UNIT ( * ) SI_UNIT ( $, .STERADIAN. ) SOLID_ANGLE_UNIT ( ) );
#34190 = CARTESIAN_POINT ( 'NONE',  ( -87.01690208926603987, -60.20973691192937594, -8.193354508930786650 ) ) ;
#34191 = FACE_OUTER_BOUND ( 'NONE', #31451, .T. ) ;
#34192 = CARTESIAN_POINT ( 'NONE',  ( -5.126029744276100253, 6.171265713471635550, -4.999999999999998224 ) ) ;
#34193 = CIRCLE ( 'NONE', #47920, 4.000000000000001776 ) ;
#34195 = CYLINDRICAL_SURFACE ( 'NONE', #1112, 5.000000000000000888 ) ;
#34194 = VECTOR ( 'NONE', #58581, 1000.000000000000000 ) ;
#34196 = CARTESIAN_POINT ( 'NONE',  ( -47.37019975550713724, 41.99999999999999289, 36.40416150952766827 ) ) ;
#34197 = EDGE_CURVE ( 'NONE', #16689, #90625, #94741, .T. ) ;
#34198 = AXIS2_PLACEMENT_3D ( 'NONE', #58781, #17792, #100807 ) ;
#34199 = EDGE_CURVE ( 'NONE', #23846, #19012, #36165, .T. ) ;
#34200 = DIRECTION ( 'NONE',  ( -1.000000000000000000, -1.224606353822377258E-16, -0.000000000000000000 ) ) ;
#34201 = CARTESIAN_POINT ( 'NONE',  ( 35.94918560889485093, -14.21045842199434439, 40.02951443902858841 ) ) ;
#34202 = CARTESIAN_POINT ( 'NONE',  ( -35.93056730070349403, 437.9188583894979274, 4.302256410573773948 ) ) ;
#34203 = CARTESIAN_POINT ( 'NONE',  ( -57.68513734192992359, -30.00000000000002487, -33.51766283710919225 ) ) ;
#34204 = CARTESIAN_POINT ( 'NONE',  ( -67.76884453457680024, -32.53527454055805634, 90.78174967798416617 ) ) ;
#34205 = ORIENTED_EDGE ( 'NONE', *, *, #105765, .F. ) ;
#34206 = CARTESIAN_POINT ( 'NONE',  ( 70.85242353449750397, -59.99999999999999289, 164.3672743468505359 ) ) ;
#34207 = CARTESIAN_POINT ( 'NONE',  ( 7.744168461338432508, 88.46254061715157491, 2.019395720771550273 ) ) ;
#34208 = CARTESIAN_POINT ( 'NONE',  ( 94.10310489044364601, -57.65276993155347895, -13.84278669819006247 ) ) ;
#34209 = CIRCLE ( 'NONE', #29078, 5.000000000000002665 ) ;
#34210 = VERTEX_POINT ( 'NONE', #73778 ) ;
#34211 = CARTESIAN_POINT ( 'NONE',  ( 14.88296266491841635, 41.91403693906578098, -82.91974649391508478 ) ) ;
#34212 = CARTESIAN_POINT ( 'NONE',  ( 41.50669491856072568, 3.851859888774471706E-31, 5.000000000000001776 ) ) ;
#34213 = ORIENTED_EDGE ( 'NONE', *, *, #34620, .F. ) ;
#34214 = CARTESIAN_POINT ( 'NONE',  ( 3.011045263346121992, 15.20713166912945624, -6.322393913128321330 ) ) ;
#34215 = DIRECTION ( 'NONE',  ( 0.7071067811865456854, 8.659560562354955045E-17, 0.7071067811865493491 ) ) ;
#34216 = LINE ( 'NONE', #58997, #65657 ) ;
#34217 = CARTESIAN_POINT ( 'NONE',  ( -5.082755093536326818, -13.71875000204838457, 5.082755093536325042 ) ) ;
#34218 = DIRECTION ( 'NONE',  ( -0.5000000000000006661, -0.8660254037844383745, 0.000000000000000000 ) ) ;
#34219 = CARTESIAN_POINT ( 'NONE',  ( 36.08349330513379982, 1.593028355512270962E-15, 0.000000000000000000 ) ) ;
#34220 = CARTESIAN_POINT ( 'NONE',  ( -12.48209226849267317, -3.606693023214783356, -13.63090450099858053 ) ) ;
#34221 = B_SPLINE_CURVE_WITH_KNOTS ( 'NONE', 3,
 ( #25815, #45673, #62393, #20389, #36554, #79089, #46203, #53751 ),
 .UNSPECIFIED., .F., .F.,
 ( 4, 2, 2, 4 ),
 ( 2.602085213965210642E-18, 0.002636210293396384820, 0.003954315440094607371, 0.005272420586792830356 ),
 .UNSPECIFIED. ) ;
#34222 = ADVANCED_FACE ( 'NONE', ( #26879 ), #102857, .T. ) ;
#34223 = ORIENTED_EDGE ( 'NONE', *, *, #86522, .T. ) ;
#34224 = CARTESIAN_POINT ( 'NONE',  ( -7.013017686808002971, 40.92324844527869487, -70.84400559904489114 ) ) ;
#34226 = CARTESIAN_POINT ( 'NONE',  ( 32.30811475795603371, -46.43045952615185712, 35.30348012445732309 ) ) ;
#34225 = PRESENTATION_STYLE_ASSIGNMENT (( #99437 ) ) ;
#34227 = CARTESIAN_POINT ( 'NONE',  ( -33.00540147334746166, 487.4196752801198613, 9.523982417603901851 ) ) ;
#34228 = ORIENTED_EDGE ( 'NONE', *, *, #52137, .T. ) ;
#34229 = EDGE_CURVE ( 'NONE', #54320, #58994, #70614, .T. ) ;
#34230 = CIRCLE ( 'NONE', #106552, 8.000000000000014211 ) ;
#34231 = VECTOR ( 'NONE', #69376, 1000.000000000000000 ) ;
#34232 = ORIENTED_EDGE ( 'NONE', *, *, #87196, .T. ) ;
#34234 = CARTESIAN_POINT ( 'NONE',  ( -2.583674962488347493, -5.000000000000000000, 9.743244787954280284 ) ) ;
#34233 = CARTESIAN_POINT ( 'NONE',  ( 0.5805565836007664515, -7.505553499465142053, -1.357586595304856736E-16 ) ) ;
#34235 = CARTESIAN_POINT ( 'NONE',  ( 22.61650669486618526, 1.474610560812782335E-15, 0.000000000000000000 ) ) ;
#34236 = DIRECTION ( 'NONE',  ( 0.8191520442889911324, 0.000000000000000000, 0.5735764363510470476 ) ) ;
#34237 = APPLICATION_CONTEXT ( 'automotive_design' ) ;
#34238 = DIRECTION ( 'NONE',  ( 0.000000000000000000, 0.000000000000000000, 1.000000000000000000 ) ) ;
#34239 = CARTESIAN_POINT ( 'NONE',  ( 32.12756478244934044, 464.8250811501558246, 14.60600970018909095 ) ) ;
#34240 = CARTESIAN_POINT ( 'NONE',  ( -36.94903695760827134, 463.9900885034068665, 19.60515700096717495 ) ) ;
#34242 = ORIENTED_EDGE ( 'NONE', *, *, #13948, .F. ) ;
#34241 = STYLED_ITEM ( 'NONE', ( #39757 ), #31515 ) ;
#34243 = CARTESIAN_POINT ( 'NONE',  ( 92.73630845656811061, -59.99999999999999289, -6.105622175954798614 ) ) ;
#34244 = CARTESIAN_POINT ( 'NONE',  ( 32.19135603494942188, 464.6890496749892350, 10.76801839735704469 ) ) ;
#34245 =( NAMED_UNIT ( * ) SI_UNIT ( $, .STERADIAN. ) SOLID_ANGLE_UNIT ( ) );
#34246 = CARTESIAN_POINT ( 'NONE',  ( 3.269135563215229023, 294.8518027752268722, -10.00000000024436453 ) ) ;
#34247 = CARTESIAN_POINT ( 'NONE',  ( -47.36618468514944880, 18.16301677597580877, -14.54218830158967179 ) ) ;
#34248 = ORIENTED_EDGE ( 'NONE', *, *, #18437, .F. ) ;
#34249 = CARTESIAN_POINT ( 'NONE',  ( 17.61650669486618881, 1.474610560812782335E-15, 0.000000000000000000 ) ) ;
#34250 = EDGE_LOOP ( 'NONE', ( #68754, #101711, #17769, #7602, #11173, #2081 ) ) ;
#34251 = ORIENTED_EDGE ( 'NONE', *, *, #73202, .F. ) ;
#34252 = CARTESIAN_POINT ( 'NONE',  ( 7.934914944860278041, 81.13154352799891456, -1.051261972695689551 ) ) ;
#34253 = CYLINDRICAL_SURFACE ( 'NONE', #64895, 4.000000000000000888 ) ;
#34254 = CARTESIAN_POINT ( 'NONE',  ( -15.73379620320076633, 35.06307335795982283, -22.31246066629909208 ) ) ;
#34255 = DIRECTION ( 'NONE',  ( 0.000000000000000000, -1.000000000000000000, 0.000000000000000000 ) ) ;
#34256 = CARTESIAN_POINT ( 'NONE',  ( 87.00105230417793223, -60.21000100938282884, -8.688507030231054529 ) ) ;
#34257 = CARTESIAN_POINT ( 'NONE',  ( -30.88942347583406089, 309.2109866158478440, -8.534727214836138387 ) ) ;
#34258 = CARTESIAN_POINT ( 'NONE',  ( -20.37278541768179707, 303.8378246129572062, -10.00297115033344042 ) ) ;
#34259 = VERTEX_POINT ( 'NONE', #77521 ) ;
#34260 = CARTESIAN_POINT ( 'NONE',  ( -6.826580258811424606, 2.695816818219042954, -6.331007506862903256 ) ) ;
#34261 = ORIENTED_EDGE ( 'NONE', *, *, #18993, .T. ) ;
#34262 = DIRECTION ( 'NONE',  ( 0.000000000000000000, 0.000000000000000000, 1.000000000000000000 ) ) ;
#34264 = ORIENTED_EDGE ( 'NONE', *, *, #34407, .F. ) ;
#34263 = DIRECTION ( 'NONE',  ( 0.000000000000000000, 0.6543614439331889576, -0.7561819230143446147 ) ) ;
#34265 = CARTESIAN_POINT ( 'NONE',  ( 76.54894832708983188, -22.13291403085647602, 114.5410150515899943 ) ) ;
#34266 = STYLED_ITEM ( 'NONE', ( #44357 ), #68817 ) ;
#34267 = ORIENTED_EDGE ( 'NONE', *, *, #58597, .F. ) ;
#34268 = CARTESIAN_POINT ( 'NONE',  ( 51.48757442383973881, 38.95383793068620548, -37.45149417477089315 ) ) ;
#34269 = CARTESIAN_POINT ( 'NONE',  ( -2.977408999572650039, -23.18750000204838813, -7.188101187500000933 ) ) ;
#34270 = CARTESIAN_POINT ( 'NONE',  ( -111.7589076751911392, -57.67119524614439285, 141.4413276519820784 ) ) ;
#34271 = ADVANCED_FACE ( 'NONE', ( #101269 ), #68870, .F. ) ;
#34272 = ORIENTED_EDGE ( 'NONE', *, *, #98633, .F. ) ;
#34273 = EDGE_CURVE ( 'NONE', #87999, #64539, #36569, .T. ) ;
#34274 = LINE ( 'NONE', #66076, #55742 ) ;
#34275 = CARTESIAN_POINT ( 'NONE',  ( 103.7274724878040928, -45.28268791833052376, 163.4000004519256208 ) ) ;
#34276 = AXIS2_PLACEMENT_3D ( 'NONE', #100685, #66737, #3063 ) ;
#34277 = EDGE_CURVE ( 'NONE', #44667, #62970, #69438, .T. ) ;
#34278 = PLANE ( 'NONE',  #101232 ) ;
#34279 = ADVANCED_FACE ( 'NONE', ( #52166 ), #97064, .F. ) ;
#34280 = B_SPLINE_CURVE_WITH_KNOTS ( 'NONE', 3,
 ( #28992, #95803, #36541, #62383, #20904, #102290, #53739, #86668, #95277, #28436, #87185, #20376, #46186, #79078, #70984, #103873, #30021, #21933, #54783, #8363, #81181, #65547, #15395, #97367, #32677, #32135, #41264, #88761, #39166, #89301, #33200, #40200, #14858, #98435 ),
 .UNSPECIFIED., .F., .F.,
 ( 4, 2, 2, 2, 2, 2, 2, 2, 2, 2, 2, 2, 2, 2, 2, 2, 4 ),
 ( 0.01279395524623341482, 0.01359199989167121127, 0.01439004453710900772, 0.01518808918254680243, 0.01598613382798460061, 0.01678417847342239533, 0.01758222311886019351, 0.01838026776429798823, 0.01917831240973578294, 0.01997635705517358112, 0.02077440170061137931, 0.02157244634604917402, 0.02237049099148696873, 0.02316853563692476692, 0.02396658028236256510, 0.02476462492780035982, 0.02556266957323815453 ),
 .UNSPECIFIED. ) ;
#34281 = CARTESIAN_POINT ( 'NONE',  ( 9.500000000000000000, -5.000000000000000000, -20.99851272547260095 ) ) ;
#34282 = CARTESIAN_POINT ( 'NONE',  ( -1.469576158976823947E-15, -22.06250000409676915, 8.000000000000000000 ) ) ;
#34283 = DIRECTION ( 'NONE',  ( -1.000000000000000000, -0.000000000000000000, -0.000000000000000000 ) ) ;
#34284 = CARTESIAN_POINT ( 'NONE',  ( 0.000000000000000000, 0.000000000000000000, -3.852324522925831385 ) ) ;
#34285 = ADVANCED_FACE ( 'NONE', ( #78563, #4696, #37629, #100716, #93170 ), #62012, .T. ) ;
#34286 = DIRECTION ( 'NONE',  ( -1.000000000000000000, -1.224606353822377258E-16, -0.000000000000000000 ) ) ;
#34287 = DIRECTION ( 'NONE',  ( -1.000000000000000000, 0.000000000000000000, 0.000000000000000000 ) ) ;
#34288 = CARTESIAN_POINT ( 'NONE',  ( 6.123233995736765296E-16, 0.000000000000000000, 4.999999999999999112 ) ) ;
#34289 = DIRECTION ( 'NONE',  ( 4.233437538138742344E-17, 0.1845977156002912289, 0.9828141652393672656 ) ) ;
#34290 =( NAMED_UNIT ( * ) PLANE_ANGLE_UNIT ( ) SI_UNIT ( $, .RADIAN. ) );
#34291 = ORIENTED_EDGE ( 'NONE', *, *, #37140, .F. ) ;
#34292 = CARTESIAN_POINT ( 'NONE',  ( -9.500000000000003553, -5.000000000000000000, -68.91429205785459544 ) ) ;
#34293 = ADVANCED_FACE ( 'NONE', ( #44091 ), #67152, .T. ) ;
#34294 = LINE ( 'NONE', #59077, #81866 ) ;
#34295 = CARTESIAN_POINT ( 'NONE',  ( -5.000000000000000000, -23.50454593378518453, -3.099858002006805613 ) ) ;
#34296 = CARTESIAN_POINT ( 'NONE',  ( -89.78872880365601361, -30.00000000000000711, 189.6862794871168774 ) ) ;
#34297 = VECTOR ( 'NONE', #103407, 1000.000000000000000 ) ;
#34298 = ORIENTED_EDGE ( 'NONE', *, *, #90958, .F. ) ;
#34299 =( GEOMETRIC_REPRESENTATION_CONTEXT ( 3 ) GLOBAL_UNCERTAINTY_ASSIGNED_CONTEXT ( ( #44834 ) ) GLOBAL_UNIT_ASSIGNED_CONTEXT ( ( #25951, #27000, #17820 ) ) REPRESENTATION_CONTEXT ( 'NONE', 'WORKASPACE' ) );
#34300 = CARTESIAN_POINT ( 'NONE',  ( 2.464820640578141209, -49.72436178699376086, 44.56749791512065428 ) ) ;
#34301 = CARTESIAN_POINT ( 'NONE',  ( 72.83774066108748002, -57.65622831221423183, 179.9088005362346792 ) ) ;
#34303 = CARTESIAN_POINT ( 'NONE',  ( -8.719010170337146093, 53.63221892593892193, 4.031152949374982697 ) ) ;
#34302 = CARTESIAN_POINT ( 'NONE',  ( -15.37029426978759084, 3.165964433752528784, -3.249157221772423831 ) ) ;
#34304 = AXIS2_PLACEMENT_3D ( 'NONE', #101477, #27628, #35171 ) ;
#34305 = AXIS2_PLACEMENT_3D ( 'NONE', #68778, #60686, #13153 ) ;
#34306 = CARTESIAN_POINT ( 'NONE',  ( 24.88129734378813751, -27.66378606029807585, -38.37538378080514434 ) ) ;
#34307 = CARTESIAN_POINT ( 'NONE',  ( -0.3381768955574565028, 44.07166901386596436, 16.28514545986189077 ) ) ;
#34308 = CARTESIAN_POINT ( 'NONE',  ( -39.41275501335248777, 489.7121233615637834, 11.67778311875232333 ) ) ;
#34309 = CARTESIAN_POINT ( 'NONE',  ( -45.08300348252168277, -60.00000000000001421, 60.74044995775830103 ) ) ;
#34310 = CYLINDRICAL_SURFACE ( 'NONE', #74415, 1.250000000000001110 ) ;
#34311 =( GEOMETRIC_REPRESENTATION_CONTEXT ( 3 ) GLOBAL_UNCERTAINTY_ASSIGNED_CONTEXT ( ( #18161 ) ) GLOBAL_UNIT_ASSIGNED_CONTEXT ( ( #48351, #8432, #98497 ) ) REPRESENTATION_CONTEXT ( 'NONE', 'WORKASPACE' ) );
#34312 = CARTESIAN_POINT ( 'NONE',  ( 6.068667535695539073, 53.39711552543036532, 8.262660017157307024 ) ) ;
#34313 = CARTESIAN_POINT ( 'NONE',  ( -85.89194148627102265, -42.88414227571757209, 188.0209850057943015 ) ) ;
#34314 = ORIENTED_EDGE ( 'NONE', *, *, #37396, .T. ) ;
#34315 = CARTESIAN_POINT ( 'NONE',  ( 30.22667580650593422, 12.95764659710603262, 41.98307762325157455 ) ) ;
#34316 = CARTESIAN_POINT ( 'NONE',  ( -7.155724036906063290, -42.95763110478070246, 31.03959182391562521 ) ) ;
#34317 = DIRECTION ( 'NONE',  ( 0.000000000000000000, 1.000000000000000000, -0.000000000000000000 ) ) ;
#34318 = CARTESIAN_POINT ( 'NONE',  ( -6.499999999999999112, -3.752776749732587902, -6.064240316920403551 ) ) ;
#34319 = B_SPLINE_SURFACE_WITH_KNOTS ( 'NONE', 1, 3, ( 
 ( #35627, #19986, #34564, #77649, #67957, #44219, #3226, #60941, #101392, #43676, #75507, #36168, #27543, #36696, #85757, #69037, #93301, #76564, #93831, #52830, #59885, #28594, #43155, #61478, #60423, #94371, #50676, #83591 ),
 ( #10242, #67439, #100312, #59346, #18366, #2134, #35087, #100841, #27004, #92758, #18917, #51761, #84675, #2675, #54938, #88396, #86816, #46860, #78166, #79229, #5356, #53883, #13416, #64137, #78685, #96488, #70082, #63601 ) ),
 .UNSPECIFIED., .F., .F., .F.,
 ( 2, 2 ),
 ( 4, 2, 2, 2, 2, 2, 2, 2, 2, 2, 2, 2, 2, 4 ),
 ( 0.000000000000000000, 1.000000000000000000 ),
 ( 0.08901491201581737678, 0.1032490540155679704, 0.1174831960153185778, 0.1317173380150691853, 0.1459514800148197788, 0.1744197640143299588, 0.2028880480138401388, 0.2598246160128514504, 0.3167611840118632616, 0.4306343200098861623, 0.5445074560079088410, 0.6583805920059359051, 0.7722537280039543095, 1.000000000000000000 ),
 .UNSPECIFIED. ) ;
#34321 = CARTESIAN_POINT ( 'NONE',  ( 4.394945503249887864, -66.37976763068485297, 13.13806607437854446 ) ) ;
#34320 = CARTESIAN_POINT ( 'NONE',  ( -34.40498866140573853, 302.2778906776350709, 3.632078850025649341 ) ) ;
#34322 = ORIENTED_EDGE ( 'NONE', *, *, #81419, .F. ) ;
#34323 = ADVANCED_FACE ( 'NONE', ( #46735 ), #60316, .T. ) ;
#34324 = DIRECTION ( 'NONE',  ( 0.000000000000000000, -1.000000000000000000, 0.000000000000000000 ) ) ;
#34325 = VECTOR ( 'NONE', #92864, 1000.000000000000000 ) ;
#34326 = CARTESIAN_POINT ( 'NONE',  ( 0.4150691409093130169, 27.32056545513875534, 40.68202461718954055 ) ) ;
#34327 = CARTESIAN_POINT ( 'NONE',  ( -30.48935137155294228, 7.748232456195979445, -41.81352479775729591 ) ) ;
#34328 = CARTESIAN_POINT ( 'NONE',  ( 29.93558873341680027, 297.4490136268220795, -9.432928331562733248 ) ) ;
#34329 = CARTESIAN_POINT ( 'NONE',  ( 26.27902093981875709, 306.9027577142574614, -9.548073367145329726 ) ) ;
#34330 = CLOSED_SHELL ( 'NONE', ( #2839, #9074, #20124, #32808, #65014, #46538, #94210, #92228, #36977, #74535, #42217, #7243, #22479, #78075, #96383, #105486, #8624, #54681, #37267, #10612, #83747, #11618, #100517, #60180, #49635, #105264, #22744, #58655, #101535, #75146, #76635, #15584, #104263, #105736, #39830, #71923, #105296, #21684, #94022, #29087, #25773, #51756, #39482, #47171, #99679, #30166, #69992, #75024, #83313, #9458, #65743, #104834, #38253, #102196, #84160, #104122, #6463, #40032, #13170, #95413, #35226, #47630, #6081, #37457, #87605, #34279, #94518, #30781, #38564, #99646, #55361, #6558, #79239, #95825, #24340, #20246, #9483, #24477, #1917, #29714, #72273, #31211, #36513, #99496, #96501, #33746, #51420, #58167, #28583, #78550, #101798, #76174, #62987, #3520, #26768, #38641, #13157, #48801, #52408, #70682, #83657, #60244, #92245, #42684, #40209, #66950, #98434, #93154, #2712, #80319, #70334, #82689, #3742, #58476, #62519, #61216, #24083, #104065, #76848, #33798, #88957, #91028, #63899, #21188, #20436, #94148, #40168, #20115, #71620, #74001, #103142, #106673, #1129, #34634, #7411, #993, #58360, #49779, #38898, #13427, #54955, #34371, #30244, #463, #2878, #28487, #49388, #24079, #20080, #72685, #102510, #15848, #56138, #9201, #83719, #9876, #36590, #15807, #75778, #98582, #20687, #67051, #30951, #5331, #59696, #102047, #21447, #63584, #72589, #52293, #46108, #75644, #72019, #11265, #95645, #101609, #23057, #58609, #94832, #52638, #12894, #63375, #33585, #9512, #87855, #33077, #41334, #96246, #45338, #92329, #103474, #55001, #6935, #64303, #101351, #83151, #78309, #14547, #62693, #42146, #18855, #25012, #30261, #19676, #98839, #71426, #51330, #29275, #88584, #38594, #8658, #104337, #96537, #70804, #69728, #44462, #85344, #21481, #77055, #45772, #71128, #26919, #7319, #99206, #105986, #67570, #2995, #48385, #72309, #49885, #83605, #62180, #32726, #81705, #87051, #39233, #11133, #41254, #46837, #45229, #61133, #23822, #93555 ) ) ;
#34331 = EDGE_CURVE ( 'NONE', #58519, #36397, #70493, .T. ) ;
#34332 = EDGE_CURVE ( 'NONE', #57426, #3882, #72302, .T. ) ;
#34333 = CARTESIAN_POINT ( 'NONE',  ( 32.10528697966009304, 486.1671898930079578, 5.449875171705039989 ) ) ;
#34334 = CARTESIAN_POINT ( 'NONE',  ( 108.4360931436784767, -30.00000000000001066, 186.7338794867829677 ) ) ;
#34335 = CARTESIAN_POINT ( 'NONE',  ( -79.83446298086737158, -46.43891928859385843, 152.6746585543230026 ) ) ;
#34336 = EDGE_LOOP ( 'NONE', ( #25968, #68650, #8465, #88952 ) ) ;
#34337 = CARTESIAN_POINT ( 'NONE',  ( 0.000000000000000000, -30.00000000000000000, 0.000000000000000000 ) ) ;
#34338 = CARTESIAN_POINT ( 'NONE',  ( 0.01688885742776283228, -6.535341423375585101, 4.680456609903972165 ) ) ;
#34339 = CARTESIAN_POINT ( 'NONE',  ( 0.000000000000000000, 4.898587196589412829E-16, -4.000000000000000000 ) ) ;
#34340 = DIRECTION ( 'NONE',  ( 0.000000000000000000, 0.8802307401770171902, 0.4745459346021421165 ) ) ;
#34341 =( BOUNDED_CURVE ( )  B_SPLINE_CURVE ( 2, ( #51000, #297, #25737, #57495, #81765, #17607, #8429, #42935, #41328 ),
 .UNSPECIFIED., .F., .F. ) 
 B_SPLINE_CURVE_WITH_KNOTS ( ( 3, 2, 2, 2, 3 ),
 ( 0.4852941176470589868, 0.4926470588235296044, 0.5000000000000002220, 0.5073529411764707842, 0.5147058823529413463 ),
 .UNSPECIFIED. ) 
 CURVE ( )  GEOMETRIC_REPRESENTATION_ITEM ( )  RATIONAL_B_SPLINE_CURVE ( ( 0.9999999999999982236, 0.9238795325112885148, 1.000000000000000000, 0.9238795325112867385, 1.000000000000000000, 0.9238795325112867385, 1.000000000000000000, 0.9238795325112844070, 1.000000000000002220 ) ) 
 REPRESENTATION_ITEM ( '' )  );
#34342 = CARTESIAN_POINT ( 'NONE',  ( 45.44493243946729422, 426.7325925718847657, 7.514341639838392872 ) ) ;
#34343 = AXIS2_PLACEMENT_3D ( 'NONE', #1197, #84812, #36311 ) ;
#34344 = CARTESIAN_POINT ( 'NONE',  ( 7.500000000000007105, -3.000000000000000000, -68.91429205785459544 ) ) ;
#34345 = ORIENTED_EDGE ( 'NONE', *, *, #89956, .F. ) ;
#34346 = UNCERTAINTY_MEASURE_WITH_UNIT (LENGTH_MEASURE( 1.000000000000000082E-05 ), #91963, 'distance_accuracy_value', 'NONE');
#34347 = CARTESIAN_POINT ( 'NONE',  ( -21.40103372500290035, 305.0975791469744536, 9.989648404215305533 ) ) ;
#34348 = VERTEX_POINT ( 'NONE', #29534 ) ;
#34349 = CARTESIAN_POINT ( 'NONE',  ( 33.51155624906014197, 484.9914999643505666, -0.2834665992334333695 ) ) ;
#34350 = CARTESIAN_POINT ( 'NONE',  ( -1.400881274228119588, 15.45483377860037955, 9.907626560209529032 ) ) ;
#34351 = CARTESIAN_POINT ( 'NONE',  ( 32.67430661331284369, 485.6291057174275352, 6.589190333399087329 ) ) ;
#34352 = CARTESIAN_POINT ( 'NONE',  ( -28.00203968317432057, 50.00000000000000000, 56.72941417029706201 ) ) ;
#34353 = CARTESIAN_POINT ( 'NONE',  ( 5.000000000000000000, -14.30429124282204079, 12.05126107871916297 ) ) ;
#34354 = DIRECTION ( 'NONE',  ( 0.000000000000000000, 0.000000000000000000, 1.000000000000000000 ) ) ;
#34355 = ORIENTED_EDGE ( 'NONE', *, *, #47887, .T. ) ;
#34356 = CARTESIAN_POINT ( 'NONE',  ( 102.7236711658890158, -59.99999999999997868, 200.7889012320235622 ) ) ;
#34358 = CARTESIAN_POINT ( 'NONE',  ( 21.59831149744555390, -49.91455128373721095, 32.92735310832569695 ) ) ;
#34357 = CARTESIAN_POINT ( 'NONE',  ( -94.36268555338997999, -29.99999999999996803, 200.0833938634536935 ) ) ;
#34359 = STYLED_ITEM ( 'NONE', ( #105472 ), #90230 ) ;
#34360 = CARTESIAN_POINT ( 'NONE',  ( 34.40458878342295890, 463.9182705154310611, 5.552276315902680892 ) ) ;
#34361 = CARTESIAN_POINT ( 'NONE',  ( 17.50000000000002842, 50.00000000000000000, 63.82142195508322402 ) ) ;
#34362 = ADVANCED_FACE ( 'NONE', ( #104430 ), #103402, .T. ) ;
#34363 = CARTESIAN_POINT ( 'NONE',  ( -39.81795437584664654, -53.34937766137575466, 41.56781054599359493 ) ) ;
#34364 = CARTESIAN_POINT ( 'NONE',  ( -8.559508646656370345, 53.68473964988125857, -4.031152949374577688 ) ) ;
#34365 = UNCERTAINTY_MEASURE_WITH_UNIT (LENGTH_MEASURE( 1.000000000000000082E-05 ), #86523, 'distance_accuracy_value', 'NONE');
#34366 = ORIENTED_EDGE ( 'NONE', *, *, #33878, .T. ) ;
#34367 = FACE_BOUND ( 'NONE', #68351, .T. ) ;
#34368 = CARTESIAN_POINT ( 'NONE',  ( 5.960000261375881792, -13.79916237020871073, 13.82526581198426108 ) ) ;
#34369 = VECTOR ( 'NONE', #82217, 1000.000000000000000 ) ;
#34370 =( NAMED_UNIT ( * ) SI_UNIT ( $, .STERADIAN. ) SOLID_ANGLE_UNIT ( ) );
#34371 = ADVANCED_FACE ( 'NONE', ( #105499 ), #105320, .F. ) ;
#34372 = CARTESIAN_POINT ( 'NONE',  ( 18.61218452878530982, 304.6205044140078257, -10.04916398453198134 ) ) ;
#34373 = CARTESIAN_POINT ( 'NONE',  ( -30.00000000000000355, 488.9470845376447414, 4.704489282118356819 ) ) ;
#34374 = ORIENTED_EDGE ( 'NONE', *, *, #45544, .T. ) ;
#34375 = DIRECTION ( 'NONE',  ( -1.000000000000000000, -0.000000000000000000, -0.000000000000000000 ) ) ;
#34376 = ORIENTED_EDGE ( 'NONE', *, *, #29187, .F. ) ;
#34377 = CARTESIAN_POINT ( 'NONE',  ( 81.05248856670681334, -30.00000000000004619, -11.71509379367667414 ) ) ;
#34378 = CARTESIAN_POINT ( 'NONE',  ( 16.20053603399965070, 41.96864385763039706, -84.86819136098323213 ) ) ;
#34379 = CARTESIAN_POINT ( 'NONE',  ( 24.43701635837512498, 25.27496214381292106, -32.24253520507857473 ) ) ;
#34380 = DIRECTION ( 'NONE',  ( -1.000000000000000000, 0.000000000000000000, 0.000000000000000000 ) ) ;
#34381 = CARTESIAN_POINT ( 'NONE',  ( 83.01728599698354572, -30.00000000000000000, 43.06514241403382215 ) ) ;
#34382 = VERTEX_POINT ( 'NONE', #5742 ) ;
#34383 = VECTOR ( 'NONE', #43463, 1000.000000000000000 ) ;
#34384 = ORIENTED_EDGE ( 'NONE', *, *, #99147, .T. ) ;
#34385 = ORIENTED_EDGE ( 'NONE', *, *, #104139, .T. ) ;
#34386 = CARTESIAN_POINT ( 'NONE',  ( -47.14858110737391428, 13.36679009520639205, -14.71571165017404326 ) ) ;
#34387 = DIRECTION ( 'NONE',  ( -1.000000000000000000, -0.000000000000000000, -0.000000000000000000 ) ) ;
#34388 = DIRECTION ( 'NONE',  ( -0.000000000000000000, -0.000000000000000000, 1.000000000000000000 ) ) ;
#34389 = CARTESIAN_POINT ( 'NONE',  ( 42.77484754423761615, 436.8064166223269353, 20.35382343675431471 ) ) ;
#34390 = CARTESIAN_POINT ( 'NONE',  ( -31.93160697752860955, 357.0395867317242846, 21.73737814537944502 ) ) ;
#34391 = LINE ( 'NONE', #58640, #5346 ) ;
#34393 = VERTEX_POINT ( 'NONE', #56391 ) ;
#34392 = PRESENTATION_LAYER_ASSIGNMENT (  '', '', ( #51589 ) ) ;
#34394 = CARTESIAN_POINT ( 'NONE',  ( 1.469576158976823356E-15, 50.00000000000000000, -73.00000000000001421 ) ) ;
#34395 = VERTEX_POINT ( 'NONE', #89327 ) ;
#34396 = CARTESIAN_POINT ( 'NONE',  ( 16.08349330513380337, -4.000000000000000888, 4.898587196589416773E-16 ) ) ;
#34397 = CARTESIAN_POINT ( 'NONE',  ( 61.83185530181933132, -38.34112017042167508, 102.3246735217670675 ) ) ;
#34398 = CARTESIAN_POINT ( 'NONE',  ( 6.222742520105473574, 7.673830019007162662, 0.2914634815676387380 ) ) ;
#34399 = CARTESIAN_POINT ( 'NONE',  ( 25.74782367108087655, 305.2883975259064755, 10.48383779441362762 ) ) ;
#34400 = AXIS2_PLACEMENT_3D ( 'NONE', #44827, #77713, #102519 ) ;
#34401 = B_SPLINE_CURVE_WITH_KNOTS ( 'NONE', 3,
 ( #12846, #37176, #68042, #53847, #26569, #13372 ),
 .UNSPECIFIED., .F., .F.,
 ( 4, 2, 4 ),
 ( 2.380733003139562229E-07, 0.001898835937927374632, 0.003797433802554435033 ),
 .UNSPECIFIED. ) ;
#34402 = CARTESIAN_POINT ( 'NONE',  ( -6.000469943554647578, 245.9992950832949248, 0.2622423038614526969 ) ) ;
#34403 = ORIENTED_EDGE ( 'NONE', *, *, #9345, .T. ) ;
#34404 = CARTESIAN_POINT ( 'NONE',  ( 17.89160253087129604, 45.33672951329190681, -5.299667771043276687 ) ) ;
#34405 = DIRECTION ( 'NONE',  ( 0.000000000000000000, -0.5000000000000009992, -0.8660254037844380415 ) ) ;
#34406 = CARTESIAN_POINT ( 'NONE',  ( -7.500000000000000888, 0.000000000000000000, 0.000000000000000000 ) ) ;
#34407 = EDGE_CURVE ( 'NONE', #63428, #15295, #46215, .T. ) ;
#34408 = CARTESIAN_POINT ( 'NONE',  ( 14.98958921077330508, 2.030821136742458233, -0.4231615532927078260 ) ) ;
#34409 = VERTEX_POINT ( 'NONE', #88791 ) ;
#34410 = CONICAL_SURFACE ( 'NONE', #25804, 7.000000000000000000, 0.9599310885968753704 ) ;
#34412 = CARTESIAN_POINT ( 'NONE',  ( -24.17732587070753780, 304.0407788276623933, 10.19688566026630561 ) ) ;
#34411 =( LENGTH_UNIT ( ) NAMED_UNIT ( * ) SI_UNIT ( .MILLI., .METRE. ) );
#34413 = CARTESIAN_POINT ( 'NONE',  ( 8.559508646656350805, 53.96349637827587031, -1.531152949374623651 ) ) ;
#34414 = UNCERTAINTY_MEASURE_WITH_UNIT (LENGTH_MEASURE( 1.000000000000000082E-05 ), #38276, 'distance_accuracy_value', 'NONE');
#34415 = CARTESIAN_POINT ( 'NONE',  ( 5.799999999999999822, 8.000000000000000000, 0.000000000000000000 ) ) ;
#34416 = CARTESIAN_POINT ( 'NONE',  ( -6.658902113226989883, -5.287118297636340003, -7.776713651266857319 ) ) ;
#34417 = DIRECTION ( 'NONE',  ( -0.000000000000000000, -1.000000000000000000, -0.000000000000000000 ) ) ;
#34418 = EDGE_CURVE ( 'NONE', #70900, #74232, #36244, .T. ) ;
#34419 = EDGE_CURVE ( 'NONE', #6164, #64268, #38153, .T. ) ;
#34420 = VECTOR ( 'NONE', #35275, 1000.000000000000000 ) ;
#34421 = CARTESIAN_POINT ( 'NONE',  ( 0.000000000000000000, 0.000000000000000000, -0.02540000000000007530 ) ) ;
#34422 = CARTESIAN_POINT ( 'NONE',  ( 85.48307987227248361, -42.91479745304676641, 187.0500961933685744 ) ) ;
#34423 = CARTESIAN_POINT ( 'NONE',  ( 16.91704105317847961, 37.08060170114688958, -21.81528127871695233 ) ) ;
#34424 = CARTESIAN_POINT ( 'NONE',  ( -8.241419208061959267, 35.69988999158593401, 5.000000000002541078 ) ) ;
#34425 = ORIENTED_EDGE ( 'NONE', *, *, #24057, .F. ) ;
#34426 = CARTESIAN_POINT ( 'NONE',  ( 94.39065875124650518, -57.65262801469535248, -12.18580112889518041 ) ) ;
#34427 = B_SPLINE_CURVE_WITH_KNOTS ( 'NONE', 3,
 ( #16294, #7137, #33567, #90728, #15235, #23900, #99323, #56742, #89667, #49181, #48647, #47591, #41642, #82084, #98794, #8202 ),
 .UNSPECIFIED., .F., .F.,
 ( 4, 2, 2, 2, 2, 2, 2, 4 ),
 ( 0.006944648340236465184, 0.007952274378483222689, 0.008959900416729980194, 0.009211806926291664366, 0.009463713435853348538, 0.009967526454976709943, 0.01047133947410007135, 0.01097515249322343275 ),
 .UNSPECIFIED. ) ;
#34428 = CARTESIAN_POINT ( 'NONE',  ( 62.33904886068935980, 6.975173280561618775E-15, 0.000000000000000000 ) ) ;
#34429 = CARTESIAN_POINT ( 'NONE',  ( 14.83349330513380337, 4.000000000000002665, 0.000000000000000000 ) ) ;
#34430 = ADVANCED_FACE ( 'NONE', ( #72069 ), #50963, .T. ) ;
#34431 = DIRECTION ( 'NONE',  ( -0.000000000000000000, -1.000000000000000000, -0.000000000000000000 ) ) ;
#34432 = CARTESIAN_POINT ( 'NONE',  ( -83.18484191182862730, -30.00000000000000711, 44.38092683156298079 ) ) ;
#34433 = B_SPLINE_CURVE_WITH_KNOTS ( 'NONE', 3,
 ( #53042, #64197, #53568, #71714, #101591, #45497, #10959, #63665, #44963, #94582, #104630, #31313, #6453, #80339, #77845, #78365, #39389, #93511, #77314, #52490 ),
 .UNSPECIFIED., .F., .F.,
 ( 4, 2, 2, 2, 2, 2, 2, 2, 2, 4 ),
 ( 0.006888862763265872317, 0.007392898550706275898, 0.007896934338146680346, 0.008905005913027484038, 0.009157023806747679323, 0.009409041700467876343, 0.009913077487908265178, 0.01016509538162846220, 0.01041711327534865748, 0.01092114906278904979 ),
 .UNSPECIFIED. ) ;
#34434 = FACE_OUTER_BOUND ( 'NONE', #14387, .T. ) ;
#34435 = CARTESIAN_POINT ( 'NONE',  ( 42.08762648273149409, 487.0030674539048618, 9.106351919857861077 ) ) ;
#34436 = CARTESIAN_POINT ( 'NONE',  ( -7.848314987057847247, 4.129027267381559341, -7.493854785173809319 ) ) ;
#34437 = COLOUR_RGB ( '', 0.72549020, 0.75294118, 0.79215686) ;
#34439 = DIRECTION ( 'NONE',  ( 1.000000000000000000, 0.000000000000000000, 1.160749806054361473E-16 ) ) ;
#34438 = CARTESIAN_POINT ( 'NONE',  ( -7.894787914004607998, -1.231000152045941975E-13, -7.591390474663426424 ) ) ;
#34440 = FILL_AREA_STYLE ('',( #98061 ) ) ;
#34441 = CARTESIAN_POINT ( 'NONE',  ( 9.833493305133805151, -3.851859888774471706E-31, 4.000000000000001776 ) ) ;
#34442 = CARTESIAN_POINT ( 'NONE',  ( -3.825321387738104166E-14, -1.200000000000000030E-05, -29.75000000000000355 ) ) ;
#34443 = CARTESIAN_POINT ( 'NONE',  ( 5.384233811324310892, -81.99782908655225810, 2.655407383564611923 ) ) ;
#34444 = CARTESIAN_POINT ( 'NONE',  ( -61.22706150350772702, -37.51812599910320500, -25.43655289629557004 ) ) ;
#34445 = LINE ( 'NONE', #51096, #73501 ) ;
#34446 = VECTOR ( 'NONE', #94336, 1000.000000000000000 ) ;
#34447 = CARTESIAN_POINT ( 'NONE',  ( 39.44553997851354410, -24.70023121783347264, -30.40899877233305304 ) ) ;
#34448 = CARTESIAN_POINT ( 'NONE',  ( -23.00482107871162185, -56.87968423956402120, 34.33352247912110755 ) ) ;
#34449 = ORIENTED_EDGE ( 'NONE', *, *, #7373, .F. ) ;
#34450 = CARTESIAN_POINT ( 'NONE',  ( 6.075240630612074533, 10.96939156344817690, -3.485377474036338352 ) ) ;
#34451 = LINE ( 'NONE', #32837, #86584 ) ;
#34452 = CARTESIAN_POINT ( 'NONE',  ( -7.213352437320216914, 82.98163526992318850, -3.463014597543480733 ) ) ;
#34453 = CARTESIAN_POINT ( 'NONE',  ( -63.89019755539457179, -29.65979330600327302, -23.51777689157650642 ) ) ;
#34454 = CARTESIAN_POINT ( 'NONE',  ( -67.20361504359703986, -47.40886506081861995, -25.20267518921325589 ) ) ;
#34455 = EDGE_LOOP ( 'NONE', ( #16255, #5930, #51502, #20277, #38819 ) ) ;
#34456 = AXIS2_PLACEMENT_3D ( 'NONE', #42529, #66818, #33950 ) ;
#34457 = LINE ( 'NONE', #34981, #71979 ) ;
#34458 = VERTEX_POINT ( 'NONE', #9434 ) ;
#34459 = DIRECTION ( 'NONE',  ( 0.000000000000000000, 0.000000000000000000, 1.000000000000000000 ) ) ;
#34460 = CONICAL_SURFACE ( 'NONE', #10314, 4.250000000000000000, 0.9599310885968754814 ) ;
#34461 = EDGE_CURVE ( 'NONE', #38377, #85099, #80707, .T. ) ;
#34462 = CARTESIAN_POINT ( 'NONE',  ( 16.01731991114695575, 3.900112512635703244, 1.615757124600548433 ) ) ;
#34463 = CARTESIAN_POINT ( 'NONE',  ( -81.47805564997403849, -59.99999999999999289, -27.03802318630214430 ) ) ;
#34464 = ORIENTED_EDGE ( 'NONE', *, *, #94417, .F. ) ;
#34465 = FILL_AREA_STYLE_COLOUR ( '', #1515 ) ;
#34466 = CARTESIAN_POINT ( 'NONE',  ( -7.718587331531163720, 294.7084858445363693, -6.364235840924446386 ) ) ;
#34467 = CARTESIAN_POINT ( 'NONE',  ( 98.52377646302282699, -37.77507002369925715, 192.2321652874637152 ) ) ;
#34469 = CARTESIAN_POINT ( 'NONE',  ( -7.896254658894419798, -6.210708172458008214, 1.307282859663295493 ) ) ;
#34468 = DIRECTION ( 'NONE',  ( 0.000000000000000000, 0.000000000000000000, 1.000000000000000000 ) ) ;
#34470 = AXIS2_PLACEMENT_3D ( 'NONE', #33299, #106624, #24678 ) ;
#34471 = ORIENTED_EDGE ( 'NONE', *, *, #85918, .F. ) ;
#34472 = ORIENTED_EDGE ( 'NONE', *, *, #2146, .F. ) ;
#34473 = ORIENTED_EDGE ( 'NONE', *, *, #64345, .F. ) ;
#34475 =( BOUNDED_SURFACE ( )  B_SPLINE_SURFACE ( 3, 2, ( 
 ( #60280, #74813, #50536 ),
 ( #43539, #101247, #897 ),
 ( #93689, #75353, #83449 ),
 ( #33873, #10618, #75893 ) ),
 .UNSPECIFIED., .F., .F., .F. ) 
 B_SPLINE_SURFACE_WITH_KNOTS ( ( 4, 4 ),
 ( 3, 3 ),
 ( -1.617629641348372616E-16, 0.002038086101534472387 ),
 ( 0.000000000000000000, 1.000000000000000000 ),
 .UNSPECIFIED. ) 
 GEOMETRIC_REPRESENTATION_ITEM ( )  RATIONAL_B_SPLINE_SURFACE ( (
 ( 1.000000000000000000, 0.7927020107002088478, 1.000000000000000000),
 ( 1.000000000000000000, 0.8068894940779032243, 1.000000000000000000),
 ( 1.000000000000000000, 0.8212065780166589724, 1.000000000000000000),
 ( 1.000000000000000000, 0.8350736500407835994, 1.000000000000000000) ) ) 
 REPRESENTATION_ITEM ( '' )  SURFACE ( )  );
#34474 = CARTESIAN_POINT ( 'NONE',  ( 30.93388742938943636, 332.2947140929742886, 16.85568211106954095 ) ) ;
#34476 = VECTOR ( 'NONE', #324, 1000.000000000000000 ) ;
#34477 = EDGE_CURVE ( 'NONE', #59035, #34768, #100060, .T. ) ;
#34478 = CARTESIAN_POINT ( 'NONE',  ( -13.50000000000000355, 5.257130651325599757, -12.46102409077683326 ) ) ;
#34479 = CARTESIAN_POINT ( 'NONE',  ( 9.749646486200582274, 53.39674446004222119, 3.172643523868706961 ) ) ;
#34480 = ORIENTED_EDGE ( 'NONE', *, *, #96851, .T. ) ;
#34481 = CARTESIAN_POINT ( 'NONE',  ( -42.51080986285575847, 487.1495428173020059, 7.889844863765286931 ) ) ;
#34482 = CARTESIAN_POINT ( 'NONE',  ( -32.82691535583477105, 485.1045372766795367, 1.724905475514941999 ) ) ;
#34483 = DIRECTION ( 'NONE',  ( 0.000000000000000000, 0.000000000000000000, 1.000000000000000000 ) ) ;
#34484 = CARTESIAN_POINT ( 'NONE',  ( -68.42433815231228778, -57.68192485334662933, 143.8276693603407068 ) ) ;
#34485 = CIRCLE ( 'NONE', #5116, 4.000000000000000888 ) ;
#34486 = CARTESIAN_POINT ( 'NONE',  ( -30.25691101598808075, 17.21809272184236761, 39.73659737107620771 ) ) ;
#34487 = CARTESIAN_POINT ( 'NONE',  ( -35.44563196690202744, 355.0508310518326311, 1.542887188955126110 ) ) ;
#34488 = CARTESIAN_POINT ( 'NONE',  ( 69.67238219402268840, 6.975173280561618775E-15, 0.000000000000000000 ) ) ;
#34489 = CARTESIAN_POINT ( 'NONE',  ( -94.85933876937251341, -60.00000000000005684, 26.66572952598730595 ) ) ;
#34490 = CARTESIAN_POINT ( 'NONE',  ( -51.21545289590059724, -22.18992440698552215, 46.87729257222688517 ) ) ;
#34491 = AXIS2_PLACEMENT_3D ( 'NONE', #68017, #69100, #50234 ) ;
#34492 = DIRECTION ( 'NONE',  ( -1.000000000000000000, -1.224606353822377258E-16, -0.000000000000000000 ) ) ;
#34493 = ORIENTED_EDGE ( 'NONE', *, *, #67597, .T. ) ;
#34494 = DIRECTION ( 'NONE',  ( -0.5735764363510494901, -0.8191520442889894671, 0.000000000000000000 ) ) ;
#34495 = CARTESIAN_POINT ( 'NONE',  ( -9.581329576352811017, 294.6545431190999125, -2.865389023815151592 ) ) ;
#34496 = EDGE_CURVE ( 'NONE', #5037, #106154, #63765, .T. ) ;
#34497 = CIRCLE ( 'NONE', #8574, 4.000000000000001776 ) ;
#34498 = CARTESIAN_POINT ( 'NONE',  ( 13.80788977721196886, 1.043589425646265889, 14.96468393437554845 ) ) ;
#34499 = ORIENTED_EDGE ( 'NONE', *, *, #36895, .F. ) ;
#34501 = B_SPLINE_CURVE_WITH_KNOTS ( 'NONE', 3,
 ( #68951, #85663, #44673, #26394, #59258, #43591 ),
 .UNSPECIFIED., .F., .F.,
 ( 4, 2, 4 ),
 ( 0.01913986446825127405, 0.02104055318008571374, 0.02294124189192014995 ),
 .UNSPECIFIED. ) ;
#34500 = CARTESIAN_POINT ( 'NONE',  ( 5.856955515201468288, 246.2171094111913305, 1.326217528971456172 ) ) ;
#34502 = CARTESIAN_POINT ( 'NONE',  ( 106.0128498860127877, -38.37620446819514086, 196.3282179351167258 ) ) ;
#34503 = CARTESIAN_POINT ( 'NONE',  ( 49.25998992636648666, 12.93544608831382625, 15.83190612885223381 ) ) ;
#34504 = FACE_OUTER_BOUND ( 'NONE', #29754, .T. ) ;
#34505 = CARTESIAN_POINT ( 'NONE',  ( -9.601913782316103152, -10.04478976116414835, -12.77952306666688287 ) ) ;
#34506 = CARTESIAN_POINT ( 'NONE',  ( -88.20421627925436781, 42.00000000000000000, 23.70422451878991765 ) ) ;
#34507 = CARTESIAN_POINT ( 'NONE',  ( 89.25784830564948891, -29.99999999999999645, 189.0691493792201925 ) ) ;
#34508 = CARTESIAN_POINT ( 'NONE',  ( -11.27197637059353852, 43.63422769103391374, -13.37297449460065657 ) ) ;
#34509 = DIRECTION ( 'NONE',  ( -0.000000000000000000, -1.000000000000000000, -0.000000000000000000 ) ) ;
#34510 = ORIENTED_EDGE ( 'NONE', *, *, #25136, .F. ) ;
#34511 = ORIENTED_EDGE ( 'NONE', *, *, #20294, .F. ) ;
#34512 = CARTESIAN_POINT ( 'NONE',  ( 52.87357985501328983, -53.37229541906862806, 61.20433885443490141 ) ) ;
#34513 = CARTESIAN_POINT ( 'NONE',  ( 5.363597346081439454, 41.33266196706086504, -58.39526881795586633 ) ) ;
#34514 = AXIS2_PLACEMENT_3D ( 'NONE', #47638, #96224, #7707 ) ;
#34515 = CARTESIAN_POINT ( 'NONE',  ( -7.500000000000007105, 42.00000000000000711, -58.09827136975972195 ) ) ;
#34516 = ORIENTED_EDGE ( 'NONE', *, *, #255, .T. ) ;
#34517 = CARTESIAN_POINT ( 'NONE',  ( -90.76089875232968041, -38.34354976312844343, 6.139603795565712119 ) ) ;
#34518 = VERTEX_POINT ( 'NONE', #1340 ) ;
#34519 = CARTESIAN_POINT ( 'NONE',  ( 16.07816244837400177, 5.101897851402082296, 4.232350007277328352 ) ) ;
#34520 = CARTESIAN_POINT ( 'NONE',  ( 110.6797206184853621, -38.35606018631307990, 162.8134989819215832 ) ) ;
#34521 = CARTESIAN_POINT ( 'NONE',  ( 13.76825510980707001, 22.95345116768091742, 1.005136556262091307 ) ) ;
#34522 = CARTESIAN_POINT ( 'NONE',  ( 89.59839892097701863, -60.15026689961409545, 51.75009883440984026 ) ) ;
#34523 = CARTESIAN_POINT ( 'NONE',  ( -0.6462747240831046014, 46.14873864537771908, -16.41685720443574681 ) ) ;
#34524 = CARTESIAN_POINT ( 'NONE',  ( -25.24358573813086437, 305.1635960858602630, -9.714717598486441119 ) ) ;
#34525 = LINE ( 'NONE', #67394, #60862 ) ;
#34526 = FACE_OUTER_BOUND ( 'NONE', #90308, .T. ) ;
#34527 = CARTESIAN_POINT ( 'NONE',  ( 17.56579856165942388, 45.00000000000002132, 63.22721773057084249 ) ) ;
#34528 = ORIENTED_EDGE ( 'NONE', *, *, #83070, .F. ) ;
#34529 = CARTESIAN_POINT ( 'NONE',  ( 58.77986657205519805, -56.85775167507390648, 77.19278662003875979 ) ) ;
#34530 = DIRECTION ( 'NONE',  ( -1.000000000000000000, -1.224606353822377258E-16, -0.000000000000000000 ) ) ;
#34531 = ADVANCED_BREP_SHAPE_REPRESENTATION ( '', ( #19335, #10728 ), #66095 ) ;
#34532 = VECTOR ( 'NONE', #16824, 1000.000000000000000 ) ;
#34533 = CARTESIAN_POINT ( 'NONE',  ( -80.00000000000000000, -60.00000000000000000, -23.09707704303352926 ) ) ;
#34534 = CARTESIAN_POINT ( 'NONE',  ( -33.94783393359914214, 484.1261039197349305, 1.321740980884732686 ) ) ;
#34535 = CARTESIAN_POINT ( 'NONE',  ( -40.92186998856096380, 418.6655855945966209, 27.42381574914823972 ) ) ;
#34536 = DIRECTION ( 'NONE',  ( 0.000000000000000000, 0.000000000000000000, 1.000000000000000000 ) ) ;
#34537 = LINE ( 'NONE', #17269, #5956 ) ;
#34538 = CARTESIAN_POINT ( 'NONE',  ( 3.313708498984762052, -25.71874999999999645, -8.000000000000000000 ) ) ;
#34539 = CARTESIAN_POINT ( 'NONE',  ( -31.69663852278251781, -22.50060937418604112, 32.41930772561958207 ) ) ;
#34540 = VECTOR ( 'NONE', #43958, 1000.000000000000000 ) ;
#34541 = CARTESIAN_POINT ( 'NONE',  ( 16.32339259644602691, 43.86638882296026765, -4.188650191876186035 ) ) ;
#34542 = ORIENTED_EDGE ( 'NONE', *, *, #47419, .F. ) ;
#34543 = CARTESIAN_POINT ( 'NONE',  ( 86.34230506928878413, -18.09223085222674143, 171.9728401114309975 ) ) ;
#34544 = CARTESIAN_POINT ( 'NONE',  ( -27.99999999999999645, 0.000000000000000000, 0.000000000000000000 ) ) ;
#34545 = EDGE_LOOP ( 'NONE', ( #12529, #48684, #24003, #79371, #10511 ) ) ;
#34546 = DIRECTION ( 'NONE',  ( -0.000000000000000000, 1.000000000000000000, -0.000000000000000000 ) ) ;
#34547 = CIRCLE ( 'NONE', #1764, 3.309500000000001663 ) ;
#34548 = DIRECTION ( 'NONE',  ( -0.000000000000000000, -0.000000000000000000, -1.000000000000000000 ) ) ;
#34549 = PRESENTATION_STYLE_ASSIGNMENT (( #75493 ) ) ;
#34550 = CARTESIAN_POINT ( 'NONE',  ( 11.51753701180622613, 304.6035715647410598, 8.884240010328225523 ) ) ;
#34551 = EDGE_CURVE ( 'NONE', #12439, #65026, #24609, .T. ) ;
#34552 = CARTESIAN_POINT ( 'NONE',  ( -40.34222971095775989, -33.04913957068288255, -37.41736829041874302 ) ) ;
#34553 = CARTESIAN_POINT ( 'NONE',  ( 38.58349330513380693, 4.000000000000003553, 0.000000000000000000 ) ) ;
#34554 = VECTOR ( 'NONE', #21250, 1000.000000000000000 ) ;
#34555 = EDGE_CURVE ( 'NONE', #75282, #39269, #57458, .T. ) ;
#34556 = CIRCLE ( 'NONE', #101662, 8.000000000000000000 ) ;
#34557 = CARTESIAN_POINT ( 'NONE',  ( 43.68292435923753914, -60.00000000000001421, 58.09727205077876278 ) ) ;
#34558 = CARTESIAN_POINT ( 'NONE',  ( 7.413471587080148417, 107.6435215916832675, -3.013058070223554985 ) ) ;
#34559 = CARTESIAN_POINT ( 'NONE',  ( 14.05888324584411109, -14.89647871732337592, 31.68400523270869229 ) ) ;
#34561 = CARTESIAN_POINT ( 'NONE',  ( -12.03221859608693833, 21.77027319522744619, -7.001194585145907645 ) ) ;
#34560 = CARTESIAN_POINT ( 'NONE',  ( -32.95192556782836846, -34.33711306273711727, 42.52861473283787319 ) ) ;
#34562 = AXIS2_PLACEMENT_3D ( 'NONE', #23354, #56193, #48118 ) ;
#34563 = CARTESIAN_POINT ( 'NONE',  ( 11.84999999999999787, 3.309500000000003439, 0.000000000000000000 ) ) ;
#34564 = CARTESIAN_POINT ( 'NONE',  ( 24.37088254901632567, 295.3567874699774620, -9.892597027136796228 ) ) ;
#34565 = DIRECTION ( 'NONE',  ( -0.000000000000000000, 1.000000000000000000, -0.000000000000000000 ) ) ;
#34566 = CARTESIAN_POINT ( 'NONE',  ( 40.02592568779148507, -5.000000000000000000, 6.123233995736768255E-16 ) ) ;
#34567 = ORIENTED_EDGE ( 'NONE', *, *, #36655, .F. ) ;
#34568 =( GEOMETRIC_REPRESENTATION_CONTEXT ( 3 ) GLOBAL_UNCERTAINTY_ASSIGNED_CONTEXT ( ( #41860 ) ) GLOBAL_UNIT_ASSIGNED_CONTEXT ( ( #4728, #63506, #38188 ) ) REPRESENTATION_CONTEXT ( 'NONE', 'WORKASPACE' ) );
#34569 = CARTESIAN_POINT ( 'NONE',  ( 31.39943587937961311, -30.09334884167371271, -38.12009580904052086 ) ) ;
#34570 = CARTESIAN_POINT ( 'NONE',  ( -19.49999999999970512, 49.99999999999990052, 59.71562975593384692 ) ) ;
#34571 = UNCERTAINTY_MEASURE_WITH_UNIT (LENGTH_MEASURE( 1.000000000000000082E-05 ), #84528, 'distance_accuracy_value', 'NONE');
#34572 = CARTESIAN_POINT ( 'NONE',  ( 23.21751746555303342, 25.98869614573808207, 30.70617127781016720 ) ) ;
#34573 = CARTESIAN_POINT ( 'NONE',  ( 16.08349330513380337, 1.593028355512270962E-15, 0.000000000000000000 ) ) ;
#34575 = CARTESIAN_POINT ( 'NONE',  ( 35.59138712027602480, -60.22815789036102530, -34.49238072042346914 ) ) ;
#34574 = CARTESIAN_POINT ( 'NONE',  ( 4.189070928813702466, 54.25757288370531484, 6.683458472214860002 ) ) ;
#34576 = EDGE_LOOP ( 'NONE', ( #59236, #56673, #25282 ) ) ;
#34577 = CARTESIAN_POINT ( 'NONE',  ( -5.858881034796412202, -88.78586324002982622, 1.317748741875969687 ) ) ;
#34578 = CARTESIAN_POINT ( 'NONE',  ( -4.659280067791637059, 51.51274114929807979, 8.372560506775856837 ) ) ;
#34579 = ORIENTED_EDGE ( 'NONE', *, *, #31886, .T. ) ;
#34580 = VECTOR ( 'NONE', #6519, 1000.000000000000114 ) ;
#34581 = CARTESIAN_POINT ( 'NONE',  ( 11.08349330513380515, 1.593028355512270962E-15, 0.000000000000000000 ) ) ;
#34582 = EDGE_CURVE ( 'NONE', #1352, #94076, #13850, .T. ) ;
#34583 = DIRECTION ( 'NONE',  ( 0.000000000000000000, -1.000000000000000000, 0.000000000000000000 ) ) ;
#34584 = CIRCLE ( 'NONE', #94860, 5.000000000000001776 ) ;
#34585 = DIRECTION ( 'NONE',  ( 0.000000000000000000, 0.000000000000000000, -1.000000000000000000 ) ) ;
#34586 = CARTESIAN_POINT ( 'NONE',  ( -103.8364008283201940, -59.99999999999998579, 103.4830970040553666 ) ) ;
#34587 = DIRECTION ( 'NONE',  ( -0.4157805170468990563, -0.4085867419963748470, -0.8125167296179206522 ) ) ;
#34588 = FACE_OUTER_BOUND ( 'NONE', #95659, .T. ) ;
#34589 = CARTESIAN_POINT ( 'NONE',  ( 32.11411341898570981, 317.7919323371296514, -6.873671351699469412 ) ) ;
#34590 = FILL_AREA_STYLE ('',( #35653 ) ) ;
#34591 = CARTESIAN_POINT ( 'NONE',  ( -34.24135949700323778, 434.2621254486631983, 10.63646157856311802 ) ) ;
#34592 = CARTESIAN_POINT ( 'NONE',  ( -85.96019084596983362, -18.45086501588650307, 165.1132801238956063 ) ) ;
#34593 = ORIENTED_EDGE ( 'NONE', *, *, #45167, .F. ) ;
#34594 = CARTESIAN_POINT ( 'NONE',  ( -2.100000000000004530, 1.040949779275250140E-15, -8.500000000000000000 ) ) ;
#34595 = ORIENTED_EDGE ( 'NONE', *, *, #34890, .T. ) ;
#34596 = ORIENTED_EDGE ( 'NONE', *, *, #72874, .T. ) ;
#34597 = CARTESIAN_POINT ( 'NONE',  ( -3.398604459340648809, 303.8518027749813086, -10.00000000027307223 ) ) ;
#34598 = EDGE_CURVE ( 'NONE', #14406, #52643, #91456, .T. ) ;
#34599 = EDGE_CURVE ( 'NONE', #82896, #26696, #31083, .T. ) ;
#34600 = CARTESIAN_POINT ( 'NONE',  ( 0.1061556211655340504, 6.421950209808279020, 1.876855952934452620 ) ) ;
#34601 = VERTEX_POINT ( 'NONE', #34837 ) ;
#34602 = AXIS2_PLACEMENT_3D ( 'NONE', #101187, #8969, #75841 ) ;
#34603 = CARTESIAN_POINT ( 'NONE',  ( 0.000000000000000000, 0.000000000000000000, 0.000000000000000000 ) ) ;
#34604 = DIRECTION ( 'NONE',  ( 0.000000000000000000, 0.000000000000000000, -1.000000000000000000 ) ) ;
#34605 = CARTESIAN_POINT ( 'NONE',  ( -6.826399921716642005, -2.638123634694639730, -6.344399053232586461 ) ) ;
#34606 = CIRCLE ( 'NONE', #98320, 1.000000000000004441 ) ;
#34607 = CARTESIAN_POINT ( 'NONE',  ( -2.020600889975352921, 14.39097068952101743, 6.705821464114419150 ) ) ;
#34608 = CARTESIAN_POINT ( 'NONE',  ( -1.013900655853712918, 53.56097311263275174, 9.749521719900309691 ) ) ;
#34609 = CARTESIAN_POINT ( 'NONE',  ( -5.000000000000000000, -13.83000330156203006, 11.07490067672335066 ) ) ;
#34610 = CARTESIAN_POINT ( 'NONE',  ( 99.88996038257948840, -14.21045842199439946, 111.7630621600675198 ) ) ;
#34611 = CARTESIAN_POINT ( 'NONE',  ( -97.75001763179835734, -59.99999999999991473, 204.9118596629033675 ) ) ;
#34612 = CARTESIAN_POINT ( 'NONE',  ( -57.77607850381885157, -32.55063884621782933, 63.57510918078556017 ) ) ;
#34613 = ORIENTED_EDGE ( 'NONE', *, *, #16880, .T. ) ;
#34614 = DIRECTION ( 'NONE',  ( -1.000000000000000000, -1.224606353822377258E-16, -0.000000000000000000 ) ) ;
#34615 = CARTESIAN_POINT ( 'NONE',  ( 2.377971214860273304E-07, -59.99999999999998579, 39.63907915656436387 ) ) ;
#34616 = MECHANICAL_DESIGN_GEOMETRIC_PRESENTATION_REPRESENTATION (  '', ( #79541 ), #39207 ) ;
#34617 = EDGE_LOOP ( 'NONE', ( #16021, #28489, #80798, #60646, #104467, #66980 ) ) ;
#34618 = CARTESIAN_POINT ( 'NONE',  ( 5.174065430531224585, -60.35881594324177968, 33.93881697174609258 ) ) ;
#34619 = CARTESIAN_POINT ( 'NONE',  ( -101.9946220817418663, -45.26526879604974596, 189.2069091854172598 ) ) ;
#34620 = EDGE_CURVE ( 'NONE', #93549, #27771, #96485, .T. ) ;
#34621 = CARTESIAN_POINT ( 'NONE',  ( 15.33074037313114246, 43.81340351859345361, -89.42371653412330090 ) ) ;
#34622 = EDGE_LOOP ( 'NONE', ( #7676, #67767, #37578 ) ) ;
#34623 = CARTESIAN_POINT ( 'NONE',  ( 19.49683355508617311, 49.99979114368868949, 59.98567652804494799 ) ) ;
#34624 = CARTESIAN_POINT ( 'NONE',  ( -71.26649465934139016, -60.00000000000000000, 149.0547838307006430 ) ) ;
#34625 = CARTESIAN_POINT ( 'NONE',  ( 36.48001451349853852, 26.06917801760574704, -11.58280953890916720 ) ) ;
#34626 = CARTESIAN_POINT ( 'NONE',  ( -7.188101187500000044, -18.78125000204838457, -8.802885111219163269E-16 ) ) ;
#34627 = VECTOR ( 'NONE', #47607, 1000.000000000000227 ) ;
#34628 = DIRECTION ( 'NONE',  ( -0.000000000000000000, -1.000000000000000000, -0.000000000000000000 ) ) ;
#34629 = CARTESIAN_POINT ( 'NONE',  ( 42.98746414932995208, 1.482358050883964840E-15, 0.000000000000000000 ) ) ;
#34630 = CARTESIAN_POINT ( 'NONE',  ( 8.521411446770892795, 0.000000000000000000, 14.76969908562504408 ) ) ;
#34631 = CARTESIAN_POINT ( 'NONE',  ( -31.03867016165222026, 468.3124986733989772, 18.90871194958903345 ) ) ;
#34632 = CIRCLE ( 'NONE', #39755, 5.000000000000011546 ) ;
#34633 = CARTESIAN_POINT ( 'NONE',  ( 29.01988888469873018, 321.8047804620298393, 14.12772110426748284 ) ) ;
#34634 = ADVANCED_FACE ( 'NONE', ( #94658 ), #35097, .T. ) ;
#34635 = CARTESIAN_POINT ( 'NONE',  ( -9.508798884265706519, 44.08617864742008408, -13.17536625225998215 ) ) ;
#34636 = SURFACE_SIDE_STYLE ('',( #73440 ) ) ;
#34637 = CARTESIAN_POINT ( 'NONE',  ( 86.31767834415556706, -59.99999999999999289, 20.32226923651656847 ) ) ;
#34638 = CARTESIAN_POINT ( 'NONE',  ( -31.57922577310468526, -32.55042699868089784, 32.45668791033146050 ) ) ;
#34639 = CIRCLE ( 'NONE', #61, 5.000000000000000000 ) ;
#34640 = CARTESIAN_POINT ( 'NONE',  ( 46.25750148850488586, -32.61358005543022642, 43.24939596980505030 ) ) ;
#34641 = CARTESIAN_POINT ( 'NONE',  ( -32.00986601473474735, 486.4616239121606895, 6.105527853528552207 ) ) ;
#34642 = COLOUR_RGB ( '', 0.31764706, 0.68627451, 0.89019608) ;
#34643 = EDGE_LOOP ( 'NONE', ( #101627, #1297, #21835, #24153, #67657, #47319 ) ) ;
#34644 = CARTESIAN_POINT ( 'NONE',  ( -6.943926999490791729, 85.53300992626147092, -3.973092371898545139 ) ) ;
#34645 = CARTESIAN_POINT ( 'NONE',  ( -81.44491332629058888, -38.84114197386964662, 195.2043805330731345 ) ) ;
#34646 = VERTEX_POINT ( 'NONE', #11570 ) ;
#34647 = CYLINDRICAL_SURFACE ( 'NONE', #9037, 7.000000000000000000 ) ;
#34648 = CARTESIAN_POINT ( 'NONE',  ( 10.44019003300671500, -59.99999999999997158, 33.89246852536604848 ) ) ;
#34650 = EDGE_CURVE ( 'NONE', #61487, #86629, #102189, .T. ) ;
#34649 = LINE ( 'NONE', #84226, #25204 ) ;
#34651 = CARTESIAN_POINT ( 'NONE',  ( -7.493944919676032157, 40.57567429012536309, -59.86116873889386625 ) ) ;
#34652 = CARTESIAN_POINT ( 'NONE',  ( 9.701736001019304112, 15.75130202679986624, -2.450449656239129137 ) ) ;
#34653 = DIRECTION ( 'NONE',  ( 0.000000000000000000, 0.000000000000000000, -1.000000000000000000 ) ) ;
#34654 = CARTESIAN_POINT ( 'NONE',  ( -24.09682408347498139, 306.3733087561651587, 9.274668387549985127 ) ) ;
#34655 = CARTESIAN_POINT ( 'NONE',  ( 16.64348903516523848, 45.88445698070336221, 4.157797401561420081 ) ) ;
#34656 = CARTESIAN_POINT ( 'NONE',  ( 103.6205286009478215, -60.00000000000002132, 102.2157128241041590 ) ) ;
#34657 = DIRECTION ( 'NONE',  ( 0.5735764363510557073, -0.8191520442889850262, 1.003171929053516612E-16 ) ) ;
#34658 = DIRECTION ( 'NONE',  ( 0.000000000000000000, -1.000000000000000000, 0.000000000000000000 ) ) ;
#34659 = EDGE_LOOP ( 'NONE', ( #50199, #94060, #51582, #22289 ) ) ;
#34660 = AXIS2_PLACEMENT_3D ( 'NONE', #9853, #33633, #66513 ) ;
#34661 = CARTESIAN_POINT ( 'NONE',  ( -97.33989514445055136, -29.99999999999995026, 190.9629009002478597 ) ) ;
#34662 = ORIENTED_EDGE ( 'NONE', *, *, #82849, .T. ) ;
#34663 = CYLINDRICAL_SURFACE ( 'NONE', #54498, 8.000000000000000000 ) ;
#34664 = CARTESIAN_POINT ( 'NONE',  ( 30.60303901177592323, 328.0989884029825703, 15.88304988518486915 ) ) ;
#34665 = CARTESIAN_POINT ( 'NONE',  ( 9.176645556628253431, 29.47260967593268788, 3.973966573947708802 ) ) ;
#34666 = CARTESIAN_POINT ( 'NONE',  ( -7.188101187500000044, -18.78125000204838457, -8.802885111219163269E-16 ) ) ;
#34667 = AXIS2_PLACEMENT_3D ( 'NONE', #37218, #51763, #35629 ) ;
#34668 = CARTESIAN_POINT ( 'NONE',  ( -6.043427762771305112, -5.000000000000002665, -95.48543666094731464 ) ) ;
#34669 = AXIS2_PLACEMENT_3D ( 'NONE', #33856, #65663, #99612 ) ;
#34670 = B_SPLINE_CURVE_WITH_KNOTS ( 'NONE', 3,
 ( #33550, #90713, #49161, #81515, #1128, #58, #49708, #42683, #82068, #66421, #58335, #90173, #48631, #8187, #82614, #66974, #42145, #8716, #9770, #41624, #41094, #65894, #99306, #99853 ),
 .UNSPECIFIED., .F., .F.,
 ( 4, 2, 2, 2, 2, 2, 2, 2, 2, 2, 2, 4 ),
 ( 0.004982639409921949328, 0.005234721249241279864, 0.005486803088560610400, 0.005990966767199284483, 0.006495130445837957699, 0.006999294124476631782, 0.007251375963795969257, 0.007503457803115305864, 0.008007621481753976478, 0.008511785160392649693, 0.008763866999711983699, 0.009015948839031319439 ),
 .UNSPECIFIED. ) ;
#34671 = DIRECTION ( 'NONE',  ( 0.000000000000000000, -1.000000000000000000, 0.000000000000000000 ) ) ;
#34673 = ORIENTED_EDGE ( 'NONE', *, *, #59744, .T. ) ;
#34672 = CYLINDRICAL_SURFACE ( 'NONE', #42614, 1.250000000000001110 ) ;
#34674 = CARTESIAN_POINT ( 'NONE',  ( 84.36382179597347886, -25.57599070838802646, 160.3264503554693761 ) ) ;
#34675 = CARTESIAN_POINT ( 'NONE',  ( -46.00000000000000000, 462.4470051410875726, 6.587392890220048258 ) ) ;
#34676 = DIRECTION ( 'NONE',  ( 0.000000000000000000, -1.000000000000000000, 0.000000000000000000 ) ) ;
#34677 = ORIENTED_EDGE ( 'NONE', *, *, #92997, .F. ) ;
#34678 = CARTESIAN_POINT ( 'NONE',  ( -7.500000000000006217, 152.0000000000000000, 5.000000000000000000 ) ) ;
#34679 = CARTESIAN_POINT ( 'NONE',  ( -4.852941176792862521, 41.29999999999999005, -70.80672828645249695 ) ) ;
#34680 = CARTESIAN_POINT ( 'NONE',  ( 5.082755093536325930, -9.968750002048384573, -5.082755093536325042 ) ) ;
#34681 = DIRECTION ( 'NONE',  ( 0.000000000000000000, -1.000000000000000000, 0.000000000000000000 ) ) ;
#34682 = CARTESIAN_POINT ( 'NONE',  ( 11.36440886748424361, 45.70401808670207799, 13.50555938308142245 ) ) ;
#34683 = B_SPLINE_CURVE_WITH_KNOTS ( 'NONE', 3,
 ( #104071, #6426, #47947, #30214, #6966, #73284, #71694, #30757, #106179, #32342, #63643, #72243, #79801, #98107, #47424, #5899, #96531, #22663 ),
 .UNSPECIFIED., .F., .F.,
 ( 4, 2, 2, 2, 2, 2, 2, 2, 4 ),
 ( 0.5671276150162705143, 0.6212366631392367555, 0.6753457112622028857, 0.7294547593851690159, 0.7835638075081352572, 0.8376728556311014984, 0.8917819037540676286, 0.9458909518770337588, 1.000000000000000000 ),
 .UNSPECIFIED. ) ;
#34684 = DIRECTION ( 'NONE',  ( -0.1270361284032253957, -0.9918980905719697594, 0.000000000000000000 ) ) ;
#34685 = EDGE_CURVE ( 'NONE', #86295, #55315, #38238, .T. ) ;
#34686 = VERTEX_POINT ( 'NONE', #53638 ) ;
#34687 =( LENGTH_UNIT ( ) NAMED_UNIT ( * ) SI_UNIT ( .MILLI., .METRE. ) );
#34688 = DIRECTION ( 'NONE',  ( -0.5735764363510494901, -0.8191520442889894671, 0.000000000000000000 ) ) ;
#34689 = EDGE_CURVE ( 'NONE', #27470, #95088, #44841, .T. ) ;
#34690 = CARTESIAN_POINT ( 'NONE',  ( -5.000000000000000000, -57.63307216814066436, 11.09944177371828289 ) ) ;
#34691 = CARTESIAN_POINT ( 'NONE',  ( 0.000000000000000000, -1.200583151104953394, 112.0000000000000000 ) ) ;
#34692 = FACE_OUTER_BOUND ( 'NONE', #76602, .T. ) ;
#34693 = CARTESIAN_POINT ( 'NONE',  ( 5.082755093536324154, -26.84375000204838813, 5.082755093536326818 ) ) ;
#34694 = FACE_OUTER_BOUND ( 'NONE', #97249, .T. ) ;
#34695 = CARTESIAN_POINT ( 'NONE',  ( 7.738564917571006063, 52.10541356253746414, 1.834888082847005997 ) ) ;
#34696 = FACE_OUTER_BOUND ( 'NONE', #43569, .T. ) ;
#34697 = ORIENTED_EDGE ( 'NONE', *, *, #12344, .T. ) ;
#34698 = AXIS2_PLACEMENT_3D ( 'NONE', #8747, #83173, #26582 ) ;
#34699 =( NAMED_UNIT ( * ) PLANE_ANGLE_UNIT ( ) SI_UNIT ( $, .RADIAN. ) );
#34700 = CIRCLE ( 'NONE', #79473, 2.000000000000000000 ) ;
#34701 = CARTESIAN_POINT ( 'NONE',  ( -9.995757844698658801, 7.506119843431433125, -4.999999999999999112 ) ) ;
#34702 = LINE ( 'NONE', #2276, #1563 ) ;
#34703 = EDGE_CURVE ( 'NONE', #79952, #60839, #3482, .T. ) ;
#34704 = ORIENTED_EDGE ( 'NONE', *, *, #11734, .T. ) ;
#34705 = CIRCLE ( 'NONE', #72544, 4.000000000000007105 ) ;
#34706 =( NAMED_UNIT ( * ) PLANE_ANGLE_UNIT ( ) SI_UNIT ( $, .RADIAN. ) );
#34707 = CARTESIAN_POINT ( 'NONE',  ( 0.000000000000000000, -3.252606517456512513E-15, -10.00000000000000178 ) ) ;
#34709 = CARTESIAN_POINT ( 'NONE',  ( 31.03678703375048187, 438.6650838204853926, 21.86890379897692327 ) ) ;
#34708 = AXIS2_PLACEMENT_3D ( 'NONE', #34421, #51616, #33341 ) ;
#34710 = EDGE_CURVE ( 'NONE', #103853, #28486, #17272, .T. ) ;
#34711 = CARTESIAN_POINT ( 'NONE',  ( -0.9888730084721008007, 12.53170386526280211, -49.73224619698263638 ) ) ;
#34712 = LINE ( 'NONE', #7729, #4533 ) ;
#34713 = CARTESIAN_POINT ( 'NONE',  ( 12.12012043129136529, 302.5867796431402326, 9.880676409032833618 ) ) ;
#34714 = CARTESIAN_POINT ( 'NONE',  ( -78.47844370984229556, -60.00000000000001421, 193.7840747555254950 ) ) ;
#34715 = CARTESIAN_POINT ( 'NONE',  ( 9.203147141233843698, 43.65617212538753478, -14.80172050158656383 ) ) ;
#34716 = CARTESIAN_POINT ( 'NONE',  ( -43.41290683822509067, 487.0833545439620593, 7.569976829064872348 ) ) ;
#34717 = FILL_AREA_STYLE ('',( #92909 ) ) ;
#34718 = CARTESIAN_POINT ( 'NONE',  ( -84.44772399558564757, -46.57216599554897130, 186.0917793300985750 ) ) ;
#34719 = EDGE_LOOP ( 'NONE', ( #81273, #43158, #31734, #66335 ) ) ;
#34720 =( NAMED_UNIT ( * ) PLANE_ANGLE_UNIT ( ) SI_UNIT ( $, .RADIAN. ) );
#34721 = EDGE_LOOP ( 'NONE', ( #44509, #78743 ) ) ;
#34722 = CARTESIAN_POINT ( 'NONE',  ( 102.6464385083043283, 1.030564683017419500E-14, 0.000000000000000000 ) ) ;
#34723 = EDGE_CURVE ( 'NONE', #88009, #103713, #29382, .T. ) ;
#34724 = EDGE_CURVE ( 'NONE', #65781, #10582, #43128, .T. ) ;
#34725 = CARTESIAN_POINT ( 'NONE',  ( 3.787335548950983899, -1.092153040503932582, 104.1352136098632997 ) ) ;
#34726 = CARTESIAN_POINT ( 'NONE',  ( -83.89485214324410833, -45.26916324968230043, 4.375863353757575069 ) ) ;
#34728 = B_SPLINE_CURVE_WITH_KNOTS ( 'NONE', 3,
 ( #95885, #54319, #4744, #103436, #71580, #103955, #62985, #54865 ),
 .UNSPECIFIED., .F., .F.,
 ( 4, 2, 2, 4 ),
 ( 0.000000000000000000, 0.5000000000000000000, 0.7500000000000000000, 1.000000000000000000 ),
 .UNSPECIFIED. ) ;
#34727 = DIRECTION ( 'NONE',  ( 0.2776092459793209066, -0.06763270420234848701, 0.9583104527599972666 ) ) ;
#34729 = CARTESIAN_POINT ( 'NONE',  ( -16.02936841876867291, 43.70325603760588251, 6.508067950779399702 ) ) ;
#34730 = CIRCLE ( 'NONE', #96684, 4.000000000000001776 ) ;
#34731 = DIRECTION ( 'NONE',  ( 0.000000000000000000, 1.000000000000000000, 0.000000000000000000 ) ) ;
#34732 = CARTESIAN_POINT ( 'NONE',  ( -5.958501008717178138, -13.50719282745122563, 13.62690037880521920 ) ) ;
#34733 = CARTESIAN_POINT ( 'NONE',  ( 88.20421627921849961, 42.00000000000000000, -23.70422451876603631 ) ) ;
#34734 = CARTESIAN_POINT ( 'NONE',  ( 10.12668159690567826, 0.000000000000000000, -9.226681596905679683 ) ) ;
#34735 = CARTESIAN_POINT ( 'NONE',  ( 72.31505286502601848, -14.21045842199433373, 125.5027806063605595 ) ) ;
#34736 = DIRECTION ( 'NONE',  ( -0.000000000000000000, 1.000000000000000000, -0.000000000000000000 ) ) ;
#34737 = CARTESIAN_POINT ( 'NONE',  ( -89.80806051762600362, -30.00000000000005684, 26.19611557095339904 ) ) ;
#34738 = CARTESIAN_POINT ( 'NONE',  ( -67.34159380897033031, -56.86460610103189595, 103.2059302081343901 ) ) ;
#34739 = ORIENTED_EDGE ( 'NONE', *, *, #97312, .F. ) ;
#34740 = CARTESIAN_POINT ( 'NONE',  ( 62.54367487775790124, -59.99999999999994316, 118.0935059193921575 ) ) ;
#34741 = CARTESIAN_POINT ( 'NONE',  ( -65.06413714112721891, 40.83767784448016158, 0.8155869308389190886 ) ) ;
#34742 = CARTESIAN_POINT ( 'NONE',  ( 44.09900958218985778, -59.99999999999509726, 64.08949965347366629 ) ) ;
#34743 = VERTEX_POINT ( 'NONE', #35368 ) ;
#34744 = CARTESIAN_POINT ( 'NONE',  ( 8.559508646656103892, 51.55638410492932167, -4.031152949375861105 ) ) ;
#34745 = CARTESIAN_POINT ( 'NONE',  ( 5.082755093536324154, -25.71875000204838813, 5.082755093536326818 ) ) ;
#34746 = EDGE_CURVE ( 'NONE', #105753, #64733, #49966, .T. ) ;
#34747 = CARTESIAN_POINT ( 'NONE',  ( -0.3375343507057477765, 27.30883569689895296, -40.71519194888146131 ) ) ;
#34748 = VERTEX_POINT ( 'NONE', #38028 ) ;
#34749 = LINE ( 'NONE', #90831, #23469 ) ;
#34750 = CARTESIAN_POINT ( 'NONE',  ( 16.84999999999999787, 3.309500000000003439, 0.000000000000000000 ) ) ;
#34751 = CARTESIAN_POINT ( 'NONE',  ( -10.61958778326375175, 43.19936960986098740, 15.37415780603073578 ) ) ;
#34752 = CARTESIAN_POINT ( 'NONE',  ( -2.977408999572650039, -15.68750000204838457, -7.188101187500001821 ) ) ;
#34753 = CARTESIAN_POINT ( 'NONE',  ( -49.22174280021781811, 12.91003493663466628, 15.98497293137739561 ) ) ;
#34754 = CARTESIAN_POINT ( 'NONE',  ( -7.500000000000000000, -4.330127018922201643, -10.00000000000000000 ) ) ;
#34755 = SURFACE_STYLE_FILL_AREA ( #28261 ) ;
#34756 = CARTESIAN_POINT ( 'NONE',  ( -9.739726766105677669, 49.99999999999999289, -82.38252115500968387 ) ) ;
#34757 = EDGE_CURVE ( 'NONE', #101241, #48515, #70694, .T. ) ;
#34758 = CARTESIAN_POINT ( 'NONE',  ( -8.000000000000000000, -14.84374999999999289, -3.313708498984762496 ) ) ;
#34759 = CARTESIAN_POINT ( 'NONE',  ( 12.13034742782427955, 48.00000000000000000, -93.82352941176471006 ) ) ;
#34760 = UNCERTAINTY_MEASURE_WITH_UNIT (LENGTH_MEASURE( 1.000000000000000082E-05 ), #76236, 'distance_accuracy_value', 'NONE');
#34761 = ORIENTED_EDGE ( 'NONE', *, *, #15713, .T. ) ;
#34762 = CARTESIAN_POINT ( 'NONE',  ( -6.974441889477841272, 41.03925918661743566, -70.79755109234586996 ) ) ;
#34763 = CARTESIAN_POINT ( 'NONE',  ( 31.31534349697233921, -22.13725448416145980, 30.43540540151346718 ) ) ;
#34764 = CARTESIAN_POINT ( 'NONE',  ( 35.53880462860536937, 395.8745130103307019, 6.882435263909567169 ) ) ;
#34765 = ORIENTED_EDGE ( 'NONE', *, *, #1653, .F. ) ;
#34766 = EDGE_CURVE ( 'NONE', #24805, #84222, #30452, .T. ) ;
#34767 = CARTESIAN_POINT ( 'NONE',  ( -0.7804417267264509572, 13.54273479047304285, 51.48091406469324482 ) ) ;
#34768 = VERTEX_POINT ( 'NONE', #71405 ) ;
#34769 = CARTESIAN_POINT ( 'NONE',  ( 0.000000000000000000, -5.629165124598847214, 3.250000000000005329 ) ) ;
#34770 = CARTESIAN_POINT ( 'NONE',  ( 4.852941176470595863, 39.99999999999999289, -70.80672828634229177 ) ) ;
#34771 = CARTESIAN_POINT ( 'NONE',  ( -44.26720285007399269, 485.4142925135642486, 2.510465450176162960 ) ) ;
#34772 =( NAMED_UNIT ( * ) SI_UNIT ( $, .STERADIAN. ) SOLID_ANGLE_UNIT ( ) );
#34773 = DIRECTION ( 'NONE',  ( -1.000000000000000000, -0.000000000000000000, -0.000000000000000000 ) ) ;
#34774 = ORIENTED_EDGE ( 'NONE', *, *, #28060, .F. ) ;
#34775 = CARTESIAN_POINT ( 'NONE',  ( 87.25490207742672055, -60.00000000000000711, -22.40272287519551853 ) ) ;
#34776 = DIRECTION ( 'NONE',  ( 0.000000000000000000, -1.000000000000000000, 0.000000000000000000 ) ) ;
#34777 = CONICAL_SURFACE ( 'NONE', #58846, 7.000000000000000000, 0.9599310885968753704 ) ;
#34779 = EDGE_CURVE ( 'NONE', #62342, #60518, #58608, .T. ) ;
#34778 = COLOUR_RGB ( '', 0.31764706, 0.68627451, 0.89019608) ;
#34780 = DIRECTION ( 'NONE',  ( -1.000000000000000000, -1.224606353822377258E-16, -0.000000000000000000 ) ) ;
#34781 =( BOUNDED_SURFACE ( )  B_SPLINE_SURFACE ( 3, 2, ( 
 ( #84343, #102108, #103187 ),
 ( #94581, #51957, #19657 ),
 ( #3957, #35285, #20187 ),
 ( #10436, #28268, #69756 ),
 ( #61137, #18566, #53039 ),
 ( #86498, #20729, #2344 ),
 ( #59548, #84872, #78364 ),
 ( #12557, #101049, #27203 ),
 ( #45496, #60093, #10957 ),
 ( #37423, #4486, #92415 ),
 ( #60620, #19119, #76769 ),
 ( #52489, #43874, #85409 ) ),
 .UNSPECIFIED., .F., .F., .F. ) 
 B_SPLINE_SURFACE_WITH_KNOTS ( ( 4, 2, 2, 2, 2, 4 ),
 ( 3, 3 ),
 ( -6.938893903907228378E-18, 0.001187588843296126778, 0.001781383264944193636, 0.002375177686592260494, 0.003562766529888394210, 0.004750355373184527927 ),
 ( 0.000000000000000000, 1.000000000000000000 ),
 .UNSPECIFIED. ) 
 GEOMETRIC_REPRESENTATION_ITEM ( )  RATIONAL_B_SPLINE_SURFACE ( (
 ( 1.000000000000000000, 0.9359444767143315635, 1.000000000000000000),
 ( 1.000000000000000000, 0.9295581727144293094, 1.000000000000000000),
 ( 1.000000000000000000, 0.9234593375675015370, 1.000000000000000000),
 ( 1.000000000000000000, 0.9150808072273350913, 1.000000000000000000),
 ( 1.000000000000000000, 0.9124161408737814227, 1.000000000000000000),
 ( 1.000000000000000000, 0.9074047588826392730, 1.000000000000000000),
 ( 1.000000000000000000, 0.9050663310860352917, 1.000000000000000000),
 ( 1.000000000000000000, 0.8987692007139010952, 1.000000000000000000),
 ( 1.000000000000000000, 0.8954627112850603865, 1.000000000000000000),
 ( 1.000000000000000000, 0.8909338199771259514, 1.000000000000000000),
 ( 1.000000000000000000, 0.8897377579433781714, 1.000000000000000000),
 ( 1.000000000000000000, 0.8897565210026093796, 1.000000000000000000) ) ) 
 REPRESENTATION_ITEM ( '' )  SURFACE ( )  );
#34782 = VECTOR ( 'NONE', #41931, 1000.000000000000000 ) ;
#34783 = DIRECTION ( 'NONE',  ( 0.000000000000000000, -1.000000000000000000, 0.000000000000000000 ) ) ;
#34784 = ORIENTED_EDGE ( 'NONE', *, *, #82026, .T. ) ;
#34785 = DIRECTION ( 'NONE',  ( -1.000000000000000000, -0.000000000000000000, -0.000000000000000000 ) ) ;
#34786 = ORIENTED_EDGE ( 'NONE', *, *, #40339, .F. ) ;
#34787 = VERTEX_POINT ( 'NONE', #14754 ) ;
#34788 = CARTESIAN_POINT ( 'NONE',  ( 7.412906595240167817, 82.35811727147745387, 3.014362223629231341 ) ) ;
#34789 = CARTESIAN_POINT ( 'NONE',  ( 6.585468679846623985, -3.617797563910821079, -6.733790807807556789 ) ) ;
#34790 = CARTESIAN_POINT ( 'NONE',  ( -16.11301951124610099, 35.08081939474628541, -21.97927874236063417 ) ) ;
#34791 = DIRECTION ( 'NONE',  ( -1.000000000000000000, -1.224606353822377258E-16, -0.000000000000000000 ) ) ;
#34792 = CARTESIAN_POINT ( 'NONE',  ( 83.10716226388446159, -37.79806746364081249, -10.04868559838506670 ) ) ;
#34793 = CARTESIAN_POINT ( 'NONE',  ( -37.61245331168856154, 304.9616315839961089, -7.671943079217724559 ) ) ;
#34794 = DIRECTION ( 'NONE',  ( -1.000000000000000000, -1.224606353822377258E-16, -0.000000000000000000 ) ) ;
#34795 = CARTESIAN_POINT ( 'NONE',  ( 12.50000000000000355, 27.55321248621640606, -45.11687107644303296 ) ) ;
#34796 = EDGE_LOOP ( 'NONE', ( #74656, #28956, #83212, #12391, #79280, #70454 ) ) ;
#34797 = CARTESIAN_POINT ( 'NONE',  ( 6.499999999999999112, 3.752776749732595452, -0.7999999999999977129 ) ) ;
#34798 = AXIS2_PLACEMENT_3D ( 'NONE', #21414, #36552, #11145 ) ;
#34799 = ORIENTED_EDGE ( 'NONE', *, *, #59305, .T. ) ;
#34800 = LINE ( 'NONE', #92452, #1974 ) ;
#34801 = CARTESIAN_POINT ( 'NONE',  ( 2.503857664561936320E-16, -8.660254037844401509, -7.422398894150040505 ) ) ;
#34802 = B_SPLINE_CURVE_WITH_KNOTS ( 'NONE', 3,
 ( #72471, #63874, #105378, #65449, #96240, #22893, #79503, #97800 ),
 .UNSPECIFIED., .F., .F.,
 ( 4, 2, 2, 4 ),
 ( 0.02285338878549946634, 0.02519297481083175930, 0.02636276782349790751, 0.02753256083616405225 ),
 .UNSPECIFIED. ) ;
#34804 = VERTEX_POINT ( 'NONE', #80025 ) ;
#34803 = DIRECTION ( 'NONE',  ( 0.000000000000000000, -1.000000000000000000, 0.000000000000000000 ) ) ;
#34805 = CARTESIAN_POINT ( 'NONE',  ( 71.85279723664308449, -56.85193184329963856, 119.4851267806225508 ) ) ;
#34806 = ORIENTED_EDGE ( 'NONE', *, *, #49904, .T. ) ;
#34807 = CARTESIAN_POINT ( 'NONE',  ( 2.406968675509042921, -53.72544228834411939, 40.79299294490898831 ) ) ;
#34808 = CARTESIAN_POINT ( 'NONE',  ( 3.202579070477590495, -48.99829897912727006, 104.2977202916031700 ) ) ;
#34809 = CARTESIAN_POINT ( 'NONE',  ( 5.082755093536325930, -27.96875000204838457, -5.082755093536325042 ) ) ;
#34810 = CARTESIAN_POINT ( 'NONE',  ( -84.95435462066053844, -57.67079294309295534, -27.04779982294425977 ) ) ;
#34811 = EDGE_CURVE ( 'NONE', #90141, #89211, #13697, .T. ) ;
#34812 = ORIENTED_EDGE ( 'NONE', *, *, #97991, .F. ) ;
#34813 = CIRCLE ( 'NONE', #3756, 5.000000000000002665 ) ;
#34814 =( NAMED_UNIT ( * ) PLANE_ANGLE_UNIT ( ) SI_UNIT ( $, .RADIAN. ) );
#34815 = LINE ( 'NONE', #59062, #7558 ) ;
#34816 = CARTESIAN_POINT ( 'NONE',  ( 102.9736477862243191, -45.28271309083630314, 185.6071471573901874 ) ) ;
#34817 = ADVANCED_FACE ( 'NONE', ( #37500 ), #104816, .F. ) ;
#34818 = CYLINDRICAL_SURFACE ( 'NONE', #4823, 4.000000000000000888 ) ;
#34819 = AXIS2_PLACEMENT_3D ( 'NONE', #75248, #10521, #1349 ) ;
#34820 = CARTESIAN_POINT ( 'NONE',  ( 12.33349330513380337, 1.593028355512270567E-15, 0.000000000000000000 ) ) ;
#34821 = CARTESIAN_POINT ( 'NONE',  ( 3.313708498984762496, -21.96875000409677270, 7.999999999999998224 ) ) ;
#34822 = CARTESIAN_POINT ( 'NONE',  ( 0.000000000000000000, -3.000000000000000000, 8.000000000000000000 ) ) ;
#34823 = LINE ( 'NONE', #75770, #18146 ) ;
#34824 = CARTESIAN_POINT ( 'NONE',  ( -7.149999999999890221, 41.65000000000012648, -59.82695526680724640 ) ) ;
#34825 = CYLINDRICAL_SURFACE ( 'NONE', #60735, 5.000000000000002665 ) ;
#34826 = CARTESIAN_POINT ( 'NONE',  ( 30.00000000000000000, 450.0000000000002274, 13.20242257375370976 ) ) ;
#34827 = DIRECTION ( 'NONE',  ( 0.000000000000000000, 0.9751326242170613723, -0.2216221225138578221 ) ) ;
#34828 = DIRECTION ( 'NONE',  ( -1.000000000000000000, -1.224606353822377258E-16, -0.000000000000000000 ) ) ;
#34829 = EDGE_LOOP ( 'NONE', ( #15867, #11466, #23831, #42213, #41877 ) ) ;
#34830 = DIRECTION ( 'NONE',  ( 1.776356839400250465E-15, 0.000000000000000000, 1.000000000000000000 ) ) ;
#34831 = CARTESIAN_POINT ( 'NONE',  ( 48.10000000000000142, 0.000000000000000000, 0.000000000000000000 ) ) ;
#34832 = CARTESIAN_POINT ( 'NONE',  ( 0.3592208079800993104, 13.57940237358916669, 49.30120215405869999 ) ) ;
#34833 = CARTESIAN_POINT ( 'NONE',  ( -87.74742208423795375, -30.00000000000000355, 186.1250627137971492 ) ) ;
#34834 = VERTEX_POINT ( 'NONE', #42499 ) ;
#34835 = CARTESIAN_POINT ( 'NONE',  ( 38.81137242944067367, 25.17601004987945501, -12.34914416957476568 ) ) ;
#34836 = CARTESIAN_POINT ( 'NONE',  ( 71.48264316122191531, -57.67967896547522599, 166.8593090913044819 ) ) ;
#34837 = CARTESIAN_POINT ( 'NONE',  ( 0.000000000000000000, 27.68727484027578356, 33.82893434829263413 ) ) ;
#34838 = CARTESIAN_POINT ( 'NONE',  ( 37.38852656643516070, -32.12008312474581118, -37.68358437264794958 ) ) ;
#34839 = DIRECTION ( 'NONE',  ( 0.8139476909583217568, 0.000000000000000000, 0.5809381691571112727 ) ) ;
#34840 = DIRECTION ( 'NONE',  ( 0.000000000000000000, 0.000000000000000000, 1.000000000000000000 ) ) ;
#34841 = CARTESIAN_POINT ( 'NONE',  ( -41.36542036488555851, -59.99999999999999289, 54.13965941178337005 ) ) ;
#34842 = CARTESIAN_POINT ( 'NONE',  ( -31.00196442608961789, 438.8341882283345967, 22.04045832193504850 ) ) ;
#34843 = CARTESIAN_POINT ( 'NONE',  ( -39.04923757935653583, 48.00000000000000000, 52.30342408741262972 ) ) ;
#34844 = CARTESIAN_POINT ( 'NONE',  ( -86.61008243043399091, -20.70827441317174333, 184.3512822565784575 ) ) ;
#34845 = AXIS2_PLACEMENT_3D ( 'NONE', #41145, #55701, #14722 ) ;
#34846 = ORIENTED_EDGE ( 'NONE', *, *, #51035, .F. ) ;
#34847 = FACE_OUTER_BOUND ( 'NONE', #38382, .T. ) ;
#34848 = CARTESIAN_POINT ( 'NONE',  ( -3.091320174682205657, -60.36579976115420720, 33.94522616076510246 ) ) ;
#34849 = CARTESIAN_POINT ( 'NONE',  ( -6.731699483773395443, 41.74873219887699349, -59.11937119210400482 ) ) ;
#34850 = VECTOR ( 'NONE', #20108, 1000.000000000000000 ) ;
#34851 = CARTESIAN_POINT ( 'NONE',  ( -42.57401446191834538, 489.2306033394490896, 6.899174279275240629 ) ) ;
#34853 = CARTESIAN_POINT ( 'NONE',  ( 2.437998975427489778, -69.36002461153142917, 12.93669399823944133 ) ) ;
#34852 = CARTESIAN_POINT ( 'NONE',  ( -21.58423181737243368, 294.9402007847133973, 1.955789080085255982 ) ) ;
#34854 = ORIENTED_EDGE ( 'NONE', *, *, #81656, .F. ) ;
#34855 = CARTESIAN_POINT ( 'NONE',  ( -34.97110905785431356, 329.4978619204799770, -3.714909018897103454 ) ) ;
#34856 = CARTESIAN_POINT ( 'NONE',  ( 0.1685692406266287302, 27.29958877905243142, 40.74143671976548120 ) ) ;
#34857 = CYLINDRICAL_SURFACE ( 'NONE', #56844, 6.999999999999993783 ) ;
#34858 = COLOUR_RGB ( '', 0.08235294, 0.09019608, 0.10196078) ;
#34859 = CARTESIAN_POINT ( 'NONE',  ( 22.52750012656957423, 295.0402877133163315, -9.959936289882007188 ) ) ;
#34860 = CARTESIAN_POINT ( 'NONE',  ( 33.56345473223404241, 299.9083031499212666, -8.874823776836098688 ) ) ;
#34861 = CARTESIAN_POINT ( 'NONE',  ( 4.898587196589412829E-16, 3.500000000000000000, 4.000000000000000000 ) ) ;
#34862 = DIRECTION ( 'NONE',  ( 0.000000000000000000, 0.000000000000000000, 1.000000000000000000 ) ) ;
#34863 = CARTESIAN_POINT ( 'NONE',  ( 105.8603286302927984, -14.21045842199436571, 153.6005582235227678 ) ) ;
#34864 = CARTESIAN_POINT ( 'NONE',  ( -79.31517829596272406, -53.37869160261720936, 157.6496308188775117 ) ) ;
#34865 = ORIENTED_EDGE ( 'NONE', *, *, #94074, .F. ) ;
#34866 = CARTESIAN_POINT ( 'NONE',  ( -1.647285698089624884, -3.000000000000002665, -70.00000000000000000 ) ) ;
#34867 = CARTESIAN_POINT ( 'NONE',  ( 4.472135954999576057, 250.2741185099831682, -4.000000000000002665 ) ) ;
#34868 = CARTESIAN_POINT ( 'NONE',  ( 0.000000000000000000, -50.00000000000000000, 27.00000000000000000 ) ) ;
#34869 = LINE ( 'NONE', #27858, #56255 ) ;
#34870 = CARTESIAN_POINT ( 'NONE',  ( 3.996126808948458731, 15.12551640256268826, -4.999999999999999112 ) ) ;
#34871 = CARTESIAN_POINT ( 'NONE',  ( 7.500000000000003553, -3.000000000000000888, -36.97043916959993481 ) ) ;
#34872 = ORIENTED_EDGE ( 'NONE', *, *, #106185, .T. ) ;
#34873 = DIRECTION ( 'NONE',  ( -1.000000000000000000, -0.000000000000000000, -0.000000000000000000 ) ) ;
#34874 = ORIENTED_EDGE ( 'NONE', *, *, #61300, .T. ) ;
#34875 = SURFACE_SIDE_STYLE ('',( #18690 ) ) ;
#34876 = DIRECTION ( 'NONE',  ( -0.8660254037844381525, -0.5000000000000008882, 0.000000000000000000 ) ) ;
#34877 = DIRECTION ( 'NONE',  ( 0.000000000000000000, 1.000000000000000000, 0.000000000000000000 ) ) ;
#34878 = ADVANCED_FACE ( 'NONE', ( #74849 ), #2031, .T. ) ;
#34879 = CARTESIAN_POINT ( 'NONE',  ( -62.59524157945776324, 49.99999999999999289, 18.50207713769457030 ) ) ;
#34880 = CARTESIAN_POINT ( 'NONE',  ( 4.999999999999960032, -13.68989806552482946, 13.02619096221374129 ) ) ;
#34881 = EDGE_CURVE ( 'NONE', #41735, #70272, #68932, .T. ) ;
#34882 = CARTESIAN_POINT ( 'NONE',  ( 31.84999999999999787, 1.533819458162526451E-15, 0.000000000000000000 ) ) ;
#34883 = ORIENTED_EDGE ( 'NONE', *, *, #1562, .F. ) ;
#34884 = CARTESIAN_POINT ( 'NONE',  ( 108.5319597222283079, -60.00000000000001421, 194.6846619470310316 ) ) ;
#34885 = AXIS2_PLACEMENT_3D ( 'NONE', #33561, #83154, #48642 ) ;
#34887 = CARTESIAN_POINT ( 'NONE',  ( 25.60135656087680545, -60.34811172916996469, 35.42567114881672552 ) ) ;
#34886 = CARTESIAN_POINT ( 'NONE',  ( -88.91591484687975822, -30.00000000000007105, 199.0554621605764680 ) ) ;
#34888 = DIRECTION ( 'NONE',  ( 0.000000000000000000, -1.000000000000000000, 0.000000000000000000 ) ) ;
#34889 = CARTESIAN_POINT ( 'NONE',  ( 37.69154037552305425, 413.5868078396032388, 6.418144976575544725 ) ) ;
#34890 = EDGE_CURVE ( 'NONE', #21929, #99989, #8623, .T. ) ;
#34891 = CARTESIAN_POINT ( 'NONE',  ( -40.77353850287842363, -29.15401300376588267, 36.95902376227557085 ) ) ;
#34892 = TOROIDAL_SURFACE ( 'NONE', #22790, 8.000000000000007105, 1.000000000000000888 ) ;
#34893 = DIRECTION ( 'NONE',  ( 0.000000000000000000, 0.000000000000000000, 1.000000000000000000 ) ) ;
#34894 = UNCERTAINTY_MEASURE_WITH_UNIT (LENGTH_MEASURE( 1.000000000000000082E-05 ), #91410, 'distance_accuracy_value', 'NONE');
#34895 = ORIENTED_EDGE ( 'NONE', *, *, #84976, .F. ) ;
#34896 = CARTESIAN_POINT ( 'NONE',  ( 36.08349330513379982, 4.000000000000002665, 0.000000000000000000 ) ) ;
#34897 = CARTESIAN_POINT ( 'NONE',  ( -43.79329400983250764, 434.3557490607461773, 12.18619556048586006 ) ) ;
#34898 = CARTESIAN_POINT ( 'NONE',  ( -8.000000000000000000, 0.000000000000000000, -12.97459999999999525 ) ) ;
#34899 = FACE_OUTER_BOUND ( 'NONE', #40220, .T. ) ;
#34900 = CARTESIAN_POINT ( 'NONE',  ( 6.333820801330125150, 4.275724398227219503, 5.594228103108966010 ) ) ;
#34901 = CARTESIAN_POINT ( 'NONE',  ( -30.00000000000000355, 489.3008774416998108, 5.491695563541885150 ) ) ;
#34902 = ORIENTED_EDGE ( 'NONE', *, *, #50054, .T. ) ;
#34903 = CARTESIAN_POINT ( 'NONE',  ( -5.833333333333328596, -4.000000000000003553, 103.8776713793258608 ) ) ;
#34904 = ORIENTED_EDGE ( 'NONE', *, *, #33140, .T. ) ;
#34905 = CARTESIAN_POINT ( 'NONE',  ( 81.49538808793018063, -30.00000000000000000, 29.79622834626826489 ) ) ;
#34906 = CARTESIAN_POINT ( 'NONE',  ( 23.97434870411618846, 41.62134556306904898, -74.34079015579241911 ) ) ;
#34908 = EDGE_CURVE ( 'NONE', #21459, #444, #67325, .T. ) ;
#34907 = DIRECTION ( 'NONE',  ( 0.000000000000000000, -1.000000000000000000, 0.000000000000000000 ) ) ;
#34909 = DIRECTION ( 'NONE',  ( 0.000000000000000000, 0.000000000000000000, -1.000000000000000000 ) ) ;
#34910 = CARTESIAN_POINT ( 'NONE',  ( 85.92470906003214282, -30.00000000000000355, 63.76399589821353686 ) ) ;
#34911 = CARTESIAN_POINT ( 'NONE',  ( -26.51187371842186025, 308.1715024495429134, 10.94285474946573622 ) ) ;
#34912 = ORIENTED_EDGE ( 'NONE', *, *, #9827, .F. ) ;
#34913 = VERTEX_POINT ( 'NONE', #10650 ) ;
#34914 = EDGE_LOOP ( 'NONE', ( #21744, #61358, #41206, #47811, #52433 ) ) ;
#34915 = CARTESIAN_POINT ( 'NONE',  ( -46.96405579082744453, 13.62080378033662420, -14.94667195310861985 ) ) ;
#34916 = CARTESIAN_POINT ( 'NONE',  ( 65.03872891708842019, 4.000000000000015099, 4.898587196589422689E-16 ) ) ;
#34917 = DIRECTION ( 'NONE',  ( -1.000000000000000000, -0.000000000000000000, -0.000000000000000000 ) ) ;
#34918 = CARTESIAN_POINT ( 'NONE',  ( 37.03121509147988633, 439.7235855775043660, 24.13066540521764836 ) ) ;
#34919 = CARTESIAN_POINT ( 'NONE',  ( -31.43460449399193024, 410.2305464698810624, 24.47796294967516317 ) ) ;
#34920 = EDGE_LOOP ( 'NONE', ( #65377, #78131 ) ) ;
#34921 = CARTESIAN_POINT ( 'NONE',  ( 1.469576158976823356E-15, 50.00000000000000000, -73.00000000000001421 ) ) ;
#34922 = ORIENTED_EDGE ( 'NONE', *, *, #104303, .F. ) ;
#34923 = DIRECTION ( 'NONE',  ( 0.000000000000000000, -1.000000000000000000, 0.000000000000000000 ) ) ;
#34924 = CARTESIAN_POINT ( 'NONE',  ( 75.45573842239058138, -38.35112759154727513, 173.8072745080378070 ) ) ;
#34925 = DIRECTION ( 'NONE',  ( -1.000000000000000000, -0.000000000000000000, -0.000000000000000000 ) ) ;
#34926 = CARTESIAN_POINT ( 'NONE',  ( 32.49403296435929889, 299.9991840122719964, 3.091681079173501434 ) ) ;
#34927 = CIRCLE ( 'NONE', #29762, 3.000000000000009326 ) ;
#34928 = CARTESIAN_POINT ( 'NONE',  ( -5.650483388624516934, 246.5443340314961063, 2.031129859422147632 ) ) ;
#34929 = AXIS2_PLACEMENT_3D ( 'NONE', #40348, #80800, #30158 ) ;
#34930 = EDGE_LOOP ( 'NONE', ( #24918, #36639 ) ) ;
#34931 = CARTESIAN_POINT ( 'NONE',  ( 17.40646473312635578, 45.37698912868005863, -6.411815653116820002 ) ) ;
#34932 = CARTESIAN_POINT ( 'NONE',  ( 39.34669569945254608, 315.1114205638089629, 6.831757979675468384 ) ) ;
#34933 = CARTESIAN_POINT ( 'NONE',  ( 6.849999999999999645, -9.237604307034018802, 3.355146209984123968E-17 ) ) ;
#34934 = ADVANCED_FACE ( 'NONE', ( #403 ), #72366, .T. ) ;
#34935 = CARTESIAN_POINT ( 'NONE',  ( 14.84861631010743999, 2.245468665773563632, -2.074511027864127222 ) ) ;
#34936 = EDGE_LOOP ( 'NONE', ( #89404, #10581, #83410, #61336 ) ) ;
#34937 = PRESENTATION_STYLE_ASSIGNMENT (( #26858 ) ) ;
#34938 = DIRECTION ( 'NONE',  ( 0.000000000000000000, -1.000000000000000000, 0.000000000000000000 ) ) ;
#34939 = CARTESIAN_POINT ( 'NONE',  ( 20.00000000000000000, 12.99999999999999289, 0.000000000000000000 ) ) ;
#34940 = CARTESIAN_POINT ( 'NONE',  ( -1.013163106017260562, -8.075304045852337964, -7.231838333420566478 ) ) ;
#34941 = CARTESIAN_POINT ( 'NONE',  ( 6.426095497085385411, 294.7471186225963606, 9.914748094734409989 ) ) ;
#34942 = EDGE_CURVE ( 'NONE', #39671, #30449, #12085, .T. ) ;
#34943 = FACE_OUTER_BOUND ( 'NONE', #94842, .T. ) ;
#34944 = DIRECTION ( 'NONE',  ( -1.000000000000000000, -0.000000000000000000, -0.000000000000000000 ) ) ;
#34945 = CARTESIAN_POINT ( 'NONE',  ( 86.39650202725968597, -17.44888770226837948, 178.9044480368839629 ) ) ;
#34946 = DIRECTION ( 'NONE',  ( 0.000000000000000000, 0.000000000000000000, 1.000000000000000000 ) ) ;
#34947 = CARTESIAN_POINT ( 'NONE',  ( -8.203754751779342769, 114.5734753959361711, -1.270355564599584843E-12 ) ) ;
#34948 = ORIENTED_EDGE ( 'NONE', *, *, #63395, .T. ) ;
#34949 = CARTESIAN_POINT ( 'NONE',  ( 16.75187969033515145, -1.200000000000000030E-05, -24.30698433968624883 ) ) ;
#34950 = CARTESIAN_POINT ( 'NONE',  ( 9.609486011791426918, 143.0915023496523020, 0.000000000000000000 ) ) ;
#34951 = DIRECTION ( 'NONE',  ( 0.000000000000000000, -1.000000000000000000, 0.000000000000000000 ) ) ;
#34952 = DIRECTION ( 'NONE',  ( -1.000000000000000000, -1.224606353822377258E-16, -0.000000000000000000 ) ) ;
#34953 = EDGE_CURVE ( 'NONE', #93240, #82573, #25291, .T. ) ;
#34954 = STYLED_ITEM ( 'NONE', ( #36429 ), #96260 ) ;
#34955 = CARTESIAN_POINT ( 'NONE',  ( -83.17859549212624870, -30.00000000000000000, 44.33109224352784850 ) ) ;
#34956 = EDGE_CURVE ( 'NONE', #17636, #47279, #2187, .T. ) ;
#34957 = CIRCLE ( 'NONE', #2179, 1.000000000000001110 ) ;
#34958 = CARTESIAN_POINT ( 'NONE',  ( -17.49999999999997513, 50.00000000000000000, 63.82142195434425958 ) ) ;
#34959 = CARTESIAN_POINT ( 'NONE',  ( -6.928203230275508773, -10.00000000000000711, -4.000000000000000000 ) ) ;
#34960 = CARTESIAN_POINT ( 'NONE',  ( 13.37207953394533355, 1.482358050883964840E-15, 0.000000000000000000 ) ) ;
#34962 = CARTESIAN_POINT ( 'NONE',  ( 0.7145311798161616545, -4.618802153517262532, -8.000000000000001776 ) ) ;
#34961 = CARTESIAN_POINT ( 'NONE',  ( -9.176855344543007220, 249.4703957302258459, -3.973472207155925862 ) ) ;
#34963 =( BOUNDED_CURVE ( )  B_SPLINE_CURVE ( 1, ( #81071, #1053 ),
 .UNSPECIFIED., .F., .F. ) 
 B_SPLINE_CURVE_WITH_KNOTS ( ( 2, 2 ),
 ( 0.000000000000000000, 1.000000000000000000 ),
 .UNSPECIFIED. ) 
 CURVE ( )  GEOMETRIC_REPRESENTATION_ITEM ( )  RATIONAL_B_SPLINE_CURVE ( ( 0.9660720326926630630, 0.9660720326926630630 ) ) 
 REPRESENTATION_ITEM ( '' )  );
#34964 = EDGE_CURVE ( 'NONE', #93530, #68880, #99075, .T. ) ;
#34965 =( NAMED_UNIT ( * ) PLANE_ANGLE_UNIT ( ) SI_UNIT ( $, .RADIAN. ) );
#34966 = DIRECTION ( 'NONE',  ( -1.000000000000000000, 0.000000000000000000, -0.000000000000000000 ) ) ;
#34967 = FACE_OUTER_BOUND ( 'NONE', #98019, .T. ) ;
#34968 = PLANE ( 'NONE',  #85678 ) ;
#34969 = CARTESIAN_POINT ( 'NONE',  ( 17.50000000000000711, -2.499999999999999556, 25.00000000000000000 ) ) ;
#34970 = EDGE_CURVE ( 'NONE', #84082, #79044, #10132, .T. ) ;
#34971 = CARTESIAN_POINT ( 'NONE',  ( 48.18193197797202032, -27.07217853350000780, -28.43546366937567882 ) ) ;
#34972 = CARTESIAN_POINT ( 'NONE',  ( -26.71263552688614240, -39.48221859129683509, 32.14868509336800173 ) ) ;
#34973 = VERTEX_POINT ( 'NONE', #94798 ) ;
#34974 = CARTESIAN_POINT ( 'NONE',  ( 26.08349330513380337, 4.898587196589405926E-16, -4.000000000000001776 ) ) ;
#34975 = CARTESIAN_POINT ( 'NONE',  ( -9.333079356992097786, 106.7783308007486909, 3.592383266237785922 ) ) ;
#34976 = CARTESIAN_POINT ( 'NONE',  ( -19.48547116245557476, -60.36370404294115843, 34.43491227761722939 ) ) ;
#34977 = CARTESIAN_POINT ( 'NONE',  ( -67.88365031951838091, -29.91622526688993844, -21.77912222725431235 ) ) ;
#34979 = CARTESIAN_POINT ( 'NONE',  ( -72.65287874387934153, -47.40885675805417065, -22.95091789652445158 ) ) ;
#34978 = CARTESIAN_POINT ( 'NONE',  ( -0.5691298260866446412, 27.34388701663959509, 40.61608021419867498 ) ) ;
#34980 = ORIENTED_EDGE ( 'NONE', *, *, #77900, .T. ) ;
#34981 = CARTESIAN_POINT ( 'NONE',  ( 5.000000000000000888, 6.123233995736767268E-16, 5.000000000000000000 ) ) ;
#34982 = VERTEX_POINT ( 'NONE', #36584 ) ;
#34983 = FILL_AREA_STYLE_COLOUR ( '', #71797 ) ;
#34984 = CARTESIAN_POINT ( 'NONE',  ( 0.5805565836007605673, 3.752776749732565253, 6.499999999999997335 ) ) ;
#34985 = ORIENTED_EDGE ( 'NONE', *, *, #48029, .T. ) ;
#34986 = SURFACE_STYLE_FILL_AREA ( #91611 ) ;
#34987 = CARTESIAN_POINT ( 'NONE',  ( 15.12883458092736788, 3.606451457941568517, 4.265946247307269346 ) ) ;
#34988 = CARTESIAN_POINT ( 'NONE',  ( 100.4734033239317057, -45.27744650063931431, 192.0868348784580348 ) ) ;
#34989 = AXIS2_PLACEMENT_3D ( 'NONE', #6435, #8032, #32349 ) ;
#34991 = CARTESIAN_POINT ( 'NONE',  ( -4.284822031654928587, -1.092833614412262122, 104.4267991316945370 ) ) ;
#34990 = CARTESIAN_POINT ( 'NONE',  ( -46.00000000000000000, 488.9831568219305495, 4.757012338623842318 ) ) ;
#34992 = ORIENTED_EDGE ( 'NONE', *, *, #22623, .T. ) ;
#34993 = CIRCLE ( 'NONE', #103789, 9.999999999999998224 ) ;
#34994 = ORIENTED_EDGE ( 'NONE', *, *, #98299, .F. ) ;
#34995 = AXIS2_PLACEMENT_3D ( 'NONE', #59098, #76320, #20278 ) ;
#34996 = EDGE_LOOP ( 'NONE', ( #4956, #37827, #82297, #42372, #46924 ) ) ;
#34997 = CARTESIAN_POINT ( 'NONE',  ( 26.22660380935851521, 309.5493840096061149, 10.04179730271015103 ) ) ;
#34998 = DIRECTION ( 'NONE',  ( -1.000000000000000000, -0.000000000000000000, -0.000000000000000000 ) ) ;
#34999 = CARTESIAN_POINT ( 'NONE',  ( 9.500000000000001776, -5.000000000000000000, -36.97043916959993481 ) ) ;
#35000 = ORIENTED_EDGE ( 'NONE', *, *, #52969, .T. ) ;
#35001 = EDGE_CURVE ( 'NONE', #7582, #48477, #20231, .T. ) ;
#35002 = DIRECTION ( 'NONE',  ( -1.000000000000000000, -0.000000000000000000, -0.000000000000000000 ) ) ;
#35003 = CARTESIAN_POINT ( 'NONE',  ( 6.289572920342626716, 5.584521518880458224, 3.985288806461539046 ) ) ;
#35004 = DIRECTION ( 'NONE',  ( -1.000000000000000000, -0.000000000000000000, -0.000000000000000000 ) ) ;
#35005 = CARTESIAN_POINT ( 'NONE',  ( -69.72050231116651275, -57.68271840123205862, 152.1212729744891590 ) ) ;
#35006 = CARTESIAN_POINT ( 'NONE',  ( 7.002990960197236880, -66.05266818383458371, 3.868040364119525343 ) ) ;
#35007 = DIRECTION ( 'NONE',  ( 0.000000000000000000, -1.000000000000000000, 0.000000000000000000 ) ) ;
#35008 = DIRECTION ( 'NONE',  ( 0.000000000000000000, -1.000000000000000000, 0.000000000000000000 ) ) ;
#35009 = COLOUR_RGB ( '', 0.08235294, 0.09019608, 0.10196078) ;
#35010 = CARTESIAN_POINT ( 'NONE',  ( -95.18184656059791848, -59.99999999999997158, -7.511930356246473650 ) ) ;
#35011 = EDGE_CURVE ( 'NONE', #106068, #67879, #25356, .T. ) ;
#35012 = EDGE_CURVE ( 'NONE', #59308, #69676, #29550, .T. ) ;
#35013 = CARTESIAN_POINT ( 'NONE',  ( -49.14104052736104933, -49.90578126524030722, 52.73558596523304232 ) ) ;
#35014 = EDGE_LOOP ( 'NONE', ( #95081, #28793, #64201 ) ) ;
#35015 = LINE ( 'NONE', #67880, #91795 ) ;
#35016 = ORIENTED_EDGE ( 'NONE', *, *, #59568, .F. ) ;
#35017 = CARTESIAN_POINT ( 'NONE',  ( 12.50000000000000000, -2.171334581115599516, -15.32410535964003095 ) ) ;
#35018 = EDGE_CURVE ( 'NONE', #33011, #53678, #20417, .T. ) ;
#35019 = CARTESIAN_POINT ( 'NONE',  ( -4.240736524251620843, 300.6921934601531348, -10.01075408398145861 ) ) ;
#35020 = EDGE_CURVE ( 'NONE', #102954, #94099, #45182, .T. ) ;
#35021 = CARTESIAN_POINT ( 'NONE',  ( 9.784980416533748837, -3.383375863471970391, 15.02393414357561596 ) ) ;
#35022 = ORIENTED_EDGE ( 'NONE', *, *, #88752, .T. ) ;
#35023 = CARTESIAN_POINT ( 'NONE',  ( 74.64902420247312875, -38.33065913207683906, 166.1686744667666176 ) ) ;
#35024 = CARTESIAN_POINT ( 'NONE',  ( 49.18580537133217945, 13.60959006579815700, 15.12486994001107909 ) ) ;
#35025 = CARTESIAN_POINT ( 'NONE',  ( -6.536855819840425852, 51.40560724102103052, -7.402653316414548712 ) ) ;
#35027 = ADVANCED_FACE ( 'NONE', ( #86707 ), #105925, .T. ) ;
#35026 = DIRECTION ( 'NONE',  ( -1.000000000000000000, -0.000000000000000000, -0.000000000000000000 ) ) ;
#35028 = EDGE_CURVE ( 'NONE', #15128, #36676, #54918, .T. ) ;
#35029 = CARTESIAN_POINT ( 'NONE',  ( 45.60838156032635027, 42.00000000000000000, 79.13121736029046360 ) ) ;
#35030 = CARTESIAN_POINT ( 'NONE',  ( 91.95784082022851180, -29.99999999999999289, 190.8526501999825200 ) ) ;
#35031 = VECTOR ( 'NONE', #41950, 1000.000000000000227 ) ;
#35032 = CARTESIAN_POINT ( 'NONE',  ( 0.3381990287830299868, 46.20001774662581084, -16.28516304919335411 ) ) ;
#35033 = DIRECTION ( 'NONE',  ( 1.000000000000000000, 0.000000000000000000, 0.000000000000000000 ) ) ;
#35034 = ORIENTED_EDGE ( 'NONE', *, *, #1876, .T. ) ;
#35035 = ORIENTED_EDGE ( 'NONE', *, *, #4281, .F. ) ;
#35036 = CARTESIAN_POINT ( 'NONE',  ( 51.66197549029767799, -46.43860231094777902, 56.12756693511081352 ) ) ;
#35037 = CIRCLE ( 'NONE', #9180, 3.309500000000001663 ) ;
#35038 = CARTESIAN_POINT ( 'NONE',  ( 6.744833588908348609, 41.44195294531055396, -58.57194835312484571 ) ) ;
#35039 = CARTESIAN_POINT ( 'NONE',  ( -1.469576158976823947E-15, -15.87499999999999289, 8.000000000000000000 ) ) ;
#35040 = ORIENTED_EDGE ( 'NONE', *, *, #14085, .T. ) ;
#35041 = CARTESIAN_POINT ( 'NONE',  ( -90.49795102847224371, -38.40269404522611296, -14.57212712810775201 ) ) ;
#35042 = VERTEX_POINT ( 'NONE', #95843 ) ;
#35043 = CARTESIAN_POINT ( 'NONE',  ( 4.898587196589412829E-16, -28.81250000409677270, -8.000000000000000000 ) ) ;
#35044 = CARTESIAN_POINT ( 'NONE',  ( 106.9166147825914663, -38.36521485666400366, 194.9876764072000697 ) ) ;
#35045 = CARTESIAN_POINT ( 'NONE',  ( 14.81649318718688235, 22.00128301469023384, 4.391045811938269594 ) ) ;
#35046 = CARTESIAN_POINT ( 'NONE',  ( 91.05926484896966144, -45.28280038615342562, 77.50342918606192200 ) ) ;
#35047 = CARTESIAN_POINT ( 'NONE',  ( -0.3377172304431446115, 45.31573710349624662, -18.71511598565236056 ) ) ;
#35048 = CARTESIAN_POINT ( 'NONE',  ( -6.145467199749147014, -3.000000000000003109, -77.00333157601822620 ) ) ;
#35049 = FILL_AREA_STYLE_COLOUR ( '', #5721 ) ;
#35050 = CARTESIAN_POINT ( 'NONE',  ( -23.30007435341033073, 25.23546008595426215, -33.20617127781038391 ) ) ;
#35051 = CARTESIAN_POINT ( 'NONE',  ( 0.000000000000000000, 0.000000000000000000, 4.000000000000000000 ) ) ;
#35052 = CARTESIAN_POINT ( 'NONE',  ( 3.168333439191699075, 112.8173450435234315, 5.000000000000000000 ) ) ;
#35053 = VERTEX_POINT ( 'NONE', #13838 ) ;
#35054 = CARTESIAN_POINT ( 'NONE',  ( 3.337161262018383995E-15, 37.21016666119768246, 27.25000000000000000 ) ) ;
#35055 = CARTESIAN_POINT ( 'NONE',  ( 0.000000000000000000, 0.000000000000000000, 0.000000000000000000 ) ) ;
#35056 = VERTEX_POINT ( 'NONE', #64538 ) ;
#35057 = CARTESIAN_POINT ( 'NONE',  ( -35.58611802053648177, 485.2911282079576267, -2.949779747020754517 ) ) ;
#35058 = CARTESIAN_POINT ( 'NONE',  ( -40.74344824707514334, 359.9914281314131017, 24.28752742797811237 ) ) ;
#35059 = DIRECTION ( 'NONE',  ( 0.000000000000000000, 1.000000000000000000, 0.000000000000000000 ) ) ;
#35060 = CARTESIAN_POINT ( 'NONE',  ( 3.313708498984800688, -23.28125000000000000, 7.999999999999960032 ) ) ;
#35061 = CARTESIAN_POINT ( 'NONE',  ( 8.000000000000000000, -24.49999999999999289, 0.000000000000000000 ) ) ;
#35062 = CARTESIAN_POINT ( 'NONE',  ( 44.21857466350731869, -28.02261279241452385, 39.26658464693652917 ) ) ;
#35063 = EDGE_CURVE ( 'NONE', #34125, #97567, #100770, .T. ) ;
#35064 = DIRECTION ( 'NONE',  ( 0.000000000000000000, -1.000000000000000000, 0.000000000000000000 ) ) ;
#35065 = VECTOR ( 'NONE', #45296, 1000.000000000000341 ) ;
#35066 = ORIENTED_EDGE ( 'NONE', *, *, #75972, .T. ) ;
#35067 = CARTESIAN_POINT ( 'NONE',  ( 82.00125028607160971, -60.71606377786684305, 187.9277208723676154 ) ) ;
#35068 =( LENGTH_UNIT ( ) NAMED_UNIT ( * ) SI_UNIT ( .MILLI., .METRE. ) );
#35069 = B_SPLINE_CURVE_WITH_KNOTS ( 'NONE', 3,
 ( #99990, #41224, #25070, #26159, #74111, #50366, #198, #18031 ),
 .UNSPECIFIED., .F., .F.,
 ( 4, 2, 2, 4 ),
 ( 0.01336725833835631684, 0.01453745203451946473, 0.01570764573068261435, 0.01804803312300891013 ),
 .UNSPECIFIED. ) ;
#35070 = FILL_AREA_STYLE_COLOUR ( '', #102045 ) ;
#35071 = ORIENTED_EDGE ( 'NONE', *, *, #65428, .T. ) ;
#35072 = DIRECTION ( 'NONE',  ( 0.000000000000000000, 0.000000000000000000, -1.000000000000000000 ) ) ;
#35073 = DIRECTION ( 'NONE',  ( -1.000000000000000000, -0.000000000000000000, -0.000000000000000000 ) ) ;
#35074 = PLANE ( 'NONE',  #42068 ) ;
#35075 = CARTESIAN_POINT ( 'NONE',  ( 14.61924042696503712, -3.000000000000002665, -89.34162378225711620 ) ) ;
#35076 = CARTESIAN_POINT ( 'NONE',  ( 97.15356149169568312, 5.000000000000042633, 6.123233995736805725E-16 ) ) ;
#35077 = CARTESIAN_POINT ( 'NONE',  ( -42.67177486380370510, -33.72132305402984542, -37.16294406443787324 ) ) ;
#35078 = AXIS2_PLACEMENT_3D ( 'NONE', #94690, #12141, #52597 ) ;
#35079 = EDGE_CURVE ( 'NONE', #74552, #52930, #50791, .T. ) ;
#35080 = CARTESIAN_POINT ( 'NONE',  ( 43.30523961208659500, -60.00000000000001421, 57.40393935450531160 ) ) ;
#35081 = PRESENTATION_LAYER_ASSIGNMENT (  '', '', ( #38538 ) ) ;
#35082 = CARTESIAN_POINT ( 'NONE',  ( 27.14852178964998686, -30.51280503760606777, 39.13343489206324932 ) ) ;
#35083 = DIRECTION ( 'NONE',  ( -1.000000000000000000, -1.224606353822377258E-16, -0.000000000000000000 ) ) ;
#35085 = CARTESIAN_POINT ( 'NONE',  ( -13.26885379642688889, 24.19022360890687651, -3.253372505828892702 ) ) ;
#35084 = CARTESIAN_POINT ( 'NONE',  ( -32.35805919302102041, -33.97132168949374886, 42.09303864586733113 ) ) ;
#35086 = CARTESIAN_POINT ( 'NONE',  ( 8.890893604443357745, 294.6744728344714304, -4.583208782230876466 ) ) ;
#35087 = CARTESIAN_POINT ( 'NONE',  ( 30.55228927099183522, 298.7536840786443690, 10.80461237140096209 ) ) ;
#35088 = FILL_AREA_STYLE_COLOUR ( '', #40521 ) ;
#35089 = CYLINDRICAL_SURFACE ( 'NONE', #25971, 1.250000000000001110 ) ;
#35090 = ORIENTED_EDGE ( 'NONE', *, *, #43431, .T. ) ;
#35091 = ADVANCED_FACE ( 'NONE', ( #55867 ), #66357, .F. ) ;
#35092 = CARTESIAN_POINT ( 'NONE',  ( 30.00000000000000000, 500.0000000000002274, 12.00000000000000888 ) ) ;
#35093 = CARTESIAN_POINT ( 'NONE',  ( -17.49999999999998579, 51.12013589170755523, 63.06608111886978207 ) ) ;
#35094 = AXIS2_PLACEMENT_3D ( 'NONE', #70990, #29514, #38134 ) ;
#35095 = CARTESIAN_POINT ( 'NONE',  ( -9.301034387593361430, -2.623043302277163313, 14.76518561301066867 ) ) ;
#35096 = CARTESIAN_POINT ( 'NONE',  ( -39.21851180500383549, 464.6178194517503357, 18.47749881120159898 ) ) ;
#35097 =( BOUNDED_SURFACE ( )  B_SPLINE_SURFACE ( 3, 2, ( 
 ( #76311, #19202, #20804 ),
 ( #11039, #44500, #52038 ),
 ( #102729, #52567, #53117 ),
 ( #76847, #93580, #2424 ) ),
 .UNSPECIFIED., .F., .F., .F. ) 
 B_SPLINE_SURFACE_WITH_KNOTS ( ( 4, 4 ),
 ( 3, 3 ),
 ( 0.01611645847898209721, 0.01831749139115259814 ),
 ( 0.1613811371914657955, 1.000000000000000000 ),
 .UNSPECIFIED. ) 
 GEOMETRIC_REPRESENTATION_ITEM ( )  RATIONAL_B_SPLINE_SURFACE ( (
 ( 0.9207212652179901369, 0.7543742219143241279, 1.000000000000000000),
 ( 0.9269995412618095010, 0.7738259253571211360, 1.000000000000000000),
 ( 0.9331146633523605960, 0.7927721361627118046, 1.000000000000000000),
 ( 0.9388524989238742346, 0.8105494169260341053, 1.000000000000000000) ) ) 
 REPRESENTATION_ITEM ( '' )  SURFACE ( )  );
#35098 = PRESENTATION_LAYER_ASSIGNMENT (  '', '', ( #7476 ) ) ;
#35100 = CARTESIAN_POINT ( 'NONE',  ( 50.82574175334806910, -47.40887837029733021, -29.75606519997849730 ) ) ;
#35099 = SURFACE_SIDE_STYLE ('',( #84152 ) ) ;
#35101 = COLOUR_RGB ( '', 0.08235294, 0.09019608, 0.10196078) ;
#35102 = VERTEX_POINT ( 'NONE', #71025 ) ;
#35103 = AXIS2_PLACEMENT_3D ( 'NONE', #56383, #89316, #41281 ) ;
#35104 = CARTESIAN_POINT ( 'NONE',  ( 9.928454760406586033, 294.6449062848762992, 1.239352149953448334 ) ) ;
#35105 = AXIS2_PLACEMENT_3D ( 'NONE', #51741, #69542, #85740 ) ;
#35106 = ORIENTED_EDGE ( 'NONE', *, *, #26732, .T. ) ;
#35107 = DIRECTION ( 'NONE',  ( 0.000000000000000000, 0.000000000000000000, 1.000000000000000000 ) ) ;
#35108 = CARTESIAN_POINT ( 'NONE',  ( 30.90131729786656223, 8.441056540751519677, -41.14701368050901920 ) ) ;
#35109 = CARTESIAN_POINT ( 'NONE',  ( 81.84444444444444855, 1.023464760207051730E-14, 0.000000000000000000 ) ) ;
#35110 = PRODUCT_RELATED_PRODUCT_CATEGORY ( 'part', '', ( #14592 ) ) ;
#35111 = CARTESIAN_POINT ( 'NONE',  ( -91.86600403542094284, -59.99999999999998579, 10.85315903371735757 ) ) ;
#35112 = CARTESIAN_POINT ( 'NONE',  ( -43.00000000000004263, 435.7055874969797173, 20.39059140826869765 ) ) ;
#35113 = DIRECTION ( 'NONE',  ( -0.000000000000000000, -0.000000000000000000, -1.000000000000000000 ) ) ;
#35114 = CARTESIAN_POINT ( 'NONE',  ( 34.72474116627837759, 338.3618661353910966, -1.881472242819908436 ) ) ;
#35115 = CARTESIAN_POINT ( 'NONE',  ( 39.26668904305612529, 460.2385666352532780, 2.228751329589347741 ) ) ;
#35116 = CARTESIAN_POINT ( 'NONE',  ( -5.036189802311180408, -3.000000000000002665, -93.73786388412156612 ) ) ;
#35117 = CARTESIAN_POINT ( 'NONE',  ( -83.47784681200417367, -39.47383177809769705, 174.2413187030911956 ) ) ;
#35118 = EDGE_LOOP ( 'NONE', ( #8149, #70884, #66135, #84108 ) ) ;
#35119 = DIRECTION ( 'NONE',  ( -0.000000000000000000, 1.000000000000000000, -0.000000000000000000 ) ) ;
#35120 = VERTEX_POINT ( 'NONE', #21974 ) ;
#35121 = ORIENTED_EDGE ( 'NONE', *, *, #13823, .F. ) ;
#35122 = DIRECTION ( 'NONE',  ( -0.5735764363510459374, -0.8191520442889919096, 0.000000000000000000 ) ) ;
#35123 = DIRECTION ( 'NONE',  ( -0.000000000000000000, -0.000000000000000000, -1.000000000000000000 ) ) ;
#35124 = SURFACE_STYLE_USAGE ( .BOTH. , #52327 ) ;
#35125 = ORIENTED_EDGE ( 'NONE', *, *, #44908, .F. ) ;
#35126 = AXIS2_PLACEMENT_3D ( 'NONE', #77704, #60998, #60480 ) ;
#35127 = CARTESIAN_POINT ( 'NONE',  ( 38.58349330513380693, -4.000000000000000888, 4.898587196589416773E-16 ) ) ;
#35128 = CARTESIAN_POINT ( 'NONE',  ( 0.000000000000000000, 2.999999999999992450, 0.000000000000000000 ) ) ;
#35129 = CARTESIAN_POINT ( 'NONE',  ( -7.744329845603313167, -61.53711769846545820, -2.018701143083236449 ) ) ;
#35130 = CARTESIAN_POINT ( 'NONE',  ( 43.69363714723023406, 464.9777160013941852, 8.439175988291857777 ) ) ;
#35131 = CARTESIAN_POINT ( 'NONE',  ( -5.000000000000000000, -14.03205060597777809, 9.639947695590496579 ) ) ;
#35132 = CARTESIAN_POINT ( 'NONE',  ( 97.22633417984880566, -59.99999999999997158, 47.92222960719137603 ) ) ;
#35133 = EDGE_CURVE ( 'NONE', #64798, #37996, #84558, .T. ) ;
#35134 = CARTESIAN_POINT ( 'NONE',  ( -103.2140057312332715, -60.00000000000000000, 203.2732544657875167 ) ) ;
#35135 = CARTESIAN_POINT ( 'NONE',  ( -58.23786245037103981, -53.38855727373060489, 74.09665987365666240 ) ) ;
#35136 = VERTEX_POINT ( 'NONE', #54828 ) ;
#35137 =( LENGTH_UNIT ( ) NAMED_UNIT ( * ) SI_UNIT ( .MILLI., .METRE. ) );
#35138 = VERTEX_POINT ( 'NONE', #22514 ) ;
#35139 = CARTESIAN_POINT ( 'NONE',  ( -102.5594303321801277, -52.71277882121110281, 191.0325329949383217 ) ) ;
#35140 = CARTESIAN_POINT ( 'NONE',  ( 6.162888688655344005, 3.752776749732561257, -6.499999999999999112 ) ) ;
#35141 = CARTESIAN_POINT ( 'NONE',  ( 8.000000000000000000, -18.59375000409676915, -3.313708498984761164 ) ) ;
#35142 = EDGE_LOOP ( 'NONE', ( #26431, #28192, #39181, #55380, #72343 ) ) ;
#35143 = CARTESIAN_POINT ( 'NONE',  ( 7.141975279388227626, -3.000000000000119016, -70.98863559356006192 ) ) ;
#35144 = CARTESIAN_POINT ( 'NONE',  ( -77.97286044409068495, -60.00000000000002132, 192.7800898974841175 ) ) ;
#35145 = CARTESIAN_POINT ( 'NONE',  ( 22.25669491856071858, 1.482358050883964840E-15, 0.000000000000000000 ) ) ;
#35146 = CARTESIAN_POINT ( 'NONE',  ( 4.401442555609581635E-16, -23.65625000204838457, -7.188101187500000044 ) ) ;
#35147 = DIRECTION ( 'NONE',  ( 1.000000000000000000, -0.000000000000000000, -0.000000000000000000 ) ) ;
#35149 = ADVANCED_FACE ( 'NONE', ( #62947 ), #90197, .F. ) ;
#35148 = CARTESIAN_POINT ( 'NONE',  ( 32.69883954133203474, 464.5926484747985796, 16.74362576150353021 ) ) ;
#35150 = CARTESIAN_POINT ( 'NONE',  ( 5.483261958904508404, -0.000000000000000000, -16.14668631625339046 ) ) ;
#35151 = CARTESIAN_POINT ( 'NONE',  ( -20.52350613252515643, 304.8999024697870937, 9.947223320822450532 ) ) ;
#35152 = EDGE_CURVE ( 'NONE', #85099, #38377, #11169, .T. ) ;
#35153 = CARTESIAN_POINT ( 'NONE',  ( 5.849799967470243445, -7.702454342450949731, 13.78846266272944554 ) ) ;
#35154 = CARTESIAN_POINT ( 'NONE',  ( 13.50000000000000178, 0.000000000000000000, -13.00000000000000000 ) ) ;
#35155 = CARTESIAN_POINT ( 'NONE',  ( 13.14242568359541607, 42.00000000000000000, -92.43215185542086942 ) ) ;
#35156 = UNCERTAINTY_MEASURE_WITH_UNIT (LENGTH_MEASURE( 1.000000000000000082E-05 ), #70053, 'distance_accuracy_value', 'NONE');
#35157 = CARTESIAN_POINT ( 'NONE',  ( -30.57629521487107738, -42.96300971420584602, 33.95585917984841728 ) ) ;
#35158 = FILL_AREA_STYLE_COLOUR ( '', #69693 ) ;
#35159 = UNCERTAINTY_MEASURE_WITH_UNIT (LENGTH_MEASURE( 1.000000000000000082E-05 ), #1533, 'distance_accuracy_value', 'NONE');
#35160 = CARTESIAN_POINT ( 'NONE',  ( 45.44314741231004717, -32.61510095533251530, 42.31814636275050390 ) ) ;
#35161 = CARTESIAN_POINT ( 'NONE',  ( 5.691929483231186637, 5.629165124598853431, 3.249999999999998668 ) ) ;
#35162 = CARTESIAN_POINT ( 'NONE',  ( -0.7777183698329714900, 45.39552846407493547, 18.48206553968775268 ) ) ;
#35163 = CARTESIAN_POINT ( 'NONE',  ( -90.23139260845938736, -38.51326215213924797, 200.6299674765010366 ) ) ;
#35164 = ORIENTED_EDGE ( 'NONE', *, *, #57378, .F. ) ;
#35166 = CARTESIAN_POINT ( 'NONE',  ( -43.71217423904473520, 435.6632154632216043, 9.092528312227512899 ) ) ;
#35165 = CARTESIAN_POINT ( 'NONE',  ( 83.84769081256168022, -38.35769379593097739, -23.82778957254525665 ) ) ;
#35167 = CARTESIAN_POINT ( 'NONE',  ( 41.68366003721723700, -59.99999999999995026, 44.95385205308215859 ) ) ;
#35168 = CARTESIAN_POINT ( 'NONE',  ( -48.98943663899283507, 7.951733423214400354, -16.40652009737680217 ) ) ;
#35169 = CARTESIAN_POINT ( 'NONE',  ( -7.126148247341457242, 41.12758119229482645, -58.55282700859728351 ) ) ;
#35170 = CARTESIAN_POINT ( 'NONE',  ( 36.12951349333496154, 461.0357385931042700, 3.035048805483111511 ) ) ;
#35171 = DIRECTION ( 'NONE',  ( 0.000000000000000000, 0.000000000000000000, -1.000000000000000000 ) ) ;
#35172 = CARTESIAN_POINT ( 'NONE',  ( 82.42421628608209971, 1.030564683017419500E-14, 0.000000000000000000 ) ) ;
#35173 = DIRECTION ( 'NONE',  ( 0.000000000000000000, -1.000000000000000000, 0.000000000000000000 ) ) ;
#35174 = CARTESIAN_POINT ( 'NONE',  ( 108.5077592403022066, -60.00000000000002842, 194.7355029765727465 ) ) ;
#35175 = CARTESIAN_POINT ( 'NONE',  ( -8.673617379884035472E-16, 15.58845726811991561, -1.205771365940065953 ) ) ;
#35176 = TOROIDAL_SURFACE ( 'NONE', #48904, 7.025805963803935406, 3.000000000000000000 ) ;
#35177 = AXIS2_PLACEMENT_3D ( 'NONE', #43532, #42452, #59724 ) ;
#35178 = CARTESIAN_POINT ( 'NONE',  ( -7.344505440741524005, -67.44618927298704136, -3.175463080953004891 ) ) ;
#35179 = ORIENTED_EDGE ( 'NONE', *, *, #10500, .T. ) ;
#35180 =( GEOMETRIC_REPRESENTATION_CONTEXT ( 3 ) GLOBAL_UNCERTAINTY_ASSIGNED_CONTEXT ( ( #17622 ) ) GLOBAL_UNIT_ASSIGNED_CONTEXT ( ( #94362, #28585, #20524 ) ) REPRESENTATION_CONTEXT ( 'NONE', 'WORKASPACE' ) );
#35181 = PRESENTATION_LAYER_ASSIGNMENT (  '', '', ( #52387 ) ) ;
#35182 = CARTESIAN_POINT ( 'NONE',  ( -80.82737729657345938, -30.00000000000002132, 17.73016317466827729 ) ) ;
#35183 = ORIENTED_EDGE ( 'NONE', *, *, #53296, .F. ) ;
#35185 = DIRECTION ( 'NONE',  ( 1.000000000000000000, 0.000000000000000000, 0.000000000000000000 ) ) ;
#35184 = CARTESIAN_POINT ( 'NONE',  ( -76.78686838515666579, -38.43714460091105423, 183.3497871105654440 ) ) ;
#35186 = SURFACE_STYLE_FILL_AREA ( #51321 ) ;
#35187 =( LENGTH_UNIT ( ) NAMED_UNIT ( * ) SI_UNIT ( .MILLI., .METRE. ) );
#35188 = SURFACE_STYLE_FILL_AREA ( #59451 ) ;
#35189 = CARTESIAN_POINT ( 'NONE',  ( 4.401442555609581635E-16, -17.65625000204838813, -7.188101187500000044 ) ) ;
#35190 = CARTESIAN_POINT ( 'NONE',  ( -43.63899620156477965, 434.3182181978404515, 14.37213632273176422 ) ) ;
#35191 = ADVANCED_FACE ( 'NONE', ( #52583 ), #86050, .T. ) ;
#35192 = CARTESIAN_POINT ( 'NONE',  ( 30.55667715332029744, 16.37467338430768038, -39.95293003182862890 ) ) ;
#35194 = EDGE_LOOP ( 'NONE', ( #58342, #59192, #1748, #94174 ) ) ;
#35193 = DIRECTION ( 'NONE',  ( -1.000000000000000000, -0.000000000000000000, -0.000000000000000000 ) ) ;
#35195 = CARTESIAN_POINT ( 'NONE',  ( 80.66719333992175223, -53.39832462065744068, 170.0938344876146857 ) ) ;
#35196 = CARTESIAN_POINT ( 'NONE',  ( 0.000000000000000000, -78.00000000000000000, 39.00000000000000000 ) ) ;
#35197 = CARTESIAN_POINT ( 'NONE',  ( 9.253800200985686786, 86.30010331088172393, -3.791983798715484522 ) ) ;
#35198 = ORIENTED_EDGE ( 'NONE', *, *, #59486, .F. ) ;
#35199 = DIRECTION ( 'NONE',  ( 0.000000000000000000, 0.000000000000000000, 1.000000000000000000 ) ) ;
#35200 = CARTESIAN_POINT ( 'NONE',  ( 0.000000000000000000, 4.898587196589413815E-16, -4.000000000000000888 ) ) ;
#35201 = DIRECTION ( 'NONE',  ( -0.000000000000000000, -1.000000000000000000, -0.000000000000000000 ) ) ;
#35202 = CARTESIAN_POINT ( 'NONE',  ( 0.000000000000000000, 115.0000000000000000, -8.000000000000000000 ) ) ;
#35203 = CARTESIAN_POINT ( 'NONE',  ( -23.88903980719504716, 303.8749885964456894, 10.15971976529453080 ) ) ;
#35204 = PRODUCT ( 'MAS-677', 'MAS-677', '', ( #14196 ) ) ;
#35205 = CARTESIAN_POINT ( 'NONE',  ( 5.385673916453011856, 3.157894736842103534, 14.66382285868950852 ) ) ;
#35206 = EDGE_CURVE ( 'NONE', #45468, #25329, #57716, .T. ) ;
#35207 = VERTEX_POINT ( 'NONE', #94117 ) ;
#35208 = PRESENTATION_LAYER_ASSIGNMENT (  '', '', ( #61063 ) ) ;
#35209 = CYLINDRICAL_SURFACE ( 'NONE', #16482, 4.250000000000000000 ) ;
#35210 = FACE_OUTER_BOUND ( 'NONE', #50689, .T. ) ;
#35211 = CARTESIAN_POINT ( 'NONE',  ( 87.09139377491906941, -35.39572006237809632, 188.3556698165368459 ) ) ;
#35212 = DIRECTION ( 'NONE',  ( 0.000000000000000000, 0.000000000000000000, 1.000000000000000000 ) ) ;
#35213 = MECHANICAL_DESIGN_GEOMETRIC_PRESENTATION_REPRESENTATION (  '', ( #57563 ), #9365 ) ;
#35214 = CARTESIAN_POINT ( 'NONE',  ( 4.401442555609581635E-16, -27.78125000204838457, -7.188101187500000044 ) ) ;
#35215 = CARTESIAN_POINT ( 'NONE',  ( -40.96842839773133704, 488.3806639627545110, 10.59944728061772956 ) ) ;
#35216 = AXIS2_PLACEMENT_3D ( 'NONE', #41568, #97142, #72346 ) ;
#35217 = CARTESIAN_POINT ( 'NONE',  ( 32.81992448453895150, 465.7192846569213316, 11.17271167765130890 ) ) ;
#35218 = EDGE_CURVE ( 'NONE', #7894, #59944, #78461, .T. ) ;
#35219 = CARTESIAN_POINT ( 'NONE',  ( 43.00000000000000000, 436.5989882784185738, 19.94133085611157341 ) ) ;
#35220 = STYLED_ITEM ( 'NONE', ( #11604 ), #85165 ) ;
#35221 = ITEM_DEFINED_TRANSFORMATION ( 'NONE', 'NONE', #17988,  #10728 ) ;
#35222 = EDGE_LOOP ( 'NONE', ( #13448, #20353, #52187, #92184 ) ) ;
#35223 = CARTESIAN_POINT ( 'NONE',  ( 39.30650688512051971, 485.8522658471749764, -4.984147873724974254 ) ) ;
#35224 = SURFACE_STYLE_USAGE ( .BOTH. , #42752 ) ;
#35225 = CARTESIAN_POINT ( 'NONE',  ( -10.11479301378072648, 7.336058586181090746, -5.000000000000000888 ) ) ;
#35226 = ADVANCED_FACE ( 'NONE', ( #94674, #45580 ), #4581, .F. ) ;
#35227 = DIRECTION ( 'NONE',  ( -1.000000000000000000, -0.000000000000000000, -0.000000000000000000 ) ) ;
#35228 = EDGE_LOOP ( 'NONE', ( #47918, #9339, #46907, #33432, #8856 ) ) ;
#35229 = DIRECTION ( 'NONE',  ( 0.000000000000000000, -1.000000000000000000, 0.000000000000000000 ) ) ;
#35230 = DIRECTION ( 'NONE',  ( -1.000000000000000000, 0.000000000000000000, 0.000000000000000000 ) ) ;
#35231 = FACE_OUTER_BOUND ( 'NONE', #60779, .T. ) ;
#35232 = CARTESIAN_POINT ( 'NONE',  ( 32.84237740334622657, 485.2251842821286800, 5.746442123025142124 ) ) ;
#35233 = CARTESIAN_POINT ( 'NONE',  ( 36.57467119294569358, 26.05182110615610469, 11.44111246432268736 ) ) ;
#35234 = CARTESIAN_POINT ( 'NONE',  ( -76.29495167748918050, -60.00000000000000000, 188.1436829353336861 ) ) ;
#35235 = CARTESIAN_POINT ( 'NONE',  ( 0.000000000000000000, 0.000000000000000000, -8.553285714285713937 ) ) ;
#35236 = DIRECTION ( 'NONE',  ( 0.000000000000000000, 0.9952410070626042105, -0.09744402424476066027 ) ) ;
#35237 = SURFACE_STYLE_FILL_AREA ( #34717 ) ;
#35238 = EDGE_CURVE ( 'NONE', #26262, #37787, #14689, .T. ) ;
#35239 = CARTESIAN_POINT ( 'NONE',  ( -85.97713623827759477, -24.93338126948129485, 178.6360369055118724 ) ) ;
#35241 = ADVANCED_FACE ( 'NONE', ( #28905 ), #19916, .T. ) ;
#35240 = VECTOR ( 'NONE', #91049, 1000.000000000000000 ) ;
#35242 = AXIS2_PLACEMENT_3D ( 'NONE', #66342, #59870, #9156 ) ;
#35243 = ORIENTED_EDGE ( 'NONE', *, *, #13178, .T. ) ;
#35244 = CARTESIAN_POINT ( 'NONE',  ( -1.128077836147719282, 302.8478239976500390, 9.936168295454388399 ) ) ;
#35245 = CARTESIAN_POINT ( 'NONE',  ( 3.604576940039115218, -1.047841513645711764, 104.3731177596920787 ) ) ;
#35246 = AXIS2_PLACEMENT_3D ( 'NONE', #4020, #36947, #94645 ) ;
#35247 = CIRCLE ( 'NONE', #2497, 5.000000000000010658 ) ;
#35248 = CARTESIAN_POINT ( 'NONE',  ( -86.56086951948698527, -60.14310811859036221, 1.458335607829068126 ) ) ;
#35249 = CARTESIAN_POINT ( 'NONE',  ( 34.35000000000000142, 1.533819458162526451E-15, 0.000000000000000000 ) ) ;
#35250 = CARTESIAN_POINT ( 'NONE',  ( -35.74363442581862671, 380.1068966271811860, 4.951945592532029927 ) ) ;
#35251 = DIRECTION ( 'NONE',  ( -1.000000000000000000, -1.224606353822377258E-16, -0.000000000000000000 ) ) ;
#35252 = CARTESIAN_POINT ( 'NONE',  ( -15.18610346951687440, -6.148569791254295147, 13.68542098333100299 ) ) ;
#35253 = CARTESIAN_POINT ( 'NONE',  ( 28.34968022077493188, 36.30790721977597713, -8.950547681938596511 ) ) ;
#35254 = CARTESIAN_POINT ( 'NONE',  ( -23.70422451879018055, 42.00000000000000000, 88.20421627933653497 ) ) ;
#35255 = CARTESIAN_POINT ( 'NONE',  ( 71.80342808059909032, -30.00000000000000000, -19.71766482350836469 ) ) ;
#35256 = CARTESIAN_POINT ( 'NONE',  ( 72.40119513776858184, -29.99999999999997868, 139.7542682952119719 ) ) ;
#35257 = SURFACE_SIDE_STYLE ('',( #2310 ) ) ;
#35258 = CARTESIAN_POINT ( 'NONE',  ( -87.78075539319912934, -14.21045842199443499, -8.620330001511526063 ) ) ;
#35259 = CARTESIAN_POINT ( 'NONE',  ( -64.67222873873710398, -60.34389612767258626, 96.31452158953769072 ) ) ;
#35260 = VERTEX_POINT ( 'NONE', #19746 ) ;
#35261 = CARTESIAN_POINT ( 'NONE',  ( 75.88724551625310255, -29.99999999999989697, 164.4338130987444231 ) ) ;
#35262 = CARTESIAN_POINT ( 'NONE',  ( -64.71215703819380849, 40.83860938991785616, 6.807632145269733925 ) ) ;
#35263 = CARTESIAN_POINT ( 'NONE',  ( 5.691016455591895173, -59.99999999998026823, 41.97878891002031310 ) ) ;
#35264 = ORIENTED_EDGE ( 'NONE', *, *, #12962, .T. ) ;
#35265 = CARTESIAN_POINT ( 'NONE',  ( 7.939818003892609610, 52.04606761948748073, -1.683583523684331729 ) ) ;
#35266 = CARTESIAN_POINT ( 'NONE',  ( -1.320432766682874540E-15, -22.90625000204838457, 7.188101187500000044 ) ) ;
#35267 = CARTESIAN_POINT ( 'NONE',  ( -5.649205854336970312, -6.546454671884853305, -2.034449005107561437 ) ) ;
#35268 = VERTEX_POINT ( 'NONE', #85507 ) ;
#35269 = ORIENTED_EDGE ( 'NONE', *, *, #20313, .F. ) ;
#35270 = CARTESIAN_POINT ( 'NONE',  ( 29.34999999999999787, 3.309500000000003439, 4.052968581778167743E-16 ) ) ;
#35271 = SURFACE_SIDE_STYLE ('',( #701 ) ) ;
#35272 = CARTESIAN_POINT ( 'NONE',  ( -50.35455267728183770, -59.99999999998047429, 79.24196553474639870 ) ) ;
#35273 = CARTESIAN_POINT ( 'NONE',  ( 32.74032929948388926, 316.4554875038838873, -6.969597370910324940 ) ) ;
#35274 = CARTESIAN_POINT ( 'NONE',  ( 2.977408999572651815, -11.93750000204838457, 7.188101187500000933 ) ) ;
#35275 = DIRECTION ( 'NONE',  ( -0.5735764363510494901, -0.8191520442889894671, 0.000000000000000000 ) ) ;
#35276 = CARTESIAN_POINT ( 'NONE',  ( 0.9999999999999940048, 0.000000000000000000, 101.0455488498966758 ) ) ;
#35277 = CARTESIAN_POINT ( 'NONE',  ( 0.000000000000000000, 4.000000000000003553, 0.000000000000000000 ) ) ;
#35278 = CARTESIAN_POINT ( 'NONE',  ( -6.145467200823436116, 49.99999999999999289, -92.99666842290275781 ) ) ;
#35279 = AXIS2_PLACEMENT_3D ( 'NONE', #57521, #40819, #40293 ) ;
#35280 = EDGE_CURVE ( 'NONE', #51147, #50622, #80138, .T. ) ;
#35281 = CARTESIAN_POINT ( 'NONE',  ( -12.48827636465884083, -3.503589027571160308, -13.74991316378451423 ) ) ;
#35282 = DIRECTION ( 'NONE',  ( -1.000000000000000000, -0.000000000000000000, -0.000000000000000000 ) ) ;
#35283 = AXIS2_PLACEMENT_3D ( 'NONE', #105057, #31198, #4765 ) ;
#35284 = VERTEX_POINT ( 'NONE', #15312 ) ;
#35285 = CARTESIAN_POINT ( 'NONE',  ( 4.348929473936389734, -1.784082633676211449, 103.6864098602936082 ) ) ;
#35286 = CARTESIAN_POINT ( 'NONE',  ( 33.05110402582430851, -42.96104700131527210, 35.01015022028214929 ) ) ;
#35287 = SURFACE_STYLE_USAGE ( .BOTH. , #36373 ) ;
#35288 = EDGE_CURVE ( 'NONE', #84701, #26386, #8499, .T. ) ;
#35289 = ORIENTED_EDGE ( 'NONE', *, *, #86962, .F. ) ;
#35290 = CARTESIAN_POINT ( 'NONE',  ( -22.10805348356095124, 26.03559744305474055, -31.35713886023327390 ) ) ;
#35291 =( GEOMETRIC_REPRESENTATION_CONTEXT ( 3 ) GLOBAL_UNCERTAINTY_ASSIGNED_CONTEXT ( ( #68153 ) ) GLOBAL_UNIT_ASSIGNED_CONTEXT ( ( #106514, #59050, #25102 ) ) REPRESENTATION_CONTEXT ( 'NONE', 'WORKASPACE' ) );
#35292 = EDGE_LOOP ( 'NONE', ( #22979, #99239, #92151, #52488, #21581 ) ) ;
#35293 = CARTESIAN_POINT ( 'NONE',  ( -0.1698333930863181740, 44.08205155922173901, -16.25874923821028162 ) ) ;
#35294 = DIRECTION ( 'NONE',  ( 1.000000000000000000, 0.000000000000000000, 0.000000000000000000 ) ) ;
#35295 = DIRECTION ( 'NONE',  ( -0.000000000000000000, -0.000000000000000000, 1.000000000000000000 ) ) ;
#35296 = CIRCLE ( 'NONE', #23195, 4.000000000000001776 ) ;
#35297 = CIRCLE ( 'NONE', #28452, 5.000000000000002665 ) ;
#35298 = DIRECTION ( 'NONE',  ( -1.000000000000000000, -0.000000000000000000, -0.000000000000000000 ) ) ;
#35299 =( GEOMETRIC_REPRESENTATION_CONTEXT ( 3 ) GLOBAL_UNCERTAINTY_ASSIGNED_CONTEXT ( ( #59195 ) ) GLOBAL_UNIT_ASSIGNED_CONTEXT ( ( #105425, #56309, #32085 ) ) REPRESENTATION_CONTEXT ( 'NONE', 'WORKASPACE' ) );
#35300 = DIRECTION ( 'NONE',  ( -0.000000000000000000, -0.000000000000000000, 1.000000000000000000 ) ) ;
#35301 = DIRECTION ( 'NONE',  ( 1.000000000000000000, 0.000000000000000000, 0.000000000000000000 ) ) ;
#35302 = VERTEX_POINT ( 'NONE', #55230 ) ;
#35303 = CARTESIAN_POINT ( 'NONE',  ( 65.90086000808869926, -60.00000000000000000, -33.92264569605602276 ) ) ;
#35304 = B_SPLINE_CURVE_WITH_KNOTS ( 'NONE', 3,
 ( #82301, #7871, #98479, #73670, #8411, #56951, #91477, #58016, #81223, #24106, #40251, #50453, #82838, #25164, #8939, #90944, #97957, #89871 ),
 .UNSPECIFIED., .F., .F.,
 ( 4, 2, 2, 2, 2, 2, 2, 2, 4 ),
 ( 0.005485713726180331713, 0.005989477085366931401, 0.006493240444553531089, 0.006997003803740123838, 0.007500767162926716587, 0.008004530522113308469, 0.008508293881299901218, 0.009012057240486493967, 0.009515820599673086716 ),
 .UNSPECIFIED. ) ;
#35305 = PRESENTATION_STYLE_ASSIGNMENT (( #52508 ) ) ;
#35306 = CIRCLE ( 'NONE', #14530, 4.000000000000001776 ) ;
#35307 = SURFACE_STYLE_USAGE ( .BOTH. , #59028 ) ;
#35308 = AXIS2_PLACEMENT_3D ( 'NONE', #100014, #60652, #50918 ) ;
#35309 = CARTESIAN_POINT ( 'NONE',  ( 91.09088295274877112, -5.000000000000000000, 6.123233995736778115E-16 ) ) ;
#35310 = ORIENTED_EDGE ( 'NONE', *, *, #23124, .T. ) ;
#35311 = ADVANCED_FACE ( 'NONE', ( #72999 ), #7762, .T. ) ;
#35312 = CARTESIAN_POINT ( 'NONE',  ( -85.46292727709757742, -29.99999999999107914, 197.4394013638547278 ) ) ;
#35313 = EDGE_LOOP ( 'NONE', ( #101211, #98537, #76746, #91092 ) ) ;
#35314 = B_SPLINE_CURVE_WITH_KNOTS ( 'NONE', 3,
 ( #16566, #47848, #41368, #49449, #80754, #39792, #68857, #83419, #19803, #10063, #60245, #93113, #3036, #10587, #92575, #67776, #34911, #35441, #51039, #59697, #100134, #85572, #101209, #44576, #92044, #83954, #18728, #44032, #68313, #3580, #42973, #75864, #1958, #77467, #18178, #91529, #19285, #84497, #2493, #99594, #36516, #25771, #76925, #27900, #60767, #58631, #26823, #27365 ),
 .UNSPECIFIED., .F., .F.,
 ( 4, 2, 2, 2, 2, 2, 2, 2, 2, 2, 2, 2, 2, 2, 2, 2, 2, 2, 2, 2, 2, 2, 2, 4 ),
 ( -6.000000000621486066E-08, 0.001110492795678789599, 0.002221045591357585346, 0.003331598387036381094, 0.004442151182715176408, 0.005552703978393972589, 0.006663256774072767903, 0.007773809569751563217, 0.008884362365430359398, 0.01110546795678795176, 0.01332657354814554239, 0.01776878473086072538, 0.02221099591357591010, 0.02665320709629109136, 0.03109541827900627262, 0.03553762946172146081, 0.04442205182715165679, 0.05330647419258186664, 0.07107531892344241820, 0.08884416365430296281, 0.1066130083851635352, 0.1243818531160240798, 0.1332662754814543937, 0.1421506978468846660 ),
 .UNSPECIFIED. ) ;
#35315 = ORIENTED_EDGE ( 'NONE', *, *, #70678, .F. ) ;
#35316 = CARTESIAN_POINT ( 'NONE',  ( 7.151217271224856731, 83.21250599554284122, -3.587901469523282927 ) ) ;
#35317 = CARTESIAN_POINT ( 'NONE',  ( 5.975663821522259944, -4.257391242883624471, -5.625982059626766230 ) ) ;
#35318 = CARTESIAN_POINT ( 'NONE',  ( -15.50700860752355759, 34.82687621134751055, -23.25438777637638310 ) ) ;
#35319 = CARTESIAN_POINT ( 'NONE',  ( 0.000000000000000000, 0.000000000000000000, -6.838999999999999524 ) ) ;
#35320 = CARTESIAN_POINT ( 'NONE',  ( 84.40332656976852377, -45.28403232242267507, -9.145071154980445982 ) ) ;
#35321 = CARTESIAN_POINT ( 'NONE',  ( -31.43882072741231681, 310.1515563548447858, -8.305534716118780025 ) ) ;
#35322 = DIRECTION ( 'NONE',  ( 0.5735764363510442720, -0.8191520442889930198, 1.003171929053526349E-16 ) ) ;
#35323 = CARTESIAN_POINT ( 'NONE',  ( -17.99814426515498056, 34.31762318392226518, 23.18337261660863291 ) ) ;
#35324 = CARTESIAN_POINT ( 'NONE',  ( 0.000000000000000000, 0.000000000000000000, 0.000000000000000000 ) ) ;
#35325 = ORIENTED_EDGE ( 'NONE', *, *, #16783, .T. ) ;
#35326 = CARTESIAN_POINT ( 'NONE',  ( -6.838238953609875104, 3.993985489099926678, -6.572971244646267586 ) ) ;
#35327 = ORIENTED_EDGE ( 'NONE', *, *, #30789, .T. ) ;
#35328 = EDGE_CURVE ( 'NONE', #54801, #13998, #71962, .T. ) ;
#35329 = CARTESIAN_POINT ( 'NONE',  ( 48.90200833301634731, 9.381371963275078940, -14.70088518568461566 ) ) ;
#35330 = SURFACE_SIDE_STYLE ('',( #52529 ) ) ;
#35331 = B_SPLINE_CURVE_WITH_KNOTS ( 'NONE', 3,
 ( #45418, #12482, #38912, #30297, #96080, #22211 ),
 .UNSPECIFIED., .F., .F.,
 ( 4, 2, 4 ),
 ( 2.380731629582122378E-07, 0.002336973833157553367, 0.004673709593152147908 ),
 .UNSPECIFIED. ) ;
#35333 = ORIENTED_EDGE ( 'NONE', *, *, #100360, .F. ) ;
#35332 = CARTESIAN_POINT ( 'NONE',  ( 6.046357265851751706, 51.82880103987274367, 6.273311111885435665 ) ) ;
#35334 = CARTESIAN_POINT ( 'NONE',  ( 76.07410448762261979, -39.49124980177613509, 125.1990055723632906 ) ) ;
#35335 = EDGE_CURVE ( 'NONE', #101821, #78629, #18111, .T. ) ;
#35336 = VERTEX_POINT ( 'NONE', #39612 ) ;
#35337 = CARTESIAN_POINT ( 'NONE',  ( 2.994908303143255957, -49.57328227368260087, 40.82351491602005211 ) ) ;
#35338 = CARTESIAN_POINT ( 'NONE',  ( 0.000000000000000000, 0.000000000000000000, -4.425378966781146950 ) ) ;
#35339 = CARTESIAN_POINT ( 'NONE',  ( 4.401442555609581635E-16, -26.28125000204838813, -7.188101187500000044 ) ) ;
#35340 = AXIS2_PLACEMENT_3D ( 'NONE', #76549, #60407, #37743 ) ;
#35341 = CARTESIAN_POINT ( 'NONE',  ( -94.67953089133513345, -57.66492561105124537, -4.550087184288205577 ) ) ;
#35342 = EDGE_CURVE ( 'NONE', #22572, #8098, #63361, .T. ) ;
#35343 = PRODUCT_DEFINITION_FORMATION_WITH_SPECIFIED_SOURCE ( 'ANY', '', #35204, .NOT_KNOWN. ) ;
#35344 = VERTEX_POINT ( 'NONE', #95715 ) ;
#35345 = CARTESIAN_POINT ( 'NONE',  ( 32.74728942619678662, 438.8764684952982975, 23.82517967440744400 ) ) ;
#35346 = CARTESIAN_POINT ( 'NONE',  ( 105.5944179521240756, -60.15122995615571710, 185.0766847636498085 ) ) ;
#35347 = CARTESIAN_POINT ( 'NONE',  ( -9.165151389911684987, 84.73704489083661429, 4.000000000000000000 ) ) ;
#35348 = LINE ( 'NONE', #76293, #13716 ) ;
#35349 = CARTESIAN_POINT ( 'NONE',  ( 5.656854249492378806, -18.87500000409677270, 5.656854249492381470 ) ) ;
#35350 = CARTESIAN_POINT ( 'NONE',  ( -39.88018151434195602, -26.27442631564857578, 35.88468731287488822 ) ) ;
#35351 = LINE ( 'NONE', #18084, #55891 ) ;
#35352 = EDGE_CURVE ( 'NONE', #9677, #42925, #59458, .T. ) ;
#35353 = CARTESIAN_POINT ( 'NONE',  ( 9.253800200985683233, 31.30010331088172748, -3.791983798715485410 ) ) ;
#35354 = DIRECTION ( 'NONE',  ( 0.000000000000000000, -1.000000000000000000, 0.000000000000000000 ) ) ;
#35355 = DIRECTION ( 'NONE',  ( 1.000000000000000000, 0.000000000000000000, 0.000000000000000000 ) ) ;
#35356 = CARTESIAN_POINT ( 'NONE',  ( 0.000000000000000000, 4.898587196589412829E-16, -4.000000000000000000 ) ) ;
#35357 = ORIENTED_EDGE ( 'NONE', *, *, #17490, .F. ) ;
#35358 = DIRECTION ( 'NONE',  ( -1.000000000000000000, -1.224606353822377258E-16, -0.000000000000000000 ) ) ;
#35359 = CARTESIAN_POINT ( 'NONE',  ( 0.2968935920006570695, 7.824247317432593718, 51.71637011724927646 ) ) ;
#35360 = CARTESIAN_POINT ( 'NONE',  ( -89.04407725700431797, -30.00000000000000355, 188.7674523140026679 ) ) ;
#35361 = EDGE_CURVE ( 'NONE', #22931, #23441, #31010, .T. ) ;
#35362 = AXIS2_PLACEMENT_3D ( 'NONE', #96180, #5559, #22842 ) ;
#35363 = VERTEX_POINT ( 'NONE', #81101 ) ;
#35364 = CARTESIAN_POINT ( 'NONE',  ( 3.645564603016916649, -49.01020369241541630, 43.86897233032998145 ) ) ;
#35365 = CARTESIAN_POINT ( 'NONE',  ( 81.35062306902976559, -57.51595381549781649, 200.0166916054824071 ) ) ;
#35366 = AXIS2_PLACEMENT_3D ( 'NONE', #92835, #51842, #84755 ) ;
#35368 = CARTESIAN_POINT ( 'NONE',  ( 37.56673239365899519, 25.75719283951025318, -10.95617127780834998 ) ) ;
#35367 = CARTESIAN_POINT ( 'NONE',  ( -14.98958921077340456, 2.030821136742817945, 0.4231615533124187256 ) ) ;
#35369 = EDGE_CURVE ( 'NONE', #68317, #41649, #63936, .T. ) ;
#35370 = CARTESIAN_POINT ( 'NONE',  ( 31.06825638305650727, -29.95875917721051351, -38.12153552884113594 ) ) ;
#35371 = STYLED_ITEM ( 'NONE', ( #50969 ), #87588 ) ;
#35372 = CARTESIAN_POINT ( 'NONE',  ( -41.39662806798475003, -59.99999999999998579, 54.18885812487171449 ) ) ;
#35373 = CIRCLE ( 'NONE', #6074, 5.000000000000000888 ) ;
#35374 = AXIS2_PLACEMENT_3D ( 'NONE', #33121, #42234, #97819 ) ;
#35375 = DIRECTION ( 'NONE',  ( 0.5735764363510466035, -0.8191520442889914655, 1.003171929053524500E-16 ) ) ;
#35376 =( LENGTH_UNIT ( ) NAMED_UNIT ( * ) SI_UNIT ( .MILLI., .METRE. ) );
#35377 = COLOUR_RGB ( '', 0.66274510, 0.83137255, 0.94901961) ;
#35378 = CARTESIAN_POINT ( 'NONE',  ( -86.46969285347701373, -17.03976896954880615, 183.6895310209484364 ) ) ;
#35379 = ORIENTED_EDGE ( 'NONE', *, *, #102752, .T. ) ;
#35380 = CARTESIAN_POINT ( 'NONE',  ( 30.63818566637229779, 16.09127295623281029, 40.04027533505442449 ) ) ;
#35381 = CARTESIAN_POINT ( 'NONE',  ( -2.020640315534143028, -42.95763966138775913, 31.04680227545052773 ) ) ;
#35382 = CONICAL_SURFACE ( 'NONE', #95646, 6.900000000000000355, 0.9599310885968801443 ) ;
#35383 = CARTESIAN_POINT ( 'NONE',  ( -6.566498363475146149, 41.80386921324385696, -59.12741086741073104 ) ) ;
#35384 = FACE_OUTER_BOUND ( 'NONE', #23070, .T. ) ;
#35386 = CARTESIAN_POINT ( 'NONE',  ( -7.345544385418572908, 54.30768395588341946, 2.471487999594874196 ) ) ;
#35385 = CARTESIAN_POINT ( 'NONE',  ( -35.64312564391374138, 304.2402637384089985, 4.107419002728130764 ) ) ;
#35387 = VERTEX_POINT ( 'NONE', #90269 ) ;
#35388 = B_SPLINE_CURVE_WITH_KNOTS ( 'NONE', 3,
 ( #33884, #60807, #83462, #74826, #907, #99645, #18777, #58673, #2005, #75365, #1466, #18226, #67300, #92086, #51080, #84001, #10107, #62928, #95822, #61881 ),
 .UNSPECIFIED., .F., .F.,
 ( 4, 2, 2, 2, 2, 2, 2, 2, 2, 4 ),
 ( 0.007150819864390691935, 0.007654630284942562542, 0.008158440705494433148, 0.008662251126046304622, 0.009166061546598176096, 0.009669871967150047570, 0.01017368238770191731, 0.01042558759797785305, 0.01067749280825378705, 0.01118130322880565505 ),
 .UNSPECIFIED. ) ;
#35389 = CARTESIAN_POINT ( 'NONE',  ( -36.73034038993296235, 408.1380310545363272, 6.297704266999571310 ) ) ;
#35390 = CARTESIAN_POINT ( 'NONE',  ( 1.250300626116370273, 27.68715609264891597, 39.65716501001974592 ) ) ;
#35391 = DIRECTION ( 'NONE',  ( -0.2271661929664648139, 0.3956501727912606903, 0.8898631701241311864 ) ) ;
#35392 = CARTESIAN_POINT ( 'NONE',  ( 26.72825103767788235, 296.1707100295333817, -1.715122094987715062 ) ) ;
#35393 = CARTESIAN_POINT ( 'NONE',  ( 45.33180403702434091, 464.4945808635454227, 2.178908857919817699 ) ) ;
#35394 = CARTESIAN_POINT ( 'NONE',  ( 57.45015997180046696, 6.975173280561618775E-15, 0.000000000000000000 ) ) ;
#35395 = DIRECTION ( 'NONE',  ( -0.2908996821237400665, 0.5336441332591916886, 0.7941040951779264612 ) ) ;
#35396 = CARTESIAN_POINT ( 'NONE',  ( 93.38347165230982228, -30.00000000000000711, 56.44843285056885662 ) ) ;
#35397 = CARTESIAN_POINT ( 'NONE',  ( -82.53661707010365944, -22.15634074740264126, 142.5693487567720865 ) ) ;
#35398 = ORIENTED_EDGE ( 'NONE', *, *, #85309, .F. ) ;
#35399 = CARTESIAN_POINT ( 'NONE',  ( -17.49999999999996803, 47.99999999999997868, 64.09949417230998847 ) ) ;
#35400 = CARTESIAN_POINT ( 'NONE',  ( 5.647817967127114258, 253.4512640652878872, -2.038183545141138531 ) ) ;
#35401 =( NAMED_UNIT ( * ) PLANE_ANGLE_UNIT ( ) SI_UNIT ( $, .RADIAN. ) );
#35402 = CARTESIAN_POINT ( 'NONE',  ( 14.34999999999999787, 1.533819458162526451E-15, 0.000000000000000000 ) ) ;
#35403 = CARTESIAN_POINT ( 'NONE',  ( 34.79138225435746534, 321.1841114852068131, -5.534975474723330180 ) ) ;
#35404 = DIRECTION ( 'NONE',  ( -1.000000000000000000, 0.000000000000000000, 0.000000000000000000 ) ) ;
#35405 = ORIENTED_EDGE ( 'NONE', *, *, #11141, .T. ) ;
#35406 = UNCERTAINTY_MEASURE_WITH_UNIT (LENGTH_MEASURE( 1.000000000000000082E-05 ), #81083, 'distance_accuracy_value', 'NONE');
#35407 = CARTESIAN_POINT ( 'NONE',  ( -13.76424046522695122, 304.5457540960956067, -10.06505265514019065 ) ) ;
#35408 = CARTESIAN_POINT ( 'NONE',  ( 31.34138169376840466, 438.6792511472767160, 22.89137509121641401 ) ) ;
#35409 = ORIENTED_EDGE ( 'NONE', *, *, #12626, .F. ) ;
#35410 = AXIS2_PLACEMENT_3D ( 'NONE', #42747, #76698, #34157 ) ;
#35411 = CARTESIAN_POINT ( 'NONE',  ( 0.7768758660235928204, 15.00000000000000000, 9.999999999999998224 ) ) ;
#35412 = CARTESIAN_POINT ( 'NONE',  ( 6.546995434871612396, 41.93635067897446334, -69.23592083470533964 ) ) ;
#35413 = EDGE_CURVE ( 'NONE', #83609, #1254, #73203, .T. ) ;
#35414 = CARTESIAN_POINT ( 'NONE',  ( 61.09659575456475977, 50.00000000000000000, -16.41787579823443366 ) ) ;
#35415 = CARTESIAN_POINT ( 'NONE',  ( 41.50669491856072568, -5.000000000000000888, 6.123233995736769241E-16 ) ) ;
#35416 = EDGE_LOOP ( 'NONE', ( #64437, #44898, #106047, #100532, #21382 ) ) ;
#35417 = DIRECTION ( 'NONE',  ( 1.000000000000000000, -0.000000000000000000, -0.000000000000000000 ) ) ;
#35419 = CARTESIAN_POINT ( 'NONE',  ( 22.09608613383313980, -25.55606579312770066, 28.90373523675440381 ) ) ;
#35418 = CARTESIAN_POINT ( 'NONE',  ( -77.57376394631657490, -29.99999999999998934, 180.9696502640093172 ) ) ;
#35420 = CARTESIAN_POINT ( 'NONE',  ( 113.4944653854903720, 14.17434517210798006, 56.74723269274521442 ) ) ;
#35422 = EDGE_CURVE ( 'NONE', #32960, #16973, #21255, .T. ) ;
#35421 = CARTESIAN_POINT ( 'NONE',  ( 37.70493684217908026, 407.6483267487184321, 6.531453235178003247 ) ) ;
#35423 = CARTESIAN_POINT ( 'NONE',  ( -35.82267405487428391, -18.72926178012174603, 31.62524112213710481 ) ) ;
#35424 = FACE_OUTER_BOUND ( 'NONE', #4877, .T. ) ;
#35425 = UNCERTAINTY_MEASURE_WITH_UNIT (LENGTH_MEASURE( 1.000000000000000082E-05 ), #73187, 'distance_accuracy_value', 'NONE');
#35426 = VERTEX_POINT ( 'NONE', #9324 ) ;
#35427 =( NAMED_UNIT ( * ) PLANE_ANGLE_UNIT ( ) SI_UNIT ( $, .RADIAN. ) );
#35428 = CARTESIAN_POINT ( 'NONE',  ( 0.000000000000000000, 79.50000000000000000, 66.50000000000000000 ) ) ;
#35429 = CARTESIAN_POINT ( 'NONE',  ( -13.66195738444678831, -56.44203391523139146, 23.93843443166228724 ) ) ;
#35430 = SURFACE_SIDE_STYLE ('',( #50493 ) ) ;
#35431 = CARTESIAN_POINT ( 'NONE',  ( 48.10000000000000142, 0.000000000000000000, 0.000000000000000000 ) ) ;
#35432 = CARTESIAN_POINT ( 'NONE',  ( 9.112177013564760841, -0.3479193102801454995, 19.74070280225997109 ) ) ;
#35433 = EDGE_LOOP ( 'NONE', ( #15896, #90418, #57944, #27854 ) ) ;
#35434 = CYLINDRICAL_SURFACE ( 'NONE', #44229, 15.00000000000000000 ) ;
#35435 = ORIENTED_EDGE ( 'NONE', *, *, #72140, .F. ) ;
#35436 = AXIS2_PLACEMENT_3D ( 'NONE', #61751, #37490, #19190 ) ;
#35437 = CARTESIAN_POINT ( 'NONE',  ( 98.21845683671166682, -30.00000000000000711, 190.2718979233115419 ) ) ;
#35438 = CARTESIAN_POINT ( 'NONE',  ( 95.70911704725124025, -2.002967142162725287E-29, 5.000000000000011546 ) ) ;
#35439 = CARTESIAN_POINT ( 'NONE',  ( -5.475947152006322760, -81.83782269890876648, 2.462898245435134470 ) ) ;
#35440 = CARTESIAN_POINT ( 'NONE',  ( 86.62833229249164901, -30.00000000000000355, 68.18189329567420032 ) ) ;
#35441 = CARTESIAN_POINT ( 'NONE',  ( -26.98213138876943162, 309.1463827484340072, 11.18347436010351537 ) ) ;
#35442 = VERTEX_POINT ( 'NONE', #74600 ) ;
#35443 = EDGE_CURVE ( 'NONE', #65538, #20373, #81822, .T. ) ;
#35444 = VERTEX_POINT ( 'NONE', #73532 ) ;
#35445 = ORIENTED_EDGE ( 'NONE', *, *, #12607, .T. ) ;
#35447 = EDGE_LOOP ( 'NONE', ( #48164, #73508, #61997, #3280, #83153 ) ) ;
#35446 = CARTESIAN_POINT ( 'NONE',  ( -47.90468627969800508, 11.89467801380304834, -14.35535821593460781 ) ) ;
#35448 = CARTESIAN_POINT ( 'NONE',  ( 3.313708498984800688, -15.78124999999999289, 7.999999999999960032 ) ) ;
#35449 = STYLED_ITEM ( 'NONE', ( #85559 ), #11818 ) ;
#35450 = STYLED_ITEM ( 'NONE', ( #92967 ), #9284 ) ;
#35451 = CARTESIAN_POINT ( 'NONE',  ( 33.49732520203519215, 439.8560114000520116, 24.25307120326154475 ) ) ;
#35452 = CARTESIAN_POINT ( 'NONE',  ( -30.85687531707146292, 345.5963099307835478, 18.44619323452473125 ) ) ;
#35453 = ORIENTED_EDGE ( 'NONE', *, *, #79459, .T. ) ;
#35454 = ORIENTED_EDGE ( 'NONE', *, *, #32944, .T. ) ;
#35455 = CARTESIAN_POINT ( 'NONE',  ( -3.484756791224363770, 15.95824666716552365, -9.380169522195147991 ) ) ;
#35456 = CARTESIAN_POINT ( 'NONE',  ( 74.24387853852118724, -38.32799764064220227, 162.4765421416901177 ) ) ;
#35457 = CARTESIAN_POINT ( 'NONE',  ( 7.999999999999998224, -11.28125000409677092, 3.313708498984766049 ) ) ;
#35458 = CIRCLE ( 'NONE', #11214, 5.000000000000001776 ) ;
#35459 = VECTOR ( 'NONE', #103195, 1000.000000000000000 ) ;
#35460 = CARTESIAN_POINT ( 'NONE',  ( 24.95205008382144030, 304.5524501393400669, 10.31272274050776439 ) ) ;
#35461 = AXIS2_PLACEMENT_3D ( 'NONE', #1510, #17202, #84589 ) ;
#35462 = CARTESIAN_POINT ( 'NONE',  ( -4.472135954999576946, 249.8642079505344498, 4.000000000000004441 ) ) ;
#35463 = VECTOR ( 'NONE', #76121, 1000.000000000000227 ) ;
#35464 = VERTEX_POINT ( 'NONE', #57882 ) ;
#35465 = CARTESIAN_POINT ( 'NONE',  ( 28.43950163419728483, 12.73412882672191770, -40.70661530191392785 ) ) ;
#35466 = AXIS2_PLACEMENT_3D ( 'NONE', #60019, #67561, #10360 ) ;
#35467 = CARTESIAN_POINT ( 'NONE',  ( -44.11327388758650159, 464.4313852428384735, 9.822198357558047377 ) ) ;
#35468 = DIRECTION ( 'NONE',  ( -1.000000000000000000, -1.224606353822377258E-16, -0.000000000000000000 ) ) ;
#35469 = PLANE ( 'NONE',  #29141 ) ;
#35470 = EDGE_CURVE ( 'NONE', #8224, #35344, #49095, .T. ) ;
#35471 = CARTESIAN_POINT ( 'NONE',  ( 14.84237598262652646, 1.406801708889429348, 2.172554589314652063 ) ) ;
#35472 = EDGE_LOOP ( 'NONE', ( #30398, #41674, #405, #17429 ) ) ;
#35474 = CARTESIAN_POINT ( 'NONE',  ( 7.002990960197232440, -86.05266818383456950, 3.868040364119523566 ) ) ;
#35473 = SHAPE_REPRESENTATION_RELATIONSHIP ( 'NONE' , 'NONE' ,  #63931, #56232 ) ;
#35475 = CARTESIAN_POINT ( 'NONE',  ( 40.11650669486618881, 1.474610560812782335E-15, 0.000000000000000000 ) ) ;
#35476 = DIRECTION ( 'NONE',  ( 1.000000000000000000, 0.000000000000000000, 0.000000000000000000 ) ) ;
#35477 = CARTESIAN_POINT ( 'NONE',  ( -0.6169862416617590828, -8.783631307150894685, -7.913704048099813093 ) ) ;
#35478 = CARTESIAN_POINT ( 'NONE',  ( 8.363851124833434625, 294.6905162191789600, 1.902776341390910453 ) ) ;
#35479 = CARTESIAN_POINT ( 'NONE',  ( -7.801777176595946273, 101.4117201418736727, -1.786991866639925597 ) ) ;
#35480 = LINE ( 'NONE', #900, #86371 ) ;
#35481 = CARTESIAN_POINT ( 'NONE',  ( 85.12024738230812204, -50.19341801944306525, 189.4198906295553400 ) ) ;
#35482 = CARTESIAN_POINT ( 'NONE',  ( -7.883792884241596965, 61.98032949400206348, 0.000000000000000000 ) ) ;
#35483 = ORIENTED_EDGE ( 'NONE', *, *, #22418, .F. ) ;
#35484 = CARTESIAN_POINT ( 'NONE',  ( 55.74658202726395473, -57.67088109086454750, -38.72831865961387621 ) ) ;
#35485 = DIRECTION ( 'NONE',  ( -1.000000000000000000, -1.224606353822377258E-16, -0.000000000000000000 ) ) ;
#35486 = CARTESIAN_POINT ( 'NONE',  ( 31.08349330513380693, 1.593028355512270962E-15, 0.000000000000000000 ) ) ;
#35487 = DIRECTION ( 'NONE',  ( 0.000000000000000000, 0.000000000000000000, 1.000000000000000000 ) ) ;
#35488 = MECHANICAL_DESIGN_GEOMETRIC_PRESENTATION_REPRESENTATION (  '', ( #44085 ), #64706 ) ;
#35489 = CARTESIAN_POINT ( 'NONE',  ( -93.51094265731104827, -29.99999999999998934, 109.0518179395232892 ) ) ;
#35490 = EDGE_CURVE ( 'NONE', #59773, #103513, #43964, .T. ) ;
#35491 = DIRECTION ( 'NONE',  ( -1.000000000000000000, -1.224606353822377258E-16, -0.000000000000000000 ) ) ;
#35493 = CARTESIAN_POINT ( 'NONE',  ( 6.953930663124324063, 304.7325910270068334, -10.02533923955978779 ) ) ;
#35492 = CARTESIAN_POINT ( 'NONE',  ( -9.989435848181802413, 246.0261970747156397, -0.5278651953176011213 ) ) ;
#35494 = EDGE_CURVE ( 'NONE', #66787, #72025, #98356, .T. ) ;
#35495 = CARTESIAN_POINT ( 'NONE',  ( 3.048295934048691258, -53.45399299688504868, 40.66583558471658932 ) ) ;
#35496 = FACE_OUTER_BOUND ( 'NONE', #16604, .T. ) ;
#35497 = CARTESIAN_POINT ( 'NONE',  ( 37.96538461538461462, 4.172000000000003261, 0.000000000000000000 ) ) ;
#35498 = CARTESIAN_POINT ( 'NONE',  ( 7.347171990167082001, -3.439186728100506851, -18.43985286355972519 ) ) ;
#35499 = CARTESIAN_POINT ( 'NONE',  ( 0.000000000000000000, 4.898587196589412829E-16, -4.000000000000000000 ) ) ;
#35500 = CARTESIAN_POINT ( 'NONE',  ( 21.83701553852647947, -19.09061506513711493, -33.46987204855414433 ) ) ;
#35501 = AXIS2_PLACEMENT_3D ( 'NONE', #90953, #40784, #65599 ) ;
#35502 = CARTESIAN_POINT ( 'NONE',  ( -25.36348844297524963, -53.39683697002490703, 34.19068731400996342 ) ) ;
#35503 = EDGE_CURVE ( 'NONE', #97818, #39874, #48421, .T. ) ;
#35504 = ORIENTED_EDGE ( 'NONE', *, *, #38069, .T. ) ;
#35505 = CARTESIAN_POINT ( 'NONE',  ( 6.999768563658489207, 9.000405013899001716, -0.2746924679829751414 ) ) ;
#35506 = CARTESIAN_POINT ( 'NONE',  ( -9.176645556628256983, 105.5273903240672837, 3.973966573947711023 ) ) ;
#35507 = CARTESIAN_POINT ( 'NONE',  ( -19.65540319560976101, -18.59144410933823366, 27.44006592855480520 ) ) ;
#35508 = DIRECTION ( 'NONE',  ( -1.000000000000000000, -0.000000000000000000, -0.000000000000000000 ) ) ;
#35510 = CARTESIAN_POINT ( 'NONE',  ( 0.1689026954396629643, 37.21016666119767535, -27.24999999999999289 ) ) ;
#35509 = CARTESIAN_POINT ( 'NONE',  ( -0.1683297036434198424, 28.20649408426939786, 38.25000000000000711 ) ) ;
#35511 = AXIS2_PLACEMENT_3D ( 'NONE', #19831, #75883, #76404 ) ;
#35512 = EDGE_LOOP ( 'NONE', ( #32985, #84659, #77674, #23200, #104230 ) ) ;
#35513 = CARTESIAN_POINT ( 'NONE',  ( 104.3757837139179117, 5.000000000000023093, 6.123233995736781074E-16 ) ) ;
#35514 = ORIENTED_EDGE ( 'NONE', *, *, #80825, .F. ) ;
#35515 = PRESENTATION_STYLE_ASSIGNMENT (( #3657 ) ) ;
#35516 = DIRECTION ( 'NONE',  ( 0.000000000000000000, 0.000000000000000000, 1.000000000000000000 ) ) ;
#35517 = B_SPLINE_CURVE_WITH_KNOTS ( 'NONE', 3,
 ( #25290, #58699, #9583, #73794, #81344, #56537, #89468, #41435 ),
 .UNSPECIFIED., .F., .F.,
 ( 4, 2, 2, 4 ),
 ( 0.007886720825438788343, 0.009850969036564002912, 0.01181521724768921748, 0.01574371366993964488 ),
 .UNSPECIFIED. ) ;
#35518 = PRESENTATION_LAYER_ASSIGNMENT (  '', '', ( #81967 ) ) ;
#35519 = CARTESIAN_POINT ( 'NONE',  ( 0.2595206531158509300, 2.531175536751804511, 6.499999999999996447 ) ) ;
#35520 = EDGE_LOOP ( 'NONE', ( #76691, #26222, #65185, #46815 ) ) ;
#35521 = FACE_OUTER_BOUND ( 'NONE', #59762, .T. ) ;
#35522 = AXIS2_PLACEMENT_3D ( 'NONE', #59433, #24948, #92296 ) ;
#35523 = FACE_OUTER_BOUND ( 'NONE', #81285, .T. ) ;
#35524 = CIRCLE ( 'NONE', #52725, 65.50000000000000000 ) ;
#35525 = CARTESIAN_POINT ( 'NONE',  ( 98.68619524362034667, -37.78306943100542270, 192.1284777729563302 ) ) ;
#35526 = CIRCLE ( 'NONE', #25208, 4.000000000000000888 ) ;
#35528 = DIRECTION ( 'NONE',  ( -1.000000000000000000, -1.224606353822377258E-16, -0.000000000000000000 ) ) ;
#35527 = DIRECTION ( 'NONE',  ( 0.000000000000000000, -1.000000000000000000, 0.000000000000000000 ) ) ;
#35529 = ORIENTED_EDGE ( 'NONE', *, *, #83581, .F. ) ;
#35530 = ORIENTED_EDGE ( 'NONE', *, *, #75629, .T. ) ;
#35531 = CIRCLE ( 'NONE', #49258, 5.000000000000001776 ) ;
#35532 = ORIENTED_EDGE ( 'NONE', *, *, #97424, .F. ) ;
#35533 = CARTESIAN_POINT ( 'NONE',  ( 25.02429500009634822, 305.9718288055595963, 10.41235884080700203 ) ) ;
#35534 = DIRECTION ( 'NONE',  ( -0.000000000000000000, 1.000000000000000000, 2.311253228826400140E-16 ) ) ;
#35535 = LINE ( 'NONE', #68410, #27879 ) ;
#35536 = EDGE_LOOP ( 'NONE', ( #92056, #101483, #78062, #64248 ) ) ;
#35537 = ADVANCED_FACE ( 'NONE', ( #89747 ), #54323, .T. ) ;
#35538 = DIRECTION ( 'NONE',  ( 1.000000000000000000, 1.224606353822377258E-16, 0.000000000000000000 ) ) ;
#35539 = SURFACE_STYLE_USAGE ( .BOTH. , #91098 ) ;
#35540 = CARTESIAN_POINT ( 'NONE',  ( 9.797174393178825657E-16, -30.00000000000000000, -8.000000000000000000 ) ) ;
#35541 = CARTESIAN_POINT ( 'NONE',  ( -91.59607114535849348, -60.00000000000365219, -20.75833340651075787 ) ) ;
#35542 = CARTESIAN_POINT ( 'NONE',  ( 7.150931910075639664, -66.78625798522263324, -3.588457848165360620 ) ) ;
#35543 = CARTESIAN_POINT ( 'NONE',  ( -30.95643954367146833, 313.8918926584737505, -7.857037206977866006 ) ) ;
#35544 = DIRECTION ( 'NONE',  ( -1.000000000000000000, -1.224606353822377258E-16, -0.000000000000000000 ) ) ;
#35545 = CARTESIAN_POINT ( 'NONE',  ( -86.84190767202800032, -14.21045842199442788, 3.676479754794546473 ) ) ;
#35546 = ADVANCED_FACE ( 'NONE', ( #60579 ), #2296, .F. ) ;
#35548 = ADVANCED_FACE ( 'NONE', ( #18526 ), #51385, .T. ) ;
#35547 = CARTESIAN_POINT ( 'NONE',  ( -46.00000000000000000, 437.9690125970932968, 14.09127711025707796 ) ) ;
#35549 = CARTESIAN_POINT ( 'NONE',  ( -52.50648933632491833, -18.71248995424286932, 47.73799938596632586 ) ) ;
#35550 = VERTEX_POINT ( 'NONE', #76194 ) ;
#35551 = CARTESIAN_POINT ( 'NONE',  ( 7.000000000000000000, 0.000000000000000000, -2.575493252495433261 ) ) ;
#35552 = ORIENTED_EDGE ( 'NONE', *, *, #5219, .T. ) ;
#35553 = CARTESIAN_POINT ( 'NONE',  ( 12.49989493515518646, 18.64301898209307140, -36.27145154709465658 ) ) ;
#35554 = CARTESIAN_POINT ( 'NONE',  ( -9.740083726526439278, 294.6493269980080072, -10.04303756037268158 ) ) ;
#35555 = CARTESIAN_POINT ( 'NONE',  ( 5.190609988845229950, -7.360777132564092717, -3.016375611400007095 ) ) ;
#35557 = ORIENTED_EDGE ( 'NONE', *, *, #99103, .T. ) ;
#35556 = AXIS2_PLACEMENT_3D ( 'NONE', #86607, #12671, #35948 ) ;
#35558 = CARTESIAN_POINT ( 'NONE',  ( 4.497472161260642309, 249.4577745337406043, -3.972129482042469739 ) ) ;
#35559 = CARTESIAN_POINT ( 'NONE',  ( 84.40133724763363432, -29.99999999999239364, -21.52947726462551969 ) ) ;
#35560 = DIRECTION ( 'NONE',  ( -1.000000000000000000, -1.224606353822377258E-16, -0.000000000000000000 ) ) ;
#35561 = CARTESIAN_POINT ( 'NONE',  ( 9.999999999999994671, 16.00000000000000000, 4.582575694955847823 ) ) ;
#35562 = CIRCLE ( 'NONE', #2799, 5.000000000000000000 ) ;
#35563 = CARTESIAN_POINT ( 'NONE',  ( 11.85444436786839084, 42.00000000000000000, -90.56128410203886858 ) ) ;
#35564 = CARTESIAN_POINT ( 'NONE',  ( 89.35863705434196902, -29.99999999999999645, 189.1991920285174160 ) ) ;
#35565 = DIRECTION ( 'NONE',  ( 0.000000000000000000, -1.000000000000000000, 0.000000000000000000 ) ) ;
#35566 = DIRECTION ( 'NONE',  ( 0.000000000000000000, -1.000000000000000000, -0.000000000000000000 ) ) ;
#35567 = EDGE_CURVE ( 'NONE', #104315, #71900, #72861, .T. ) ;
#35568 = ORIENTED_EDGE ( 'NONE', *, *, #27462, .T. ) ;
#35569 = ORIENTED_EDGE ( 'NONE', *, *, #57813, .T. ) ;
#35570 = CARTESIAN_POINT ( 'NONE',  ( 52.08973531413104041, -32.57578831394647523, 51.93190986806391862 ) ) ;
#35571 = CARTESIAN_POINT ( 'NONE',  ( 6.516858182563246338, 41.40454334770866751, -58.45804045544070959 ) ) ;
#35572 = CARTESIAN_POINT ( 'NONE',  ( -43.71297783477830734, 485.1278128289774259, -1.116606130290624721 ) ) ;
#35573 = EDGE_CURVE ( 'NONE', #6732, #26726, #106285, .T. ) ;
#35574 = ORIENTED_EDGE ( 'NONE', *, *, #3686, .F. ) ;
#35575 = CARTESIAN_POINT ( 'NONE',  ( -89.77470481043597772, -38.39469723191136552, -16.55334520362848849 ) ) ;
#35576 = VERTEX_POINT ( 'NONE', #69719 ) ;
#35577 = CARTESIAN_POINT ( 'NONE',  ( 106.0169255512641087, -38.37657707414045660, 196.3210357038191205 ) ) ;
#35578 = CARTESIAN_POINT ( 'NONE',  ( 10.62194528067082189, 14.25751096852423494, 9.925505253905029690 ) ) ;
#35579 = CARTESIAN_POINT ( 'NONE',  ( 86.03480774772026507, -52.71534935679705569, 32.67177944397322875 ) ) ;
#35580 = CARTESIAN_POINT ( 'NONE',  ( 34.24300530784454111, 434.2296727341958444, 10.63337750349099764 ) ) ;
#35581 = CARTESIAN_POINT ( 'NONE',  ( 43.00000000000000000, 450.0000000000002274, 13.20242257375370976 ) ) ;
#35582 =( LENGTH_UNIT ( ) NAMED_UNIT ( * ) SI_UNIT ( .MILLI., .METRE. ) );
#35583 = CARTESIAN_POINT ( 'NONE',  ( 6.222582369487714260, -4.088457415080680057, 6.500000000000000888 ) ) ;
#35584 = FILL_AREA_STYLE_COLOUR ( '', #19975 ) ;
#35585 = CARTESIAN_POINT ( 'NONE',  ( 3.443379947490608828, 124.1431617552111817, 4.999999999999999112 ) ) ;
#35586 = VERTEX_POINT ( 'NONE', #102611 ) ;
#35587 = CARTESIAN_POINT ( 'NONE',  ( 1.249225752714849813, 36.86244653973282226, 28.17767836393376513 ) ) ;
#35588 = CIRCLE ( 'NONE', #95844, 5.000000000000000888 ) ;
#35590 = B_SPLINE_CURVE_WITH_KNOTS ( 'NONE', 3,
 ( #52819, #26994, #93817, #34550, #18902, #60930, #28058, #19973, #10748, #101378 ),
 .UNSPECIFIED., .F., .F.,
 ( 4, 2, 2, 2, 4 ),
 ( 3.698327573679174046E-29, 0.009876477788552447123, 0.01481471668282867589, 0.01728383612996678420, 0.01975295557710489425 ),
 .UNSPECIFIED. ) ;
#35589 = CARTESIAN_POINT ( 'NONE',  ( 7.428753218262151847, 40.00000000162874869, -70.23138194497943232 ) ) ;
#35591 = CARTESIAN_POINT ( 'NONE',  ( 44.46823338009918558, 1.482358050883964840E-15, 0.000000000000000000 ) ) ;
#35592 = ORIENTED_EDGE ( 'NONE', *, *, #43186, .F. ) ;
#35593 = CARTESIAN_POINT ( 'NONE',  ( -35.10770204084435875, 352.9232395558267399, 2.060922233138942072 ) ) ;
#35594 = CARTESIAN_POINT ( 'NONE',  ( -34.17726614582090150, 303.5588809801041634, 11.95427360728275445 ) ) ;
#35595 = DIRECTION ( 'NONE',  ( -1.000000000000000000, -1.224606353822377258E-16, -0.000000000000000000 ) ) ;
#35596 = DIRECTION ( 'NONE',  ( 0.000000000000000000, 1.000000000000000000, 0.000000000000000000 ) ) ;
#35597 = CARTESIAN_POINT ( 'NONE',  ( 8.000000000000000000, -18.40624999999998934, -3.313708498984761608 ) ) ;
#35598 = CARTESIAN_POINT ( 'NONE',  ( -53.08935917470198262, -30.00000000000002132, 52.21147893555088615 ) ) ;
#35599 = CONICAL_SURFACE ( 'NONE', #38955, 3.400000000000000355, 0.9599310885968748153 ) ;
#35600 = VECTOR ( 'NONE', #12718, 1000.000000000000114 ) ;
#35601 = PRESENTATION_LAYER_ASSIGNMENT (  '', '', ( #4541 ) ) ;
#35602 = DIRECTION ( 'NONE',  ( 0.000000000000000000, -1.000000000000000000, 0.000000000000000000 ) ) ;
#35603 = COLOUR_RGB ( '', 0.40784314, 0.44705882, 0.49803922) ;
#35604 = ORIENTED_EDGE ( 'NONE', *, *, #41266, .T. ) ;
#35605 = CARTESIAN_POINT ( 'NONE',  ( 86.20298226707136280, -18.29538666924914025, 168.7790078290781253 ) ) ;
#35606 = DIRECTION ( 'NONE',  ( -1.000000000000000000, -1.224606353822377258E-16, -0.000000000000000000 ) ) ;
#35607 = FACE_OUTER_BOUND ( 'NONE', #21574, .T. ) ;
#35608 = ORIENTED_EDGE ( 'NONE', *, *, #45450, .F. ) ;
#35609 = CARTESIAN_POINT ( 'NONE',  ( -85.13303551996550311, -45.26552266227979260, 36.04504711083556856 ) ) ;
#35610 = AXIS2_PLACEMENT_3D ( 'NONE', #4948, #78290, #62663 ) ;
#35611 = CARTESIAN_POINT ( 'NONE',  ( 0.05533025579361924157, -6.264553569211837036, 2.149474931388137389 ) ) ;
#35612 = CARTESIAN_POINT ( 'NONE',  ( 14.73122683063179217, -3.000000000000002665, -81.05502296679115659 ) ) ;
#35613 = CARTESIAN_POINT ( 'NONE',  ( 13.24502500596364740, -3.000000000000001776, -77.83160543688525479 ) ) ;
#35614 = AXIS2_PLACEMENT_3D ( 'NONE', #3380, #68103, #35236 ) ;
#35615 = CARTESIAN_POINT ( 'NONE',  ( -14.02598654517192678, -23.76892447270615705, -38.53458435890105704 ) ) ;
#35616 = EDGE_CURVE ( 'NONE', #70143, #53794, #57095, .T. ) ;
#35618 = CIRCLE ( 'NONE', #95877, 15.00000000000001243 ) ;
#35617 = CARTESIAN_POINT ( 'NONE',  ( 45.83015609643102550, -60.00000000000000000, 62.25697969437710810 ) ) ;
#35619 = DIRECTION ( 'NONE',  ( -0.5735764363510497121, 0.8191520442889892450, 1.003171929053521665E-16 ) ) ;
#35620 = CARTESIAN_POINT ( 'NONE',  ( 7.934996450857311423, 108.8686245647253088, -1.050865690281775677 ) ) ;
#35621 = DIRECTION ( 'NONE',  ( -1.000000000000000000, -0.000000000000000000, -0.000000000000000000 ) ) ;
#35622 = ADVANCED_FACE ( 'NONE', ( #1767 ), #83596, .T. ) ;
#35624 = CARTESIAN_POINT ( 'NONE',  ( -11.87699017361764753, 16.68016500116531020, 9.302345733532593641 ) ) ;
#35623 = CARTESIAN_POINT ( 'NONE',  ( -2.499999999999996447, -19.94872641843396721, -28.09930264074299444 ) ) ;
#35625 = EDGE_CURVE ( 'NONE', #70018, #77725, #68669, .T. ) ;
#35626 = CARTESIAN_POINT ( 'NONE',  ( 4.913676358839419223, 296.1360674232993802, -10.01007018187845077 ) ) ;
#35627 = CARTESIAN_POINT ( 'NONE',  ( 21.51569398614858031, 294.9107018935607130, -9.987480606144490736 ) ) ;
#35628 =( NAMED_UNIT ( * ) PLANE_ANGLE_UNIT ( ) SI_UNIT ( $, .RADIAN. ) );
#35629 = DIRECTION ( 'NONE',  ( 0.000000000000000000, -1.000000000000000000, 0.000000000000000000 ) ) ;
#35630 = EDGE_CURVE ( 'NONE', #2025, #16424, #59505, .T. ) ;
#35631 = ORIENTED_EDGE ( 'NONE', *, *, #91993, .F. ) ;
#35632 = LINE ( 'NONE', #92216, #60592 ) ;
#35633 = CIRCLE ( 'NONE', #78689, 4.000000000000001776 ) ;
#35634 = EDGE_CURVE ( 'NONE', #32321, #38839, #47086, .T. ) ;
#35635 = ORIENTED_EDGE ( 'NONE', *, *, #4287, .T. ) ;
#35636 = SURFACE_STYLE_USAGE ( .BOTH. , #52300 ) ;
#35637 = CARTESIAN_POINT ( 'NONE',  ( 0.000000000000000000, 50.89575828009192549, -11.27631144943088692 ) ) ;
#35638 = CIRCLE ( 'NONE', #87276, 1.000000000000001110 ) ;
#35639 = DIRECTION ( 'NONE',  ( -1.000000000000000000, -1.224606353822377258E-16, -0.000000000000000000 ) ) ;
#35641 = CARTESIAN_POINT ( 'NONE',  ( 9.564681418035569038, -47.40889936360509438, -34.57825658523572798 ) ) ;
#35640 = CARTESIAN_POINT ( 'NONE',  ( 9.644834624769996978, 253.0089050020578156, 2.648308524638408823 ) ) ;
#35642 = ORIENTED_EDGE ( 'NONE', *, *, #53030, .F. ) ;
#35643 = CARTESIAN_POINT ( 'NONE',  ( 28.18125686882138226, 36.45097005328995721, 8.150216328741358041 ) ) ;
#35644 = DIRECTION ( 'NONE',  ( 0.000000000000000000, 0.000000000000000000, 1.000000000000000000 ) ) ;
#35645 = ORIENTED_EDGE ( 'NONE', *, *, #32967, .T. ) ;
#35646 = FACE_OUTER_BOUND ( 'NONE', #64631, .T. ) ;
#35647 = DIRECTION ( 'NONE',  ( 0.000000000000000000, -1.000000000000000000, 0.000000000000000000 ) ) ;
#35648 = CARTESIAN_POINT ( 'NONE',  ( -94.53821169941970481, -60.00000000000002132, 45.58263737987853403 ) ) ;
#35649 = DIRECTION ( 'NONE',  ( -1.000000000000000000, -1.224606353822377258E-16, -0.000000000000000000 ) ) ;
#35650 = DIRECTION ( 'NONE',  ( 0.000000000000000000, 0.000000000000000000, 1.000000000000000000 ) ) ;
#35651 = CARTESIAN_POINT ( 'NONE',  ( 40.97307933990123985, 465.3163409530395711, 16.72193089366239960 ) ) ;
#35653 = FILL_AREA_STYLE_COLOUR ( '', #18503 ) ;
#35652 =( REPRESENTATION_RELATIONSHIP ('NONE','NONE', #69581, #88164 ) REPRESENTATION_RELATIONSHIP_WITH_TRANSFORMATION ( #28206 )SHAPE_REPRESENTATION_RELATIONSHIP( ) );
#35654 = CARTESIAN_POINT ( 'NONE',  ( -1.308996937480702005, -3.000000000000002665, -95.00000000000000000 ) ) ;
#35655 = CARTESIAN_POINT ( 'NONE',  ( -83.68639855425038832, -35.98482338576268802, 170.8203333709438425 ) ) ;
#35656 = CIRCLE ( 'NONE', #66643, 5.000000000000001776 ) ;
#35657 = VERTEX_POINT ( 'NONE', #78325 ) ;
#35658 = FACE_OUTER_BOUND ( 'NONE', #93755, .T. ) ;
#35659 = ORIENTED_EDGE ( 'NONE', *, *, #77534, .F. ) ;
#35660 = VERTEX_POINT ( 'NONE', #63224 ) ;
#35661 = CARTESIAN_POINT ( 'NONE',  ( -16.13870609129251221, 303.5610354609489150, -10.06180398438553247 ) ) ;
#35662 = CARTESIAN_POINT ( 'NONE',  ( 10.34493385746861627, -4.332661967061061326, -14.59917742215513314 ) ) ;
#35663 = CARTESIAN_POINT ( 'NONE',  ( 32.62207953394533178, 5.000000000000003553, 0.000000000000000000 ) ) ;
#35664 = VERTEX_POINT ( 'NONE', #95584 ) ;
#35666 = B_SPLINE_CURVE_WITH_KNOTS ( 'NONE', 3,
 ( #41188, #155, #97289, #1222, #74070, #98867, #56827, #89748, #15845, #48726 ),
 .UNSPECIFIED., .F., .F.,
 ( 4, 2, 2, 2, 4 ),
 ( 0.000000000000000000, 0.5000000000000000000, 0.7500000000000000000, 0.8750000000000000000, 1.000000000000000000 ),
 .UNSPECIFIED. ) ;
#35665 = CARTESIAN_POINT ( 'NONE',  ( 91.09088295274877112, 1.030564683017419500E-14, 0.000000000000000000 ) ) ;
#35667 = CARTESIAN_POINT ( 'NONE',  ( -113.5700743903323087, -57.67116359713492812, 158.3188924881959849 ) ) ;
#35668 = CARTESIAN_POINT ( 'NONE',  ( 7.046357527897574968, -11.30615650601004596, -3.789683693877206050 ) ) ;
#35669 = DIRECTION ( 'NONE',  ( 0.000000000000000000, 1.000000000000000000, 0.000000000000000000 ) ) ;
#35670 = CONICAL_SURFACE ( 'NONE', #30502, 15.00000000000000178, 0.7292773806962717931 ) ;
#35671 = FILL_AREA_STYLE_COLOUR ( '', #63561 ) ;
#35672 = DIRECTION ( 'NONE',  ( 1.000000000000000000, 1.224606353822377258E-16, 0.000000000000000000 ) ) ;
#35673 = CIRCLE ( 'NONE', #14903, 5.000000000000002665 ) ;
#35674 = CARTESIAN_POINT ( 'NONE',  ( -43.00000000000000000, 464.8825480873695710, 15.07585856869432206 ) ) ;
#35675 = CARTESIAN_POINT ( 'NONE',  ( 97.09801539114592117, -30.00000000000000711, 79.69841507686976456 ) ) ;
#35676 = EDGE_CURVE ( 'NONE', #33529, #96258, #57806, .T. ) ;
#35677 = CARTESIAN_POINT ( 'NONE',  ( -94.36268555338997999, -29.99999999999996803, 200.0833938634536935 ) ) ;
#35678 = CARTESIAN_POINT ( 'NONE',  ( -60.76648917972766384, -22.12019031114792966, 66.06036334567909307 ) ) ;
#35679 = EDGE_LOOP ( 'NONE', ( #89925, #20754, #103224, #99682 ) ) ;
#35680 = CARTESIAN_POINT ( 'NONE',  ( 0.000000000000000000, 0.000000000000000000, 1.734723475976807094E-15 ) ) ;
#35682 = ORIENTED_EDGE ( 'NONE', *, *, #131, .F. ) ;
#35681 = CONICAL_SURFACE ( 'NONE', #64897, 3.309500000000001663, 0.9599310885968770357 ) ;
#35683 = AXIS2_PLACEMENT_3D ( 'NONE', #87293, #27097, #43245 ) ;
#35684 = CARTESIAN_POINT ( 'NONE',  ( -102.5236597725247947, -45.26536941210562759, 187.4725801446850255 ) ) ;
#35686 = VECTOR ( 'NONE', #54856, 1000.000000000000000 ) ;
#35685 = CYLINDRICAL_SURFACE ( 'NONE', #35126, 2.000000000000001776 ) ;
#35687 = DIRECTION ( 'NONE',  ( -1.000000000000000000, -1.224606353822377258E-16, -0.000000000000000000 ) ) ;
#35688 = CARTESIAN_POINT ( 'NONE',  ( 0.9654893961777153422, -30.00000000000000355, 7.122964895856731538 ) ) ;
#35689 = EDGE_LOOP ( 'NONE', ( #47554, #69333, #75486, #70395, #95452, #51971 ) ) ;
#35690 = CARTESIAN_POINT ( 'NONE',  ( 4.000000000000002665, 4.898587196589416773E-16, -7.974599999999995248 ) ) ;
#35691 = CARTESIAN_POINT ( 'NONE',  ( -42.15816230349173566, -59.99999999999998579, 55.39162115207339099 ) ) ;
#35692 = CARTESIAN_POINT ( 'NONE',  ( 36.31532598674183987, 26.06253081513260739, -12.14693892978808876 ) ) ;
#35693 = CARTESIAN_POINT ( 'NONE',  ( 7.188101187499999156, -12.12500000204838990, 2.977408999572654924 ) ) ;
#35694 = FACE_BOUND ( 'NONE', #58077, .T. ) ;
#35695 = CONICAL_SURFACE ( 'NONE', #39140, 4.000000000000007105, 0.9599310885968835860 ) ;
#35696 = CARTESIAN_POINT ( 'NONE',  ( 13.52495681778930958, -0.000000000000000000, -10.38447319517952216 ) ) ;
#35697 = CARTESIAN_POINT ( 'NONE',  ( -12.06346645439339937, -4.728929080161973886, -12.59383595213993523 ) ) ;
#35698 = CARTESIAN_POINT ( 'NONE',  ( 27.57151080649627417, 314.0751515626058676, 12.18133379269485239 ) ) ;
#35699 =( NAMED_UNIT ( * ) PLANE_ANGLE_UNIT ( ) SI_UNIT ( $, .RADIAN. ) );
#35700 = CARTESIAN_POINT ( 'NONE',  ( -15.39661048887588102, 46.16593794825681130, -5.596966726906050127 ) ) ;
#35701 = CARTESIAN_POINT ( 'NONE',  ( -7.500000000000003553, -0.03736385522455209357, -23.73594627047615901 ) ) ;
#35702 = CARTESIAN_POINT ( 'NONE',  ( -30.83233686821828456, -18.66184128751320515, 29.63134590784697409 ) ) ;
#35703 = CARTESIAN_POINT ( 'NONE',  ( 44.20965380832324598, -53.34280533345454955, 46.32928704068250880 ) ) ;
#35704 = CARTESIAN_POINT ( 'NONE',  ( -30.00000000000000000, 1.040949779275249548E-15, 7.999999999999986677 ) ) ;
#35705 = CARTESIAN_POINT ( 'NONE',  ( -1.010678914899137304, 46.02204249784927725, 16.74682395785559663 ) ) ;
#35706 = EDGE_CURVE ( 'NONE', #80759, #44815, #38895, .T. ) ;
#35707 = CARTESIAN_POINT ( 'NONE',  ( -97.86142940197255768, -38.48039219746727468, 201.0047720557965363 ) ) ;
#35708 = VERTEX_POINT ( 'NONE', #71822 ) ;
#35710 = CARTESIAN_POINT ( 'NONE',  ( 31.08349330513380337, 4.000000000000002665, 0.000000000000000000 ) ) ;
#35709 = DIRECTION ( 'NONE',  ( 0.000000000000000000, -1.000000000000000000, 0.000000000000000000 ) ) ;
#35711 = CARTESIAN_POINT ( 'NONE',  ( 47.15958797797829050, -60.00000000000000711, 52.51100894563059995 ) ) ;
#35712 = CARTESIAN_POINT ( 'NONE',  ( -19.10613678898662471, 49.68048510767285109, 61.72917303677328960 ) ) ;
#35713 = CARTESIAN_POINT ( 'NONE',  ( -7.416285793330573028, 41.02764771990347015, -59.17152505158298936 ) ) ;
#35714 = CARTESIAN_POINT ( 'NONE',  ( 6.616217471285501084, 40.56071481283028390, -71.17595774755042726 ) ) ;
#35715 = CARTESIAN_POINT ( 'NONE',  ( 0.000000000000000000, -1.200583151104947843, 112.0000000000000000 ) ) ;
#35716 = CARTESIAN_POINT ( 'NONE',  ( 0.000000000000000000, 0.000000000000000000, -8.000000000000000000 ) ) ;
#35717 = CARTESIAN_POINT ( 'NONE',  ( 32.04696785526762426, 435.9094004289368627, 19.86239142642784117 ) ) ;
#35718 = ADVANCED_FACE ( 'NONE', ( #4439 ), #30280, .F. ) ;
#35719 = CARTESIAN_POINT ( 'NONE',  ( 112.1770130220217112, -60.00000000000001421, 169.0659528092184587 ) ) ;
#35720 = CIRCLE ( 'NONE', #28881, 4.000000000000001776 ) ;
#35721 = CARTESIAN_POINT ( 'NONE',  ( -7.986539162393899716, -68.97327171057453654, -0.5321833565149920453 ) ) ;
#35722 = ORIENTED_EDGE ( 'NONE', *, *, #71183, .F. ) ;
#35723 = CARTESIAN_POINT ( 'NONE',  ( 36.73887825314411515, 438.2333816059632454, 3.899276075025526644 ) ) ;
#35724 = CARTESIAN_POINT ( 'NONE',  ( -80.17022493459282373, -30.00000000000006040, -13.56932818816917496 ) ) ;
#35725 = ORIENTED_EDGE ( 'NONE', *, *, #33574, .T. ) ;
#35727 = CARTESIAN_POINT ( 'NONE',  ( 87.62222222222222001, 1.023464760207051730E-14, 0.000000000000000000 ) ) ;
#35726 = CARTESIAN_POINT ( 'NONE',  ( -71.97172513630449942, -38.32687865468555088, 145.5980316631960818 ) ) ;
#35728 = CARTESIAN_POINT ( 'NONE',  ( -1.469576158976823947E-15, -21.87499999999999289, 8.000000000000000000 ) ) ;
#35729 = CARTESIAN_POINT ( 'NONE',  ( -2.093983074874246508, -3.000000000000000444, 7.791781413346522633 ) ) ;
#35730 = CARTESIAN_POINT ( 'NONE',  ( -1.589967640018407291, -5.000000000000000888, -16.33917143506446124 ) ) ;
#35731 = CARTESIAN_POINT ( 'NONE',  ( -5.082755093536326818, -17.09375000204838813, 5.082755093536325042 ) ) ;
#35732 = VECTOR ( 'NONE', #42525, 1000.000000000000000 ) ;
#35733 = ADVANCED_FACE ( 'NONE', ( #22778 ), #62179, .T. ) ;
#35734 = CARTESIAN_POINT ( 'NONE',  ( 30.77329953030971765, 15.53171713056514491, -40.23250653748806371 ) ) ;
#35735 = MECHANICAL_DESIGN_GEOMETRIC_PRESENTATION_REPRESENTATION (  '', ( #30561 ), #9806 ) ;
#35736 = ORIENTED_EDGE ( 'NONE', *, *, #35753, .T. ) ;
#35737 = CARTESIAN_POINT ( 'NONE',  ( 81.74643333074975260, -46.44958790937922544, 169.1855094761081943 ) ) ;
#35738 = B_SPLINE_CURVE_WITH_KNOTS ( 'NONE', 3,
 ( #103794, #61777, #29937, #12648, #23298, #80962, #56133, #87103, #89078, #4580, #70379, #103274, #102205, #29424, #7078, #64793 ),
 .UNSPECIFIED., .F., .F.,
 ( 4, 2, 2, 2, 2, 2, 2, 4 ),
 ( 1.366913666845653131E-16, 0.001031042176150235266, 0.001546563264225255321, 0.002062084352300275810, 0.002577605440375296299, 0.003093126528450315920, 0.003608647616525335975, 0.004124168704600356464 ),
 .UNSPECIFIED. ) ;
#35739 = DIRECTION ( 'NONE',  ( 0.5735764363510557073, -0.8191520442889850262, 1.003171929053516612E-16 ) ) ;
#35740 = CIRCLE ( 'NONE', #1243, 4.000000000000000888 ) ;
#35741 = CARTESIAN_POINT ( 'NONE',  ( 56.96666666666666856, 6.915964383211875250E-15, 0.000000000000000000 ) ) ;
#35742 = ORIENTED_EDGE ( 'NONE', *, *, #21730, .F. ) ;
#35743 = CARTESIAN_POINT ( 'NONE',  ( 0.000000000000000000, -50.00000000000000000, 122.0000000000000000 ) ) ;
#35744 = CARTESIAN_POINT ( 'NONE',  ( -0.8337482156482161066, 18.10529858437485728, -49.56546807274770572 ) ) ;
#35745 = CARTESIAN_POINT ( 'NONE',  ( 38.81818101478957317, 27.31133193661636227, -12.26431571994239000 ) ) ;
#35746 = DIRECTION ( 'NONE',  ( -0.5735764363510494901, -0.8191520442889894671, 0.000000000000000000 ) ) ;
#35747 = CARTESIAN_POINT ( 'NONE',  ( -5.727189096784630173, 253.5786987524874405, -1.806430436190359368 ) ) ;
#35748 =( BOUNDED_SURFACE ( )  B_SPLINE_SURFACE ( 3, 2, ( 
 ( #10980, #87951, #101610 ),
 ( #30256, #102128, #63145 ),
 ( #85426, #47465, #60639 ),
 ( #97085, #96042, #5943 ),
 ( #39406, #104647, #77333 ),
 ( #38870, #85980, #63686 ),
 ( #76786, #2890, #27765 ),
 ( #44982, #77866, #3445 ),
 ( #36907, #55545, #36389 ),
 ( #102669, #69257, #72284 ),
 ( #31333, #94045, #28284 ),
 ( #64215, #61158, #53061 ),
 ( #73870, #32385, #105704 ),
 ( #32913, #58220, #65790 ),
 ( #90595, #33986, #81416 ),
 ( #8072, #65256, #15103 ),
 ( #82503, #64729, #99746 ),
 ( #49594, #47990, #33441 ),
 ( #7527, #89009, #97603 ),
 ( #106765, #91147, #72799 ),
 ( #106223, #8604, #41506 ),
 ( #89540, #98667, #98147 ),
 ( #50127, #24819, #17256 ),
 ( #74919, #16705, #66856 ),
 ( #73325, #40981, #1003 ),
 ( #40445, #80898, #74394 ),
 ( #57672, #90061, #23769 ),
 ( #473, #16165, #56617 ),
 ( #24299, #49052, #57148 ),
 ( #9127, #25915, #66315 ),
 ( #83036, #81948, #99197 ),
 ( #25360, #42037, #7007 ),
 ( #39927, #31847, #15632 ),
 ( #48525, #28030, #68456 ),
 ( #101348, #85160, #1560 ),
 ( #51717, #11248, #43109 ),
 ( #17783, #84097, #27503 ),
 ( #92174, #10719, #60378 ),
 ( #43635, #67912, #34524 ),
 ( #44177, #59302, #93253 ),
 ( #59841, #92713, #26437 ),
 ( #50635, #100799, #18873 ),
 ( #84632, #75997, #67393 ),
 ( #42566, #36126, #60899 ) ),
 .UNSPECIFIED., .F., .F., .F. ) 
 B_SPLINE_SURFACE_WITH_KNOTS ( ( 4, 2, 2, 2, 2, 2, 2, 2, 2, 2, 2, 2, 2, 2, 2, 2, 2, 2, 2, 2, 2, 4 ),
 ( 3, 3 ),
 ( 0.05136275451448887863, 0.06919263422628305071, 0.08702251393807722279, 0.1048523936498713949, 0.1137673335057684809, 0.1226822733616655670, 0.1315972132175626530, 0.1405121530734597390, 0.1583420327852539111, 0.1672569726411509972, 0.1717144425690995402, 0.1761719124970480832, 0.1784006474610223547, 0.1806293824249966262, 0.1828581173889708977, 0.1850868523529451692, 0.1862012198349323189, 0.1873155873169194408, 0.1884299547989065626, 0.1895443222808937123, 0.1917730572448679838, 0.1940017922088422553 ),
 ( 0.000000000000000000, 1.000000000000000000 ),
 .UNSPECIFIED. ) 
 GEOMETRIC_REPRESENTATION_ITEM ( )  RATIONAL_B_SPLINE_SURFACE ( (
 ( 1.000000000000000000, 0.7071066982518089405, 1.000000000000000000),
 ( 1.000000000000000000, 0.7071066243399852791, 1.000000000000000000),
 ( 1.000000000000000000, 0.7071067817164773395, 1.000000000000000000),
 ( 1.000000000000000000, 0.7071067817164773395, 1.000000000000000000),
 ( 1.000000000000000000, 0.7071067820464573828, 1.000000000000000000),
 ( 1.000000000000000000, 0.7071067820464573828, 1.000000000000000000),
 ( 1.000000000000000000, 0.7071085455477897908, 1.000000000000000000),
 ( 1.000000000000000000, 0.7071090295291238004, 1.000000000000000000),
 ( 1.000000000000000000, 0.7071083385704458601, 1.000000000000000000),
 ( 1.000000000000000000, 0.7071068389492060069, 1.000000000000000000),
 ( 1.000000000000000000, 0.7071066205750288214, 1.000000000000000000),
 ( 1.000000000000000000, 0.7071083160947816415, 1.000000000000000000),
 ( 1.000000000000000000, 0.7071093954417188021, 1.000000000000000000),
 ( 1.000000000000000000, 0.7071094620417358589, 1.000000000000000000),
 ( 1.000000000000000000, 0.7071083849275382471, 1.000000000000000000),
 ( 1.000000000000000000, 0.7071056411300526978, 1.000000000000000000),
 ( 1.000000000000000000, 0.7070875072514104520, 1.000000000000000000),
 ( 1.000000000000000000, 0.7071202496626299849, 1.000000000000000000),
 ( 1.000000000000000000, 0.7071338852168149725, 1.000000000000000000),
 ( 1.000000000000000000, 0.7071095136704249606, 1.000000000000000000),
 ( 1.000000000000000000, 0.7071065123001155639, 1.000000000000000000),
 ( 1.000000000000000000, 0.7071128202845421429, 1.000000000000000000),
 ( 1.000000000000000000, 0.7071080869018205872, 1.000000000000000000),
 ( 1.000000000000000000, 0.7071063200084551914, 1.000000000000000000),
 ( 1.000000000000000000, 0.7071396742970895710, 1.000000000000000000),
 ( 1.000000000000000000, 0.7071960107269280593, 1.000000000000000000),
 ( 1.000000000000000000, 0.7072035974108880074, 1.000000000000000000),
 ( 1.000000000000000000, 0.7071532259081326766, 1.000000000000000000),
 ( 1.000000000000000000, 0.7071047821262952393, 1.000000000000000000),
 ( 1.000000000000000000, 0.7071096296259671288, 1.000000000000000000),
 ( 1.000000000000000000, 0.7071125913011165887, 1.000000000000000000),
 ( 1.000000000000000000, 0.7071062656804929514, 1.000000000000000000),
 ( 1.000000000000000000, 0.7071058024559618849, 1.000000000000000000),
 ( 1.000000000000000000, 0.7071001851375554592, 1.000000000000000000),
 ( 1.000000000000000000, 0.7070990685193431213, 1.000000000000000000),
 ( 1.000000000000000000, 0.7071030088798048174, 1.000000000000000000),
 ( 1.000000000000000000, 0.7071042265699299945, 1.000000000000000000),
 ( 1.000000000000000000, 0.7071104316389814626, 1.000000000000000000),
 ( 1.000000000000000000, 0.7071217845162482973, 1.000000000000000000),
 ( 1.000000000000000000, 0.7071252912931403900, 1.000000000000000000),
 ( 1.000000000000000000, 0.7071009329475237415, 1.000000000000000000),
 ( 1.000000000000000000, 0.7071402609100536640, 1.000000000000000000),
 ( 1.000000000000000000, 0.7071206810161836387, 1.000000000000000000),
 ( 1.000000000000000000, 0.7071067811865464625, 1.000000000000000000) ) ) 
 REPRESENTATION_ITEM ( '' )  SURFACE ( )  );
#35749 = CARTESIAN_POINT ( 'NONE',  ( 1.167749971007850274, 14.75947676340571313, 50.96289688649348193 ) ) ;
#35750 = CARTESIAN_POINT ( 'NONE',  ( 8.439582558336111262, -0.2091310867994085887, 19.51128387820496002 ) ) ;
#35751 = ORIENTED_EDGE ( 'NONE', *, *, #88011, .F. ) ;
#35752 = FILL_AREA_STYLE_COLOUR ( '', #91894 ) ;
#35753 = EDGE_CURVE ( 'NONE', #68586, #100942, #23430, .T. ) ;
#35754 =( GEOMETRIC_REPRESENTATION_CONTEXT ( 3 ) GLOBAL_UNCERTAINTY_ASSIGNED_CONTEXT ( ( #19269 ) ) GLOBAL_UNIT_ASSIGNED_CONTEXT ( ( #67332, #102341, #101290 ) ) REPRESENTATION_CONTEXT ( 'NONE', 'WORKASPACE' ) );
#35755 = CONICAL_SURFACE ( 'NONE', #92519, 4.000000000000001776, 0.9599310885968808105 ) ;
#35756 = FACE_OUTER_BOUND ( 'NONE', #80255, .T. ) ;
#35757 = CARTESIAN_POINT ( 'NONE',  ( 87.19375473865754600, -31.68694345013608427, 187.9059264421138948 ) ) ;
#35758 = EDGE_CURVE ( 'NONE', #5970, #78368, #5825, .T. ) ;
#35759 = LINE ( 'NONE', #45420, #98183 ) ;
#35760 = ADVANCED_FACE ( 'NONE', ( #97156 ), #105263, .F. ) ;
#35761 = CARTESIAN_POINT ( 'NONE',  ( 7.188101187499999156, -23.75000000204839168, 2.977408999572654924 ) ) ;
#35762 = AXIS2_PLACEMENT_3D ( 'NONE', #51065, #43002, #892 ) ;
#35763 = COLOUR_RGB ( '', 0.08235294, 0.09019608, 0.10196078) ;
#35764 = CARTESIAN_POINT ( 'NONE',  ( -42.44022245594207732, 488.6041665467083135, 9.766690314390181982 ) ) ;
#35765 = CIRCLE ( 'NONE', #101164, 4.250000000000000000 ) ;
#35766 = AXIS2_PLACEMENT_3D ( 'NONE', #43869, #76762, #59542 ) ;
#35767 = DIRECTION ( 'NONE',  ( 0.000000000000000000, 0.000000000000000000, -1.000000000000000000 ) ) ;
#35768 = FACE_OUTER_BOUND ( 'NONE', #14427, .T. ) ;
#35769 = ORIENTED_EDGE ( 'NONE', *, *, #14896, .F. ) ;
#35770 = CARTESIAN_POINT ( 'NONE',  ( 40.81956795959206374, 485.7841149218990040, -4.786840289929677361 ) ) ;
#35771 = EDGE_CURVE ( 'NONE', #48969, #62332, #69838, .T. ) ;
#35772 = SURFACE_SIDE_STYLE ('',( #2816 ) ) ;
#35773 = CARTESIAN_POINT ( 'NONE',  ( -9.999497344909480390, 7.500719060593830534, 0.000000000000000000 ) ) ;
#35774 = AXIS2_PLACEMENT_3D ( 'NONE', #33920, #2974, #4584 ) ;
#35775 = VERTEX_POINT ( 'NONE', #21201 ) ;
#35776 = FACE_BOUND ( 'NONE', #39892, .T. ) ;
#35777 =( NAMED_UNIT ( * ) PLANE_ANGLE_UNIT ( ) SI_UNIT ( $, .RADIAN. ) );
#35778 = ORIENTED_EDGE ( 'NONE', *, *, #61347, .T. ) ;
#35779 = FACE_OUTER_BOUND ( 'NONE', #92126, .T. ) ;
#35780 = CYLINDRICAL_SURFACE ( 'NONE', #60484, 1.249999999999999778 ) ;
#35781 = CARTESIAN_POINT ( 'NONE',  ( 9.482856158761270748, 102.5569288414527875, 3.177891129109652546 ) ) ;
#35782 = CARTESIAN_POINT ( 'NONE',  ( -16.91846161659832859, 36.35180932965544542, 24.29864124313478868 ) ) ;
#35783 = CARTESIAN_POINT ( 'NONE',  ( -99.64086268788143741, -60.00000000000001421, 202.0020366782889880 ) ) ;
#35784 = CARTESIAN_POINT ( 'NONE',  ( 19.50000000000223466, 49.99999999999952394, 59.71562975593440115 ) ) ;
#35785 = CARTESIAN_POINT ( 'NONE',  ( -45.29905483467455696, 497.0732240353902398, -8.041250874568902418 ) ) ;
#35786 = DIRECTION ( 'NONE',  ( -0.000000000000000000, -0.000000000000000000, -1.000000000000000000 ) ) ;
#35787 = AXIS2_PLACEMENT_3D ( 'NONE', #99862, #90719, #26035 ) ;
#35788 = CARTESIAN_POINT ( 'NONE',  ( -85.30085673280602521, -35.74314973840716192, 182.5942498631214050 ) ) ;
#35789 = CIRCLE ( 'NONE', #18524, 46.61112130868859538 ) ;
#35790 = ORIENTED_EDGE ( 'NONE', *, *, #52053, .T. ) ;
#35791 = DIRECTION ( 'NONE',  ( 0.000000000000000000, 1.000000000000000000, 0.000000000000000000 ) ) ;
#35792 = DIRECTION ( 'NONE',  ( 0.000000000000000000, 0.000000000000000000, -1.000000000000000000 ) ) ;
#35793 = CARTESIAN_POINT ( 'NONE',  ( -82.61673979528575273, -37.83313480826174668, 4.882814718300323875 ) ) ;
#35794 = SURFACE_SIDE_STYLE ('',( #42238 ) ) ;
#35795 = CARTESIAN_POINT ( 'NONE',  ( 12.33349330513380337, 4.000000000000002665, 0.000000000000000000 ) ) ;
#35796 = CARTESIAN_POINT ( 'NONE',  ( -13.50676536913941028, -9.130490673981565664, 11.91195374128086115 ) ) ;
#35797 = CARTESIAN_POINT ( 'NONE',  ( -5.983613182656017493, -12.98062839397022294, 13.15810238988803071 ) ) ;
#35798 = CARTESIAN_POINT ( 'NONE',  ( -1.905220702120325443E-14, 42.00000000000000711, -59.23741894013591036 ) ) ;
#35799 = AXIS2_PLACEMENT_3D ( 'NONE', #34882, #60741, #67750 ) ;
#35800 = CARTESIAN_POINT ( 'NONE',  ( 77.87328754808491738, -14.21045842199420228, 157.7472683744473159 ) ) ;
#35801 = ADVANCED_FACE ( 'NONE', ( #89084 ), #25123, .T. ) ;
#35802 = CARTESIAN_POINT ( 'NONE',  ( -89.52600508066183238, -29.99999999999992539, 22.05060892610427814 ) ) ;
#35803 = CARTESIAN_POINT ( 'NONE',  ( -71.71757422039344476, -29.06626939408458554, 101.3046069043710560 ) ) ;
#35804 = ORIENTED_EDGE ( 'NONE', *, *, #27636, .T. ) ;
#35805 = CARTESIAN_POINT ( 'NONE',  ( 81.10520000301197285, -14.21045842199436926, 192.6066858413676925 ) ) ;
#35806 = CARTESIAN_POINT ( 'NONE',  ( 62.84401523694076275, 40.83901776069048850, -16.86776260340353062 ) ) ;
#35807 = CARTESIAN_POINT ( 'NONE',  ( 27.27612554697342517, -60.00000000000986233, 44.35091487113613340 ) ) ;
#35808 = ORIENTED_EDGE ( 'NONE', *, *, #64692, .T. ) ;
#35809 = CARTESIAN_POINT ( 'NONE',  ( 7.561403392358007736, 52.15275433178552333, -2.010202227193783830 ) ) ;
#35810 = CARTESIAN_POINT ( 'NONE',  ( 7.188101187499999156, -25.62500000204838813, 2.977408999572654924 ) ) ;
#35811 = DIRECTION ( 'NONE',  ( 1.000000000000000000, 0.000000000000000000, -0.000000000000000000 ) ) ;
#35812 = ORIENTED_EDGE ( 'NONE', *, *, #55486, .T. ) ;
#35814 = DIRECTION ( 'NONE',  ( -1.000000000000000000, 0.000000000000000000, 0.000000000000000000 ) ) ;
#35813 = CONICAL_SURFACE ( 'NONE', #80561, 4.250000000000000000, 0.9599310885968754814 ) ;
#35815 = ORIENTED_EDGE ( 'NONE', *, *, #43391, .F. ) ;
#35816 = CARTESIAN_POINT ( 'NONE',  ( 8.169585525225409484, 41.99999999999999289, -72.41994148081866456 ) ) ;
#35817 = CARTESIAN_POINT ( 'NONE',  ( -70.42324668238815377, -59.99999999998043876, 160.4961440857183277 ) ) ;
#35818 = CARTESIAN_POINT ( 'NONE',  ( 25.36273202697566020, 305.2221405902974425, -9.701703692503940601 ) ) ;
#35819 = CARTESIAN_POINT ( 'NONE',  ( -7.188101187500001821, -11.00000000204838635, -2.977408999572651371 ) ) ;
#35820 = CARTESIAN_POINT ( 'NONE',  ( -49.26989972136284024, 12.96118195421251507, 15.76560135797571505 ) ) ;
#35822 = B_SPLINE_CURVE_WITH_KNOTS ( 'NONE', 3,
 ( #13212, #37549, #103313, #87666, #5667, #79028, #65889, #71454, #57779, #21358, #104353, #29460, #5147, #65364, #38080, #70936 ),
 .UNSPECIFIED., .F., .F.,
 ( 4, 2, 2, 2, 2, 2, 2, 4 ),
 ( 7.757919228897728493E-18, 0.001041806880168140350, 0.001562710320252229824, 0.002083613760336319298, 0.002604517200420408338, 0.003125420640504497811, 0.003646324080588587285, 0.004167227520672676759 ),
 .UNSPECIFIED. ) ;
#35821 = PLANE ( 'NONE',  #98092 ) ;
#35823 = SURFACE_STYLE_USAGE ( .BOTH. , #61130 ) ;
#35824 = CARTESIAN_POINT ( 'NONE',  ( 10.48543666094595217, 50.00000000000000000, -78.95657223723276275 ) ) ;
#35825 = CARTESIAN_POINT ( 'NONE',  ( -12.40258157393384764, -4.192292395472819955, -12.98887677823726960 ) ) ;
#35826 = UNCERTAINTY_MEASURE_WITH_UNIT (LENGTH_MEASURE( 1.000000000000000082E-05 ), #40720, 'distance_accuracy_value', 'NONE');
#35827 = ORIENTED_EDGE ( 'NONE', *, *, #65444, .F. ) ;
#35828 = CIRCLE ( 'NONE', #61605, 8.000000000000000000 ) ;
#35829 = AXIS2_PLACEMENT_3D ( 'NONE', #92249, #76074, #18403 ) ;
#35831 = CARTESIAN_POINT ( 'NONE',  ( 31.63731285819285688, -39.48887728662363372, 33.75230942950094715 ) ) ;
#35830 = CARTESIAN_POINT ( 'NONE',  ( -3.350247031702008993, -48.92879585575168022, 104.4269854689288053 ) ) ;
#35832 = PRESENTATION_STYLE_ASSIGNMENT (( #35287 ) ) ;
#35833 = ORIENTED_EDGE ( 'NONE', *, *, #17963, .F. ) ;
#35834 = CARTESIAN_POINT ( 'NONE',  ( -42.79777464980524826, 484.2777864412636291, -1.379167304946371964 ) ) ;
#35836 = CARTESIAN_POINT ( 'NONE',  ( 81.26467260280679739, -5.000000000000000000, 0.000000000000000000 ) ) ;
#35835 = CARTESIAN_POINT ( 'NONE',  ( -2.100000000000004530, 0.000000000000000000, 0.000000000000000000 ) ) ;
#35837 = AXIS2_PLACEMENT_3D ( 'NONE', #37900, #84824, #44912 ) ;
#35838 = CARTESIAN_POINT ( 'NONE',  ( 0.000000000000000000, -30.00000000000000000, 0.000000000000000000 ) ) ;
#35839 = CARTESIAN_POINT ( 'NONE',  ( -43.68138489372817901, 484.4283016034073057, 2.027755642628957578 ) ) ;
#35840 = PRESENTATION_LAYER_ASSIGNMENT (  '', '', ( #15071 ) ) ;
#35841 = CIRCLE ( 'NONE', #18656, 4.000000000000000000 ) ;
#35842 = CARTESIAN_POINT ( 'NONE',  ( 100.6222222222222200, -4.171999999999998820, 5.616230220889773285E-16 ) ) ;
#35843 = CARTESIAN_POINT ( 'NONE',  ( -35.52386467438594764, 464.2380653034055058, 19.26634992204778030 ) ) ;
#35844 = VERTEX_POINT ( 'NONE', #37910 ) ;
#35845 = EDGE_CURVE ( 'NONE', #15190, #62284, #44054, .T. ) ;
#35846 = CARTESIAN_POINT ( 'NONE',  ( 91.86088825387464851, -60.00000000000000711, 13.72134700691805698 ) ) ;
#35847 = DIRECTION ( 'NONE',  ( -1.000000000000000000, 0.000000000000000000, 0.000000000000000000 ) ) ;
#35848 = CARTESIAN_POINT ( 'NONE',  ( 16.64348903516523848, -1.200000000000000030E-05, 5.407797401561420969 ) ) ;
#35849 = CARTESIAN_POINT ( 'NONE',  ( 48.10000000000000142, 4.052968581778165278E-16, -3.309499999999999886 ) ) ;
#35850 = EDGE_CURVE ( 'NONE', #105782, #74189, #64799, .T. ) ;
#35851 = CARTESIAN_POINT ( 'NONE',  ( -6.836424185777212337, 40.92324829897224703, -70.97025588718011591 ) ) ;
#35852 = DIRECTION ( 'NONE',  ( -0.000000000000000000, 1.000000000000000000, -0.000000000000000000 ) ) ;
#35853 = VERTEX_POINT ( 'NONE', #73941 ) ;
#35854 = CIRCLE ( 'NONE', #96095, 5.000000000000000000 ) ;
#35855 = CARTESIAN_POINT ( 'NONE',  ( -109.5118039930968052, -30.00000000000000000, 177.2736533842592621 ) ) ;
#35856 = ORIENTED_EDGE ( 'NONE', *, *, #29608, .F. ) ;
#35857 = CARTESIAN_POINT ( 'NONE',  ( 0.000000000000000000, -30.00000000000000000, 0.000000000000000000 ) ) ;
#35858 = SURFACE_STYLE_FILL_AREA ( #27236 ) ;
#35859 = FACE_OUTER_BOUND ( 'NONE', #97815, .T. ) ;
#35860 = CARTESIAN_POINT ( 'NONE',  ( 11.08349330513380515, -4.000000000000000000, 4.898587196589415787E-16 ) ) ;
#35861 = CARTESIAN_POINT ( 'NONE',  ( 84.04211440375647157, -45.27896428354746661, -11.65066557963491967 ) ) ;
#35862 = CARTESIAN_POINT ( 'NONE',  ( -33.58551248210795848, 315.8335180326819795, -6.885581302250129987 ) ) ;
#35863 = CARTESIAN_POINT ( 'NONE',  ( -1.496989374907284246E-10, 304.8518027762757470, -10.00000000000000533 ) ) ;
#35864 = CARTESIAN_POINT ( 'NONE',  ( -18.03527632919914581, 45.00000000000000711, 62.54344397016589596 ) ) ;
#35865 = FACE_OUTER_BOUND ( 'NONE', #8846, .T. ) ;
#35866 = ORIENTED_EDGE ( 'NONE', *, *, #35470, .T. ) ;
#35867 = CARTESIAN_POINT ( 'NONE',  ( -42.80674476975001852, 434.8200572689409000, 17.89667068453010046 ) ) ;
#35868 = VERTEX_POINT ( 'NONE', #99817 ) ;
#35869 = CIRCLE ( 'NONE', #101270, 61.50000000000000000 ) ;
#35870 = CARTESIAN_POINT ( 'NONE',  ( 49.27018817646321480, 7.792903869376768711, -15.76322754694156281 ) ) ;
#35871 = CIRCLE ( 'NONE', #13399, 5.000000000000011546 ) ;
#35873 = ORIENTED_EDGE ( 'NONE', *, *, #56279, .F. ) ;
#35872 = CARTESIAN_POINT ( 'NONE',  ( 5.454359399073367420, 52.03812987433942538, 6.039366617364852807 ) ) ;
#35874 = CARTESIAN_POINT ( 'NONE',  ( 76.67219034576102388, -32.54950668678723957, 122.5186054704328882 ) ) ;
#35875 = ORIENTED_EDGE ( 'NONE', *, *, #62328, .T. ) ;
#35876 = CARTESIAN_POINT ( 'NONE',  ( 3.552225580476869649, -53.17955991417163375, 40.54727264511482332 ) ) ;
#35877 = CARTESIAN_POINT ( 'NONE',  ( 12.13034742782427955, 41.99999999999999289, -93.82352941176471006 ) ) ;
#35878 = CARTESIAN_POINT ( 'NONE',  ( 5.082755093536324154, -25.34375000204838813, 5.082755093536326818 ) ) ;
#35879 = CARTESIAN_POINT ( 'NONE',  ( -102.4013124767651135, -57.63331223797548120, 203.1247769353137755 ) ) ;
#35880 = ORIENTED_EDGE ( 'NONE', *, *, #39193, .T. ) ;
#35881 =( LENGTH_UNIT ( ) NAMED_UNIT ( * ) SI_UNIT ( .MILLI., .METRE. ) );
#35882 = B_SPLINE_CURVE_WITH_KNOTS ( 'NONE', 3,
 ( #5243, #97406, #6273, #64025 ),
 .UNSPECIFIED., .F., .F.,
 ( 4, 4 ),
 ( 0.000000000000000000, 1.000000000000000000 ),
 .UNSPECIFIED. ) ;
#35883 =( LENGTH_UNIT ( ) NAMED_UNIT ( * ) SI_UNIT ( .MILLI., .METRE. ) );
#35884 = AXIS2_PLACEMENT_3D ( 'NONE', #86035, #60690, #19727 ) ;
#35885 = CARTESIAN_POINT ( 'NONE',  ( 104.2870107326527034, -52.71696054412868193, 185.3521057339551135 ) ) ;
#35886 = AXIS2_PLACEMENT_3D ( 'NONE', #33963, #41483, #91124 ) ;
#35887 = CARTESIAN_POINT ( 'NONE',  ( -36.58618025929193607, 27.99671736784095799, -12.99775655248998874 ) ) ;
#35888 = CARTESIAN_POINT ( 'NONE',  ( 0.2916160024871935486, -70.53271932724192084, 13.00000000000000000 ) ) ;
#35889 = CARTESIAN_POINT ( 'NONE',  ( -1.469576158976823947E-15, -16.06250000409677270, 8.000000000000000000 ) ) ;
#35890 = CARTESIAN_POINT ( 'NONE',  ( -50.73617477660454966, -29.81564531741702595, 47.82844993627990249 ) ) ;
#35891 = CARTESIAN_POINT ( 'NONE',  ( -3.857142857142850989, -1.200583151104938517, 103.1763305333244318 ) ) ;
#35892 = CIRCLE ( 'NONE', #39327, 4.000000000000001776 ) ;
#35893 = AXIS2_PLACEMENT_3D ( 'NONE', #62143, #95542, #28724 ) ;
#35894 = CARTESIAN_POINT ( 'NONE',  ( 34.35000000000000142, 1.533819458162526451E-15, 0.000000000000000000 ) ) ;
#35895 = CARTESIAN_POINT ( 'NONE',  ( -43.66729043033831914, 435.6676719292337907, 17.39374879622100423 ) ) ;
#35896 = DIRECTION ( 'NONE',  ( 1.000000000000000000, 6.989781874810890086E-17, -5.620325286447034103E-17 ) ) ;
#35897 = CARTESIAN_POINT ( 'NONE',  ( 5.936373709703198998, -30.00000000000001066, -4.453514806643029011 ) ) ;
#35898 = EDGE_LOOP ( 'NONE', ( #42799, #16524, #93342, #79795 ) ) ;
#35899 = CARTESIAN_POINT ( 'NONE',  ( -2.757402973851224903, -49.69848065189508191, 40.86068941039670221 ) ) ;
#35900 = LINE ( 'NONE', #86562, #80185 ) ;
#35901 = EDGE_CURVE ( 'NONE', #39684, #106458, #66388, .T. ) ;
#35902 = CARTESIAN_POINT ( 'NONE',  ( 8.455951367436818379E-15, 13.70447791526914294, 49.24999999999998579 ) ) ;
#35903 = CARTESIAN_POINT ( 'NONE',  ( -87.46766941343894075, -30.00000000000000000, 185.3710213780722427 ) ) ;
#35904 = EDGE_CURVE ( 'NONE', #11120, #30663, #19989, .T. ) ;
#35905 = VERTEX_POINT ( 'NONE', #8151 ) ;
#35906 = CYLINDRICAL_SURFACE ( 'NONE', #9962, 24.55262289886175964 ) ;
#35907 = AXIS2_PLACEMENT_3D ( 'NONE', #82185, #63915, #8303 ) ;
#35908 = CARTESIAN_POINT ( 'NONE',  ( 86.15165790503920107, -57.57631507345369926, 202.7687108331410286 ) ) ;
#35909 = CONICAL_SURFACE ( 'NONE', #8284, 3.309500000000001663, 0.9599310885968770357 ) ;
#35910 = ADVANCED_FACE ( 'NONE', ( #31923, #49669, #41585, #16240, #97684 ), #23359, .T. ) ;
#35912 = CARTESIAN_POINT ( 'NONE',  ( 30.11650669486618881, 1.474610560812782335E-15, 0.000000000000000000 ) ) ;
#35911 = CARTESIAN_POINT ( 'NONE',  ( -14.90069340504740758, 2.164550790749281362, 1.672538227389957166 ) ) ;
#35913 = CARTESIAN_POINT ( 'NONE',  ( 67.49251172716176939, -38.07658496841629869, -32.03956923833649029 ) ) ;
#35914 = CARTESIAN_POINT ( 'NONE',  ( -15.72426027928782588, 22.05433369633805896, -3.882282778265964129 ) ) ;
#35915 = DIRECTION ( 'NONE',  ( -0.000000000000000000, -1.000000000000000000, -0.000000000000000000 ) ) ;
#35916 = CARTESIAN_POINT ( 'NONE',  ( -65.63516414262727494, -59.99999999999999289, 120.8879485127422129 ) ) ;
#35917 = AXIS2_PLACEMENT_3D ( 'NONE', #79341, #104678, #53485 ) ;
#35918 = DIRECTION ( 'NONE',  ( 0.000000000000000000, 0.000000000000000000, 1.000000000000000000 ) ) ;
#35919 =( LENGTH_UNIT ( ) NAMED_UNIT ( * ) SI_UNIT ( .MILLI., .METRE. ) );
#35920 = CARTESIAN_POINT ( 'NONE',  ( -84.61161887829497630, -61.08739850468023036, 193.0979379198380173 ) ) ;
#35921 = EDGE_LOOP ( 'NONE', ( #33557, #65333, #82625, #29178 ) ) ;
#35922 = CARTESIAN_POINT ( 'NONE',  ( 30.93371285580988328, 14.00361151752279198, 40.91601221254699539 ) ) ;
#35923 = CARTESIAN_POINT ( 'NONE',  ( -4.963955403123392784, -18.58604024885853434, 26.97813512196605856 ) ) ;
#35924 = CARTESIAN_POINT ( 'NONE',  ( -6.738100187484505454, 41.71798639774085160, -59.05424569925489209 ) ) ;
#35925 = CARTESIAN_POINT ( 'NONE',  ( 5.007715329123895321E-16, -7.505553499465175804, -6.064240316920414209 ) ) ;
#35927 = CARTESIAN_POINT ( 'NONE',  ( -7.561790601661408928, 54.28098289519358843, 2.010020282033269989 ) ) ;
#35926 = CARTESIAN_POINT ( 'NONE',  ( -30.32981733298740323, 298.1626997294918056, 2.667535392438074915 ) ) ;
#35928 = ORIENTED_EDGE ( 'NONE', *, *, #98743, .F. ) ;
#35929 =( NAMED_UNIT ( * ) PLANE_ANGLE_UNIT ( ) SI_UNIT ( $, .RADIAN. ) );
#35930 = LINE ( 'NONE', #53136, #64985 ) ;
#35931 = CIRCLE ( 'NONE', #77234, 1.000000000000002220 ) ;
#35932 = DIRECTION ( 'NONE',  ( -1.000000000000000000, -1.224606353822377258E-16, -0.000000000000000000 ) ) ;
#35933 = CARTESIAN_POINT ( 'NONE',  ( -30.59731729458119531, 7.793314453875768599, -41.71112871039140657 ) ) ;
#35934 = CARTESIAN_POINT ( 'NONE',  ( 25.99908587619278322, 295.9244531611905700, -1.769008014947292429 ) ) ;
#35935 = CARTESIAN_POINT ( 'NONE',  ( 32.16694665535142406, 298.7751107022914425, -9.134474995493537364 ) ) ;
#35936 = EDGE_CURVE ( 'NONE', #96494, #2234, #74468, .T. ) ;
#35937 = AXIS2_PLACEMENT_3D ( 'NONE', #5416, #86881, #38339 ) ;
#35938 = CARTESIAN_POINT ( 'NONE',  ( 94.85921371064608820, -60.00000000000004263, 26.66736809083038651 ) ) ;
#35939 = B_SPLINE_CURVE_WITH_KNOTS ( 'NONE', 3,
 ( #70064, #79212, #40740, #87319, #12345, #71636, #94353, #102965, #71120, #78666, #45271, #22064, #45787, #54923, #13398, #21540, #20516, #37739, #104546, #5336, #63039, #14457, #70600, #47368, #46842, #38259, #87849, #104009, #53351, #103492 ),
 .UNSPECIFIED., .F., .F.,
 ( 4, 2, 2, 2, 2, 2, 2, 2, 2, 2, 2, 2, 2, 2, 4 ),
 ( 0.01009607051181185544, 0.01101525429224261762, 0.01193443807267337807, 0.01285362185310414025, 0.01377280563353490243, 0.01423239752375028352, 0.01446219346885797494, 0.01469198941396566288, 0.01492178535907335256, 0.01515158130418104224, 0.01538137724928873018, 0.01561117319439641812, 0.01607076508461179054, 0.01653035697482716296, 0.01744954075525791126 ),
 .UNSPECIFIED. ) ;
#35940 = CARTESIAN_POINT ( 'NONE',  ( -78.78664253753292712, -53.37736891008503903, 153.4667062920331659 ) ) ;
#35941 = ORIENTED_EDGE ( 'NONE', *, *, #1677, .T. ) ;
#35942 = SURFACE_STYLE_USAGE ( .BOTH. , #86601 ) ;
#35943 = DIRECTION ( 'NONE',  ( -0.000000000000000000, 1.000000000000000000, -0.000000000000000000 ) ) ;
#35944 = CARTESIAN_POINT ( 'NONE',  ( 50.82724289091086689, -57.67763088439131280, 79.42815591981056400 ) ) ;
#35945 = DIRECTION ( 'NONE',  ( -1.000000000000000000, -0.000000000000000000, -0.000000000000000000 ) ) ;
#35947 = AXIS2_PLACEMENT_3D ( 'NONE', #86770, #71087, #70571 ) ;
#35946 = CARTESIAN_POINT ( 'NONE',  ( 44.90265637069953186, 347.4290076447818478, 2.367369570399655565 ) ) ;
#35948 = DIRECTION ( 'NONE',  ( 0.000000000000000000, -1.000000000000000000, 0.000000000000000000 ) ) ;
#35949 = ORIENTED_EDGE ( 'NONE', *, *, #45516, .F. ) ;
#35950 = CARTESIAN_POINT ( 'NONE',  ( 4.512020406555891761, 54.30832494546023526, -6.299191669131390725 ) ) ;
#35951 = CARTESIAN_POINT ( 'NONE',  ( 31.50721393268916870, 439.7147443804711315, 23.57029083728580687 ) ) ;
#35952 = CARTESIAN_POINT ( 'NONE',  ( 5.082755093536324154, -32.84375000204838813, 5.082755093536326818 ) ) ;
#35953 = ORIENTED_EDGE ( 'NONE', *, *, #4748, .T. ) ;
#35954 = SURFACE_STYLE_USAGE ( .BOTH. , #34875 ) ;
#35955 = DIRECTION ( 'NONE',  ( 0.000000000000000000, 0.000000000000000000, 1.000000000000000000 ) ) ;
#35956 = CARTESIAN_POINT ( 'NONE',  ( 5.308064239167483933, 41.67430808361707761, -70.56675995020941627 ) ) ;
#35957 = ADVANCED_FACE ( 'NONE', ( #65334 ), #78448, .T. ) ;
#35958 = CARTESIAN_POINT ( 'NONE',  ( -5.774137037018697960, 50.00000000000000000, 63.00000000000000000 ) ) ;
#35959 = CARTESIAN_POINT ( 'NONE',  ( -30.00000000000000000, 450.0000000000002274, 8.202422573753707979 ) ) ;
#35961 = CARTESIAN_POINT ( 'NONE',  ( -23.55048488053928324, 27.32134238698565554, -33.17259636481922769 ) ) ;
#35960 =( GEOMETRIC_REPRESENTATION_CONTEXT ( 3 ) GLOBAL_UNCERTAINTY_ASSIGNED_CONTEXT ( ( #43488 ) ) GLOBAL_UNIT_ASSIGNED_CONTEXT ( ( #78700, #86832, #7332 ) ) REPRESENTATION_CONTEXT ( 'NONE', 'WORKASPACE' ) );
#35962 = ORIENTED_EDGE ( 'NONE', *, *, #78940, .F. ) ;
#35963 = CARTESIAN_POINT ( 'NONE',  ( 36.03932222122800511, -60.00000000000000000, -40.18715066664060487 ) ) ;
#35965 = CARTESIAN_POINT ( 'NONE',  ( 19.82456495684694531, -25.55224884438233701, 28.62604876544009969 ) ) ;
#35964 = CARTESIAN_POINT ( 'NONE',  ( -64.82027869498183748, -30.00000000000004619, 107.4038593739741430 ) ) ;
#35966 = CARTESIAN_POINT ( 'NONE',  ( 8.176795461013406112E-15, 46.03420836107012093, -33.38430095398285147 ) ) ;
#35967 = TOROIDAL_SURFACE ( 'NONE', #46235, 8.499999999999992895, 0.5000000000000000000 ) ;
#35968 = CARTESIAN_POINT ( 'NONE',  ( -38.48681241573974887, -25.68051362833467977, 34.55373408003233493 ) ) ;
#35969 = VERTEX_POINT ( 'NONE', #9200 ) ;
#35970 = CARTESIAN_POINT ( 'NONE',  ( -16.66764709352488083, -4.285714285714295357, 19.00223544648543950 ) ) ;
#35971 = FACE_BOUND ( 'NONE', #20733, .T. ) ;
#35972 = CARTESIAN_POINT ( 'NONE',  ( -13.48739679499482058, -55.04004794677399559, 23.24594036347893677 ) ) ;
#35973 = CIRCLE ( 'NONE', #44321, 1.000000000000000666 ) ;
#35974 = CARTESIAN_POINT ( 'NONE',  ( 7.896165657598945842, -61.21088868628029900, -1.307894402814547385 ) ) ;
#35975 = VERTEX_POINT ( 'NONE', #32991 ) ;
#35976 = FACE_OUTER_BOUND ( 'NONE', #29055, .T. ) ;
#35977 = EDGE_CURVE ( 'NONE', #67283, #83820, #98222, .T. ) ;
#35978 = CIRCLE ( 'NONE', #56620, 4.250000000000000000 ) ;
#35979 = VERTEX_POINT ( 'NONE', #22 ) ;
#35980 = CARTESIAN_POINT ( 'NONE',  ( 97.98091450867445928, -29.99999999999992184, 190.5507201259314627 ) ) ;
#35981 = CARTESIAN_POINT ( 'NONE',  ( 48.49756656482988859, 39.00440506456347123, -41.54750411436693014 ) ) ;
#35982 = CARTESIAN_POINT ( 'NONE',  ( -4.905018583967755141, -82.97640014320325008, -3.459768807258293055 ) ) ;
#35983 = CARTESIAN_POINT ( 'NONE',  ( 80.94547152824299019, -30.00000000000000000, 20.01427389387851719 ) ) ;
#35984 = ADVANCED_FACE ( 'NONE', ( #42111 ), #81485, .T. ) ;
#35985 = ORIENTED_EDGE ( 'NONE', *, *, #69952, .F. ) ;
#35986 = ORIENTED_EDGE ( 'NONE', *, *, #83081, .F. ) ;
#35987 = ORIENTED_EDGE ( 'NONE', *, *, #59664, .T. ) ;
#35988 =( GEOMETRIC_REPRESENTATION_CONTEXT ( 3 ) GLOBAL_UNCERTAINTY_ASSIGNED_CONTEXT ( ( #93638 ) ) GLOBAL_UNIT_ASSIGNED_CONTEXT ( ( #32748, #32205, #17613 ) ) REPRESENTATION_CONTEXT ( 'NONE', 'WORKASPACE' ) );
#35989 = CARTESIAN_POINT ( 'NONE',  ( -47.50656546823834958, 12.72630541683655458, -14.46671989142072512 ) ) ;
#35990 = SURFACE_STYLE_FILL_AREA ( #18735 ) ;
#35991 = FACE_OUTER_BOUND ( 'NONE', #102834, .T. ) ;
#35992 = ADVANCED_FACE ( 'NONE', ( #73400 ), #74994, .F. ) ;
#35993 = AXIS2_PLACEMENT_3D ( 'NONE', #57101, #90015, #24774 ) ;
#35994 = CARTESIAN_POINT ( 'NONE',  ( 5.094000037296076755, -12.44634123771225198, -3.174960020027660867 ) ) ;
#35995 = CARTESIAN_POINT ( 'NONE',  ( -16.96448817358102801, 43.37119804630366104, -6.626685396512355553 ) ) ;
#35997 = LINE ( 'NONE', #3046, #30343 ) ;
#35996 = AXIS2_PLACEMENT_3D ( 'NONE', #32256, #65670, #72692 ) ;
#35998 = SURFACE_SIDE_STYLE ('',( #28977 ) ) ;
#35999 = VERTEX_POINT ( 'NONE', #549 ) ;
#36000 = CARTESIAN_POINT ( 'NONE',  ( -1.570796324976843295, 50.00000000000000000, -73.00000000000001421 ) ) ;
#36001 = ORIENTED_EDGE ( 'NONE', *, *, #71127, .F. ) ;
#36002 = CARTESIAN_POINT ( 'NONE',  ( 72.04471834908918026, -38.32678965749821032, 146.1819033111827935 ) ) ;
#36003 = DIRECTION ( 'NONE',  ( -1.000000000000000000, -0.000000000000000000, -0.000000000000000000 ) ) ;
#36004 = EDGE_CURVE ( 'NONE', #14145, #18144, #31976, .T. ) ;
#36005 = CARTESIAN_POINT ( 'NONE',  ( 24.95947819434403669, 295.7176545011159874, 10.12322481647160899 ) ) ;
#36006 = CARTESIAN_POINT ( 'NONE',  ( -5.384233811324302010, 246.9978290865521444, 2.655407383564630575 ) ) ;
#36007 = ORIENTED_EDGE ( 'NONE', *, *, #41762, .T. ) ;
#36008 = CARTESIAN_POINT ( 'NONE',  ( 28.56401049668863479, 13.37477103922271304, -40.29034081819158075 ) ) ;
#36009 = DIRECTION ( 'NONE',  ( -0.000000000000000000, -1.000000000000000000, -0.000000000000000000 ) ) ;
#36010 = CARTESIAN_POINT ( 'NONE',  ( 29.36753485554255505, 297.5156562771362587, 2.520813113073917755 ) ) ;
#36011 = CARTESIAN_POINT ( 'NONE',  ( -9.655270732726616956, 51.27407282810504086, 3.405563007191358960 ) ) ;
#36012 = ORIENTED_EDGE ( 'NONE', *, *, #62302, .T. ) ;
#36013 = AXIS2_PLACEMENT_3D ( 'NONE', #87889, #86839, #46877 ) ;
#36014 = FILL_AREA_STYLE_COLOUR ( '', #62500 ) ;
#36015 = DIRECTION ( 'NONE',  ( 0.000000000000000000, -1.000000000000000000, 0.000000000000000000 ) ) ;
#36016 = CARTESIAN_POINT ( 'NONE',  ( 0.4053525175236814548, 3.145852061456249960, 6.499999999999998224 ) ) ;
#36017 = CYLINDRICAL_SURFACE ( 'NONE', #88711, 4.000000000000000000 ) ;
#36018 = AXIS2_PLACEMENT_3D ( 'NONE', #47900, #80806, #39318 ) ;
#36019 = CARTESIAN_POINT ( 'NONE',  ( -32.85555225121258616, 465.7063523440040171, 11.00064571225268217 ) ) ;
#36020 = AXIS2_PLACEMENT_3D ( 'NONE', #81019, #72922, #52377 ) ;
#36021 = CIRCLE ( 'NONE', #8391, 4.000000000000001776 ) ;
#36022 = DIRECTION ( 'NONE',  ( 0.9735618822052878318, 0.000000000000000000, 0.2284234259372218689 ) ) ;
#36023 = CARTESIAN_POINT ( 'NONE',  ( 85.18141407811432941, -53.83922793184471800, 190.9676820986030350 ) ) ;
#36024 = CARTESIAN_POINT ( 'NONE',  ( 39.44615384615384812, 1.411358822780289120E-15, 0.000000000000000000 ) ) ;
#36025 = CARTESIAN_POINT ( 'NONE',  ( -8.745545711746213868, 132.0170111787129201, -6.344649108150348220E-13 ) ) ;
#36026 = VERTEX_POINT ( 'NONE', #24895 ) ;
#36027 = CARTESIAN_POINT ( 'NONE',  ( 75.60846622749433266, -57.67119937720136136, -32.37792878120276896 ) ) ;
#36028 = CARTESIAN_POINT ( 'NONE',  ( 69.26914063590702142, -29.97404492864524883, -21.11895981858886984 ) ) ;
#36029 = FACE_OUTER_BOUND ( 'NONE', #84541, .T. ) ;
#36030 = DIRECTION ( 'NONE',  ( -1.000000000000000000, -1.224606353822377258E-16, -0.000000000000000000 ) ) ;
#36031 = CARTESIAN_POINT ( 'NONE',  ( 5.000000000000000000, -13.80294717155101125, 10.52286356750360241 ) ) ;
#36032 = CARTESIAN_POINT ( 'NONE',  ( -92.47187049835589789, -30.00000000000000355, 102.9253929577534592 ) ) ;
#36033 = EDGE_CURVE ( 'NONE', #72914, #7841, #948, .T. ) ;
#36034 = AXIS2_PLACEMENT_3D ( 'NONE', #57296, #16319, #42189 ) ;
#36035 = SURFACE_STYLE_USAGE ( .BOTH. , #44088 ) ;
#36036 = CARTESIAN_POINT ( 'NONE',  ( 0.2599417667399435139, -57.67120205748143036, 41.61181906779697215 ) ) ;
#36037 = ADVANCED_FACE ( 'NONE', ( #66936 ), #90672, .F. ) ;
#36039 = PRESENTATION_STYLE_ASSIGNMENT (( #11697 ) ) ;
#36038 = CARTESIAN_POINT ( 'NONE',  ( -9.536842176398165449, 247.3576463011600595, 3.014135744008184847 ) ) ;
#36040 = CARTESIAN_POINT ( 'NONE',  ( 4.196261321702323244, -52.69005874581856119, 40.35766667076264014 ) ) ;
#36041 = CYLINDRICAL_SURFACE ( 'NONE', #16048, 5.000000000000000888 ) ;
#36042 = CARTESIAN_POINT ( 'NONE',  ( -34.12349128637492157, 490.8027302422244134, 11.84948222508912252 ) ) ;
#36043 = FACE_OUTER_BOUND ( 'NONE', #94861, .T. ) ;
#36044 = DIRECTION ( 'NONE',  ( 0.8191520442889975717, 1.003171929053531773E-16, -0.5735764363510378328 ) ) ;
#36045 = CARTESIAN_POINT ( 'NONE',  ( 50.89319870900899900, -27.68869576212836847, -27.73928759546735634 ) ) ;
#36046 = VECTOR ( 'NONE', #21182, 1000.000000000000000 ) ;
#36047 = B_SPLINE_CURVE_WITH_KNOTS ( 'NONE', 3,
 ( #106, #23932, #33078, #24979, #47093, #72956, #39566, #22862, #90758, #88630, #79995, #63837, #96730, #14720, #80521, #6639, #72441, #105344, #97242, #34142, #26072, #35744, #84256, #1170, #91300, #10872, #58383, #8762, #1726, #60011 ),
 .UNSPECIFIED., .F., .F.,
 ( 4, 2, 2, 2, 2, 2, 2, 2, 2, 2, 2, 2, 2, 2, 4 ),
 ( 0.01399668719228680698, 0.01422696114353627292, 0.01445723509478573886, 0.01491778299728466380, 0.01537833089978358700, 0.01583887880228251194, 0.01675997460728035141, 0.01768107041227819087, 0.01860216621727603381, 0.01952326202227386981, 0.01998380992477279475, 0.02044435782727171969, 0.02090490572977064115, 0.02113517968102010883, 0.02136545363226957303 ),
 .UNSPECIFIED. ) ;
#36048 = CARTESIAN_POINT ( 'NONE',  ( -23.10449564462755490, -60.35990861106341754, 34.93722728922637089 ) ) ;
#36049 = VERTEX_POINT ( 'NONE', #25445 ) ;
#36050 = CARTESIAN_POINT ( 'NONE',  ( 41.13328595189572923, 484.9084785457743578, -3.795084846869928974 ) ) ;
#36051 = CARTESIAN_POINT ( 'NONE',  ( -9.165151389911679658, 104.9999999999999858, -4.000000000000001776 ) ) ;
#36052 = CARTESIAN_POINT ( 'NONE',  ( -20.76759987540068053, -18.59339395674310680, 27.55335100898648548 ) ) ;
#36054 = DIRECTION ( 'NONE',  ( 1.000000000000000000, 0.000000000000000000, 0.000000000000000000 ) ) ;
#36053 = DIRECTION ( 'NONE',  ( 0.000000000000000000, 1.000000000000000000, 0.000000000000000000 ) ) ;
#36055 = VERTEX_POINT ( 'NONE', #15180 ) ;
#36056 = CARTESIAN_POINT ( 'NONE',  ( 15.59999999999999787, 3.309500000000003439, 0.000000000000000000 ) ) ;
#36057 = EDGE_LOOP ( 'NONE', ( #47104, #27894, #57878, #14585, #81280 ) ) ;
#36058 = CARTESIAN_POINT ( 'NONE',  ( 1.544427540536530710E-15, -4.285714285714290916, -25.22241582816893057 ) ) ;
#36059 = CIRCLE ( 'NONE', #53266, 6.500000000000000000 ) ;
#36060 = DIRECTION ( 'NONE',  ( -1.000000000000000000, -0.000000000000000000, -0.000000000000000000 ) ) ;
#36061 = EDGE_CURVE ( 'NONE', #19012, #23643, #21669, .T. ) ;
#36062 = CARTESIAN_POINT ( 'NONE',  ( 24.05868969682389036, 1.340359594676612611E-15, 0.000000000000000000 ) ) ;
#36063 = VERTEX_POINT ( 'NONE', #105784 ) ;
#36064 =( NAMED_UNIT ( * ) SI_UNIT ( $, .STERADIAN. ) SOLID_ANGLE_UNIT ( ) );
#36065 = CARTESIAN_POINT ( 'NONE',  ( 12.00013170160693576, 50.00000000000001421, -83.40936345627085302 ) ) ;
#36066 = CIRCLE ( 'NONE', #96335, 10.00000000000000178 ) ;
#36067 = CARTESIAN_POINT ( 'NONE',  ( 103.7353799882583019, -52.71710819990906316, 187.7499664499858909 ) ) ;
#36068 =( GEOMETRIC_REPRESENTATION_CONTEXT ( 3 ) GLOBAL_UNCERTAINTY_ASSIGNED_CONTEXT ( ( #54182 ) ) GLOBAL_UNIT_ASSIGNED_CONTEXT ( ( #85424, #44436, #11509 ) ) REPRESENTATION_CONTEXT ( 'NONE', 'WORKASPACE' ) );
#36070 = DIRECTION ( 'NONE',  ( 0.000000000000000000, 0.000000000000000000, -1.000000000000000000 ) ) ;
#36069 = SURFACE_STYLE_USAGE ( .BOTH. , #3124 ) ;
#36071 = ORIENTED_EDGE ( 'NONE', *, *, #30380, .T. ) ;
#36072 = EDGE_LOOP ( 'NONE', ( #46165, #41327, #85964, #43645 ) ) ;
#36073 = ORIENTED_EDGE ( 'NONE', *, *, #106198, .F. ) ;
#36074 = CARTESIAN_POINT ( 'NONE',  ( 22.89314219808496986, 305.6227281603157167, 10.10461317236653400 ) ) ;
#36075 = CARTESIAN_POINT ( 'NONE',  ( 22.61650669486618526, 1.474610560812782335E-15, 0.000000000000000000 ) ) ;
#36076 =( NAMED_UNIT ( * ) PLANE_ANGLE_UNIT ( ) SI_UNIT ( $, .RADIAN. ) );
#36078 = EDGE_CURVE ( 'NONE', #53170, #28024, #56090, .T. ) ;
#36077 = VERTEX_POINT ( 'NONE', #10790 ) ;
#36080 = DIRECTION ( 'NONE',  ( -1.000000000000000000, -1.224606353822377258E-16, -0.000000000000000000 ) ) ;
#36079 = B_SPLINE_CURVE_WITH_KNOTS ( 'NONE', 3,
 ( #3769, #10764, #94377, #92762, #3230, #85761, #69041, #18370 ),
 .UNSPECIFIED., .F., .F.,
 ( 4, 2, 2, 4 ),
 ( 2.459764730620682454E-07, 0.001920659145285692239, 0.002880865729692007153, 0.003841072314098320766 ),
 .UNSPECIFIED. ) ;
#36081 = CARTESIAN_POINT ( 'NONE',  ( -4.999060807336862311, 41.75164249415626472, -70.37937597734750739 ) ) ;
#36082 = AXIS2_PLACEMENT_3D ( 'NONE', #87234, #44660, #37656 ) ;
#36083 = CARTESIAN_POINT ( 'NONE',  ( 31.33351735136876570, 438.6532904498233165, 22.86609632551569149 ) ) ;
#36084 = CARTESIAN_POINT ( 'NONE',  ( -94.39696246771445942, -59.99999999999998579, 5.332034942330889038 ) ) ;
#36085 = CARTESIAN_POINT ( 'NONE',  ( 23.58349330513380337, -4.000000000000000888, 4.898587196589416773E-16 ) ) ;
#36086 = CARTESIAN_POINT ( 'NONE',  ( -11.93400008872653295, -5.000000000000000888, 11.28327264068946079 ) ) ;
#36087 = DIRECTION ( 'NONE',  ( -1.000000000000000000, -1.224606353822377258E-16, -0.000000000000000000 ) ) ;
#36088 = CARTESIAN_POINT ( 'NONE',  ( -89.21407719722087393, -30.00000000000005684, 9.591031914958218607 ) ) ;
#36089 = CARTESIAN_POINT ( 'NONE',  ( -43.50250715914157240, 464.6389613228374742, 9.611700240009312779 ) ) ;
#36090 = COLOUR_RGB ( '', 0.40784314, 0.44705882, 0.49803922) ;
#36091 = CARTESIAN_POINT ( 'NONE',  ( -49.29312953085187132, -18.74715051740997040, 42.99385802251428146 ) ) ;
#36092 = ORIENTED_EDGE ( 'NONE', *, *, #33808, .F. ) ;
#36093 = LINE ( 'NONE', #77032, #90082 ) ;
#36094 = ORIENTED_EDGE ( 'NONE', *, *, #64505, .F. ) ;
#36095 = CARTESIAN_POINT ( 'NONE',  ( 12.50000000000000355, 5.730253167712460183, -23.74922868128247089 ) ) ;
#36096 = DIRECTION ( 'NONE',  ( 0.000000000000000000, 0.000000000000000000, 1.000000000000000000 ) ) ;
#36097 = VECTOR ( 'NONE', #31040, 1000.000000000000000 ) ;
#36098 = CARTESIAN_POINT ( 'NONE',  ( 3.400000000000000355, 0.000000000000000000, -3.852324522925831385 ) ) ;
#36099 = ORIENTED_EDGE ( 'NONE', *, *, #80253, .T. ) ;
#36100 = SURFACE_SIDE_STYLE ('',( #68970 ) ) ;
#36101 = EDGE_LOOP ( 'NONE', ( #104597, #26850, #40317, #933, #81264 ) ) ;
#36102 = CARTESIAN_POINT ( 'NONE',  ( 90.08918622825524380, -30.00000000000337153, -5.724205789237760911 ) ) ;
#36103 = CARTESIAN_POINT ( 'NONE',  ( -3.371112934716220631E-16, 8.660254037844390851, -7.564335161054499324 ) ) ;
#36104 = CARTESIAN_POINT ( 'NONE',  ( -4.247379606276268760, -12.84324797163533383, -9.569866633816575430 ) ) ;
#36105 = CARTESIAN_POINT ( 'NONE',  ( -7.754160006507099467, 42.00000000000000711, -59.23741894013591036 ) ) ;
#36106 = CARTESIAN_POINT ( 'NONE',  ( 90.37482638485310815, -29.99999999999999645, 190.1461905130674950 ) ) ;
#36107 = CARTESIAN_POINT ( 'NONE',  ( 9.999999999999996447, 15.00000000000000000, -10.00000000000000000 ) ) ;
#36108 = EDGE_CURVE ( 'NONE', #95845, #88418, #30077, .T. ) ;
#36109 = CARTESIAN_POINT ( 'NONE',  ( -1.250111696621528434, 36.68807930902310943, 28.65717016957791685 ) ) ;
#36110 = AXIS2_PLACEMENT_3D ( 'NONE', #10496, #57978, #82798 ) ;
#36111 = ORIENTED_EDGE ( 'NONE', *, *, #93065, .F. ) ;
#36112 = ORIENTED_EDGE ( 'NONE', *, *, #90251, .F. ) ;
#36113 = CARTESIAN_POINT ( 'NONE',  ( 53.47773224423268346, -60.31207318078936197, 65.32173576400356296 ) ) ;
#36114 = DIRECTION ( 'NONE',  ( 0.000000000000000000, -1.000000000000000000, 0.000000000000000000 ) ) ;
#36115 = CYLINDRICAL_SURFACE ( 'NONE', #49596, 6.499999999999999112 ) ;
#36116 = EDGE_CURVE ( 'NONE', #942, #22950, #10968, .T. ) ;
#36117 = ORIENTED_EDGE ( 'NONE', *, *, #73802, .T. ) ;
#36118 = CARTESIAN_POINT ( 'NONE',  ( -88.03633069172695969, -38.37099167637006047, -19.52536479018785087 ) ) ;
#36119 = PRESENTATION_LAYER_ASSIGNMENT (  '', '', ( #56764 ) ) ;
#36120 = ORIENTED_EDGE ( 'NONE', *, *, #100801, .F. ) ;
#36121 = FACE_OUTER_BOUND ( 'NONE', #83965, .T. ) ;
#36122 = CARTESIAN_POINT ( 'NONE',  ( 111.0097756496680006, -38.35607304391395189, 172.2120856835122709 ) ) ;
#36123 = CARTESIAN_POINT ( 'NONE',  ( 12.15267230755900663, 17.47167679243762350, 8.961506924172995880 ) ) ;
#36124 = CARTESIAN_POINT ( 'NONE',  ( 86.51436465318690239, -60.13692532640241240, 2.092395710485930316 ) ) ;
#36125 = FACE_OUTER_BOUND ( 'NONE', #100022, .T. ) ;
#36126 = CARTESIAN_POINT ( 'NONE',  ( -20.24579557674104890, 304.8297271373346575, -10.00469232190997282 ) ) ;
#36127 = CARTESIAN_POINT ( 'NONE',  ( 1.000000000000000000, -5.000000000000015099, -14.14213562373094923 ) ) ;
#36128 = AXIS2_PLACEMENT_3D ( 'NONE', #5245, #62952, #23038 ) ;
#36129 = CARTESIAN_POINT ( 'NONE',  ( 5.980097492742836529, -2.767486787161697492, 6.500000000000000000 ) ) ;
#36130 = EDGE_CURVE ( 'NONE', #53571, #87774, #44122, .T. ) ;
#36131 = SURFACE_SIDE_STYLE ('',( #27506 ) ) ;
#36132 = CARTESIAN_POINT ( 'NONE',  ( 3.591939471459422162, 128.3897234052070928, 4.999999999999999112 ) ) ;
#36133 = ORIENTED_EDGE ( 'NONE', *, *, #87171, .T. ) ;
#36134 = CARTESIAN_POINT ( 'NONE',  ( 1.101222382041291858, 36.52459501129955299, 29.11284624768989460 ) ) ;
#36135 = CARTESIAN_POINT ( 'NONE',  ( 7.500000000000005329, 40.28748004600710431, -68.91429205818927528 ) ) ;
#36136 = DIRECTION ( 'NONE',  ( 0.000000000000000000, 1.000000000000000000, 0.000000000000000000 ) ) ;
#36137 = ORIENTED_EDGE ( 'NONE', *, *, #2264, .T. ) ;
#36138 = DIRECTION ( 'NONE',  ( -0.000000000000000000, 0.000000000000000000, 1.000000000000000000 ) ) ;
#36139 = CARTESIAN_POINT ( 'NONE',  ( -27.19575328468113184, 307.3469062500455493, 10.97895680454243283 ) ) ;
#36140 = CARTESIAN_POINT ( 'NONE',  ( 0.000000000000000000, 0.000000000000000000, 0.000000000000000000 ) ) ;
#36141 = LINE ( 'NONE', #18338, #50669 ) ;
#36142 = CARTESIAN_POINT ( 'NONE',  ( -3.313708498984765161, -21.96875000000000000, 7.999999999999998224 ) ) ;
#36143 = CARTESIAN_POINT ( 'NONE',  ( 31.19249401299645186, -22.25766550667198374, 32.30297921700840647 ) ) ;
#36144 = CIRCLE ( 'NONE', #20454, 7.499999999992679633 ) ;
#36145 = CARTESIAN_POINT ( 'NONE',  ( 43.00000000000000000, 436.0987441542287115, 7.567257455462724991 ) ) ;
#36146 = ORIENTED_EDGE ( 'NONE', *, *, #53461, .F. ) ;
#36147 = CARTESIAN_POINT ( 'NONE',  ( 84.00677267882208810, -50.15819390199315819, 186.9337807051296352 ) ) ;
#36148 = CARTESIAN_POINT ( 'NONE',  ( -30.00000000000000000, 1.714505518806294441E-15, 13.00000000000000000 ) ) ;
#36149 = CARTESIAN_POINT ( 'NONE',  ( -16.02196273765588330, 46.08952128005078919, 4.311160109051469291 ) ) ;
#36150 = EDGE_LOOP ( 'NONE', ( #7936, #22465, #103684, #51643 ) ) ;
#36151 = CARTESIAN_POINT ( 'NONE',  ( -96.37380543725086568, -52.71037193844853874, 101.1465460539529460 ) ) ;
#36152 = CARTESIAN_POINT ( 'NONE',  ( 34.83349330513379982, 1.593028355512270567E-15, 0.000000000000000000 ) ) ;
#36153 = CARTESIAN_POINT ( 'NONE',  ( 9.797174393178803964E-16, 273.9999999999999432, 7.999999999999983125 ) ) ;
#36154 = CARTESIAN_POINT ( 'NONE',  ( -31.37180257112542847, -30.07018934284766232, -38.10741079039508605 ) ) ;
#36155 = ADVANCED_FACE ( 'NONE', ( #67470 ), #92302, .T. ) ;
#36156 =( NAMED_UNIT ( * ) PLANE_ANGLE_UNIT ( ) SI_UNIT ( $, .RADIAN. ) );
#36157 = STYLED_ITEM ( 'NONE', ( #12666 ), #45875 ) ;
#36158 = CARTESIAN_POINT ( 'NONE',  ( 25.47307600370571379, -59.99999999999998579, 41.30018710837394735 ) ) ;
#36159 = CIRCLE ( 'NONE', #15466, 4.000000000000000888 ) ;
#36160 = CARTESIAN_POINT ( 'NONE',  ( 31.55798995419172570, -33.46712117103052009, 41.53811485048920105 ) ) ;
#36161 = SURFACE_STYLE_FILL_AREA ( #77102 ) ;
#36162 = CARTESIAN_POINT ( 'NONE',  ( 51.37712067241238145, -29.89819866070208576, 48.95739146609739123 ) ) ;
#36163 = EDGE_CURVE ( 'NONE', #48298, #105469, #9623, .T. ) ;
#36166 = CARTESIAN_POINT ( 'NONE',  ( -10.06395418932315167, 12.92917864820601892, 10.57395537501041183 ) ) ;
#36165 = CIRCLE ( 'NONE', #32757, 5.000000000000002665 ) ;
#36164 = CARTESIAN_POINT ( 'NONE',  ( -32.45767638303610170, -34.03325006748782044, 42.16482906108820572 ) ) ;
#36167 = CARTESIAN_POINT ( 'NONE',  ( 9.482342435883346354, 294.6573797848125196, -3.183473687089551252 ) ) ;
#36168 = CARTESIAN_POINT ( 'NONE',  ( 41.58649125062324003, 315.0454808444952732, -5.157136739135766312 ) ) ;
#36169 = CARTESIAN_POINT ( 'NONE',  ( 67.22793774957824553, 4.000000000000013323, 0.000000000000000000 ) ) ;
#36170 = CARTESIAN_POINT ( 'NONE',  ( 0.000000000000000000, 0.000000000000000000, -4.874849604647447876 ) ) ;
#36171 = AXIS2_PLACEMENT_3D ( 'NONE', #5012, #47042, #102101 ) ;
#36172 = ORIENTED_EDGE ( 'NONE', *, *, #30526, .T. ) ;
#36173 = CARTESIAN_POINT ( 'NONE',  ( -19.36103579130787367, 294.6347466944262692, -10.04613669444748503 ) ) ;
#36174 = ORIENTED_EDGE ( 'NONE', *, *, #24389, .F. ) ;
#36175 = FACE_OUTER_BOUND ( 'NONE', #40909, .T. ) ;
#36176 = CARTESIAN_POINT ( 'NONE',  ( 6.000469943554648466, -60.99929508329501004, 0.2622423038614445368 ) ) ;
#36177 = AXIS2_PLACEMENT_3D ( 'NONE', #44692, #93761, #60872 ) ;
#36179 = CARTESIAN_POINT ( 'NONE',  ( -18.69900205392447390, -21.77036642001481681, -29.76779902863794192 ) ) ;
#36178 = CARTESIAN_POINT ( 'NONE',  ( 9.948513602188011617, 253.8697794334385378, 1.045942665286124340 ) ) ;
#36180 = EDGE_CURVE ( 'NONE', #16299, #54111, #70522, .T. ) ;
#36181 = ORIENTED_EDGE ( 'NONE', *, *, #69207, .T. ) ;
#36182 = AXIS2_PLACEMENT_3D ( 'NONE', #52545, #61193, #54123 ) ;
#36183 = DIRECTION ( 'NONE',  ( -0.000000000000000000, -1.000000000000000000, -0.000000000000000000 ) ) ;
#36184 = FACE_OUTER_BOUND ( 'NONE', #80054, .T. ) ;
#36185 = ORIENTED_EDGE ( 'NONE', *, *, #22223, .F. ) ;
#36186 = CARTESIAN_POINT ( 'NONE',  ( 14.83349330513380337, 1.593028355512270567E-15, 0.000000000000000000 ) ) ;
#36187 = LINE ( 'NONE', #44782, #69014 ) ;
#36188 = CARTESIAN_POINT ( 'NONE',  ( 100.6222222222222200, 1.023464760207051730E-14, 0.000000000000000000 ) ) ;
#36189 = CARTESIAN_POINT ( 'NONE',  ( -93.05166615780947836, -60.00000000000000000, 32.92217660829798831 ) ) ;
#36190 = LINE ( 'NONE', #43698, #70383 ) ;
#36191 = FACE_BOUND ( 'NONE', #105244, .T. ) ;
#36192 = FACE_OUTER_BOUND ( 'NONE', #224, .T. ) ;
#36193 = CARTESIAN_POINT ( 'NONE',  ( 39.82070819425764086, 460.7076632888625909, 2.105638695484907785 ) ) ;
#36195 = SURFACE_SIDE_STYLE ('',( #67463 ) ) ;
#36194 = CARTESIAN_POINT ( 'NONE',  ( -34.17998405129007722, 435.1836295971070285, 10.78820992711269788 ) ) ;
#36196 = AXIS2_PLACEMENT_3D ( 'NONE', #48729, #35123, #33125 ) ;
#36197 = CARTESIAN_POINT ( 'NONE',  ( -84.68119024137185136, -25.54381684178671108, 163.3937236597952563 ) ) ;
#36198 = VERTEX_POINT ( 'NONE', #71041 ) ;
#36199 = CARTESIAN_POINT ( 'NONE',  ( -43.60092683753732246, 434.9832283443418532, 14.46740323056809352 ) ) ;
#36200 = VERTEX_POINT ( 'NONE', #43709 ) ;
#36201 = ORIENTED_EDGE ( 'NONE', *, *, #58152, .T. ) ;
#36202 = CARTESIAN_POINT ( 'NONE',  ( -4.551587301587304957, -1.200583151104947843, 104.4018401814738155 ) ) ;
#36203 = CARTESIAN_POINT ( 'NONE',  ( 15.73927229776362680, -4.999999999999999112, -7.856667017202335401 ) ) ;
#36204 = CARTESIAN_POINT ( 'NONE',  ( -1.843253007570911225E-16, -9.147862274876562338, -8.047472243342939535 ) ) ;
#36205 = DIRECTION ( 'NONE',  ( 0.000000000000000000, -1.000000000000000000, 0.000000000000000000 ) ) ;
#36206 = ORIENTED_EDGE ( 'NONE', *, *, #84741, .F. ) ;
#36207 = CARTESIAN_POINT ( 'NONE',  ( 20.59999999999999787, 1.533819458162526451E-15, 0.000000000000000000 ) ) ;
#36208 = CARTESIAN_POINT ( 'NONE',  ( -94.50453298674098335, -57.65443526055588563, -11.14264577307068294 ) ) ;
#36209 = CARTESIAN_POINT ( 'NONE',  ( -5.725004243152313599, -68.57519148255369146, -1.812899781754688577 ) ) ;
#36210 = DIRECTION ( 'NONE',  ( -1.000000000000000000, -1.224606353822377258E-16, -0.000000000000000000 ) ) ;
#36211 = CARTESIAN_POINT ( 'NONE',  ( 24.32789867356907720, 27.33682607920834684, 32.55354264101764983 ) ) ;
#36212 = CARTESIAN_POINT ( 'NONE',  ( -48.02835407290516656, -1.200000000000000030E-05, 16.85535821593516559 ) ) ;
#36213 = CARTESIAN_POINT ( 'NONE',  ( -17.77153375527955603, 36.31766862386357531, -23.79949801963322997 ) ) ;
#36214 = VECTOR ( 'NONE', #103243, 1000.000000000000000 ) ;
#36215 = CARTESIAN_POINT ( 'NONE',  ( 100.4059631369621570, -60.00000000000003553, 69.07260714096372567 ) ) ;
#36216 = CARTESIAN_POINT ( 'NONE',  ( -78.68906450541477682, -14.21045842199436926, 170.0145061391070271 ) ) ;
#36217 = CARTESIAN_POINT ( 'NONE',  ( -55.11669765333618898, -32.56112197649012074, 57.75454668961312166 ) ) ;
#36218 = ORIENTED_EDGE ( 'NONE', *, *, #76436, .T. ) ;
#36219 = CARTESIAN_POINT ( 'NONE',  ( -29.68315524077005207, 18.29184282782459547, -39.60535821593474282 ) ) ;
#36220 = ORIENTED_EDGE ( 'NONE', *, *, #28199, .F. ) ;
#36221 = CARTESIAN_POINT ( 'NONE',  ( -100.4908920805564065, -37.81811875270330603, 189.5769949498487961 ) ) ;
#36222 = DIRECTION ( 'NONE',  ( 0.000000000000000000, -1.000000000000000000, 0.000000000000000000 ) ) ;
#36223 = VERTEX_POINT ( 'NONE', #18399 ) ;
#36224 = CARTESIAN_POINT ( 'NONE',  ( 7.500000000000003553, -2.999999999999999112, -68.91429205785459544 ) ) ;
#36225 = SURFACE_STYLE_USAGE ( .BOTH. , #85263 ) ;
#36226 = DIRECTION ( 'NONE',  ( 0.5735764363510466035, -0.8191520442889914655, 1.003171929053524500E-16 ) ) ;
#36227 = CARTESIAN_POINT ( 'NONE',  ( -7.188101187500000044, -12.78125000204838635, -8.802885111219163269E-16 ) ) ;
#36228 = CARTESIAN_POINT ( 'NONE',  ( -3.311033882356798252E-14, 37.21016666119783167, -27.24999999999961986 ) ) ;
#36229 = LINE ( 'NONE', #13480, #4742 ) ;
#36230 = CARTESIAN_POINT ( 'NONE',  ( 7.743982712349851916, -81.53786985239263174, 2.020119794285909709 ) ) ;
#36231 = CARTESIAN_POINT ( 'NONE',  ( -19.70764564238371719, 304.7954121406193622, 9.925013215726785631 ) ) ;
#36232 =( LENGTH_UNIT ( ) NAMED_UNIT ( * ) SI_UNIT ( .MILLI., .METRE. ) );
#36233 = CARTESIAN_POINT ( 'NONE',  ( -9.047759419560607697, 14.48369194312116548, 1.733336949948506312E-30 ) ) ;
#36234 = CARTESIAN_POINT ( 'NONE',  ( -15.65186372275021931, 46.18633577147561908, -4.642160826816701835 ) ) ;
#36235 = EDGE_CURVE ( 'NONE', #80843, #98077, #51251, .T. ) ;
#36236 = CARTESIAN_POINT ( 'NONE',  ( -5.168696396656956793, 1.295298111819218168, -22.28139744604624184 ) ) ;
#36237 = UNCERTAINTY_MEASURE_WITH_UNIT (LENGTH_MEASURE( 1.000000000000000082E-05 ), #84288, 'distance_accuracy_value', 'NONE');
#36238 = CARTESIAN_POINT ( 'NONE',  ( -30.06290811726797330, -32.54186696253240996, 31.90563260260433154 ) ) ;
#36239 = AXIS2_PLACEMENT_3D ( 'NONE', #52213, #100236, #26403 ) ;
#36240 = CARTESIAN_POINT ( 'NONE',  ( 3.867302399549911840, 18.90821977549292043, 5.835068021887773071 ) ) ;
#36241 = CARTESIAN_POINT ( 'NONE',  ( 47.73540206996886326, -32.60520857632516822, 45.16482891593580007 ) ) ;
#36242 = DIRECTION ( 'NONE',  ( 0.5735764363510470476, -0.8191520442889911324, 1.003171929053524007E-16 ) ) ;
#36243 = CARTESIAN_POINT ( 'NONE',  ( -7.412906595240169594, 87.64188272852254613, 3.014362223629231785 ) ) ;
#36244 = CIRCLE ( 'NONE', #56888, 6.500000000000000888 ) ;
#36245 = EDGE_CURVE ( 'NONE', #41831, #53305, #29564, .T. ) ;
#36246 = CARTESIAN_POINT ( 'NONE',  ( -96.51435786616053747, -38.48409689973218661, 201.1738884492503132 ) ) ;
#36247 = ORIENTED_EDGE ( 'NONE', *, *, #74940, .T. ) ;
#36249 = CARTESIAN_POINT ( 'NONE',  ( -28.30714194752022195, 36.37574732085258944, 8.454175457664668158 ) ) ;
#36248 = CARTESIAN_POINT ( 'NONE',  ( 33.86650669486618881, 1.474610560812782335E-15, 0.000000000000000000 ) ) ;
#36250 = CARTESIAN_POINT ( 'NONE',  ( 13.92920313560041023, 2.720439590250280482, -5.536316934251884980 ) ) ;
#36251 = CARTESIAN_POINT ( 'NONE',  ( -49.27893332325997022, 7.918143476871234654, -15.56220613712109468 ) ) ;
#36252 = CARTESIAN_POINT ( 'NONE',  ( -7.010778356522921584, 41.61257608818559817, -59.09056163754224400 ) ) ;
#36253 = CARTESIAN_POINT ( 'NONE',  ( 4.852941176470594975, 40.00000000000031974, -70.80672828634230598 ) ) ;
#36254 = CARTESIAN_POINT ( 'NONE',  ( 36.84999999999999432, 1.533819458162526451E-15, 0.000000000000000000 ) ) ;
#36255 = CARTESIAN_POINT ( 'NONE',  ( -23.67370564920981124, 306.0413591249409819, 9.198534280147706355 ) ) ;
#36256 = DIRECTION ( 'NONE',  ( -0.000000000000000000, 1.000000000000000000, -0.000000000000000000 ) ) ;
#36257 = CARTESIAN_POINT ( 'NONE',  ( 106.5750692260998278, -59.99999999999999289, 197.6315772264619284 ) ) ;
#36258 = EDGE_CURVE ( 'NONE', #106756, #77143, #45816, .T. ) ;
#36259 = CARTESIAN_POINT ( 'NONE',  ( -7.412906595240166041, -67.64188272852254613, 3.014362223629234450 ) ) ;
#36260 = CIRCLE ( 'NONE', #96500, 8.142857142857131691 ) ;
#36261 = ORIENTED_EDGE ( 'NONE', *, *, #8110, .F. ) ;
#36262 = CARTESIAN_POINT ( 'NONE',  ( 36.16847030042395517, 438.2414514106960723, 3.889105687734257799 ) ) ;
#36263 = CARTESIAN_POINT ( 'NONE',  ( -80.54403476602729484, -30.00000000000000000, -12.95354117423075024 ) ) ;
#36264 = ORIENTED_EDGE ( 'NONE', *, *, #84338, .F. ) ;
#36266 = B_SPLINE_CURVE_WITH_KNOTS ( 'NONE', 3,
 ( #49759, #57837, #26599, #40607, #98317, #66476, #41673, #67557, #99904, #1176, #58933, #75628, #89701, #57306 ),
 .UNSPECIFIED., .F., .F.,
 ( 4, 2, 2, 2, 2, 2, 4 ),
 ( 0.000000000000000000, 0.003030522498881887093, 0.004545783748322844951, 0.006061044997763803677, 0.007576306247204760667, 0.009091567496645719393, 0.01212208999552772531 ),
 .UNSPECIFIED. ) ;
#36265 = CIRCLE ( 'NONE', #20801, 14.00000000000000000 ) ;
#36268 = CARTESIAN_POINT ( 'NONE',  ( 5.307793834089975071, 21.57984177784170754, -40.64461319766989789 ) ) ;
#36267 = CARTESIAN_POINT ( 'NONE',  ( -75.25348839758508745, -38.34335650720067434, 171.9446546056112481 ) ) ;
#36269 = CARTESIAN_POINT ( 'NONE',  ( 12.49154685109993856, -3.434808443366712982, -13.82992914247694038 ) ) ;
#36270 = CARTESIAN_POINT ( 'NONE',  ( -7.791781413346523522, -3.000000000000000444, -2.093983074874246952 ) ) ;
#36271 = CARTESIAN_POINT ( 'NONE',  ( 6.943035990376878352, 41.50417910381163011, -58.81491866537869129 ) ) ;
#36272 = CARTESIAN_POINT ( 'NONE',  ( 5.082755093536324154, -10.71875000204838457, 5.082755093536326818 ) ) ;
#36273 = CARTESIAN_POINT ( 'NONE',  ( 1.570796324980112679, -5.000000000000002665, -73.00000000000001421 ) ) ;
#36274 = CIRCLE ( 'NONE', #56909, 5.000000000000001776 ) ;
#36275 = DIRECTION ( 'NONE',  ( 0.8191520442889974607, 1.003171929053531649E-16, -0.5735764363510379438 ) ) ;
#36277 = ORIENTED_EDGE ( 'NONE', *, *, #95299, .F. ) ;
#36276 = CARTESIAN_POINT ( 'NONE',  ( -7.500000000000007105, 39.99999999999998579, -68.91429205786793943 ) ) ;
#36278 = CARTESIAN_POINT ( 'NONE',  ( 85.53813280434940225, -21.95506244895780412, 166.5497984053122593 ) ) ;
#36279 = VECTOR ( 'NONE', #59128, 1000.000000000000000 ) ;
#36280 = DIRECTION ( 'NONE',  ( -1.000000000000000000, -1.224606353822377258E-16, -0.000000000000000000 ) ) ;
#36281 = CARTESIAN_POINT ( 'NONE',  ( 3.983107665916330475, -5.570601890521310828, -6.171481112545259329 ) ) ;
#36282 = VERTEX_POINT ( 'NONE', #11324 ) ;
#36283 = CARTESIAN_POINT ( 'NONE',  ( 0.000000000000000000, -30.00000000000000000, 0.000000000000000000 ) ) ;
#36284 = CARTESIAN_POINT ( 'NONE',  ( 40.92692307692308162, -4.171999999999999709, 0.000000000000000000 ) ) ;
#36285 = CARTESIAN_POINT ( 'NONE',  ( 98.31310517497099966, -5.000000000000000000, 6.123233995736778115E-16 ) ) ;
#36286 = CARTESIAN_POINT ( 'NONE',  ( 0.000000000000000000, 0.000000000000000000, -0.7408754770741831086 ) ) ;
#36287 =( NAMED_UNIT ( * ) PLANE_ANGLE_UNIT ( ) SI_UNIT ( $, .RADIAN. ) );
#36288 = CARTESIAN_POINT ( 'NONE',  ( 17.63688729554944601, 43.19915187278243707, 6.171107486271527165 ) ) ;
#36289 = SURFACE_STYLE_USAGE ( .BOTH. , #44338 ) ;
#36290 = ORIENTED_EDGE ( 'NONE', *, *, #103347, .T. ) ;
#36291 = EDGE_CURVE ( 'NONE', #15986, #102596, #61376, .T. ) ;
#36292 = SURFACE_STYLE_FILL_AREA ( #61064 ) ;
#36293 = CARTESIAN_POINT ( 'NONE',  ( -80.64317183426827285, -30.00000000000000355, -12.75789385870653270 ) ) ;
#36294 = AXIS2_PLACEMENT_3D ( 'NONE', #2810, #102040, #10889 ) ;
#36295 = CARTESIAN_POINT ( 'NONE',  ( 6.750000000000016875, -11.69134295108991495, -13.00000000000000000 ) ) ;
#36296 = DIRECTION ( 'NONE',  ( -0.5735764363510494901, -0.8191520442889894671, 0.000000000000000000 ) ) ;
#36297 = EDGE_CURVE ( 'NONE', #492, #9858, #10274, .T. ) ;
#36298 = ADVANCED_FACE ( 'NONE', ( #92790 ), #100347, .T. ) ;
#36300 = DIRECTION ( 'NONE',  ( 0.2244612941943401052, 0.4655631424235968097, 0.8560771506267808029 ) ) ;
#36299 = DIRECTION ( 'NONE',  ( -0.5735764363510494901, -0.8191520442889894671, 0.000000000000000000 ) ) ;
#36301 = CONICAL_SURFACE ( 'NONE', #13825, 3.309500000000001663, 0.9599310885968770357 ) ;
#36302 = CARTESIAN_POINT ( 'NONE',  ( 7.188101187500001821, -25.06250000204838457, -2.977408999572650483 ) ) ;
#36303 = CARTESIAN_POINT ( 'NONE',  ( 17.66137975014545347, 294.6000572424684378, -10.05351037453485574 ) ) ;
#36304 = APPLICATION_CONTEXT ( 'automotive_design' ) ;
#36305 = CARTESIAN_POINT ( 'NONE',  ( 8.716576110311626380, -5.000000000000000000, -5.062272329164819951 ) ) ;
#36306 = DIRECTION ( 'NONE',  ( -1.000000000000000000, -1.224606353822377258E-16, -0.000000000000000000 ) ) ;
#36307 = ORIENTED_EDGE ( 'NONE', *, *, #95299, .T. ) ;
#36308 = CARTESIAN_POINT ( 'NONE',  ( 0.000000000000000000, 0.000000000000000000, 0.000000000000000000 ) ) ;
#36309 =( LENGTH_UNIT ( ) NAMED_UNIT ( * ) SI_UNIT ( .MILLI., .METRE. ) );
#36310 = CARTESIAN_POINT ( 'NONE',  ( -4.782240561419170533, 7.495540900963799658, -5.000000000000000888 ) ) ;
#36311 = DIRECTION ( 'NONE',  ( 0.000000000000000000, 0.000000000000000000, 1.000000000000000000 ) ) ;
#36312 = EDGE_CURVE ( 'NONE', #26304, #41710, #93321, .T. ) ;
#36313 = VERTEX_POINT ( 'NONE', #103412 ) ;
#36314 = CARTESIAN_POINT ( 'NONE',  ( -7.481934216406634697, 52.00372086678742534, -3.435407541340197657 ) ) ;
#36315 = CARTESIAN_POINT ( 'NONE',  ( -1.469576158976823947E-15, -22.06250000409676915, 8.000000000000000000 ) ) ;
#36316 = CARTESIAN_POINT ( 'NONE',  ( 31.63611612624782410, 436.4523533804024851, 18.85849934886137191 ) ) ;
#36317 = CARTESIAN_POINT ( 'NONE',  ( -0.5307430543511253429, 13.43124519068178557, -49.36191628181192925 ) ) ;
#36318 = CARTESIAN_POINT ( 'NONE',  ( 9.798380800342661345, 101.5319934568449725, -2.010350564680324137 ) ) ;
#36319 = CARTESIAN_POINT ( 'NONE',  ( -111.1388128507345812, -60.00000000000001421, 186.5774987372416263 ) ) ;
#36320 = CARTESIAN_POINT ( 'NONE',  ( 19.16305615217603631, 49.74182397839735614, 61.63059818732328665 ) ) ;
#36321 = CYLINDRICAL_SURFACE ( 'NONE', #7282, 4.000000000000000000 ) ;
#36322 = PRESENTATION_STYLE_ASSIGNMENT (( #44371 ) ) ;
#36323 = EDGE_CURVE ( 'NONE', #19141, #53038, #104395, .T. ) ;
#36324 = CARTESIAN_POINT ( 'NONE',  ( -10.00000000000000355, 0.000000000000000000, -10.00000000000000000 ) ) ;
#36325 = CARTESIAN_POINT ( 'NONE',  ( -81.59287406109901042, -60.63717241894644161, 186.3584735478276002 ) ) ;
#36326 = DIRECTION ( 'NONE',  ( 0.000000000000000000, 1.000000000000000000, 0.000000000000000000 ) ) ;
#36327 = STYLED_ITEM ( 'NONE', ( #36780 ), #49987 ) ;
#36328 = ORIENTED_EDGE ( 'NONE', *, *, #92109, .F. ) ;
#36329 = DIRECTION ( 'NONE',  ( 1.000000000000000000, 0.000000000000000000, 0.000000000000000000 ) ) ;
#36330 = CARTESIAN_POINT ( 'NONE',  ( 4.003587701499093043, -1.050376533302863180, 104.5574048719304301 ) ) ;
#36331 = CARTESIAN_POINT ( 'NONE',  ( -86.42542376329605247, -60.13647821371448288, 3.360464890229343915 ) ) ;
#36332 = COLOUR_RGB ( '', 0.08235294, 0.09019608, 0.10196078) ;
#36333 = DIRECTION ( 'NONE',  ( 0.000000000000000000, 0.000000000000000000, -1.000000000000000000 ) ) ;
#36334 =( LENGTH_UNIT ( ) NAMED_UNIT ( * ) SI_UNIT ( .MILLI., .METRE. ) );
#36335 = CARTESIAN_POINT ( 'NONE',  ( 8.588409832220163409, 128.2015064896677643, 0.000000000000000000 ) ) ;
#36336 = CARTESIAN_POINT ( 'NONE',  ( -6.999999999999975131, -12.54465221550630183, 8.223849511754991681 ) ) ;
#36337 = PRESENTATION_STYLE_ASSIGNMENT (( #10406 ) ) ;
#36338 = CARTESIAN_POINT ( 'NONE',  ( 68.99587917277882809, -30.00000000000005329, 123.4883035811859884 ) ) ;
#36339 = CARTESIAN_POINT ( 'NONE',  ( -8.572527594031464315E-16, 61.50000000000000000, 6.999999999999992895 ) ) ;
#36340 = AXIS2_PLACEMENT_3D ( 'NONE', #100816, #17274, #35602 ) ;
#36341 = CARTESIAN_POINT ( 'NONE',  ( -86.58068678654640848, -14.21045842199428932, 15.94391106889438525 ) ) ;
#36342 = CARTESIAN_POINT ( 'NONE',  ( -71.85214048801175579, -56.85815330016787783, 119.4862648020721423 ) ) ;
#36343 = EDGE_LOOP ( 'NONE', ( #102268, #33057, #17138, #67246 ) ) ;
#36344 = CARTESIAN_POINT ( 'NONE',  ( 79.87681789614374850, -30.00000000000000711, 191.0754539389706395 ) ) ;
#36345 = CARTESIAN_POINT ( 'NONE',  ( -20.51763481795492794, 40.83832659751297456, 61.74835002636409342 ) ) ;
#36346 = ORIENTED_EDGE ( 'NONE', *, *, #94451, .T. ) ;
#36347 = CARTESIAN_POINT ( 'NONE',  ( 38.08648362024728584, -60.00000000001480061, 53.39166904922846868 ) ) ;
#36348 = EDGE_LOOP ( 'NONE', ( #57973, #104660, #53300, #100453 ) ) ;
#36349 = CARTESIAN_POINT ( 'NONE',  ( 13.64654340589911818, -56.64216131223533779, 30.13167154758286159 ) ) ;
#36350 = CARTESIAN_POINT ( 'NONE',  ( 5.082755093536325930, -25.34375000204838813, -5.082755093536325042 ) ) ;
#36351 = VECTOR ( 'NONE', #63254, 1000.000000000000000 ) ;
#36352 = CARTESIAN_POINT ( 'NONE',  ( 46.00000000000000000, 488.0336798547363628, -0.8984331811833941028 ) ) ;
#36353 = ORIENTED_EDGE ( 'NONE', *, *, #31441, .T. ) ;
#36354 = CARTESIAN_POINT ( 'NONE',  ( 43.41290683822506935, 487.0833545439620593, 7.569976829064905210 ) ) ;
#36355 = ORIENTED_EDGE ( 'NONE', *, *, #91786, .F. ) ;
#36356 = CARTESIAN_POINT ( 'NONE',  ( 87.04245038058458306, 1.016364837396684119E-14, 0.000000000000000000 ) ) ;
#36357 = CARTESIAN_POINT ( 'NONE',  ( 47.57308385268299844, 17.76309546253586191, -14.43907613026851422 ) ) ;
#36358 = CARTESIAN_POINT ( 'NONE',  ( -75.28337991137821916, -60.00000000000001421, -30.37543036780875028 ) ) ;
#36359 = FACE_BOUND ( 'NONE', #21570, .T. ) ;
#36360 = CARTESIAN_POINT ( 'NONE',  ( 5.082755093536325930, -29.84375000204838813, -5.082755093536325042 ) ) ;
#36361 = DIRECTION ( 'NONE',  ( 0.000000000000000000, 0.000000000000000000, -1.000000000000000000 ) ) ;
#36362 = CARTESIAN_POINT ( 'NONE',  ( 16.66764709352488083, -4.285714285714297134, 19.00223544648544660 ) ) ;
#36363 = FILL_AREA_STYLE_COLOUR ( '', #6440 ) ;
#36364 = CARTESIAN_POINT ( 'NONE',  ( -10.48543666094594684, 50.00000000000000000, -78.95657223723274853 ) ) ;
#36365 = DIRECTION ( 'NONE',  ( 0.000000000000000000, 1.000000000000000000, 0.000000000000000000 ) ) ;
#36366 = FACE_OUTER_BOUND ( 'NONE', #99883, .T. ) ;
#36367 = ADVANCED_FACE ( 'NONE', ( #96915 ), #32193, .F. ) ;
#36368 = ORIENTED_EDGE ( 'NONE', *, *, #98815, .T. ) ;
#36369 = FACE_OUTER_BOUND ( 'NONE', #36773, .T. ) ;
#36371 = CARTESIAN_POINT ( 'NONE',  ( 31.41811726210679723, -18.66951844216680811, 29.82563105361673550 ) ) ;
#36370 = DIRECTION ( 'NONE',  ( 0.000000000000000000, -1.000000000000000000, 0.000000000000000000 ) ) ;
#36372 = AXIS2_PLACEMENT_3D ( 'NONE', #60731, #10552, #92539 ) ;
#36373 = SURFACE_SIDE_STYLE ('',( #53570 ) ) ;
#36374 = VERTEX_POINT ( 'NONE', #15992 ) ;
#36375 = EDGE_CURVE ( 'NONE', #3555, #32846, #68219, .T. ) ;
#36376 = CARTESIAN_POINT ( 'NONE',  ( -2.617478843592807358, 48.00000000000000711, -75.26027323331686603 ) ) ;
#36377 = EDGE_CURVE ( 'NONE', #42645, #41303, #32046, .T. ) ;
#36378 = CIRCLE ( 'NONE', #17472, 11.00000000000001066 ) ;
#36380 = CARTESIAN_POINT ( 'NONE',  ( -19.70764564238371719, 304.7954121406193622, 9.925013215726785631 ) ) ;
#36379 = DIRECTION ( 'NONE',  ( 0.000000000000000000, 1.000000000000000000, 0.000000000000000000 ) ) ;
#36381 = CARTESIAN_POINT ( 'NONE',  ( 102.0666666666666629, 1.023464760207051730E-14, 0.000000000000000000 ) ) ;
#36382 = CARTESIAN_POINT ( 'NONE',  ( -44.24061507096541845, 485.5299576667499082, 3.142227259638529446 ) ) ;
#36383 = CARTESIAN_POINT ( 'NONE',  ( 36.36650669486618881, 1.474610560812782335E-15, 0.000000000000000000 ) ) ;
#36384 = CARTESIAN_POINT ( 'NONE',  ( -7.500000000000000000, -2.886751345948136205, -7.198902722707428481 ) ) ;
#36385 = VERTEX_POINT ( 'NONE', #55372 ) ;
#36386 = CARTESIAN_POINT ( 'NONE',  ( 91.92393271586485071, -59.99999999999997868, 7.963687493680886575 ) ) ;
#36387 = CARTESIAN_POINT ( 'NONE',  ( 33.68177706158841289, 464.5004658938951252, 17.05886715805537790 ) ) ;
#36388 = EDGE_CURVE ( 'NONE', #91492, #64161, #56037, .T. ) ;
#36389 = CARTESIAN_POINT ( 'NONE',  ( -36.69704126099654218, 379.5140801041114287, 5.019973760696065490 ) ) ;
#36390 = EDGE_CURVE ( 'NONE', #26814, #94271, #72101, .T. ) ;
#36391 =( BOUNDED_CURVE ( )  B_SPLINE_CURVE ( 2, ( #1800, #59545, #27744, #34758, #68704, #101585, #60615, #2338, #50884 ),
 .UNSPECIFIED., .F., .F. ) 
 B_SPLINE_CURVE_WITH_KNOTS ( ( 3, 2, 2, 2, 3 ),
 ( 0.7794117647058824705, 0.7867647058823530326, 0.7941176470588235947, 0.8014705882352942679, 0.8088235294117648300 ),
 .UNSPECIFIED. ) 
 CURVE ( )  GEOMETRIC_REPRESENTATION_ITEM ( )  RATIONAL_B_SPLINE_CURVE ( ( 0.9999999999999988898, 0.9238795325112878487, 1.000000000000000000, 0.9238795325112867385, 1.000000000000000000, 0.9238795325112867385, 1.000000000000000000, 0.9238795325112856283, 1.000000000000001110 ) ) 
 REPRESENTATION_ITEM ( '' )  );
#36392 = CARTESIAN_POINT ( 'NONE',  ( -6.499946559453495531, 41.29102226313802504, -70.87268749769670251 ) ) ;
#36393 = CARTESIAN_POINT ( 'NONE',  ( -13.07716338512343590, 8.367404540816639980, -8.868549848999556673 ) ) ;
#36394 = ORIENTED_EDGE ( 'NONE', *, *, #14307, .F. ) ;
#36395 = AXIS2_PLACEMENT_3D ( 'NONE', #60363, #93237, #28538 ) ;
#36396 = CARTESIAN_POINT ( 'NONE',  ( -107.1317281283567411, -29.99999999989391242, 141.4592884034056226 ) ) ;
#36397 = VERTEX_POINT ( 'NONE', #56963 ) ;
#36398 = CARTESIAN_POINT ( 'NONE',  ( -9.423567810130279554, -56.01223787097960383, 23.65038982378345622 ) ) ;
#36399 = SURFACE_SIDE_STYLE ('',( #3453 ) ) ;
#36400 = CARTESIAN_POINT ( 'NONE',  ( 6.575925811255157072, 7.701774614579012912, 6.632038761762336177E-16 ) ) ;
#36401 = CARTESIAN_POINT ( 'NONE',  ( 82.97322089956890068, -37.79799621115897423, -10.81212016393223330 ) ) ;
#36402 = CARTESIAN_POINT ( 'NONE',  ( -2.977408999572650039, -32.56250000204838813, -7.188101187500001821 ) ) ;
#36403 = CARTESIAN_POINT ( 'NONE',  ( 0.000000000000000000, 0.000000000000000000, 0.000000000000000000 ) ) ;
#36404 = CARTESIAN_POINT ( 'NONE',  ( 9.507180395704930120, 46.21450860196618038, -13.17662286211872669 ) ) ;
#36405 = ORIENTED_EDGE ( 'NONE', *, *, #55096, .F. ) ;
#36406 = DIRECTION ( 'NONE',  ( 0.000000000000000000, -1.000000000000000000, 0.000000000000000000 ) ) ;
#36407 = ORIENTED_EDGE ( 'NONE', *, *, #58152, .F. ) ;
#36408 = CARTESIAN_POINT ( 'NONE',  ( 48.80588606933620355, 9.656672550839653368, -14.61916856843063250 ) ) ;
#36409 = CARTESIAN_POINT ( 'NONE',  ( 28.50099738913158376, 5.000000000000004441, 6.123233995736770227E-16 ) ) ;
#36410 = ORIENTED_EDGE ( 'NONE', *, *, #10125, .F. ) ;
#36411 = CARTESIAN_POINT ( 'NONE',  ( 77.58893270196534786, -32.55198695177040946, 126.5507534963122254 ) ) ;
#36412 = ORIENTED_EDGE ( 'NONE', *, *, #44112, .T. ) ;
#36413 = CARTESIAN_POINT ( 'NONE',  ( 5.823258015267495757, -50.68891529089922443, 39.73205700961069908 ) ) ;
#36414 = CARTESIAN_POINT ( 'NONE',  ( 2.977408999572650927, -20.37500000204838813, -7.188101187500000933 ) ) ;
#36415 = AXIS2_PLACEMENT_3D ( 'NONE', #66462, #75069, #23918 ) ;
#36416 = CARTESIAN_POINT ( 'NONE',  ( -107.1080015683288025, -57.65528894494657663, 199.9870551016494744 ) ) ;
#36417 = EDGE_LOOP ( 'NONE', ( #23194, #18955, #78875, #87151, #18867 ) ) ;
#36418 = AXIS2_PLACEMENT_3D ( 'NONE', #74848, #64653, #90520 ) ;
#36419 = CARTESIAN_POINT ( 'NONE',  ( -34.50896137839294653, 42.67077640914953918, -63.05802169876201191 ) ) ;
#36420 = CARTESIAN_POINT ( 'NONE',  ( -5.909259836070536842, -13.86277204242069239, -1.072443315311454759 ) ) ;
#36421 = CARTESIAN_POINT ( 'NONE',  ( 6.250413015032560970, 51.28038719428062819, -8.085695086823610822 ) ) ;
#36422 = EDGE_CURVE ( 'NONE', #31296, #13541, #35526, .T. ) ;
#36423 = COLOUR_RGB ( '', 0.40784314, 0.44705882, 0.49803922) ;
#36424 = CARTESIAN_POINT ( 'NONE',  ( 49.26579422795299479, 13.23794831108222603, -15.39367580924973211 ) ) ;
#36425 = CARTESIAN_POINT ( 'NONE',  ( -3.313708498984765161, -17.65625000409677270, 7.999999999999998224 ) ) ;
#36426 = CARTESIAN_POINT ( 'NONE',  ( -50.27151869105384208, -29.73838331303861082, 47.05395887657598308 ) ) ;
#36427 = CARTESIAN_POINT ( 'NONE',  ( -36.81742733023035896, 25.76195274633174392, 13.21949667342699897 ) ) ;
#36428 = DIRECTION ( 'NONE',  ( 1.000000000000000000, 0.000000000000000000, 0.000000000000000000 ) ) ;
#36429 = PRESENTATION_STYLE_ASSIGNMENT (( #11022 ) ) ;
#36430 = CARTESIAN_POINT ( 'NONE',  ( -43.58525529925911002, 435.7810014872756028, 17.82021598409041729 ) ) ;
#36431 = APPLICATION_PROTOCOL_DEFINITION ( 'draft international standard', 'automotive_design', 1998, #1077 ) ;
#36432 = CARTESIAN_POINT ( 'NONE',  ( 33.95156263172585653, 464.5083255208626838, 6.608064661821390295 ) ) ;
#36433 = ORIENTED_EDGE ( 'NONE', *, *, #11079, .F. ) ;
#36434 = CARTESIAN_POINT ( 'NONE',  ( -0.9278645722921005090, -50.01492575961955822, 40.97002731333736847 ) ) ;
#36435 = SURFACE_STYLE_FILL_AREA ( #93029 ) ;
#36436 = DIRECTION ( 'NONE',  ( 0.9736964118527576817, 0.000000000000000000, 0.2278492869092748896 ) ) ;
#36437 = CARTESIAN_POINT ( 'NONE',  ( 76.12557658274100447, -38.35599704320050307, -28.58424740099938077 ) ) ;
#36438 = CARTESIAN_POINT ( 'NONE',  ( -86.68002163611333799, -30.00000000000000355, 182.3895294052472309 ) ) ;
#36439 = EDGE_CURVE ( 'NONE', #52915, #12822, #72681, .T. ) ;
#36440 = VECTOR ( 'NONE', #12385, 1000.000000000000000 ) ;
#36441 = VERTEX_POINT ( 'NONE', #8951 ) ;
#36442 = CARTESIAN_POINT ( 'NONE',  ( -17.17069302869450809, -4.333298119783913549, 5.126212997795625448 ) ) ;
#36443 = CARTESIAN_POINT ( 'NONE',  ( 86.38368744081424211, -57.57931805107565992, 202.8627517790685886 ) ) ;
#36444 = COLOUR_RGB ( '', 0.66274510, 0.83137255, 0.94901961) ;
#36445 = CARTESIAN_POINT ( 'NONE',  ( 9.999999999999996447, 48.00000000000000711, -83.69100306100425257 ) ) ;
#36446 = CARTESIAN_POINT ( 'NONE',  ( 28.32874302589403825, -28.95622013529227345, -38.25147845281513526 ) ) ;
#36447 = AXIS2_PLACEMENT_3D ( 'NONE', #15920, #21923, #79068 ) ;
#36448 = CARTESIAN_POINT ( 'NONE',  ( 5.036189803708992052, -3.000000000000002665, -93.73786388354254484 ) ) ;
#36449 = PRODUCT ( 'hex flange nut_din_Hexagon Flange Nut DIN 6923 - M10 - S', 'hex flange nut_din_Hexagon Flange Nut DIN 6923 - M10 - S', '', ( #20254 ) ) ;
#36450 = CARTESIAN_POINT ( 'NONE',  ( -61.21521598792825358, -60.00000000000000000, 104.5839967611049843 ) ) ;
#36451 = CARTESIAN_POINT ( 'NONE',  ( -31.05728869196802222, 439.4224417574423569, 22.81104631550758555 ) ) ;
#36452 = EDGE_CURVE ( 'NONE', #73090, #73065, #31644, .T. ) ;
#36453 = SURFACE_SIDE_STYLE ('',( #2430 ) ) ;
#36454 = CARTESIAN_POINT ( 'NONE',  ( -86.21391966553235875, -50.15659743610942201, 191.0482607519209921 ) ) ;
#36455 = ORIENTED_EDGE ( 'NONE', *, *, #50786, .T. ) ;
#36456 = DIRECTION ( 'NONE',  ( 0.5735764363510490460, 0.8191520442889896891, 0.000000000000000000 ) ) ;
#36457 = CARTESIAN_POINT ( 'NONE',  ( -3.060819570925945587, -49.92087050383263858, 32.20467130113398468 ) ) ;
#36458 = CARTESIAN_POINT ( 'NONE',  ( -6.533698963947263572, 41.84235549011117428, -59.21169165894567499 ) ) ;
#36459 = DIRECTION ( 'NONE',  ( 0.000000000000000000, 0.000000000000000000, 1.000000000000000000 ) ) ;
#36460 =( LENGTH_UNIT ( ) NAMED_UNIT ( * ) SI_UNIT ( .MILLI., .METRE. ) );
#36461 = ORIENTED_EDGE ( 'NONE', *, *, #23083, .T. ) ;
#36462 = CIRCLE ( 'NONE', #58827, 8.000000000000000000 ) ;
#36463 = CARTESIAN_POINT ( 'NONE',  ( -36.54584131692897131, 364.1367592788530487, 3.156418272699054395 ) ) ;
#36464 = DIRECTION ( 'NONE',  ( 0.000000000000000000, -0.4999999999999999445, 0.8660254037844385966 ) ) ;
#36465 = DIRECTION ( 'NONE',  ( -1.000000000000000000, -1.224606353822377258E-16, -0.000000000000000000 ) ) ;
#36466 = ORIENTED_EDGE ( 'NONE', *, *, #84552, .F. ) ;
#36467 = CARTESIAN_POINT ( 'NONE',  ( 17.54033449406726675, 50.00000000000000711, 62.99969680185511578 ) ) ;
#36468 = CARTESIAN_POINT ( 'NONE',  ( 45.40507512465600115, 439.2794387026467575, 6.273370203490043373 ) ) ;
#36469 = CARTESIAN_POINT ( 'NONE',  ( -13.66642973270730010, -3.469446951953614189E-15, -17.78317311658304689 ) ) ;
#36470 = DIRECTION ( 'NONE',  ( -1.000000000000000000, -1.224606353822377258E-16, -0.000000000000000000 ) ) ;
#36471 = CARTESIAN_POINT ( 'NONE',  ( 98.48959774644481513, -29.99999999999997158, 87.89110648026155559 ) ) ;
#36472 = CARTESIAN_POINT ( 'NONE',  ( -78.98497190652808797, -60.32446057300273878, 164.7472437911728207 ) ) ;
#36473 = ORIENTED_EDGE ( 'NONE', *, *, #35758, .T. ) ;
#36474 = CARTESIAN_POINT ( 'NONE',  ( -13.00000000000003730, 249.9999999999999432, -4.000000000000002665 ) ) ;
#36475 = CARTESIAN_POINT ( 'NONE',  ( 20.11650669486618881, 4.898587196589411843E-16, -4.000000000000000888 ) ) ;
#36476 = CARTESIAN_POINT ( 'NONE',  ( 21.65479446793900919, -57.67253147474830399, 42.45767589424171717 ) ) ;
#36477 = DIRECTION ( 'NONE',  ( 0.000000000000000000, -1.000000000000000000, 0.000000000000000000 ) ) ;
#36478 = B_SPLINE_CURVE_WITH_KNOTS ( 'NONE', 3,
 ( #94773, #93696, #77511, #94227, #10627, #20392 ),
 .UNSPECIFIED., .F., .F.,
 ( 4, 2, 4 ),
 ( -5.145455527296411814E-06, 0.0004153350442917297554, 0.0008358155441107577039 ),
 .UNSPECIFIED. ) ;
#36479 = CARTESIAN_POINT ( 'NONE',  ( 42.63769942292682202, 336.9641833527253425, 8.128834346956653079 ) ) ;
#36480 = CARTESIAN_POINT ( 'NONE',  ( 43.69307663853744117, 464.9794299858319278, 8.444152807414981865 ) ) ;
#36481 = ORIENTED_EDGE ( 'NONE', *, *, #105830, .F. ) ;
#36482 = UNCERTAINTY_MEASURE_WITH_UNIT (LENGTH_MEASURE( 1.000000000000000082E-05 ), #97775, 'distance_accuracy_value', 'NONE');
#36483 = DIRECTION ( 'NONE',  ( 0.000000000000000000, 1.000000000000000000, 0.000000000000000000 ) ) ;
#36484 = FACE_OUTER_BOUND ( 'NONE', #66706, .T. ) ;
#36485 = CARTESIAN_POINT ( 'NONE',  ( 7.188101187499999156, -26.75000000204838457, 2.977408999572654924 ) ) ;
#36486 = ORIENTED_EDGE ( 'NONE', *, *, #65954, .T. ) ;
#36487 =( NAMED_UNIT ( * ) SI_UNIT ( $, .STERADIAN. ) SOLID_ANGLE_UNIT ( ) );
#36488 = CARTESIAN_POINT ( 'NONE',  ( -4.165977904505308693, 16.00000000000000000, 9.090909090909091717 ) ) ;
#36489 = CARTESIAN_POINT ( 'NONE',  ( 5.625019092414621724, 41.66287055497627279, -70.61600277306789053 ) ) ;
#36490 = CARTESIAN_POINT ( 'NONE',  ( 11.54772599577024295, 50.00000000000000000, 62.20121126512098186 ) ) ;
#36491 = DIRECTION ( 'NONE',  ( 0.000000000000000000, -1.000000000000000000, 0.000000000000000000 ) ) ;
#36492 = CARTESIAN_POINT ( 'NONE',  ( -23.85899507165724032, 27.29461519911105682, -33.04201830783522809 ) ) ;
#36493 = ORIENTED_EDGE ( 'NONE', *, *, #100708, .T. ) ;
#36494 = CARTESIAN_POINT ( 'NONE',  ( 71.14491545185333621, -59.99999999999998579, -32.14747307439793644 ) ) ;
#36496 = CARTESIAN_POINT ( 'NONE',  ( 21.13798171326017439, -32.51397013334567987, 29.94121226608427833 ) ) ;
#36495 = CARTESIAN_POINT ( 'NONE',  ( -70.38749560794603610, -14.21045842199435860, 117.5518806561683078 ) ) ;
#36497 = CARTESIAN_POINT ( 'NONE',  ( 110.0428892116504755, 17.51648154115788358, 55.02144460582527330 ) ) ;
#36498 = CARTESIAN_POINT ( 'NONE',  ( -35.45552176936942601, -32.57855910578506808, 34.20812180394899826 ) ) ;
#36499 = EDGE_CURVE ( 'NONE', #21601, #4872, #50466, .T. ) ;
#36500 = PRESENTATION_LAYER_ASSIGNMENT (  '', '', ( #69184 ) ) ;
#36501 = UNCERTAINTY_MEASURE_WITH_UNIT (LENGTH_MEASURE( 1.000000000000000082E-05 ), #82971, 'distance_accuracy_value', 'NONE');
#36502 = ORIENTED_EDGE ( 'NONE', *, *, #28385, .F. ) ;
#36503 = CARTESIAN_POINT ( 'NONE',  ( -13.69901872062297166, -56.64640036516345134, 24.10656755472290769 ) ) ;
#36504 = CARTESIAN_POINT ( 'NONE',  ( -1.216929526016031105, 51.81227483227483788, -8.673337395590676735 ) ) ;
#36505 = CARTESIAN_POINT ( 'NONE',  ( 7.150053860865848598, -63.21734546086022988, 3.590189269391292015 ) ) ;
#36506 = CARTESIAN_POINT ( 'NONE',  ( -14.58597127886929101, 5.499146323188746521, 6.679532531467523349 ) ) ;
#36507 = ORIENTED_EDGE ( 'NONE', *, *, #62702, .T. ) ;
#36508 = CARTESIAN_POINT ( 'NONE',  ( -57.77825852280871999, -38.34426397139789344, 89.58174797475106743 ) ) ;
#36509 = ORIENTED_EDGE ( 'NONE', *, *, #57360, .T. ) ;
#36510 = CARTESIAN_POINT ( 'NONE',  ( 90.31977347436274783, -30.00000000000004619, 190.1102673397166996 ) ) ;
#36511 = CARTESIAN_POINT ( 'NONE',  ( -13.92190297528754783, 2.732557955353745349, -5.556343985222209625 ) ) ;
#36512 = CARTESIAN_POINT ( 'NONE',  ( -5.094000037296078531, -82.55365876228779598, -3.174960020027664420 ) ) ;
#36513 = ADVANCED_FACE ( 'NONE', ( #8424 ), #1986, .T. ) ;
#36514 = CARTESIAN_POINT ( 'NONE',  ( 80.84952124054477451, -30.00000000000000000, -12.29353673406206937 ) ) ;
#36515 = EDGE_CURVE ( 'NONE', #46431, #71163, #1995, .T. ) ;
#36516 = CARTESIAN_POINT ( 'NONE',  ( -32.19467125704959187, 397.8372596365960021, 25.61661318660594944 ) ) ;
#36517 = VERTEX_POINT ( 'NONE', #39090 ) ;
#36518 = CONICAL_SURFACE ( 'NONE', #88139, 4.000000000000001776, 0.9599310885968774798 ) ;
#36519 = VERTEX_POINT ( 'NONE', #78998 ) ;
#36520 = EDGE_LOOP ( 'NONE', ( #91345, #43733, #28180, #48763 ) ) ;
#36521 = CYLINDRICAL_SURFACE ( 'NONE', #29744, 4.000000000000000888 ) ;
#36522 = CARTESIAN_POINT ( 'NONE',  ( 40.54980110599892384, 41.80014750453505457, -54.75324010490675164 ) ) ;
#36523 = FACE_OUTER_BOUND ( 'NONE', #82021, .T. ) ;
#36524 = AXIS2_PLACEMENT_3D ( 'NONE', #47184, #102380, #88725 ) ;
#36525 = CARTESIAN_POINT ( 'NONE',  ( 5.858824175751779606, -13.78579060872359463, -1.318356988357140214 ) ) ;
#36526 = LINE ( 'NONE', #49050, #103798 ) ;
#36527 = CARTESIAN_POINT ( 'NONE',  ( 5.372128395027464975, 54.18872941621413730, 6.031152949374466665 ) ) ;
#36528 = ORIENTED_EDGE ( 'NONE', *, *, #88915, .T. ) ;
#36529 = CARTESIAN_POINT ( 'NONE',  ( 11.68767211932355998, 50.00000000000000000, -88.14097461399491351 ) ) ;
#36530 = CIRCLE ( 'NONE', #98515, 5.000000000000002665 ) ;
#36531 = ORIENTED_EDGE ( 'NONE', *, *, #44946, .F. ) ;
#36532 = CARTESIAN_POINT ( 'NONE',  ( -5.725989721596477011, -61.42322888743539977, 1.809923354557184894 ) ) ;
#36533 = CARTESIAN_POINT ( 'NONE',  ( 60.80738147631894464, -38.34211472478318683, 98.97440318161500272 ) ) ;
#36534 = CARTESIAN_POINT ( 'NONE',  ( 8.000000000000000000, -11.18750000409677092, 0.000000000000000000 ) ) ;
#36535 = CARTESIAN_POINT ( 'NONE',  ( 22.71368435182198553, 303.3994564710546342, 10.05503188144461291 ) ) ;
#36536 = CARTESIAN_POINT ( 'NONE',  ( 19.83349330513379982, 4.000000000000003553, 0.000000000000000000 ) ) ;
#36537 = CARTESIAN_POINT ( 'NONE',  ( 59.97331936630651228, -36.01454316455284754, 70.51342924789160804 ) ) ;
#36538 = ORIENTED_EDGE ( 'NONE', *, *, #43704, .T. ) ;
#36539 = LINE ( 'NONE', #78017, #9994 ) ;
#36540 = CARTESIAN_POINT ( 'NONE',  ( 23.86650669486618881, -3.999999999999998224, 0.000000000000000000 ) ) ;
#36541 = CARTESIAN_POINT ( 'NONE',  ( -5.763898627153208665, 12.46274061085392759, -3.972597389303859750 ) ) ;
#36542 = CARTESIAN_POINT ( 'NONE',  ( -30.38238271166500937, 438.0643985706049648, 22.32817737084010190 ) ) ;
#36543 = B_SPLINE_CURVE_WITH_KNOTS ( 'NONE', 3,
 ( #3569, #78502, #45104, #94722, #37028, #4636, #37565, #101723 ),
 .UNSPECIFIED., .F., .F.,
 ( 4, 2, 2, 4 ),
 ( 0.003797433802554438936, 0.004743183970586236156, 0.005688934138618033376, 0.007580434474681626948 ),
 .UNSPECIFIED. ) ;
#36544 = EDGE_LOOP ( 'NONE', ( #17198, #44590, #25576, #19820, #83101 ) ) ;
#36545 = CARTESIAN_POINT ( 'NONE',  ( 0.000000000000000000, 0.000000000000000000, -6.275264681066861527 ) ) ;
#36546 = DIRECTION ( 'NONE',  ( 0.000000000000000000, 0.000000000000000000, 1.000000000000000000 ) ) ;
#36547 = CARTESIAN_POINT ( 'NONE',  ( 39.44615384615384812, 1.411358822780289120E-15, 0.000000000000000000 ) ) ;
#36548 = CYLINDRICAL_SURFACE ( 'NONE', #49030, 4.000000000000000000 ) ;
#36549 = DIRECTION ( 'NONE',  ( 0.000000000000000000, 0.000000000000000000, -1.000000000000000000 ) ) ;
#36550 = SURFACE_STYLE_USAGE ( .BOTH. , #2530 ) ;
#36551 = EDGE_CURVE ( 'NONE', #45751, #98120, #106072, .T. ) ;
#36552 = DIRECTION ( 'NONE',  ( 0.000000000000000000, 0.000000000000000000, 1.000000000000000000 ) ) ;
#36553 = CARTESIAN_POINT ( 'NONE',  ( 86.52296945539703188, -31.80420732485877977, 185.9741549876141562 ) ) ;
#36554 = CARTESIAN_POINT ( 'NONE',  ( 44.30168388726523432, 463.8374982934681725, 7.948620458287060764 ) ) ;
#36555 = CARTESIAN_POINT ( 'NONE',  ( -7.883792884227283082, 61.98032949398166380, 5.000000000000000888 ) ) ;
#36556 = EDGE_LOOP ( 'NONE', ( #15756, #27300, #19656 ) ) ;
#36557 = STYLED_ITEM ( 'NONE', ( #52141 ), #82390 ) ;
#36558 = CARTESIAN_POINT ( 'NONE',  ( 66.68220009426445927, -29.86615941953475684, -22.35219315092264836 ) ) ;
#36559 = DIRECTION ( 'NONE',  ( -1.000000000000000000, -1.224606353822377258E-16, -0.000000000000000000 ) ) ;
#36560 = CARTESIAN_POINT ( 'NONE',  ( 5.691929483231184861, -4.336808689942017736E-16, 6.500000000000001776 ) ) ;
#36561 = CARTESIAN_POINT ( 'NONE',  ( 35.32911723019127237, 437.0667969981781198, 5.602639083905786244 ) ) ;
#36562 = COLOUR_RGB ( '', 0.40784314, 0.44705882, 0.49803922) ;
#36563 = CARTESIAN_POINT ( 'NONE',  ( -83.15749301179586439, -30.00000000000000355, 44.16248718578879107 ) ) ;
#36564 = EDGE_CURVE ( 'NONE', #31296, #56662, #80045, .T. ) ;
#36565 = CARTESIAN_POINT ( 'NONE',  ( 44.35000000000000142, -3.309499999999999886, 4.475777889183790779E-16 ) ) ;
#36566 = VECTOR ( 'NONE', #16405, 1000.000000000000000 ) ;
#36567 = CARTESIAN_POINT ( 'NONE',  ( 5.530835398441388051, -57.67122193196713908, 41.60095799607574207 ) ) ;
#36569 = LINE ( 'NONE', #43554, #51654 ) ;
#36568 = CARTESIAN_POINT ( 'NONE',  ( -9.333892298909287177, 248.2172426837495891, -3.590295303293448370 ) ) ;
#36570 = VECTOR ( 'NONE', #60814, 1000.000000000000000 ) ;
#36571 = PRESENTATION_STYLE_ASSIGNMENT (( #78047 ) ) ;
#36572 = CARTESIAN_POINT ( 'NONE',  ( -3.821462797104940634, -18.99812766127876174, 27.04963633765945374 ) ) ;
#36573 = CARTESIAN_POINT ( 'NONE',  ( -17.51746965587035376, 50.00000000000000711, 63.25210749506708652 ) ) ;
#36574 = CARTESIAN_POINT ( 'NONE',  ( -43.71217423904474231, 435.6632154632216043, 9.092528312227496912 ) ) ;
#36575 = LINE ( 'NONE', #62939, #70136 ) ;
#36576 = CARTESIAN_POINT ( 'NONE',  ( 27.01940400982110546, -20.71597891303181527, -32.68677040832736225 ) ) ;
#36577 = B_SPLINE_CURVE_WITH_KNOTS ( 'NONE', 3,
 ( #77694, #21606, #28112, #86337, #62576, #94954, #44264, #53926, #12402, #45334, #29703, #54437, #60987, #85804, #78214, #3803, #86857, #61526, #87385, #13461, #101435, #44805, #77155, #2723, #12933, #27587, #36743, #45853, #20033, #78727, #11878, #69605, #4865, #85248 ),
 .UNSPECIFIED., .F., .F.,
 ( 4, 2, 2, 2, 2, 2, 2, 2, 2, 2, 2, 2, 2, 2, 2, 2, 4 ),
 ( 0.01263889472610568547, 0.01342810546992896127, 0.01421731621375223707, 0.01500652695757551114, 0.01579573770139878694, 0.01658494844522206274, 0.01737415918904533854, 0.01816336993286861434, 0.01895258067669189014, 0.01974179142051516594, 0.02053100216433844175, 0.02132021290816171755, 0.02210942365198499335, 0.02289863439580826915, 0.02368784513963154842, 0.02447705588345482075, 0.02526626662727809655 ),
 .UNSPECIFIED. ) ;
#36578 = EDGE_CURVE ( 'NONE', #77668, #25666, #94087, .T. ) ;
#36579 = CARTESIAN_POINT ( 'NONE',  ( -23.90155539105087001, -46.43881993149235399, 32.71507686279078797 ) ) ;
#36580 = ORIENTED_EDGE ( 'NONE', *, *, #60700, .F. ) ;
#36581 = CARTESIAN_POINT ( 'NONE',  ( 41.14690903223204543, 485.7356601713281066, -4.640470638256346980 ) ) ;
#36582 = CARTESIAN_POINT ( 'NONE',  ( -18.55741136884755704, -18.59012425588017692, 27.35021598045728908 ) ) ;
#36583 = ADVANCED_FACE ( 'NONE', ( #29946 ), #56160, .T. ) ;
#36584 = CARTESIAN_POINT ( 'NONE',  ( -33.00000000000000000, 500.0000000000002274, -15.00000000000000711 ) ) ;
#36585 = ORIENTED_EDGE ( 'NONE', *, *, #82608, .T. ) ;
#36586 = CIRCLE ( 'NONE', #101981, 4.000000000000000888 ) ;
#36587 = CARTESIAN_POINT ( 'NONE',  ( 27.61650669486618881, 1.474610560812782335E-15, 0.000000000000000000 ) ) ;
#36588 = ORIENTED_EDGE ( 'NONE', *, *, #36180, .T. ) ;
#36589 = CARTESIAN_POINT ( 'NONE',  ( -9.289581398512320121, 50.00000000000000711, -94.32893702008476566 ) ) ;
#36590 = ADVANCED_FACE ( 'NONE', ( #71970 ), #17134, .F. ) ;
#36591 = FILL_AREA_STYLE ('',( #34983 ) ) ;
#36592 = DIRECTION ( 'NONE',  ( 0.000000000000000000, -1.000000000000000000, 0.000000000000000000 ) ) ;
#36593 = ORIENTED_EDGE ( 'NONE', *, *, #48124, .F. ) ;
#36594 = CARTESIAN_POINT ( 'NONE',  ( 43.75010090114224681, 464.8337800386878484, 11.75004750934975029 ) ) ;
#36595 =( LENGTH_UNIT ( ) NAMED_UNIT ( * ) SI_UNIT ( .MILLI., .METRE. ) );
#36596 = CARTESIAN_POINT ( 'NONE',  ( 100.0337298755554230, -37.84183079272108330, 190.5202142185493699 ) ) ;
#36597 = PRESENTATION_LAYER_ASSIGNMENT (  '', '', ( #55467 ) ) ;
#36599 = CARTESIAN_POINT ( 'NONE',  ( -7.150931910075644993, -8.213742014777372091, -3.588457848165353514 ) ) ;
#36598 =( NAMED_UNIT ( * ) SI_UNIT ( $, .STERADIAN. ) SOLID_ANGLE_UNIT ( ) );
#36600 = VERTEX_POINT ( 'NONE', #41721 ) ;
#36601 = EDGE_CURVE ( 'NONE', #70163, #37934, #87178, .T. ) ;
#36602 = ORIENTED_EDGE ( 'NONE', *, *, #15197, .T. ) ;
#36603 = ORIENTED_EDGE ( 'NONE', *, *, #37199, .F. ) ;
#36604 = CARTESIAN_POINT ( 'NONE',  ( 25.26398632472819727, 307.7598616557737046, 9.603387314540041686 ) ) ;
#36605 = DIRECTION ( 'NONE',  ( -0.000000000000000000, -1.000000000000000000, -0.000000000000000000 ) ) ;
#36606 = SURFACE_STYLE_USAGE ( .BOTH. , #44132 ) ;
#36607 = ORIENTED_EDGE ( 'NONE', *, *, #84176, .F. ) ;
#36608 = DIRECTION ( 'NONE',  ( 0.000000000000000000, 0.000000000000000000, 1.000000000000000000 ) ) ;
#36609 = CARTESIAN_POINT ( 'NONE',  ( -6.302263409432467434, 41.90661423625755333, -70.03646363488827831 ) ) ;
#36610 = CARTESIAN_POINT ( 'NONE',  ( -14.08095268206308504, -59.99999999999999289, -44.59230323635646442 ) ) ;
#36611 = FACE_OUTER_BOUND ( 'NONE', #100221, .T. ) ;
#36612 = CARTESIAN_POINT ( 'NONE',  ( 30.07770292690122815, -60.00000000000002132, 43.07392525451504639 ) ) ;
#36613 = CARTESIAN_POINT ( 'NONE',  ( 6.643884894376894223, 3.901062859471879030, -6.756839076125894294 ) ) ;
#36614 = CARTESIAN_POINT ( 'NONE',  ( -13.88435755502521474, 42.00000000000000000, -90.88030988970933777 ) ) ;
#36616 = CARTESIAN_POINT ( 'NONE',  ( 8.339588973682309003, -60.35896782574766917, 33.94344157875258361 ) ) ;
#36615 = CARTESIAN_POINT ( 'NONE',  ( -107.5810679786090702, -30.00000000000002487, 145.3413084537935163 ) ) ;
#36617 = CARTESIAN_POINT ( 'NONE',  ( 23.09999999999999432, -3.309499999999999886, 4.475777889183790779E-16 ) ) ;
#36618 = CARTESIAN_POINT ( 'NONE',  ( -48.09415955654135644, -32.60490053195846372, 45.64808559464792381 ) ) ;
#36619 = ORIENTED_EDGE ( 'NONE', *, *, #92466, .T. ) ;
#36620 = DIRECTION ( 'NONE',  ( -1.000000000000000000, -1.224606353822377258E-16, -0.000000000000000000 ) ) ;
#36621 = ORIENTED_EDGE ( 'NONE', *, *, #26556, .T. ) ;
#36622 = CARTESIAN_POINT ( 'NONE',  ( 0.6238343018367229487, 8.124960217122801254, -51.58729135945497291 ) ) ;
#36623 = DIRECTION ( 'NONE',  ( 0.000000000000000000, 0.000000000000000000, 1.000000000000000000 ) ) ;
#36624 = DIRECTION ( 'NONE',  ( -1.000000000000000000, -0.000000000000000000, -0.000000000000000000 ) ) ;
#36625 = ORIENTED_EDGE ( 'NONE', *, *, #105352, .T. ) ;
#36626 = VERTEX_POINT ( 'NONE', #64938 ) ;
#36627 = CARTESIAN_POINT ( 'NONE',  ( 90.04388030624265582, -29.99999999999673861, -4.623977600603863536 ) ) ;
#36628 = CARTESIAN_POINT ( 'NONE',  ( -80.00000000000000000, -52.00000000000000000, -19.09707704303353282 ) ) ;
#36629 = CARTESIAN_POINT ( 'NONE',  ( -52.56483885390524335, 49.99999999999999289, -38.23529411764707220 ) ) ;
#36630 = COLOUR_RGB ( '', 0.09019608, 0.27058824, 0.51372549) ;
#36631 = CARTESIAN_POINT ( 'NONE',  ( -3.730558560396409096, -11.49689693085219311, -10.68063119932392802 ) ) ;
#36632 = CARTESIAN_POINT ( 'NONE',  ( 57.69562748396959506, 41.99999999991776178, -15.50526908263404735 ) ) ;
#36633 = CARTESIAN_POINT ( 'NONE',  ( 98.42221274954739840, -29.99999999999999645, 189.9688103559335843 ) ) ;
#36634 = AXIS2_PLACEMENT_3D ( 'NONE', #5754, #5237, #62417 ) ;
#36635 = ADVANCED_FACE ( 'NONE', ( #57889 ), #69983, .T. ) ;
#36636 = CARTESIAN_POINT ( 'NONE',  ( -32.89533925684112603, 465.6911419323517975, 10.83014164272533542 ) ) ;
#36637 = ORIENTED_EDGE ( 'NONE', *, *, #52739, .T. ) ;
#36638 = ORIENTED_EDGE ( 'NONE', *, *, #27728, .F. ) ;
#36639 = ORIENTED_EDGE ( 'NONE', *, *, #1475, .F. ) ;
#36640 = CARTESIAN_POINT ( 'NONE',  ( 54.06037389446854036, -56.84474632814804806, 65.24979699813212619 ) ) ;
#36641 = CARTESIAN_POINT ( 'NONE',  ( 6.802270527994665805, 41.53789237612667762, -58.74929213582391441 ) ) ;
#36642 = VECTOR ( 'NONE', #47191, 1000.000000000000000 ) ;
#36643 = EDGE_CURVE ( 'NONE', #55983, #51415, #30351, .T. ) ;
#36644 = CARTESIAN_POINT ( 'NONE',  ( 0.000000000000000000, 152.0000000000000000, 0.000000000000000000 ) ) ;
#36645 = EDGE_CURVE ( 'NONE', #48387, #25099, #14792, .T. ) ;
#36646 = VERTEX_POINT ( 'NONE', #42242 ) ;
#36647 = CARTESIAN_POINT ( 'NONE',  ( -91.44502381616234743, -38.39034967759808836, -8.065114872009855773 ) ) ;
#36648 = ORIENTED_EDGE ( 'NONE', *, *, #36578, .T. ) ;
#36649 = CARTESIAN_POINT ( 'NONE',  ( 0.4042117618284710723, -3.141900367810050110, -6.500000000000000888 ) ) ;
#36650 = CARTESIAN_POINT ( 'NONE',  ( 110.4228564477537731, -38.35603995587537440, 183.0518417510637903 ) ) ;
#36651 = CARTESIAN_POINT ( 'NONE',  ( 10.06130352118416660, 12.96572514657750474, 10.57352155064043231 ) ) ;
#36652 = CARTESIAN_POINT ( 'NONE',  ( 85.16482653615426557, -52.71016913870263920, 3.865994483585396768 ) ) ;
#36653 = CARTESIAN_POINT ( 'NONE',  ( 39.77617528725443208, 332.6151105793712190, 19.06785702275038119 ) ) ;
#36654 = CARTESIAN_POINT ( 'NONE',  ( 6.163128221575932209, -12.12876728480159372, -8.844179776184985187 ) ) ;
#36655 = EDGE_CURVE ( 'NONE', #91003, #55140, #37306, .T. ) ;
#36656 = CARTESIAN_POINT ( 'NONE',  ( 6.168902648239040332, 0.6556005035805820835, 6.499999999999999112 ) ) ;
#36657 = CARTESIAN_POINT ( 'NONE',  ( -43.69860345152756764, 434.4324800463848533, 11.31831452736303945 ) ) ;
#36658 = CARTESIAN_POINT ( 'NONE',  ( 9.300689190519850769, 140.6377497888998391, 8.673617379410147005E-16 ) ) ;
#36659 = ORIENTED_EDGE ( 'NONE', *, *, #17401, .T. ) ;
#36660 = COLOUR_RGB ( '', 0.31764706, 0.68627451, 0.89019608) ;
#36661 = CARTESIAN_POINT ( 'NONE',  ( 7.187174312956649658, 40.29457745722108086, -70.92326172191368983 ) ) ;
#36662 = CARTESIAN_POINT ( 'NONE',  ( -32.17889379758944557, 439.3695696554026426, 23.63219374846805820 ) ) ;
#36663 = ORIENTED_EDGE ( 'NONE', *, *, #91155, .F. ) ;
#36664 = CARTESIAN_POINT ( 'NONE',  ( -29.57788238113521828, 311.1740376248832831, -7.528724879610501297 ) ) ;
#36665 = B_SPLINE_CURVE_WITH_KNOTS ( 'NONE', 3,
 ( #69780, #12581, #29875, #54095, #37975, #85982, #21782, #3447, #95648, #102671, #20749, #102131, #77336, #103728, #46035, #45514, #79447, #94602, #94048, #61709, #37441, #62752, #87038, #70836, #12055, #54616, #36393, #87558, #63282, #44440 ),
 .UNSPECIFIED., .F., .F.,
 ( 4, 2, 2, 2, 2, 2, 2, 2, 2, 2, 2, 2, 2, 2, 4 ),
 ( 0.02276231911146334164, 0.02503730341472417895, 0.02617479556635459934, 0.02731228771798501972, 0.02844977986961544011, 0.02958727202124586050, 0.03186225632450671863, 0.03243100240032192882, 0.03299974847613713902, 0.03413724062776756635, 0.03527473277939799368, 0.03641222493102841407, 0.03754971708265884139, 0.03868720923428926872, 0.04096219353755012338 ),
 .UNSPECIFIED. ) ;
#36666 = CARTESIAN_POINT ( 'NONE',  ( -37.63844833726898997, 314.2537075340847537, 14.63743747242352278 ) ) ;
#36667 = DIRECTION ( 'NONE',  ( 0.000000000000000000, -1.000000000000000000, 0.000000000000000000 ) ) ;
#36668 = CARTESIAN_POINT ( 'NONE',  ( 23.58349330513380337, 1.593028355512270567E-15, 0.000000000000000000 ) ) ;
#36669 = CARTESIAN_POINT ( 'NONE',  ( -5.656854249492381470, -20.56249999999999289, 5.656854249492379694 ) ) ;
#36670 = AXIS2_PLACEMENT_3D ( 'NONE', #23779, #66868, #99755 ) ;
#36671 = CARTESIAN_POINT ( 'NONE',  ( -48.90696361353268884, -29.46655839692037304, 44.90436084855983268 ) ) ;
#36672 = B_SPLINE_CURVE_WITH_KNOTS ( 'NONE', 3,
 ( #95313, #53776, #20941, #37645, #21445, #61902, #37109, #46750, #29549, #104991, #103396, #46228, #96384, #38166, #69969, #102871, #79640, #31134, #86706, #5756, #12778, #88805, #14357, #63485, #47269, #30064, #104444, #21973, #96899, #64022, #87223, #45696, #30596, #78577, #22513, #95842, #71024, #70508, #54282, #80165, #62946, #62419, #6269, #79116, #38676, #23032, #5239, #103915, #54827, #71542, #55866, #88282, #55353, #39208, #81743, #57473, #7865, #97402, #23564, #17047, #82833, #16501, #32171, #40772, #81218, #82295, #41837, #90399 ),
 .UNSPECIFIED., .F., .F.,
 ( 4, 2, 2, 2, 2, 2, 2, 2, 2, 2, 2, 2, 2, 2, 2, 2, 2, 2, 2, 2, 2, 2, 2, 2, 2, 2, 2, 2, 2, 2, 2, 2, 2, 4 ),
 ( 0.1506134683214106484, 0.1514461594375161591, 0.1522788505536216697, 0.1539442327858326909, 0.1556096150180437121, 0.1572749972502547333, 0.1606057617146767758, 0.1639365261790988182, 0.1705980551079429031, 0.1772595840367869879, 0.1839211129656310728, 0.1905826418944751577, 0.1972441708233192426, 0.2039056997521633274, 0.2172287576098514972, 0.2305518154675396392, 0.2571979311829159509, 0.2838440468982922349, 0.2971671047559804046, 0.3104901626136685744, 0.3238132204713566886, 0.3304747494002007180, 0.3371362783290448029, 0.3437978072578888877, 0.3471285717223109302, 0.3504593361867328616, 0.3537901006511549040, 0.3554554828833658697, 0.3571208651155768354, 0.3579535562316823460, 0.3587862473477878567, 0.3604516295799988779, 0.3621170118122099546, 0.3637823940444209758 ),
 .UNSPECIFIED. ) ;
#36673 = EDGE_CURVE ( 'NONE', #47025, #87124, #16132, .T. ) ;
#36674 = CARTESIAN_POINT ( 'NONE',  ( 42.68083702883374997, 436.2686870323771018, 7.148029379848829912 ) ) ;
#36675 = CIRCLE ( 'NONE', #26362, 57.86910460382442523 ) ;
#36676 = VERTEX_POINT ( 'NONE', #48207 ) ;
#36677 = CARTESIAN_POINT ( 'NONE',  ( 84.65060209411045378, -39.39181383550964455, 182.1002992804161806 ) ) ;
#36678 = LINE ( 'NONE', #69540, #98036 ) ;
#36679 = CARTESIAN_POINT ( 'NONE',  ( 71.14984002819953446, 4.000000000000015099, 4.898587196589422689E-16 ) ) ;
#36680 = EDGE_LOOP ( 'NONE', ( #13833, #102207 ) ) ;
#36681 = CARTESIAN_POINT ( 'NONE',  ( -95.18091335215243021, -45.26558765076902091, 101.5330899563590350 ) ) ;
#36682 = CARTESIAN_POINT ( 'NONE',  ( 5.691929483231186637, -3.469446951953614189E-15, -6.500000000000000000 ) ) ;
#36683 = CARTESIAN_POINT ( 'NONE',  ( 14.73122683063088445, -5.000000000000002665, -81.05502296679124186 ) ) ;
#36684 = CARTESIAN_POINT ( 'NONE',  ( 28.09999999999999787, 1.533819458162526451E-15, 0.000000000000000000 ) ) ;
#36685 = CARTESIAN_POINT ( 'NONE',  ( 5.947762761376478302, -2.501851166488387790, -6.500000000000002665 ) ) ;
#36686 =( BOUNDED_SURFACE ( )  B_SPLINE_SURFACE ( 3, 2, ( 
 ( #29159, #4300, #86308 ),
 ( #78185, #53901, #37235 ),
 ( #44778, #70096, #62033 ),
 ( #18932, #2151, #51773 ) ),
 .UNSPECIFIED., .F., .F., .F. ) 
 B_SPLINE_SURFACE_WITH_KNOTS ( ( 4, 4 ),
 ( 3, 3 ),
 ( 0.05563112469177167174, 0.08036552975359016748 ),
 ( 0.000000000000000000, 0.6299180559300312510 ),
 .UNSPECIFIED. ) 
 GEOMETRIC_REPRESENTATION_ITEM ( )  RATIONAL_B_SPLINE_SURFACE ( (
 ( 1.000000000000000000, 0.8155016482959264179, 0.8634409826473032901),
 ( 1.000000000000000000, 0.8155019398125198382, 0.8634411984173584464),
 ( 1.000000000000000000, 0.8155018685912485132, 0.8634411457019453007),
 ( 1.000000000000000000, 0.8155015759137222986, 0.8634409290726094977) ) ) 
 REPRESENTATION_ITEM ( '' )  SURFACE ( )  );
#36687 = EDGE_CURVE ( 'NONE', #15047, #1743, #79188, .T. ) ;
#36688 = FILL_AREA_STYLE_COLOUR ( '', #31710 ) ;
#36689 = CARTESIAN_POINT ( 'NONE',  ( 13.12308708762594911, -59.99999999999999289, 39.71877776328085474 ) ) ;
#36690 = CARTESIAN_POINT ( 'NONE',  ( 20.28905229919182318, -25.89519513380055926, 36.90487281070432601 ) ) ;
#36691 = CARTESIAN_POINT ( 'NONE',  ( 1.545731922506520251, -0.02842019995825076015, 101.5782547351753351 ) ) ;
#36692 = CARTESIAN_POINT ( 'NONE',  ( 34.04917345139565299, -23.61692477459231654, 33.16394827626064057 ) ) ;
#36694 = CARTESIAN_POINT ( 'NONE',  ( -14.80696975987319242, 21.98616633791558783, 4.396263791233566920 ) ) ;
#36693 = CARTESIAN_POINT ( 'NONE',  ( 45.94900261086841198, 1.482358050883964840E-15, 0.000000000000000000 ) ) ;
#36695 = CARTESIAN_POINT ( 'NONE',  ( 3.610928089892441850, 295.9072949364349938, -10.00534087566975572 ) ) ;
#36696 = CARTESIAN_POINT ( 'NONE',  ( 43.29658055318886767, 324.1952503670673877, -2.852919881210743913 ) ) ;
#36697 = CARTESIAN_POINT ( 'NONE',  ( 22.25669491856071858, 1.482358050883964840E-15, 0.000000000000000000 ) ) ;
#36698 = CARTESIAN_POINT ( 'NONE',  ( 6.289692432696767810, 6.589071317540670769, -2.245373559998994573 ) ) ;
#36699 = CIRCLE ( 'NONE', #34989, 4.000000000000000888 ) ;
#36700 = EDGE_LOOP ( 'NONE', ( #5524, #90282, #51893, #5689 ) ) ;
#36701 = CARTESIAN_POINT ( 'NONE',  ( -20.97754405179127346, 294.8763868968453608, 9.942224931492237516 ) ) ;
#36702 = CARTESIAN_POINT ( 'NONE',  ( -0.7676806199076874337, -59.99999999999999289, 39.63870301987680733 ) ) ;
#36703 = ORIENTED_EDGE ( 'NONE', *, *, #99870, .T. ) ;
#36704 = CARTESIAN_POINT ( 'NONE',  ( -15.31606227096485817, -0.5350865456626047179, 14.99202647884761852 ) ) ;
#36705 = CARTESIAN_POINT ( 'NONE',  ( 46.00000000000000711, 488.0081391511161542, -0.5582540307957969405 ) ) ;
#36706 =( GEOMETRIC_REPRESENTATION_CONTEXT ( 3 ) GLOBAL_UNCERTAINTY_ASSIGNED_CONTEXT ( ( #39469 ) ) GLOBAL_UNIT_ASSIGNED_CONTEXT ( ( #96381, #45693, #31131 ) ) REPRESENTATION_CONTEXT ( 'NONE', 'WORKASPACE' ) );
#36707 = DIRECTION ( 'NONE',  ( 5.378903587909331904E-13, -0.5626279437274303019, 0.8267102254944252993 ) ) ;
#36708 = EDGE_CURVE ( 'NONE', #53428, #39260, #106099, .T. ) ;
#36710 = CARTESIAN_POINT ( 'NONE',  ( -1.584597276592265125, -47.40884508701223155, -34.79111164743952855 ) ) ;
#36709 = CARTESIAN_POINT ( 'NONE',  ( 9.482856158761293841, 252.4430711585471840, 3.177891129109649881 ) ) ;
#36711 = ORIENTED_EDGE ( 'NONE', *, *, #5503, .F. ) ;
#36712 = CARTESIAN_POINT ( 'NONE',  ( 9.994386960703202760, 294.6428459689212787, -0.7381326186433831982 ) ) ;
#36713 = CARTESIAN_POINT ( 'NONE',  ( 1.000000000000000444, -15.98025244997938721, -10.26003014047063822 ) ) ;
#36715 = ORIENTED_EDGE ( 'NONE', *, *, #100836, .T. ) ;
#36714 = AXIS2_PLACEMENT_3D ( 'NONE', #79965, #72413, #5035 ) ;
#36716 = EDGE_CURVE ( 'NONE', #36385, #104544, #37219, .T. ) ;
#36717 = CARTESIAN_POINT ( 'NONE',  ( 0.000000000000000000, -4.000000000000003553, 122.0000000000000000 ) ) ;
#36718 = SURFACE_SIDE_STYLE ('',( #44242 ) ) ;
#36719 = CARTESIAN_POINT ( 'NONE',  ( -94.69289845178556675, -60.00000000000000711, 46.75947207219763868 ) ) ;
#36720 = VERTEX_POINT ( 'NONE', #51926 ) ;
#36721 = CARTESIAN_POINT ( 'NONE',  ( 68.45015997180047407, 6.975173280561618775E-15, 0.000000000000000000 ) ) ;
#36722 = CARTESIAN_POINT ( 'NONE',  ( -5.656854249492379694, -11.93749999999999289, -5.656854249492380582 ) ) ;
#36723 = CARTESIAN_POINT ( 'NONE',  ( 11.71694229689447297, 294.5934945994754912, 1.882065127989447584 ) ) ;
#36725 = CARTESIAN_POINT ( 'NONE',  ( 73.59428447264397732, 4.000000000000015099, 4.898587196589422689E-16 ) ) ;
#36724 = CARTESIAN_POINT ( 'NONE',  ( 44.14911905790283697, 464.3766534542007207, 9.623404994951284763 ) ) ;
#36726 = CARTESIAN_POINT ( 'NONE',  ( -84.88152158083789800, -25.51324555084091372, 165.4372525938682656 ) ) ;
#36727 = ORIENTED_EDGE ( 'NONE', *, *, #77843, .F. ) ;
#36728 = CARTESIAN_POINT ( 'NONE',  ( 15.59999999999999787, 1.533819458162526451E-15, 0.000000000000000000 ) ) ;
#36729 = ADVANCED_FACE ( 'NONE', ( #26641 ), #34195, .T. ) ;
#36730 = EDGE_CURVE ( 'NONE', #76929, #81954, #42782, .T. ) ;
#36731 = ORIENTED_EDGE ( 'NONE', *, *, #27716, .T. ) ;
#36732 = VERTEX_POINT ( 'NONE', #10923 ) ;
#36733 = CARTESIAN_POINT ( 'NONE',  ( -12.10102349785729281, -5.000000000000000000, 11.47683805494447107 ) ) ;
#36734 = AXIS2_PLACEMENT_3D ( 'NONE', #9930, #41240, #1285 ) ;
#36735 =( NAMED_UNIT ( * ) SI_UNIT ( $, .STERADIAN. ) SOLID_ANGLE_UNIT ( ) );
#36736 = DIRECTION ( 'NONE',  ( 0.000000000000000000, 0.000000000000000000, 1.000000000000000000 ) ) ;
#36737 = ORIENTED_EDGE ( 'NONE', *, *, #60865, .F. ) ;
#36738 = COLOUR_RGB ( '', 0.08235294, 0.09019608, 0.10196078) ;
#36739 = CARTESIAN_POINT ( 'NONE',  ( -84.95435462066053844, -57.67079294309295534, -27.04779982294425977 ) ) ;
#36740 = CARTESIAN_POINT ( 'NONE',  ( 7.801777176595949825, -13.58827985812634509, -1.786991866639922266 ) ) ;
#36741 = CARTESIAN_POINT ( 'NONE',  ( -0.2696830121834116190, 13.85270131633358304, 7.000000000000015987 ) ) ;
#36742 = CIRCLE ( 'NONE', #5738, 4.000000000000001776 ) ;
#36743 = CARTESIAN_POINT ( 'NONE',  ( -9.482993638194542996, 102.5565127974632560, -3.177441187500465336 ) ) ;
#36744 = FILL_AREA_STYLE_COLOUR ( '', #20232 ) ;
#36745 = SURFACE_SIDE_STYLE ('',( #77157 ) ) ;
#36746 = CARTESIAN_POINT ( 'NONE',  ( 84.17695284478443796, -14.21045842199441367, -18.06956050794424584 ) ) ;
#36747 = CARTESIAN_POINT ( 'NONE',  ( -91.59718878904411099, -29.99999999999996803, 199.7679234505767738 ) ) ;
#36748 = CARTESIAN_POINT ( 'NONE',  ( -57.43764937006150717, -22.13952449013476453, 58.37273624025862517 ) ) ;
#36749 = ORIENTED_EDGE ( 'NONE', *, *, #53413, .T. ) ;
#36750 = LINE ( 'NONE', #55509, #57497 ) ;
#36751 = ORIENTED_EDGE ( 'NONE', *, *, #72140, .T. ) ;
#36752 = CARTESIAN_POINT ( 'NONE',  ( -101.7629185681098676, -37.82064707025393346, 185.3707029836525351 ) ) ;
#36753 = CARTESIAN_POINT ( 'NONE',  ( 0.000000000000000000, -5.000000000000000000, 8.000000000000000000 ) ) ;
#36754 = DIRECTION ( 'NONE',  ( -0.5735764363510497121, 0.8191520442889892450, 1.003171929053521665E-16 ) ) ;
#36755 = ORIENTED_EDGE ( 'NONE', *, *, #48689, .T. ) ;
#36756 =( NAMED_UNIT ( * ) PLANE_ANGLE_UNIT ( ) SI_UNIT ( $, .RADIAN. ) );
#36757 = DIRECTION ( 'NONE',  ( -1.000000000000000000, 0.000000000000000000, 0.000000000000000000 ) ) ;
#36758 = CARTESIAN_POINT ( 'NONE',  ( 7.188101187499999156, -15.12500000204838457, 2.977408999572654924 ) ) ;
#36759 = DIRECTION ( 'NONE',  ( 1.000000000000000000, 0.000000000000000000, 0.000000000000000000 ) ) ;
#36760 = FACE_OUTER_BOUND ( 'NONE', #20067, .T. ) ;
#36761 = CARTESIAN_POINT ( 'NONE',  ( -31.14694070047868735, 432.3293837220155069, 24.29762062537629319 ) ) ;
#36762 = CARTESIAN_POINT ( 'NONE',  ( 21.25502769577498796, 305.0480251235313176, 9.978840188629131802 ) ) ;
#36763 = DIRECTION ( 'NONE',  ( -1.000000000000000000, -1.224606353822377258E-16, -0.000000000000000000 ) ) ;
#36764 = DIRECTION ( 'NONE',  ( 0.000000000000000000, -1.000000000000000000, 0.000000000000000000 ) ) ;
#36765 = ADVANCED_FACE ( 'NONE', ( #93994 ), #53005, .T. ) ;
#36766 = FILL_AREA_STYLE_COLOUR ( '', #46581 ) ;
#36767 = CARTESIAN_POINT ( 'NONE',  ( -27.25852268718031368, -53.39317531337917444, 34.68901558833220378 ) ) ;
#36768 = CARTESIAN_POINT ( 'NONE',  ( 47.01925740490068506, -32.61024417345276305, 44.20151961235264793 ) ) ;
#36769 = CARTESIAN_POINT ( 'NONE',  ( -32.80551872593229490, 486.0171861992463960, 5.671217483525994751 ) ) ;
#36770 = EDGE_CURVE ( 'NONE', #63953, #99126, #18533, .T. ) ;
#36771 = CARTESIAN_POINT ( 'NONE',  ( 26.36650669486618881, 4.000000000000003553, 4.898587196589414801E-16 ) ) ;
#36772 = CARTESIAN_POINT ( 'NONE',  ( -85.74841582853835575, -38.65771171113095050, 198.9235328716311813 ) ) ;
#36773 = EDGE_LOOP ( 'NONE', ( #336, #3698, #11650, #90457 ) ) ;
#36774 = DIRECTION ( 'NONE',  ( 0.000000000000000000, 0.000000000000000000, 1.000000000000000000 ) ) ;
#36775 = CARTESIAN_POINT ( 'NONE',  ( 13.02702147844135716, 6.134201042431408624, -7.309633161561180259 ) ) ;
#36776 = DIRECTION ( 'NONE',  ( -1.000000000000000000, -0.000000000000000000, -0.000000000000000000 ) ) ;
#36777 = CARTESIAN_POINT ( 'NONE',  ( 4.852941176821355285, 40.28748324523049007, -70.80672828646224559 ) ) ;
#36778 = CARTESIAN_POINT ( 'NONE',  ( 23.21751746555303342, 28.11705169068991594, 30.70617127781016720 ) ) ;
#36780 = PRESENTATION_STYLE_ASSIGNMENT (( #69644 ) ) ;
#36779 = COLOUR_RGB ( '', 0.66274510, 0.83137255, 0.94901961) ;
#36781 = CARTESIAN_POINT ( 'NONE',  ( 33.16759796689489548, 434.2047070568555114, 15.25549030506044801 ) ) ;
#36782 = CARTESIAN_POINT ( 'NONE',  ( 111.8879798515403365, -59.99999999999998579, 181.3037615216028371 ) ) ;
#36783 = B_SPLINE_CURVE_WITH_KNOTS ( 'NONE', 3,
 ( #24426, #9777, #34644, #41104, #9247, #1137, #65904, #90183, #89657, #67512, #15757, #57795, #81524, #7648, #40565, #106343, #16285, #49170, #73984, #66, #78246, #27084, #93908, #18443, #61021, #36243, #11366, #52368, #85835, #100393, #101467, #92831, #76116, #102529 ),
 .UNSPECIFIED., .F., .F.,
 ( 4, 2, 2, 2, 2, 2, 2, 2, 2, 2, 2, 2, 2, 2, 2, 2, 4 ),
 ( 0.000000000000000000, 0.0007951492273476376636, 0.001590298454695275327, 0.002385447682042913208, 0.003180596909390550654, 0.003975746136738188101, 0.004770895364085826415, 0.005566044591433463862, 0.006361193818781101308, 0.007156343046128739623, 0.007951492273476376202, 0.008746641500824015383, 0.009541790728171654565, 0.01033693995551929375, 0.01113208918286693293, 0.01192723841021457211, 0.01272238763756221129 ),
 .UNSPECIFIED. ) ;
#36784 = CARTESIAN_POINT ( 'NONE',  ( 0.000000000000000000, -30.00000000000000000, 0.000000000000000000 ) ) ;
#36785 = VERTEX_POINT ( 'NONE', #85928 ) ;
#36786 = EDGE_CURVE ( 'NONE', #33722, #99731, #71738, .T. ) ;
#36787 = DIRECTION ( 'NONE',  ( 0.000000000000000000, -1.000000000000000000, 0.000000000000000000 ) ) ;
#36788 = CARTESIAN_POINT ( 'NONE',  ( -78.58275268908097644, -29.99999999999997868, -15.35986885401157842 ) ) ;
#36789 = VERTEX_POINT ( 'NONE', #84840 ) ;
#36790 = CARTESIAN_POINT ( 'NONE',  ( 21.36650669486618881, 4.000000000000003553, 4.898587196589414801E-16 ) ) ;
#36791 = DIRECTION ( 'NONE',  ( -1.000000000000000000, -1.224606353822377258E-16, -0.000000000000000000 ) ) ;
#36792 = DIRECTION ( 'NONE',  ( 0.000000000000000000, -1.000000000000000000, 0.000000000000000000 ) ) ;
#36793 = CARTESIAN_POINT ( 'NONE',  ( 39.21279148650069146, 436.8435004666158079, 5.150741822288956051 ) ) ;
#36794 = AXIS2_PLACEMENT_3D ( 'NONE', #12850, #45766, #63560 ) ;
#36795 = CARTESIAN_POINT ( 'NONE',  ( -1.320432766682874540E-15, -13.90625000204838457, 7.188101187500000044 ) ) ;
#36796 = CARTESIAN_POINT ( 'NONE',  ( -11.99999999999999467, -5.000000000000002665, -86.57079632497431021 ) ) ;
#36797 = DIRECTION ( 'NONE',  ( -1.000000000000000000, -1.224606353822377258E-16, -0.000000000000000000 ) ) ;
#36799 = ORIENTED_EDGE ( 'NONE', *, *, #62351, .T. ) ;
#36798 = SURFACE_STYLE_USAGE ( .BOTH. , #94484 ) ;
#36800 = CARTESIAN_POINT ( 'NONE',  ( 83.91197280327008912, -32.50557349083430125, 167.3429057765409027 ) ) ;
#36801 = CARTESIAN_POINT ( 'NONE',  ( -42.18756898894582719, 484.4522853017719513, -2.425645685620470449 ) ) ;
#36802 = CARTESIAN_POINT ( 'NONE',  ( 5.299999999999999822, 3.752776749732569694, 6.499999999999997335 ) ) ;
#36803 = EDGE_LOOP ( 'NONE', ( #31482, #43873, #77051, #65981 ) ) ;
#36804 = FACE_OUTER_BOUND ( 'NONE', #71072, .T. ) ;
#36805 = PRESENTATION_STYLE_ASSIGNMENT (( #3876 ) ) ;
#36806 = LINE ( 'NONE', #3343, #71395 ) ;
#36807 = CARTESIAN_POINT ( 'NONE',  ( 101.2019940638598854, 1.030564683017419500E-14, 0.000000000000000000 ) ) ;
#36808 = FACE_OUTER_BOUND ( 'NONE', #100858, .T. ) ;
#36810 = CARTESIAN_POINT ( 'NONE',  ( 0.3605873925011542358, 13.03538297051737338, 51.69841471560108914 ) ) ;
#36809 = PRESENTATION_LAYER_ASSIGNMENT (  '', '', ( #69499 ) ) ;
#36811 = CARTESIAN_POINT ( 'NONE',  ( 6.520166676877810374, -0.2361713054966709524, 15.39474435275100284 ) ) ;
#36812 = ORIENTED_EDGE ( 'NONE', *, *, #27673, .T. ) ;
#36813 = COLOUR_RGB ( '', 0.66274510, 0.83137255, 0.94901961) ;
#36815 = CONICAL_SURFACE ( 'NONE', #83268, 5.999999999999998224, 0.7853981633974509435 ) ;
#36814 =( NAMED_UNIT ( * ) SI_UNIT ( $, .STERADIAN. ) SOLID_ANGLE_UNIT ( ) );
#36816 = CARTESIAN_POINT ( 'NONE',  ( 7.000000000000000000, 0.000000000000000000, -3.024963890361733743 ) ) ;
#36817 = CARTESIAN_POINT ( 'NONE',  ( 24.34999999999999787, 1.533819458162526451E-15, 0.000000000000000000 ) ) ;
#36818 = LINE ( 'NONE', #4408, #83751 ) ;
#36820 = DIRECTION ( 'NONE',  ( 0.000000000000000000, 0.000000000000000000, 1.000000000000000000 ) ) ;
#36819 = CARTESIAN_POINT ( 'NONE',  ( 24.83349330513380693, 4.898587196589411843E-16, -4.000000000000001776 ) ) ;
#36821 = CARTESIAN_POINT ( 'NONE',  ( 4.401442555609581635E-16, -24.78125000204838813, -7.188101187500000044 ) ) ;
#36822 = FACE_OUTER_BOUND ( 'NONE', #28520, .T. ) ;
#36823 = DIRECTION ( 'NONE',  ( 0.000000000000000000, 0.000000000000000000, 1.000000000000000000 ) ) ;
#36824 = CARTESIAN_POINT ( 'NONE',  ( 3.122695042037154867, -5.000000000000000000, -96.69538631874429768 ) ) ;
#36825 = ITEM_DEFINED_TRANSFORMATION ( 'NONE', 'NONE', #14568,  #10728 ) ;
#36826 = ORIENTED_EDGE ( 'NONE', *, *, #79828, .T. ) ;
#36827 = CARTESIAN_POINT ( 'NONE',  ( 39.13466327773082298, 485.8437493838399632, -4.960055907050037405 ) ) ;
#36828 = CARTESIAN_POINT ( 'NONE',  ( 7.500000000000000000, -4.730916290271713009, -7.493595886788495086 ) ) ;
#36829 = CARTESIAN_POINT ( 'NONE',  ( -4.652400833064921137, 8.218796697697426268, -5.000000000000000888 ) ) ;
#36830 = CARTESIAN_POINT ( 'NONE',  ( 0.000000000000000000, 61.50000000000000000, 0.000000000000000000 ) ) ;
#36831 = EDGE_CURVE ( 'NONE', #27928, #58498, #85558, .T. ) ;
#36832 = ORIENTED_EDGE ( 'NONE', *, *, #25458, .F. ) ;
#36833 = EDGE_CURVE ( 'NONE', #3430, #95900, #6027, .T. ) ;
#36834 = DIRECTION ( 'NONE',  ( -0.000000000000000000, -1.000000000000000000, -0.000000000000000000 ) ) ;
#36835 = CARTESIAN_POINT ( 'NONE',  ( 8.904581707871560781, 49.99999999999999289, -97.29851715190670802 ) ) ;
#36836 = ORIENTED_EDGE ( 'NONE', *, *, #33936, .T. ) ;
#36837 = EDGE_CURVE ( 'NONE', #26529, #9488, #86837, .T. ) ;
#36838 = DIRECTION ( 'NONE',  ( -1.000000000000000000, -1.224606353822377258E-16, -0.000000000000000000 ) ) ;
#36839 = CARTESIAN_POINT ( 'NONE',  ( -0.3616048520552285206, 7.866658882532708397, -51.69814723577159299 ) ) ;
#36840 = CARTESIAN_POINT ( 'NONE',  ( 9.537909130738276176, 102.3538516903660565, -3.010726932293859459 ) ) ;
#36841 = CARTESIAN_POINT ( 'NONE',  ( -17.99637020931157849, 36.53998198029804456, 22.85704674614657961 ) ) ;
#36842 = CARTESIAN_POINT ( 'NONE',  ( -110.8672444992828332, -59.99999999999999289, 187.9148104057422302 ) ) ;
#36843 = CARTESIAN_POINT ( 'NONE',  ( 19.07202809346016892, 49.63760697579803605, 61.78692401718791416 ) ) ;
#36844 = STYLED_ITEM ( 'NONE', ( #38415 ), #55083 ) ;
#36845 = CARTESIAN_POINT ( 'NONE',  ( 16.01635194906463866, 304.5593466744471698, -9.062162209746613684 ) ) ;
#36846 = LINE ( 'NONE', #37378, #95950 ) ;
#36847 = CARTESIAN_POINT ( 'NONE',  ( 17.85370335554367216, 34.21381263225121216, -23.65318376138480971 ) ) ;
#36848 = CARTESIAN_POINT ( 'NONE',  ( -83.19761587003101511, -53.69446230421030464, 186.7557214745879151 ) ) ;
#36849 = CARTESIAN_POINT ( 'NONE',  ( 39.25203474886774302, 42.00920105620009082, -56.53737387468299147 ) ) ;
#36850 = ADVANCED_FACE ( 'NONE', ( #63231 ), #5512, .T. ) ;
#36851 = ORIENTED_EDGE ( 'NONE', *, *, #16736, .T. ) ;
#36852 = CARTESIAN_POINT ( 'NONE',  ( -9.648094638230798381, 46.21279293231379626, -13.07965317076984135 ) ) ;
#36853 = DIRECTION ( 'NONE',  ( 0.000000000000000000, 0.000000000000000000, -1.000000000000000000 ) ) ;
#36854 = CARTESIAN_POINT ( 'NONE',  ( -86.65393392273510642, -60.14883673965872646, 0.2203813179658791754 ) ) ;
#36855 = DIRECTION ( 'NONE',  ( 0.5735764363510468256, 0.8191520442889913545, 0.000000000000000000 ) ) ;
#36856 = CARTESIAN_POINT ( 'NONE',  ( 0.000000000000000000, 45.00000000000000711, 0.000000000000000000 ) ) ;
#36857 = CARTESIAN_POINT ( 'NONE',  ( 7.955546711085375478, 98.60610140868929818, -5.000000000000000888 ) ) ;
#36858 = CARTESIAN_POINT ( 'NONE',  ( 101.4868948250290259, -2.002967142162725287E-29, 5.000000000000011546 ) ) ;
#36859 = CARTESIAN_POINT ( 'NONE',  ( 5.022013495247499293, 18.64316884711714195, -38.36535705883633085 ) ) ;
#36860 = CARTESIAN_POINT ( 'NONE',  ( 77.40131791002600892, -14.21045842199445630, 153.6837402093314324 ) ) ;
#36861 = CARTESIAN_POINT ( 'NONE',  ( -94.21198422502472170, -59.99999999999998579, 13.85022971857252649 ) ) ;
#36862 = B_SPLINE_CURVE_WITH_KNOTS ( 'NONE', 3,
 ( #64007, #7316, #259, #48833, #90375, #14881, #33225, #105498, #40755, #49908 ),
 .UNSPECIFIED., .F., .F.,
 ( 4, 2, 2, 2, 4 ),
 ( 0.000000000000000000, 0.0008538222887801227108, 0.001707644577560245422, 0.002561466866340368024, 0.003415289155120490843 ),
 .UNSPECIFIED. ) ;
#36863 = CARTESIAN_POINT ( 'NONE',  ( -62.93303494182386970, -56.86903391315339462, 89.13530110543882756 ) ) ;
#36864 = ORIENTED_EDGE ( 'NONE', *, *, #64566, .F. ) ;
#36865 = CARTESIAN_POINT ( 'NONE',  ( 106.6028846201213440, -30.00000000000002487, 192.6838848496860521 ) ) ;
#36866 = CARTESIAN_POINT ( 'NONE',  ( -58.89674073997064596, 40.83722256636393411, -28.13773381937142304 ) ) ;
#36867 = CARTESIAN_POINT ( 'NONE',  ( 52.88197059271687550, -57.67115856031815468, -39.33710569591229245 ) ) ;
#36868 = EDGE_LOOP ( 'NONE', ( #88102, #98609, #39020, #5812, #62278, #82446, #44997, #95065 ) ) ;
#36869 = DIRECTION ( 'NONE',  ( -1.000000000000000000, -1.224606353822377258E-16, -0.000000000000000000 ) ) ;
#36870 = CARTESIAN_POINT ( 'NONE',  ( -1.320432766682874540E-15, -24.40625000204838813, 7.188101187500000044 ) ) ;
#36871 = B_SPLINE_CURVE_WITH_KNOTS ( 'NONE', 3,
 ( #32737, #15450, #74213, #65604, #292, #24642, #823, #33258, #66132, #33792 ),
 .UNSPECIFIED., .F., .F.,
 ( 4, 2, 2, 2, 4 ),
 ( 0.000000000000000000, 0.002305503304226491201, 0.004611006608452982401, 0.006916509912679473168, 0.009222013216905964803 ),
 .UNSPECIFIED. ) ;
#36872 = CARTESIAN_POINT ( 'NONE',  ( -5.475947152006328089, -6.837822698908765595, 2.462898245435122924 ) ) ;
#36873 = ORIENTED_EDGE ( 'NONE', *, *, #88622, .F. ) ;
#36874 = DIRECTION ( 'NONE',  ( -1.000000000000000000, 0.000000000000000000, 0.000000000000000000 ) ) ;
#36875 = EDGE_LOOP ( 'NONE', ( #48453, #92794, #87438, #64696, #33820 ) ) ;
#36876 = CARTESIAN_POINT ( 'NONE',  ( 7.135888613856973706, 39.99999999999999289, -71.74865085751117988 ) ) ;
#36877 = CARTESIAN_POINT ( 'NONE',  ( 19.83349330513379982, 1.593028355512270567E-15, 0.000000000000000000 ) ) ;
#36878 = CARTESIAN_POINT ( 'NONE',  ( -55.33337412123101728, -60.00000000000000000, -36.77909458192313252 ) ) ;
#36879 = CARTESIAN_POINT ( 'NONE',  ( 0.9999999999999940048, -50.00000000000000000, 103.3397459621556180 ) ) ;
#36880 = CARTESIAN_POINT ( 'NONE',  ( 2.977408999572650927, -32.75000000204839523, -7.188101187500001821 ) ) ;
#36881 = CARTESIAN_POINT ( 'NONE',  ( -23.21751746555280249, -1.200000000000000030E-05, -33.20617127781034839 ) ) ;
#36882 = AXIS2_PLACEMENT_3D ( 'NONE', #12209, #94755, #88240 ) ;
#36883 = CARTESIAN_POINT ( 'NONE',  ( 42.33349330513380693, 1.593028355512270567E-15, 0.000000000000000000 ) ) ;
#36884 =( NAMED_UNIT ( * ) PLANE_ANGLE_UNIT ( ) SI_UNIT ( $, .RADIAN. ) );
#36885 = PLANE ( 'NONE',  #64527 ) ;
#36886 = DIRECTION ( 'NONE',  ( 0.000000000000000000, 0.000000000000000000, -1.000000000000000000 ) ) ;
#36887 = EDGE_CURVE ( 'NONE', #70568, #25185, #54036, .T. ) ;
#36888 = ORIENTED_EDGE ( 'NONE', *, *, #24690, .F. ) ;
#36889 = CARTESIAN_POINT ( 'NONE',  ( -7.493949047870493096, 40.57569111244914950, -68.91429205788598722 ) ) ;
#36891 = CARTESIAN_POINT ( 'NONE',  ( 34.09463002446733526, -56.83197632054391590, 38.12211492157798887 ) ) ;
#36890 = DIRECTION ( 'NONE',  ( 0.000000000000000000, 0.000000000000000000, 1.000000000000000000 ) ) ;
#36892 = CARTESIAN_POINT ( 'NONE',  ( 15.50035291838848472, -4.285714285715568117, -20.16952962162309859 ) ) ;
#36893 = ORIENTED_EDGE ( 'NONE', *, *, #105138, .T. ) ;
#36894 = EDGE_CURVE ( 'NONE', #72287, #70974, #13144, .T. ) ;
#36895 = EDGE_CURVE ( 'NONE', #58101, #59703, #99292, .T. ) ;
#36896 = CARTESIAN_POINT ( 'NONE',  ( -22.81493026622527864, 25.35530515213832459, -33.14233034566358072 ) ) ;
#36898 = CARTESIAN_POINT ( 'NONE',  ( 6.806778131844891000, 41.25019534418786549, -70.74215739200818120 ) ) ;
#36897 = CARTESIAN_POINT ( 'NONE',  ( -26.01151370334376978, 35.07581603598547559, -8.178615366860272573 ) ) ;
#36899 = CARTESIAN_POINT ( 'NONE',  ( 38.58349330513380693, -7.703719777548943412E-31, 4.000000000000001776 ) ) ;
#36900 = CARTESIAN_POINT ( 'NONE',  ( -20.36049642833716078, 294.7627513888867838, -10.01892845649183350 ) ) ;
#36901 = CARTESIAN_POINT ( 'NONE',  ( 35.59999999999999432, 1.533819458162526451E-15, 0.000000000000000000 ) ) ;
#36902 = CARTESIAN_POINT ( 'NONE',  ( 0.000000000000000000, 0.000000000000000000, 0.000000000000000000 ) ) ;
#36903 = ORIENTED_EDGE ( 'NONE', *, *, #25340, .F. ) ;
#36904 = CARTESIAN_POINT ( 'NONE',  ( 92.51399846021976714, -60.00000000000000711, -1.448676682892423795 ) ) ;
#36905 = DIRECTION ( 'NONE',  ( 0.000000000000000000, 1.000000000000000000, 0.000000000000000000 ) ) ;
#36906 = CARTESIAN_POINT ( 'NONE',  ( -7.000000000000000000, 8.572527594031471218E-16, -1.175078176076019387 ) ) ;
#36907 = CARTESIAN_POINT ( 'NONE',  ( -35.49529570007158696, 379.4505083648772938, 5.762799703950255648 ) ) ;
#36908 = CARTESIAN_POINT ( 'NONE',  ( -6.519732893028145071, 40.56016492163267628, -71.18560187175323506 ) ) ;
#36909 = CARTESIAN_POINT ( 'NONE',  ( 9.165151389911679658, 30.00000000000000000, 4.000000000000000000 ) ) ;
#36910 = ORIENTED_EDGE ( 'NONE', *, *, #88722, .F. ) ;
#36911 = EDGE_CURVE ( 'NONE', #86664, #94186, #14114, .T. ) ;
#36912 = AXIS2_PLACEMENT_3D ( 'NONE', #2190, #52891, #85258 ) ;
#36913 = CARTESIAN_POINT ( 'NONE',  ( -103.5615167553033302, -29.99999999999941380, 196.9855737867926848 ) ) ;
#36914 = ORIENTED_EDGE ( 'NONE', *, *, #87532, .F. ) ;
#36915 = CARTESIAN_POINT ( 'NONE',  ( 73.33904886068935980, 6.975173280561618775E-15, 0.000000000000000000 ) ) ;
#36916 = LINE ( 'NONE', #87044, #522 ) ;
#36917 = CARTESIAN_POINT ( 'NONE',  ( 15.79785611713298366, 22.78916061418795636, -0.5147589528736694620 ) ) ;
#36918 = CARTESIAN_POINT ( 'NONE',  ( 82.32180399435387130, -37.81125714862378828, -13.10781145855886898 ) ) ;
#36919 = CARTESIAN_POINT ( 'NONE',  ( 2.977408999572651815, -33.31250000204838813, 7.188101187500000933 ) ) ;
#36920 = CARTESIAN_POINT ( 'NONE',  ( 0.000000000000000000, 0.000000000000000000, 0.000000000000000000 ) ) ;
#36921 = CARTESIAN_POINT ( 'NONE',  ( 72.61817852641561899, -45.32557365410384875, -22.56083099965291439 ) ) ;
#36922 = VERTEX_POINT ( 'NONE', #36858 ) ;
#36923 = DIRECTION ( 'NONE',  ( 0.000000000000000000, 0.000000000000000000, 1.000000000000000000 ) ) ;
#36924 = EDGE_LOOP ( 'NONE', ( #100427, #36133, #29038, #100674, #59823 ) ) ;
#36925 = CARTESIAN_POINT ( 'NONE',  ( 8.559508646656103892, 51.55638410492932167, -4.031152949375861105 ) ) ;
#36926 = VECTOR ( 'NONE', #88539, 1000.000000000000000 ) ;
#36927 = EDGE_CURVE ( 'NONE', #26711, #31406, #6286, .T. ) ;
#36929 = ORIENTED_EDGE ( 'NONE', *, *, #64930, .F. ) ;
#36928 = DIRECTION ( 'NONE',  ( -1.000000000000000000, -0.000000000000000000, -0.000000000000000000 ) ) ;
#36930 = CARTESIAN_POINT ( 'NONE',  ( 79.07936512157644415, -25.61524179269867219, 127.8490551884245150 ) ) ;
#36931 = AXIS2_PLACEMENT_3D ( 'NONE', #47281, #40260, #72625 ) ;
#36932 = ORIENTED_EDGE ( 'NONE', *, *, #86397, .T. ) ;
#36933 = CARTESIAN_POINT ( 'NONE',  ( 2.047337005717745129, -49.86272114439862690, 44.73384807164315902 ) ) ;
#36934 = CARTESIAN_POINT ( 'NONE',  ( -2.977408999572654480, -16.62500000204838813, 7.188101187499999156 ) ) ;
#36935 = CARTESIAN_POINT ( 'NONE',  ( -81.06400256271496119, -57.51341943371168952, 199.7941202169005805 ) ) ;
#36936 = ORIENTED_EDGE ( 'NONE', *, *, #77728, .F. ) ;
#36937 =( NAMED_UNIT ( * ) PLANE_ANGLE_UNIT ( ) SI_UNIT ( $, .RADIAN. ) );
#36938 = CARTESIAN_POINT ( 'NONE',  ( 3.363235851038136826, 30.69031363909868304, 5.000000000000000000 ) ) ;
#36939 = CARTESIAN_POINT ( 'NONE',  ( -9.253800200985685009, 83.69989668911827607, -3.791983798715483189 ) ) ;
#36940 = CARTESIAN_POINT ( 'NONE',  ( 49.25896281664822141, 12.93370316445848900, -15.83749202751853780 ) ) ;
#36941 = CARTESIAN_POINT ( 'NONE',  ( -8.000000000000000000, -16.53125000409677270, -3.313708498984762496 ) ) ;
#36942 = CARTESIAN_POINT ( 'NONE',  ( -51.43727798272582419, -29.90494385022926593, 49.06446334853066560 ) ) ;
#36943 = CARTESIAN_POINT ( 'NONE',  ( 9.833493305133801599, -7.703719777548943412E-31, 4.000000000000001776 ) ) ;
#36944 = CARTESIAN_POINT ( 'NONE',  ( 20.37278541768183615, 303.8378246129572631, -10.00297115033342266 ) ) ;
#36945 = CARTESIAN_POINT ( 'NONE',  ( 7.500000000000003553, -2.999999999999876099, -69.80246343544249044 ) ) ;
#36946 = LINE ( 'NONE', #76298, #75763 ) ;
#36947 = DIRECTION ( 'NONE',  ( -0.9999999999999998890, 2.730739648532243183E-17, 4.042189804083926130E-17 ) ) ;
#36948 = DIRECTION ( 'NONE',  ( 0.000000000000000000, -0.9109553866900513830, 0.4125048890139109137 ) ) ;
#36949 = VERTEX_POINT ( 'NONE', #95073 ) ;
#36950 = CARTESIAN_POINT ( 'NONE',  ( -2.045670083595537037, -49.95306077403387945, 40.93770280784608673 ) ) ;
#36951 = DIRECTION ( 'NONE',  ( -0.000000000000000000, 1.000000000000000000, -0.000000000000000000 ) ) ;
#36952 = CARTESIAN_POINT ( 'NONE',  ( 0.9479484640198931888, 12.67371156664382070, 49.67349439981760639 ) ) ;
#36953 = B_SPLINE_CURVE_WITH_KNOTS ( 'NONE', 3,
 ( #37439, #31463, #62750, #21254 ),
 .UNSPECIFIED., .F., .F.,
 ( 4, 4 ),
 ( 0.02698643027831515440, 0.9670246242088337274 ),
 .UNSPECIFIED. ) ;
#36954 = CARTESIAN_POINT ( 'NONE',  ( -41.84433561564012649, -26.95236078925062628, -36.17932813448958029 ) ) ;
#36955 = CARTESIAN_POINT ( 'NONE',  ( -81.17922251170084280, -29.99999999999999289, 141.0271696047036301 ) ) ;
#36956 = CARTESIAN_POINT ( 'NONE',  ( -6.965116046117190152, 41.61856606226410094, -70.00485699691064667 ) ) ;
#36957 = EDGE_CURVE ( 'NONE', #85958, #38016, #12523, .T. ) ;
#36958 = AXIS2_PLACEMENT_3D ( 'NONE', #21551, #54385, #87332 ) ;
#36959 = CIRCLE ( 'NONE', #102359, 4.000000000000000888 ) ;
#36960 = ORIENTED_EDGE ( 'NONE', *, *, #19700, .T. ) ;
#36961 = CARTESIAN_POINT ( 'NONE',  ( 55.26095113931063452, -1.232595164407830946E-29, 4.000000000000007105 ) ) ;
#36962 = CARTESIAN_POINT ( 'NONE',  ( 80.71913178869228034, -57.51110409648728705, 199.5057488713411260 ) ) ;
#36963 = CARTESIAN_POINT ( 'NONE',  ( 8.737863883542575039, 48.00000000000000711, -79.96381019629100706 ) ) ;
#36964 = ADVANCED_FACE ( 'NONE', ( #4989 ), #29821, .T. ) ;
#36965 = ADVANCED_FACE ( 'NONE', ( #46501 ), #20139, .T. ) ;
#36966 = CARTESIAN_POINT ( 'NONE',  ( 0.04050535873993678371, -7.919512791578269706, -6.573129608219105968 ) ) ;
#36967 = CARTESIAN_POINT ( 'NONE',  ( -16.14595037837264968, 20.48388002475744685, -4.555408037181266856 ) ) ;
#36968 = CARTESIAN_POINT ( 'NONE',  ( 6.145467199749147014, -3.000000000000002665, -77.00333157601819778 ) ) ;
#36969 = CARTESIAN_POINT ( 'NONE',  ( -69.88144121408996057, -59.99999999999999289, 140.7071162517904668 ) ) ;
#36970 = CARTESIAN_POINT ( 'NONE',  ( -4.444974277458379142, 4.939246403833572607, -5.720331885004773298 ) ) ;
#36971 = EDGE_CURVE ( 'NONE', #86608, #73379, #9753, .T. ) ;
#36972 = FILL_AREA_STYLE_COLOUR ( '', #49090 ) ;
#36973 = CARTESIAN_POINT ( 'NONE',  ( -85.83393798185170454, -35.62537476688432747, 184.8253129914004376 ) ) ;
#36974 = ORIENTED_EDGE ( 'NONE', *, *, #71220, .F. ) ;
#36975 = CARTESIAN_POINT ( 'NONE',  ( 36.74066248129624057, 397.0785584018862551, 6.179803345696205596 ) ) ;
#36976 = CARTESIAN_POINT ( 'NONE',  ( -1.020036429124608679, -56.88429985501548458, 33.37036660210496564 ) ) ;
#36977 = ADVANCED_FACE ( 'NONE', ( #6554 ), #90697, .T. ) ;
#36978 = CARTESIAN_POINT ( 'NONE',  ( -6.914391365018432545, 41.80417567437852711, -59.57688295187696781 ) ) ;
#36979 = CARTESIAN_POINT ( 'NONE',  ( 6.281178480976146616, 3.752776749732564809, 6.499999999999995559 ) ) ;
#36980 = CARTESIAN_POINT ( 'NONE',  ( -7.465322217760688162, 54.30106466035046253, 2.153579458703050786 ) ) ;
#36982 = DIRECTION ( 'NONE',  ( 0.000000000000000000, 0.000000000000000000, 1.000000000000000000 ) ) ;
#36981 =( GEOMETRIC_REPRESENTATION_CONTEXT ( 3 ) GLOBAL_UNCERTAINTY_ASSIGNED_CONTEXT ( ( #88015 ) ) GLOBAL_UNIT_ASSIGNED_CONTEXT ( ( #61140, #60097, #28271 ) ) REPRESENTATION_CONTEXT ( 'NONE', 'WORKASPACE' ) );
#36983 = DIRECTION ( 'NONE',  ( 0.000000000000000000, 0.000000000000000000, -1.000000000000000000 ) ) ;
#36984 = CARTESIAN_POINT ( 'NONE',  ( 45.36923076923077502, -4.171999999999999709, 0.000000000000000000 ) ) ;
#36985 = DIRECTION ( 'NONE',  ( 0.000000000000000000, 0.000000000000000000, -1.000000000000000000 ) ) ;
#36986 = VERTEX_POINT ( 'NONE', #25454 ) ;
#36987 = CARTESIAN_POINT ( 'NONE',  ( 25.56253568781137986, 295.7864503539771022, -1.799098680748292045 ) ) ;
#36988 = CARTESIAN_POINT ( 'NONE',  ( 11.78635468501824057, 6.776294004930349502, 9.084523618773719278 ) ) ;
#36989 = CARTESIAN_POINT ( 'NONE',  ( 6.601913983208107517, -4.285714285714895766, -24.56594385547655790 ) ) ;
#36990 = CARTESIAN_POINT ( 'NONE',  ( -32.05241217996611169, 487.5077369493866399, 9.813907492591894766 ) ) ;
#36991 = CARTESIAN_POINT ( 'NONE',  ( 110.8743008064580664, -59.99999999999998579, 132.3768192050824268 ) ) ;
#36992 = CARTESIAN_POINT ( 'NONE',  ( -79.97908447249672292, -29.09054715422505666, 135.2929009280034904 ) ) ;
#36993 = COLOUR_RGB ( '', 0.31764706, 0.68627451, 0.89019608) ;
#36994 = VERTEX_POINT ( 'NONE', #91232 ) ;
#36995 = FILL_AREA_STYLE_COLOUR ( '', #5093 ) ;
#36996 = DIRECTION ( 'NONE',  ( 1.000000000000000000, 1.224606353822377258E-16, 0.000000000000000000 ) ) ;
#36997 = CIRCLE ( 'NONE', #12849, 4.000000000000000888 ) ;
#36998 = CARTESIAN_POINT ( 'NONE',  ( 28.69487864981134351, 50.00000000000000711, 56.30615108626901133 ) ) ;
#36999 = AXIS2_PLACEMENT_3D ( 'NONE', #83389, #18151, #10035 ) ;
#37000 = CARTESIAN_POINT ( 'NONE',  ( 37.00921004089878608, 345.1628843254408139, 0.03558237527558635871 ) ) ;
#37001 = DIRECTION ( 'NONE',  ( 0.000000000000000000, 1.000000000000000000, 0.000000000000000000 ) ) ;
#37002 = VERTEX_POINT ( 'NONE', #17338 ) ;
#37003 = PRESENTATION_LAYER_ASSIGNMENT (  '', '', ( #4249 ) ) ;
#37004 = CARTESIAN_POINT ( 'NONE',  ( 5.124566304833717112, 53.50649568328331185, -8.531152949374618544 ) ) ;
#37005 = CARTESIAN_POINT ( 'NONE',  ( 31.39297415328601915, 438.8543991500256993, 23.05892055662082996 ) ) ;
#37006 = CARTESIAN_POINT ( 'NONE',  ( 7.188101187499999156, -23.75000000204839168, 2.977408999572654924 ) ) ;
#37007 = ORIENTED_EDGE ( 'NONE', *, *, #5674, .T. ) ;
#37008 =( BOUNDED_SURFACE ( )  B_SPLINE_SURFACE ( 2, 3, ( 
 ( #25336, #26416, #50615, #49573, #100253, #58199, #1539, #74899, #8582, #18852, #34506, #10175, #51697, #75979, #9106, #43614, #91125, #66834, #2076, #35029, #98648, #16682, #67892, #74373, #99724, #100780, #58752, #84614, #450, #10700, #33420, #76506, #35563, #66294 ),
 ( #85688, #36105, #37696, #28536, #70561, #78106, #45231, #19928, #86758, #102383, #103447, #62469, #29598, #53825, #4224, #86231, #53311, #94308, #95360, #21497, #37159, #44699, #70021, #79164, #61953, #12826, #36632, #54334, #101849, #12303, #87277, #45747, #3161, #102920 ),
 ( #20470, #29088, #13354, #68976, #61416, #28010, #60880, #46281, #5295, #52771, #94846, #20991, #3706, #93770, #68437, #78623, #93234, #4757, #101330, #11765, #27482, #77586, #60359, #69497, #19397, #52229, #85139, #11232, #44157, #77045, #48906, #103967, #96949, #23084 ) ),
 .UNSPECIFIED., .F., .T., .F. ) 
 B_SPLINE_SURFACE_WITH_KNOTS ( ( 3, 3 ),
 ( 4, 2, 2, 2, 2, 2, 2, 2, 2, 2, 2, 2, 2, 2, 2, 2, 4 ),
 ( 0.000000000000000000, 1.000000000000000000 ),
 ( 3.141592653589793116, 3.534291735288517700, 3.926990816987241395, 4.319689898685965090, 4.712388980384689674, 5.105088062083414258, 5.497787143782137953, 5.890486225480861648, 6.283185307179586232, 6.675884388878310816, 7.068583470577034511, 7.461282552275758206, 7.853981633974482790, 8.246680715673207374, 8.639379797371930181, 9.032078879070654764, 9.424777960769379348 ),
 .UNSPECIFIED. ) 
 GEOMETRIC_REPRESENTATION_ITEM ( )  RATIONAL_B_SPLINE_SURFACE ( (
 ( 1.000000000000000000, 1.000000000000000000, 1.000000000000000000, 1.000000000000000000, 1.000000000000000000, 1.000000000000000000, 1.000000000000000000, 1.000000000000000000, 1.000000000000000000, 1.000000000000000000, 1.000000000000000000, 1.000000000000000000, 1.000000000000000000, 1.000000000000000000, 1.000000000000000000, 1.000000000000000000, 1.000000000000000000, 1.000000000000000000, 1.000000000000000000, 1.000000000000000000, 1.000000000000000000, 1.000000000000000000, 1.000000000000000000, 1.000000000000000000, 1.000000000000000000, 1.000000000000000000, 1.000000000000000000, 1.000000000000000000, 1.000000000000000000, 1.000000000000000000, 1.000000000000000000, 1.000000000000000000, 1.000000000000000000, 1.000000000000000000),
 ( 1.857142857142858317, 1.857142857142858317, 1.857142857142860981, 1.857142857142860981, 1.857142857142858317, 1.857142857142858317, 1.857142857142858317, 1.857142857142858317, 1.857142857142858317, 1.857142857142858317, 1.857142857142858317, 1.857142857142858317, 1.857142857142858317, 1.857142857142858317, 1.857142857142858317, 1.857142857142858317, 1.857142857142858317, 1.857142857142858317, 1.857142857142858317, 1.857142857142858317, 1.857142857142858317, 1.857142857142858317, 1.857142857142858317, 1.857142857142858317, 1.857142857142858317, 1.857142857142858317, 1.857142857142858317, 1.857142857142858317, 1.857142857142858317, 1.857142857142858317, 1.857142857142858317, 1.857142857142858317, 1.857142857142858317, 1.857142857142858317),
 ( 1.000000000000000000, 1.000000000000000000, 1.000000000000000000, 1.000000000000000000, 1.000000000000000000, 1.000000000000000000, 1.000000000000000000, 1.000000000000000000, 1.000000000000000000, 1.000000000000000000, 1.000000000000000000, 1.000000000000000000, 1.000000000000000000, 1.000000000000000000, 1.000000000000000000, 1.000000000000000000, 1.000000000000000000, 1.000000000000000000, 1.000000000000000000, 1.000000000000000000, 1.000000000000000000, 1.000000000000000000, 1.000000000000000000, 1.000000000000000000, 1.000000000000000000, 1.000000000000000000, 1.000000000000000000, 1.000000000000000000, 1.000000000000000000, 1.000000000000000000, 1.000000000000000000, 1.000000000000000000, 1.000000000000000000, 1.000000000000000000) ) ) 
 REPRESENTATION_ITEM ( '' )  SURFACE ( )  );
#37009 = DIRECTION ( 'NONE',  ( -1.000000000000000000, -0.000000000000000000, -0.000000000000000000 ) ) ;
#37010 = CARTESIAN_POINT ( 'NONE',  ( 6.921856739985489781, 41.59435684990518922, -70.13580383465753698 ) ) ;
#37011 = CARTESIAN_POINT ( 'NONE',  ( 0.4969600502617528281, -8.860760056385748484, -0.6527133886630291926 ) ) ;
#37012 = CARTESIAN_POINT ( 'NONE',  ( 2.761899744546835519E-15, 41.79151656018385097, 22.55262289886175608 ) ) ;
#37013 =( LENGTH_UNIT ( ) NAMED_UNIT ( * ) SI_UNIT ( .MILLI., .METRE. ) );
#37014 = ORIENTED_EDGE ( 'NONE', *, *, #2655, .F. ) ;
#37015 = CARTESIAN_POINT ( 'NONE',  ( 2.783335637615752756, -60.00000000000000711, -42.63908079511851668 ) ) ;
#37017 = CARTESIAN_POINT ( 'NONE',  ( 29.47255165424405021, -60.33275022954688893, 36.60376788069852694 ) ) ;
#37016 = CARTESIAN_POINT ( 'NONE',  ( -74.04808884210443409, -14.21045842199433018, 133.5060932470338741 ) ) ;
#37018 = CARTESIAN_POINT ( 'NONE',  ( -3.068228200247434202E-15, 53.37899725327129374, 25.05398456423234066 ) ) ;
#37019 = EDGE_LOOP ( 'NONE', ( #61203, #50798, #39742, #30152 ) ) ;
#37020 = EDGE_CURVE ( 'NONE', #51812, #942, #23310, .T. ) ;
#37021 = CARTESIAN_POINT ( 'NONE',  ( -38.83480971963878403, -32.60089154014189461, 36.29250106144353083 ) ) ;
#37022 = ORIENTED_EDGE ( 'NONE', *, *, #21862, .F. ) ;
#37023 = CARTESIAN_POINT ( 'NONE',  ( -25.05982991920904368, -4.285714285714296246, 3.301565691951511727 ) ) ;
#37024 = FACE_OUTER_BOUND ( 'NONE', #13754, .T. ) ;
#37025 = CARTESIAN_POINT ( 'NONE',  ( -43.69871659247020546, 464.4396234996537487, 7.060974336457711331 ) ) ;
#37026 = CARTESIAN_POINT ( 'NONE',  ( -1.221877481064467252, 51.58286532492357424, -9.308967581158638538 ) ) ;
#37027 = CARTESIAN_POINT ( 'NONE',  ( 7.986452802927061612, -61.02690242308113966, 0.5332468218996361253 ) ) ;
#37028 = CARTESIAN_POINT ( 'NONE',  ( 0.1061556211655369231, -6.421950209808287902, -1.876855952934449290 ) ) ;
#37029 = ORIENTED_EDGE ( 'NONE', *, *, #93636, .F. ) ;
#37030 = CARTESIAN_POINT ( 'NONE',  ( -59.57757130603854279, -38.34325986228989791, 95.06209312383862198 ) ) ;
#37031 = DIRECTION ( 'NONE',  ( 0.000000000000000000, 1.000000000000000000, 0.000000000000000000 ) ) ;
#37032 = CARTESIAN_POINT ( 'NONE',  ( 99.71799369003751679, -30.00000000000000000, 186.7405845989215152 ) ) ;
#37033 = CARTESIAN_POINT ( 'NONE',  ( 32.59513272651155802, 40.75989716404614427, -62.80708417208141725 ) ) ;
#37034 = CARTESIAN_POINT ( 'NONE',  ( -5.981118819178459667, -81.02816543819942297, 0.5452870891823808908 ) ) ;
#37035 = CARTESIAN_POINT ( 'NONE',  ( 81.43683860099746141, -30.00000000000000000, -9.778545213351637955 ) ) ;
#37036 = CIRCLE ( 'NONE', #19873, 7.000000000000000000 ) ;
#37037 = CARTESIAN_POINT ( 'NONE',  ( -3.400000000000000355, 4.163799117101001052E-16, -3.852324522925831385 ) ) ;
#37038 = ORIENTED_EDGE ( 'NONE', *, *, #102852, .F. ) ;
#37039 = EDGE_CURVE ( 'NONE', #68858, #78191, #21118, .T. ) ;
#37040 = EDGE_LOOP ( 'NONE', ( #97034, #27861 ) ) ;
#37041 = VERTEX_POINT ( 'NONE', #81490 ) ;
#37042 = PLANE ( 'NONE',  #26748 ) ;
#37043 = CARTESIAN_POINT ( 'NONE',  ( 16.52731600354976393, 43.98685737190852763, -87.77869701378344303 ) ) ;
#37044 = CARTESIAN_POINT ( 'NONE',  ( 29.83349330513380693, -4.000000000000000000, 4.898587196589415787E-16 ) ) ;
#37045 = CARTESIAN_POINT ( 'NONE',  ( -5.656854249492379694, -16.62500000409677270, -5.656854249492380582 ) ) ;
#37046 = SURFACE_SIDE_STYLE ('',( #12721 ) ) ;
#37047 = CARTESIAN_POINT ( 'NONE',  ( -7.414346147791995634, -87.64589157662263119, -3.010818766110534561 ) ) ;
#37048 = DIRECTION ( 'NONE',  ( 0.000000000000000000, -1.000000000000000000, 0.000000000000000000 ) ) ;
#37049 = ORIENTED_EDGE ( 'NONE', *, *, #70960, .F. ) ;
#37050 = EDGE_CURVE ( 'NONE', #105469, #26386, #81634, .T. ) ;
#37051 = CARTESIAN_POINT ( 'NONE',  ( 30.10565283232790179, 7.858405490276857641, 42.03377155531566700 ) ) ;
#37052 = ORIENTED_EDGE ( 'NONE', *, *, #16962, .T. ) ;
#37053 = CARTESIAN_POINT ( 'NONE',  ( -5.094000037296077643, -62.55365876228777466, -3.174960020027664420 ) ) ;
#37054 = CARTESIAN_POINT ( 'NONE',  ( 60.39313911039658223, -38.34249553177825476, 97.64561399884981086 ) ) ;
#37055 = CARTESIAN_POINT ( 'NONE',  ( -32.82691535583477105, 485.1045372766795367, 1.724905475514941999 ) ) ;
#37056 = CARTESIAN_POINT ( 'NONE',  ( 28.98483177930387811, 297.3119720135404123, 2.475370038500326331 ) ) ;
#37057 = EDGE_CURVE ( 'NONE', #94943, #43338, #102792, .T. ) ;
#37058 = DIRECTION ( 'NONE',  ( -1.000000000000000000, -0.000000000000000000, -0.000000000000000000 ) ) ;
#37059 = CARTESIAN_POINT ( 'NONE',  ( 65.12892237437687015, -22.10168432192453380, 77.58864540890802175 ) ) ;
#37060 = ORIENTED_EDGE ( 'NONE', *, *, #17966, .F. ) ;
#37061 = DIRECTION ( 'NONE',  ( -0.000000000000000000, -0.000000000000000000, 1.000000000000000000 ) ) ;
#37062 = DIRECTION ( 'NONE',  ( -1.000000000000000000, -1.224606353822377258E-16, -0.000000000000000000 ) ) ;
#37063 = FACE_OUTER_BOUND ( 'NONE', #78837, .T. ) ;
#37064 = LINE ( 'NONE', #85598, #46265 ) ;
#37065 = CIRCLE ( 'NONE', #54163, 4.000000000000001776 ) ;
#37066 = EDGE_LOOP ( 'NONE', ( #37826, #22944, #2569, #11716 ) ) ;
#37067 = PRESENTATION_STYLE_ASSIGNMENT (( #96346 ) ) ;
#37068 = CARTESIAN_POINT ( 'NONE',  ( -4.571008445750557314, -2.193282516568174856, 102.5889671997070849 ) ) ;
#37069 = CARTESIAN_POINT ( 'NONE',  ( -1.000000000000000444, -50.00000000000000000, 44.97220075561142494 ) ) ;
#37070 = CARTESIAN_POINT ( 'NONE',  ( 41.82792046605465686, 1.340359594676612611E-15, 0.000000000000000000 ) ) ;
#37071 = CARTESIAN_POINT ( 'NONE',  ( 0.000000000000000000, 0.000000000000000000, 4.000000000000000000 ) ) ;
#37072 = EDGE_CURVE ( 'NONE', #39953, #25507, #61458, .T. ) ;
#37073 = CIRCLE ( 'NONE', #26753, 0.5000000000000004441 ) ;
#37074 = CARTESIAN_POINT ( 'NONE',  ( 0.000000000000000000, -19.99999999999998934, 0.000000000000000000 ) ) ;
#37075 = VECTOR ( 'NONE', #31178, 1000.000000000000000 ) ;
#37076 = CARTESIAN_POINT ( 'NONE',  ( 5.589124336234648993, 4.278671059403449384, -6.219623095964921689 ) ) ;
#37077 = PRESENTATION_LAYER_ASSIGNMENT (  '', '', ( #83523 ) ) ;
#37078 = CARTESIAN_POINT ( 'NONE',  ( 85.89238073966772902, -42.87991800006673770, 188.0195928903932270 ) ) ;
#37079 = CARTESIAN_POINT ( 'NONE',  ( -5.322902945112135242, 24.87962054568887282, -43.61635594746744715 ) ) ;
#37080 = B_SPLINE_CURVE_WITH_KNOTS ( 'NONE', 3,
 ( #64470, #38611, #104928, #31068, #105958, #62355, #104373, #47197, #21378, #39139, #63946, #6743, #46161, #54215, #87156, #96832, #39665, #13237 ),
 .UNSPECIFIED., .F., .F.,
 ( 4, 2, 2, 2, 2, 2, 2, 2, 4 ),
 ( 0.000000000000000000, 0.06143467464390223176, 0.1228693492878044635, 0.2457386985756090381, 0.3686080478634136126, 0.4914773971512180761, 0.7372160957268271142, 0.8600854450146315777, 0.9829547943024361523 ),
 .UNSPECIFIED. ) ;
#37081 = CARTESIAN_POINT ( 'NONE',  ( -8.571529135618341400, 24.05510615524122642, 5.000000000001270095 ) ) ;
#37082 = ORIENTED_EDGE ( 'NONE', *, *, #24353, .F. ) ;
#37083 = MECHANICAL_DESIGN_GEOMETRIC_PRESENTATION_REPRESENTATION (  '', ( #42190 ), #93861 ) ;
#37084 = CARTESIAN_POINT ( 'NONE',  ( 44.73608156750558607, -57.67080212258656502, -40.94571872030276438 ) ) ;
#37085 =( NAMED_UNIT ( * ) SI_UNIT ( $, .STERADIAN. ) SOLID_ANGLE_UNIT ( ) );
#37086 = SURFACE_STYLE_USAGE ( .BOTH. , #86684 ) ;
#37087 = CARTESIAN_POINT ( 'NONE',  ( 5.000000000000000000, -15.62228920881129390, 12.61250543006183378 ) ) ;
#37088 = MECHANICAL_DESIGN_GEOMETRIC_PRESENTATION_REPRESENTATION (  '', ( #52579 ), #105934 ) ;
#37089 = CARTESIAN_POINT ( 'NONE',  ( -99.41669103005973795, -30.00000000000000355, 148.3901553398027318 ) ) ;
#37090 = ADVANCED_FACE ( 'NONE', ( #72363 ), #72878, .F. ) ;
#37091 = LINE ( 'NONE', #61886, #98567 ) ;
#37092 = CARTESIAN_POINT ( 'NONE',  ( 19.37286937753119176, -57.67185718821608731, 42.13248506237696489 ) ) ;
#37094 = CARTESIAN_POINT ( 'NONE',  ( 20.24579557674103469, 304.8297271373346575, -10.00469232190998525 ) ) ;
#37093 = DIRECTION ( 'NONE',  ( 0.000000000000000000, -1.000000000000000000, 0.000000000000000000 ) ) ;
#37095 = ADVANCED_FACE ( 'NONE', ( #73408 ), #11446, .T. ) ;
#37096 = CARTESIAN_POINT ( 'NONE',  ( 30.00000000000000000, 500.0000000000002274, 0.000000000000000000 ) ) ;
#37097 = CARTESIAN_POINT ( 'NONE',  ( -19.11030064134297035, 50.00000000000000711, 60.43649428885221653 ) ) ;
#37098 = SURFACE_STYLE_USAGE ( .BOTH. , #68374 ) ;
#37099 = CARTESIAN_POINT ( 'NONE',  ( 32.62207953394533178, 5.000000000000002665, 0.000000000000000000 ) ) ;
#37100 = CARTESIAN_POINT ( 'NONE',  ( 11.58986075927344750, -16.51611378721433709, -34.67831674966147659 ) ) ;
#37101 = FACE_OUTER_BOUND ( 'NONE', #55026, .T. ) ;
#37102 = DIRECTION ( 'NONE',  ( -1.000000000000000000, 0.000000000000000000, 0.000000000000000000 ) ) ;
#37103 = ORIENTED_EDGE ( 'NONE', *, *, #101781, .T. ) ;
#37104 = FACE_OUTER_BOUND ( 'NONE', #83276, .T. ) ;
#37105 = CARTESIAN_POINT ( 'NONE',  ( -18.09414824793106291, -49.92059396303074692, 32.54756357241360121 ) ) ;
#37106 = EDGE_CURVE ( 'NONE', #50441, #77482, #51099, .T. ) ;
#37107 =( GEOMETRIC_REPRESENTATION_CONTEXT ( 3 ) GLOBAL_UNCERTAINTY_ASSIGNED_CONTEXT ( ( #52365 ) ) GLOBAL_UNIT_ASSIGNED_CONTEXT ( ( #87594, #86019, #63326 ) ) REPRESENTATION_CONTEXT ( 'NONE', 'WORKASPACE' ) );
#37108 = ADVANCED_FACE ( 'NONE', ( #85249 ), #43720, .T. ) ;
#37110 = CARTESIAN_POINT ( 'NONE',  ( 40.05546360247942772, 485.1954875884470084, -4.343530646189435629 ) ) ;
#37109 = CARTESIAN_POINT ( 'NONE',  ( -86.29988659680776664, -60.00000000000005684, -13.08005935856397706 ) ) ;
#37111 = EDGE_LOOP ( 'NONE', ( #61574, #45860, #2364, #12315 ) ) ;
#37112 = EDGE_CURVE ( 'NONE', #6290, #74736, #26984, .T. ) ;
#37113 = CARTESIAN_POINT ( 'NONE',  ( 2.099928008175702901E-23, 44.08548369317413318, -16.25000000000000000 ) ) ;
#37114 = VERTEX_POINT ( 'NONE', #68549 ) ;
#37115 = FACE_OUTER_BOUND ( 'NONE', #76990, .T. ) ;
#37116 = CARTESIAN_POINT ( 'NONE',  ( -4.284822031654928587, -1.092833614412262122, 104.4267991316945370 ) ) ;
#37117 = CARTESIAN_POINT ( 'NONE',  ( -9.581570546826366552, -59.99999999999998579, -42.43254358624957234 ) ) ;
#37118 = VERTEX_POINT ( 'NONE', #76610 ) ;
#37119 = DIRECTION ( 'NONE',  ( 1.000000000000000000, 0.000000000000000000, -1.224646799147353207E-16 ) ) ;
#37120 = LINE ( 'NONE', #103408, #93652 ) ;
#37121 = CARTESIAN_POINT ( 'NONE',  ( 102.5598772604434146, -52.71961633189020091, 191.0344027114808512 ) ) ;
#37122 = CARTESIAN_POINT ( 'NONE',  ( 40.62786202543021830, -35.40383002152289293, 38.30709763539996970 ) ) ;
#37123 = ORIENTED_EDGE ( 'NONE', *, *, #70933, .T. ) ;
#37124 = AXIS2_PLACEMENT_3D ( 'NONE', #106408, #65439, #91839 ) ;
#37125 = VERTEX_POINT ( 'NONE', #1648 ) ;
#37126 = ORIENTED_EDGE ( 'NONE', *, *, #42643, .T. ) ;
#37127 = CARTESIAN_POINT ( 'NONE',  ( 24.51862614704669596, 305.4800964025654366, 10.29769302249151863 ) ) ;
#37128 = CARTESIAN_POINT ( 'NONE',  ( 0.000000000000000000, 34.00000000000000000, -8.000000000000000000 ) ) ;
#37129 = EDGE_LOOP ( 'NONE', ( #3411, #212, #101844, #84236 ) ) ;
#37130 = CIRCLE ( 'NONE', #31957, 4.000000000000007105 ) ;
#37131 = CARTESIAN_POINT ( 'NONE',  ( -7.048357505843686255, 41.75164249415629314, -68.91429205804081448 ) ) ;
#37132 = CARTESIAN_POINT ( 'NONE',  ( -95.43381492254501097, -60.00000000004885692, 32.99689897427253982 ) ) ;
#37133 = DIRECTION ( 'NONE',  ( 0.000000000000000000, 0.000000000000000000, 1.000000000000000000 ) ) ;
#37134 = CARTESIAN_POINT ( 'NONE',  ( 93.55038125663071469, -60.00000000000243006, -16.95329214822379882 ) ) ;
#37135 = CARTESIAN_POINT ( 'NONE',  ( -15.92666961941153758, -5.000000000000000000, 4.023340478472887227 ) ) ;
#37136 = CARTESIAN_POINT ( 'NONE',  ( -6.232334879375827974, 41.74193240945501771, -58.83489572151871982 ) ) ;
#37137 = AXIS2_PLACEMENT_3D ( 'NONE', #103977, #14422, #38221 ) ;
#37139 = CARTESIAN_POINT ( 'NONE',  ( 4.087897576844674141, -49.91562588958777980, 32.20126423648752478 ) ) ;
#37138 = CARTESIAN_POINT ( 'NONE',  ( -103.3502313461265771, -29.99999999999994671, 116.5677832811329893 ) ) ;
#37140 = EDGE_CURVE ( 'NONE', #15506, #57232, #51264, .T. ) ;
#37141 = CARTESIAN_POINT ( 'NONE',  ( -47.63688977005685388, -49.90354645496473296, 50.26338200732071471 ) ) ;
#37142 = ORIENTED_EDGE ( 'NONE', *, *, #84767, .F. ) ;
#37143 = CARTESIAN_POINT ( 'NONE',  ( 2.182379536667797826, -70.50492906290401152, 13.16884392366768353 ) ) ;
#37144 = MECHANICAL_DESIGN_GEOMETRIC_PRESENTATION_REPRESENTATION (  '', ( #30187 ), #18197 ) ;
#37145 = ORIENTED_EDGE ( 'NONE', *, *, #103403, .F. ) ;
#37146 = AXIS2_PLACEMENT_3D ( 'NONE', #102118, #52498, #54082 ) ;
#37147 = CARTESIAN_POINT ( 'NONE',  ( 38.83413156601710625, 459.9242647137448898, 1.954013010003052830 ) ) ;
#37148 = COLOUR_RGB ( '', 0.40784314, 0.44705882, 0.49803922) ;
#37149 = VECTOR ( 'NONE', #48598, 1000.000000000000114 ) ;
#37150 = CARTESIAN_POINT ( 'NONE',  ( 5.728413875956870349, -6.419357735466014958, 1.802282772585248827 ) ) ;
#37151 = ORIENTED_EDGE ( 'NONE', *, *, #80172, .F. ) ;
#37152 = CARTESIAN_POINT ( 'NONE',  ( -6.098092868604570782, -7.477803449953040804, 13.82040600116227758 ) ) ;
#37153 = CIRCLE ( 'NONE', #73271, 8.000000000000000000 ) ;
#37154 = ORIENTED_EDGE ( 'NONE', *, *, #79119, .F. ) ;
#37155 = CARTESIAN_POINT ( 'NONE',  ( 55.69284664406904284, -38.34494919613591435, 83.45409790606751699 ) ) ;
#37156 =( NAMED_UNIT ( * ) PLANE_ANGLE_UNIT ( ) SI_UNIT ( $, .RADIAN. ) );
#37157 = CARTESIAN_POINT ( 'NONE',  ( 19.00000000000001421, -3.999999999999999112, -2.500000000000000000 ) ) ;
#37158 = AXIS2_PLACEMENT_3D ( 'NONE', #81595, #15294, #6667 ) ;
#37159 = CARTESIAN_POINT ( 'NONE',  ( 36.40416150948652785, 42.00000000008225953, 47.37019975542485639 ) ) ;
#37160 = CARTESIAN_POINT ( 'NONE',  ( 99.05156608437981447, -30.00000000000000355, 188.7076821412088918 ) ) ;
#37161 = ADVANCED_FACE ( 'NONE', ( #84188 ), #76912, .F. ) ;
#37162 = CARTESIAN_POINT ( 'NONE',  ( -0.5692325763115247961, 36.34704713563726131, 29.61603353372992586 ) ) ;
#37163 = EDGE_LOOP ( 'NONE', ( #82704, #22247, #43620, #12382, #28370 ) ) ;
#37164 = ORIENTED_EDGE ( 'NONE', *, *, #51619, .F. ) ;
#37165 = VERTEX_POINT ( 'NONE', #101436 ) ;
#37166 = CARTESIAN_POINT ( 'NONE',  ( 54.49441714554848915, -36.02968114152674417, 57.85172732363746917 ) ) ;
#37167 = DIRECTION ( 'NONE',  ( -1.000000000000000000, -0.000000000000000000, -0.000000000000000000 ) ) ;
#37168 = CARTESIAN_POINT ( 'NONE',  ( -46.00000000000001421, 460.3161862120084606, 7.035773190462103699 ) ) ;
#37169 = ORIENTED_EDGE ( 'NONE', *, *, #8993, .T. ) ;
#37170 = CARTESIAN_POINT ( 'NONE',  ( -86.02727662308166146, -38.36114455327187045, -21.87132400657947429 ) ) ;
#37171 = ORIENTED_EDGE ( 'NONE', *, *, #101768, .T. ) ;
#37172 = PLANE ( 'NONE',  #98302 ) ;
#37173 = CARTESIAN_POINT ( 'NONE',  ( 101.5818437543623531, -38.45065087239409962, 199.8849258718219630 ) ) ;
#37174 = CARTESIAN_POINT ( 'NONE',  ( 14.09641130086054872, 20.98415506194422164, 6.027230611388303849 ) ) ;
#37175 = CARTESIAN_POINT ( 'NONE',  ( 82.65689217004747036, -37.85983059181354804, 4.241147794711082497 ) ) ;
#37176 = CARTESIAN_POINT ( 'NONE',  ( 0.4033376246892486083, 4.059728990630805612, 5.968343123267133343 ) ) ;
#37177 = CARTESIAN_POINT ( 'NONE',  ( -5.000000000000000888, -4.000000000000000000, 42.58845726811989607 ) ) ;
#37178 = CARTESIAN_POINT ( 'NONE',  ( 41.96737725787325957, 484.5368175928538221, -2.772775517607982465 ) ) ;
#37179 = EDGE_CURVE ( 'NONE', #55349, #74552, #68302, .T. ) ;
#37180 = CARTESIAN_POINT ( 'NONE',  ( 0.000000000000000000, -5.000000000000000000, 0.000000000000000000 ) ) ;
#37181 = CARTESIAN_POINT ( 'NONE',  ( 1.889561568099859423, -0.09386489487440055624, 101.9317830238467195 ) ) ;
#37182 = ORIENTED_EDGE ( 'NONE', *, *, #4236, .F. ) ;
#37183 = EDGE_CURVE ( 'NONE', #61560, #14947, #76079, .T. ) ;
#37184 = CARTESIAN_POINT ( 'NONE',  ( 0.000000000000000000, 0.000000000000000000, 0.000000000000000000 ) ) ;
#37185 = CARTESIAN_POINT ( 'NONE',  ( 15.98857071195775781, 36.61411899915854917, -24.05954505250366893 ) ) ;
#37186 = CARTESIAN_POINT ( 'NONE',  ( -3.151705372620861478, 111.9488642000127356, 4.999999999999999112 ) ) ;
#37187 = ORIENTED_EDGE ( 'NONE', *, *, #67199, .T. ) ;
#37188 = CARTESIAN_POINT ( 'NONE',  ( -30.72562631177394010, 313.8450617825646987, -6.865185343166496423 ) ) ;
#37189 = CARTESIAN_POINT ( 'NONE',  ( -36.83858993814808969, 310.7308067699071330, 13.74755661074275004 ) ) ;
#37190 = CARTESIAN_POINT ( 'NONE',  ( -11.33049201282551977, -4.963977770834580916, -77.06423821558743725 ) ) ;
#37191 = CARTESIAN_POINT ( 'NONE',  ( 5.656854249492378806, -20.18749999999999289, 5.656854249492381470 ) ) ;
#37192 = CARTESIAN_POINT ( 'NONE',  ( -28.95748274387464605, -23.76855312348390825, 38.32284098381386173 ) ) ;
#37193 = DIRECTION ( 'NONE',  ( 0.000000000000000000, 0.000000000000000000, 1.000000000000000000 ) ) ;
#37194 = ORIENTED_EDGE ( 'NONE', *, *, #33108, .F. ) ;
#37195 = CARTESIAN_POINT ( 'NONE',  ( 82.72527133745752792, -60.86633776179802169, 189.9846870754455210 ) ) ;
#37196 = CARTESIAN_POINT ( 'NONE',  ( -38.33026151711676022, 27.37213072108648504, 13.20981099482207988 ) ) ;
#37197 = DIRECTION ( 'NONE',  ( -1.000000000000000000, 0.000000000000000000, 0.000000000000000000 ) ) ;
#37198 = ORIENTED_EDGE ( 'NONE', *, *, #103232, .T. ) ;
#37199 = EDGE_CURVE ( 'NONE', #88353, #56114, #6946, .T. ) ;
#37200 = CARTESIAN_POINT ( 'NONE',  ( -97.60405816678809288, -45.26544898532436889, 115.8977766532089930 ) ) ;
#37201 = DIRECTION ( 'NONE',  ( 0.000000000000000000, 0.9900230405585784821, 0.1409055682474875948 ) ) ;
#37202 = CARTESIAN_POINT ( 'NONE',  ( -10.19007819943908011, -5.000000000014482637, -96.34610920171921578 ) ) ;
#37203 = CARTESIAN_POINT ( 'NONE',  ( -29.68315524076956180, 8.302504244945341227, 42.10535821593508388 ) ) ;
#37204 = DIRECTION ( 'NONE',  ( 0.000000000000000000, 1.000000000000000000, 0.000000000000000000 ) ) ;
#37205 = AXIS2_PLACEMENT_3D ( 'NONE', #24824, #57677, #66319 ) ;
#37206 = SURFACE_SIDE_STYLE ('',( #93822 ) ) ;
#37207 = CARTESIAN_POINT ( 'NONE',  ( 13.89252497407058939, -22.08393062168078202, 35.78427392513001593 ) ) ;
#37208 = CARTESIAN_POINT ( 'NONE',  ( 1.509254614533485528, -0.02489260075662195343, 101.6144273468640336 ) ) ;
#37209 = CARTESIAN_POINT ( 'NONE',  ( 49.49891584455601645, -29.58924679890871090, 45.82294932986923897 ) ) ;
#37211 = CARTESIAN_POINT ( 'NONE',  ( -12.60023245287857740, 22.92871684446009439, 5.621329045441238570 ) ) ;
#37210 = DIRECTION ( 'NONE',  ( 0.000000000000000000, -1.000000000000000000, 0.000000000000000000 ) ) ;
#37212 = CARTESIAN_POINT ( 'NONE',  ( 6.618938675379662406, 296.2345938571221495, -10.01875627917898548 ) ) ;
#37213 = VECTOR ( 'NONE', #19363, 1000.000000000000000 ) ;
#37214 = SURFACE_SIDE_STYLE ('',( #45811 ) ) ;
#37215 = CARTESIAN_POINT ( 'NONE',  ( -20.25105829892553899, 294.7694562253329877, 1.919496115618561261 ) ) ;
#37216 = CIRCLE ( 'NONE', #38959, 3.309500000000007880 ) ;
#37217 = CIRCLE ( 'NONE', #64751, 10.00000000000000178 ) ;
#37218 = CARTESIAN_POINT ( 'NONE',  ( 22.61650669486618526, 1.474610560812782335E-15, 0.000000000000000000 ) ) ;
#37219 = CIRCLE ( 'NONE', #97452, 4.000000000000000888 ) ;
#37220 = VERTEX_POINT ( 'NONE', #21607 ) ;
#37221 = CARTESIAN_POINT ( 'NONE',  ( -46.00000000000000000, 461.9428920847520317, 12.03309428281920113 ) ) ;
#37222 = PRODUCT_DEFINITION_SHAPE ( 'NONE', 'NONE',  #106789 ) ;
#37223 = CIRCLE ( 'NONE', #18271, 5.000000000000011546 ) ;
#37224 = EDGE_LOOP ( 'NONE', ( #39502, #74851, #76882, #91636 ) ) ;
#37225 = CARTESIAN_POINT ( 'NONE',  ( -9.960066834909762079, -3.067139625798588121, 15.24934138179222032 ) ) ;
#37226 = CARTESIAN_POINT ( 'NONE',  ( 4.250000000000000000, 0.000000000000000000, -7.657127082228716297 ) ) ;
#37227 = AXIS2_PLACEMENT_3D ( 'NONE', #56237, #6112, #39037 ) ;
#37228 = ADVANCED_FACE ( 'NONE', ( #71695 ), #71179, .F. ) ;
#37229 = CARTESIAN_POINT ( 'NONE',  ( 0.000000000000000000, 152.0000000000000000, 0.000000000000000000 ) ) ;
#37230 = ADVANCED_FACE ( 'NONE', ( #103554 ), #12403, .T. ) ;
#37232 = CARTESIAN_POINT ( 'NONE',  ( -4.768224440014436460, -47.40888642635074746, -34.73453581626768027 ) ) ;
#37231 = CARTESIAN_POINT ( 'NONE',  ( 9.220915120640610141, 251.0445488643207739, -3.870126578504832437 ) ) ;
#37233 = ORIENTED_EDGE ( 'NONE', *, *, #91402, .F. ) ;
#37234 = CARTESIAN_POINT ( 'NONE',  ( 28.30742934768286645, 36.37554873744188910, 8.455121100274956447 ) ) ;
#37235 = CARTESIAN_POINT ( 'NONE',  ( -41.45706733914236253, 469.3213988105399608, 0.9913809832463575944 ) ) ;
#37236 = CONICAL_SURFACE ( 'NONE', #50959, 4.000000000000000000, 0.9599310885968912466 ) ;
#37237 = ORIENTED_EDGE ( 'NONE', *, *, #86113, .F. ) ;
#37238 = EDGE_CURVE ( 'NONE', #98133, #53170, #69606, .T. ) ;
#37239 = CARTESIAN_POINT ( 'NONE',  ( 5.819846122303830249, 4.937269551422740044, 4.448398286273013369 ) ) ;
#37240 = CARTESIAN_POINT ( 'NONE',  ( 0.000000000000000000, 0.000000000000000000, 5.000000000000002665 ) ) ;
#37241 = CARTESIAN_POINT ( 'NONE',  ( -91.86040266156631162, -59.99999999999997868, 11.95720016906147798 ) ) ;
#37242 = ORIENTED_EDGE ( 'NONE', *, *, #73465, .T. ) ;
#37243 = CARTESIAN_POINT ( 'NONE',  ( 7.416129379029737123, 42.00000000000000000, -59.68109090346935375 ) ) ;
#37244 = CARTESIAN_POINT ( 'NONE',  ( -5.656854249492381470, -11.56249999999999289, 5.656854249492379694 ) ) ;
#37245 = CARTESIAN_POINT ( 'NONE',  ( -9.999952458099484076, 26.00011885476135376, 0.2653554233229072357 ) ) ;
#37247 = CYLINDRICAL_SURFACE ( 'NONE', #59911, 4.000000000000000888 ) ;
#37246 = CARTESIAN_POINT ( 'NONE',  ( 9.999999999999998224, -15.00000000000000000, -9.999999999999998224 ) ) ;
#37248 = CARTESIAN_POINT ( 'NONE',  ( -83.80836329334010770, -32.51672879621551715, 166.3324284733673721 ) ) ;
#37249 = ORIENTED_EDGE ( 'NONE', *, *, #22687, .T. ) ;
#37250 = CARTESIAN_POINT ( 'NONE',  ( -2.220412017512216618, -0.000000000000000000, 16.90656889033980192 ) ) ;
#37251 = ORIENTED_EDGE ( 'NONE', *, *, #64545, .F. ) ;
#37252 = VECTOR ( 'NONE', #75019, 1000.000000000000000 ) ;
#37253 = ORIENTED_EDGE ( 'NONE', *, *, #47097, .T. ) ;
#37254 = CARTESIAN_POINT ( 'NONE',  ( -16.49565406582427940, -5.000000000000000000, 2.458857127971593393 ) ) ;
#37255 = CARTESIAN_POINT ( 'NONE',  ( -5.818631380449454049, -64.91365770770519816, 14.26591935523900645 ) ) ;
#37256 =( NAMED_UNIT ( * ) PLANE_ANGLE_UNIT ( ) SI_UNIT ( $, .RADIAN. ) );
#37257 = VERTEX_POINT ( 'NONE', #104072 ) ;
#37258 = DIRECTION ( 'NONE',  ( -1.000000000000000000, -1.224606353822377258E-16, -0.000000000000000000 ) ) ;
#37259 = DIRECTION ( 'NONE',  ( 5.178224577996835961E-15, 0.3241911592372989093, 0.9459915920727711702 ) ) ;
#37260 = CARTESIAN_POINT ( 'NONE',  ( -95.95698421656685184, -57.67166530053860640, 41.39248336299490916 ) ) ;
#37261 = CARTESIAN_POINT ( 'NONE',  ( 4.699999999999999289, 0.000000000000000000, 0.000000000000000000 ) ) ;
#37262 = CARTESIAN_POINT ( 'NONE',  ( 44.12585837658421895, 464.4133740036029963, 9.756218680429697088 ) ) ;
#37263 = CARTESIAN_POINT ( 'NONE',  ( 23.55048488053951417, 27.32134238698565554, 33.17259636481905005 ) ) ;
#37264 = PRESENTATION_STYLE_ASSIGNMENT (( #30216 ) ) ;
#37265 = CARTESIAN_POINT ( 'NONE',  ( 65.67877680238373728, -29.99999999999995026, -31.25179767064105363 ) ) ;
#37266 = CARTESIAN_POINT ( 'NONE',  ( -73.77866262884730020, -30.00000000000000711, 147.9509455049667395 ) ) ;
#37267 = ADVANCED_FACE ( 'NONE', ( #94420 ), #37799, .T. ) ;
#37268 = CARTESIAN_POINT ( 'NONE',  ( -54.06122363970894895, -46.44091381175636002, 61.05526970200972414 ) ) ;
#37269 = ORIENTED_EDGE ( 'NONE', *, *, #92857, .T. ) ;
#37270 = FILL_AREA_STYLE ('',( #62073 ) ) ;
#37271 = VERTEX_POINT ( 'NONE', #54979 ) ;
#37272 = CARTESIAN_POINT ( 'NONE',  ( -101.5936365789223856, -52.72169881341778819, 192.6675009559352532 ) ) ;
#37273 = CARTESIAN_POINT ( 'NONE',  ( 96.81745522565726958, -37.99999999999980815, 192.8977754549547967 ) ) ;
#37274 = CARTESIAN_POINT ( 'NONE',  ( 31.14131030317610538, 5.000000000000002665, 0.000000000000000000 ) ) ;
#37275 = ADVANCED_FACE ( 'NONE', ( #87909 ), #1188, .T. ) ;
#37276 = ORIENTED_EDGE ( 'NONE', *, *, #86051, .F. ) ;
#37277 = CARTESIAN_POINT ( 'NONE',  ( 19.33986106772935543, 49.89322054401328188, 61.21774086638057355 ) ) ;
#37278 = VECTOR ( 'NONE', #44598, 1000.000000000000114 ) ;
#37279 = CARTESIAN_POINT ( 'NONE',  ( 95.42421628608209971, -2.002967142162725287E-29, 5.000000000000011546 ) ) ;
#37280 = CARTESIAN_POINT ( 'NONE',  ( 7.188101187499999156, -13.62500000204838457, 2.977408999572654924 ) ) ;
#37281 = CARTESIAN_POINT ( 'NONE',  ( 25.93947128054312756, 296.0094280503604978, 10.18659011856751384 ) ) ;
#37282 = CARTESIAN_POINT ( 'NONE',  ( -6.750000000000015099, -11.69134295108991495, -13.00000000000000000 ) ) ;
#37283 = CARTESIAN_POINT ( 'NONE',  ( 7.414346147791995634, -82.35410842337736881, -3.010818766110534561 ) ) ;
#37284 = CARTESIAN_POINT ( 'NONE',  ( -35.76379064120181539, 307.0162303970107587, 12.81051142610679960 ) ) ;
#37285 = CARTESIAN_POINT ( 'NONE',  ( -9.032229468219194146, 43.92653636418285856, -14.03110142013872519 ) ) ;
#37286 = EDGE_CURVE ( 'NONE', #82494, #74417, #61539, .T. ) ;
#37287 = CARTESIAN_POINT ( 'NONE',  ( 0.000000000000000000, 1.089935651241144357E-15, 8.900000000000000355 ) ) ;
#37288 = CONICAL_SURFACE ( 'NONE', #95776, 4.172000000000001485, 0.9599310885968750373 ) ;
#37289 = CARTESIAN_POINT ( 'NONE',  ( 33.58349330513380693, 1.593028355512270962E-15, 0.000000000000000000 ) ) ;
#37290 = CARTESIAN_POINT ( 'NONE',  ( -28.24552693224729794, -32.53317030909266805, 31.34561990023201972 ) ) ;
#37291 = ORIENTED_EDGE ( 'NONE', *, *, #47870, .F. ) ;
#37292 = CARTESIAN_POINT ( 'NONE',  ( 48.53168779318080084, -22.21808085982860703, 43.06350356119703804 ) ) ;
#37293 = CARTESIAN_POINT ( 'NONE',  ( 0.000000000000000000, 0.000000000000000000, 0.000000000000000000 ) ) ;
#37294 = CYLINDRICAL_SURFACE ( 'NONE', #103046, 5.000000000000002665 ) ;
#37295 = CARTESIAN_POINT ( 'NONE',  ( -89.68492724561200191, -38.52030381430500938, 200.4876829703964347 ) ) ;
#37296 = CONICAL_SURFACE ( 'NONE', #80274, 7.500000000000000888, 0.8594454914424817238 ) ;
#37297 = ORIENTED_EDGE ( 'NONE', *, *, #10539, .T. ) ;
#37298 = CARTESIAN_POINT ( 'NONE',  ( 90.75236045938613927, -38.34260670370428414, 6.374254514712724529 ) ) ;
#37299 = SURFACE_STYLE_USAGE ( .BOTH. , #94991 ) ;
#37300 = CARTESIAN_POINT ( 'NONE',  ( -49.18559949472793846, 8.441045694768776642, -15.12439388195359591 ) ) ;
#37302 = FACE_OUTER_BOUND ( 'NONE', #35228, .T. ) ;
#37301 = PRESENTATION_LAYER_ASSIGNMENT (  '', '', ( #95854 ) ) ;
#37303 = CONICAL_SURFACE ( 'NONE', #13142, 8.542937654374686218, 1.221730476396047704 ) ;
#37304 = CARTESIAN_POINT ( 'NONE',  ( 6.188824268254729866, 41.46400356848157998, -70.81766461687159619 ) ) ;
#37305 = FACE_OUTER_BOUND ( 'NONE', #19313, .T. ) ;
#37306 = CIRCLE ( 'NONE', #90620, 2.999999999999999112 ) ;
#37307 = PLANE ( 'NONE',  #26336 ) ;
#37308 = CARTESIAN_POINT ( 'NONE',  ( 111.3516866354051160, -59.99999999999999289, 185.3684648513999491 ) ) ;
#37309 = CIRCLE ( 'NONE', #56168, 8.857142857142855874 ) ;
#37310 = CONICAL_SURFACE ( 'NONE', #87183, 4.172000000000009479, 0.9599310885968813656 ) ;
#37311 =( BOUNDED_SURFACE ( )  B_SPLINE_SURFACE ( 3, 2, ( 
 ( #9439, #42898, #791 ),
 ( #67185, #75792, #52041 ),
 ( #1887, #42358, #92501 ),
 ( #10519, #43435, #76315 ) ),
 .UNSPECIFIED., .F., .F., .F. ) 
 B_SPLINE_SURFACE_WITH_KNOTS ( ( 4, 4 ),
 ( 3, 3 ),
 ( -1.734723475976807094E-17, 0.002491432948283776611 ),
 ( 0.000000000000000000, 1.000000000000000000 ),
 .UNSPECIFIED. ) 
 GEOMETRIC_REPRESENTATION_ITEM ( )  RATIONAL_B_SPLINE_SURFACE ( (
 ( 1.000000000000000000, 0.7978714159193172062, 1.000000000000000000),
 ( 1.000000000000000000, 0.8097755972627500576, 1.000000000000000000),
 ( 1.000000000000000000, 0.8213938805860364623, 1.000000000000000000),
 ( 1.000000000000000000, 0.8328393170029456671, 1.000000000000000000) ) ) 
 REPRESENTATION_ITEM ( '' )  SURFACE ( )  );
#37312 = CARTESIAN_POINT ( 'NONE',  ( -7.744991119775239241, -68.46438785425135620, -2.016316005557100333 ) ) ;
#37313 = VERTEX_POINT ( 'NONE', #49554 ) ;
#37314 = EDGE_CURVE ( 'NONE', #8448, #86295, #46106, .T. ) ;
#37315 = FACE_OUTER_BOUND ( 'NONE', #84855, .T. ) ;
#37316 = CARTESIAN_POINT ( 'NONE',  ( -81.08763726869537436, -30.00000000000003908, 2.435961963529629681 ) ) ;
#37317 = EDGE_LOOP ( 'NONE', ( #14957, #71560 ) ) ;
#37319 = LINE ( 'NONE', #29237, #68318 ) ;
#37318 = CARTESIAN_POINT ( 'NONE',  ( -82.24571663913680197, -38.83862773915732447, 196.1822678393787953 ) ) ;
#37320 = CARTESIAN_POINT ( 'NONE',  ( 12.48211703288669838, -3.606465591134454751, -13.63114202488422855 ) ) ;
#37321 = CARTESIAN_POINT ( 'NONE',  ( -4.916373759799321341, -3.000000000000000444, 6.397334739185440711 ) ) ;
#37322 = CIRCLE ( 'NONE', #68232, 4.000000000000000888 ) ;
#37323 = CARTESIAN_POINT ( 'NONE',  ( 16.36650669486618881, 1.474610560812782335E-15, 0.000000000000000000 ) ) ;
#37324 = CARTESIAN_POINT ( 'NONE',  ( -2.977408999572654480, -14.00000000204838457, 7.188101187499999156 ) ) ;
#37325 = CIRCLE ( 'NONE', #9693, 4.000000000000001776 ) ;
#37326 = CARTESIAN_POINT ( 'NONE',  ( -3.140974613990845210, -5.000000000000002665, -73.31232788067644890 ) ) ;
#37327 = ADVANCED_FACE ( 'NONE', ( #8564 ), #89075, .T. ) ;
#37328 = EDGE_CURVE ( 'NONE', #17545, #51169, #81910, .T. ) ;
#37330 = ORIENTED_EDGE ( 'NONE', *, *, #103409, .F. ) ;
#37329 = CARTESIAN_POINT ( 'NONE',  ( -33.74362713068849473, 463.9326864247044000, 7.533159870298644201 ) ) ;
#37331 = CARTESIAN_POINT ( 'NONE',  ( 81.73802953284047135, -49.94979035245339816, 174.6693918275601618 ) ) ;
#37333 = MECHANICAL_DESIGN_GEOMETRIC_PRESENTATION_REPRESENTATION (  '', ( #7945 ), #32145 ) ;
#37332 = CARTESIAN_POINT ( 'NONE',  ( 7.869023571503454662, 64.80998104766133849, 1.348150961071065097E-30 ) ) ;
#37334 = CARTESIAN_POINT ( 'NONE',  ( 2.263183130831067924, -6.566419505188308747, -6.208110906918269833 ) ) ;
#37335 = ORIENTED_EDGE ( 'NONE', *, *, #17884, .T. ) ;
#37336 = CARTESIAN_POINT ( 'NONE',  ( 32.94330508143927716, 1.340359594676612611E-15, 0.000000000000000000 ) ) ;
#37337 = CYLINDRICAL_SURFACE ( 'NONE', #68288, 5.000000000000000888 ) ;
#37338 = DIRECTION ( 'NONE',  ( 1.000000000000000000, 0.000000000000000000, 0.000000000000000000 ) ) ;
#37339 = STYLED_ITEM ( 'NONE', ( #82055 ), #100763 ) ;
#37340 = CARTESIAN_POINT ( 'NONE',  ( 104.0908829527487711, 1.030564683017419500E-14, 0.000000000000000000 ) ) ;
#37341 = CARTESIAN_POINT ( 'NONE',  ( 17.58395415724061195, 43.20953024635295492, 6.235491673352195008 ) ) ;
#37342 = VERTEX_POINT ( 'NONE', #31801 ) ;
#37343 = FILL_AREA_STYLE_COLOUR ( '', #35101 ) ;
#37344 = B_SPLINE_CURVE_WITH_KNOTS ( 'NONE', 3,
 ( #28313, #104280, #77365, #77898, #103235, #29381, #94078, #20243, #95152, #86014, #36938, #87063, #61737, #87587, #13674, #46582, #81573, #31496, #41153, #105870, #40087, #63847, #15805, #7173, #72964, #8240, #96740, #105355, #47628, #15276, #57840, #74035, #57311, #7700 ),
 .UNSPECIFIED., .F., .F.,
 ( 4, 2, 2, 2, 2, 2, 2, 2, 2, 2, 2, 2, 2, 2, 2, 2, 4 ),
 ( 0.000000000000000000, 0.002123632632474336222, 0.004247265264948672445, 0.008494530529897344889, 0.01698906105979468978, 0.02548359158969203467, 0.03397812211958937956, 0.05096718317938406934, 0.06795624423917875911, 0.08494530529897345583, 0.1019343663587681387, 0.1104288968886654870, 0.1189234274185628215, 0.1274179579484601144, 0.1316652232134088163, 0.1337888558458831534, 0.1359124884783575182 ),
 .UNSPECIFIED. ) ;
#37345 = CARTESIAN_POINT ( 'NONE',  ( -4.506320246070885993, -48.81713945999871385, 104.3949652630312528 ) ) ;
#37346 = DIRECTION ( 'NONE',  ( -1.000000000000000000, -1.224606353822377258E-16, -0.000000000000000000 ) ) ;
#37347 = DIRECTION ( 'NONE',  ( 0.000000000000000000, 1.000000000000000000, 0.000000000000000000 ) ) ;
#37348 = CARTESIAN_POINT ( 'NONE',  ( -43.00000000000000000, 450.0000000000002274, 13.20242257375370976 ) ) ;
#37349 = CARTESIAN_POINT ( 'NONE',  ( 2.977408999572651815, -22.43750000204838813, 7.188101187500000933 ) ) ;
#37350 = UNCERTAINTY_MEASURE_WITH_UNIT (LENGTH_MEASURE( 1.000000000000000082E-05 ), #105788, 'distance_accuracy_value', 'NONE');
#37351 = DIRECTION ( 'NONE',  ( 0.000000000000000000, -1.000000000000000000, 0.000000000000000000 ) ) ;
#37352 = CARTESIAN_POINT ( 'NONE',  ( 89.99999999999997158, -60.00000000000000000, 188.5238439516623146 ) ) ;
#37353 = CIRCLE ( 'NONE', #16671, 5.000000000000002665 ) ;
#37354 = AXIS2_PLACEMENT_3D ( 'NONE', #70979, #70460, #61854 ) ;
#37355 = ORIENTED_EDGE ( 'NONE', *, *, #48252, .T. ) ;
#37356 = CARTESIAN_POINT ( 'NONE',  ( -34.99298670164664316, 490.1714394129022594, 12.08179005326680056 ) ) ;
#37357 = CARTESIAN_POINT ( 'NONE',  ( 5.299999999999999822, -7.505553499465137612, 3.546421054897781431E-16 ) ) ;
#37358 = CARTESIAN_POINT ( 'NONE',  ( -9.248416039967223057, 11.93391985751763151, -5.000000000000318856 ) ) ;
#37359 = DIRECTION ( 'NONE',  ( 0.000000000000000000, -1.000000000000000000, 0.000000000000000000 ) ) ;
#37360 = EDGE_CURVE ( 'NONE', #24844, #63754, #80855, .T. ) ;
#37361 = ORIENTED_EDGE ( 'NONE', *, *, #13029, .F. ) ;
#37362 = CARTESIAN_POINT ( 'NONE',  ( 2.500000000000002665, -30.00000000000000000, -13.00000000000000000 ) ) ;
#37363 = CARTESIAN_POINT ( 'NONE',  ( -34.68490551324229898, 463.9993046474211837, 18.60480341025478523 ) ) ;
#37364 = CIRCLE ( 'NONE', #58018, 5.000000000000001776 ) ;
#37365 = ORIENTED_EDGE ( 'NONE', *, *, #84813, .F. ) ;
#37366 = EDGE_CURVE ( 'NONE', #65995, #170, #51178, .T. ) ;
#37367 = FILL_AREA_STYLE_COLOUR ( '', #81581 ) ;
#37368 = CARTESIAN_POINT ( 'NONE',  ( -3.677502082062779731, -1.015346567123904364, 104.5296620117540272 ) ) ;
#37369 = CARTESIAN_POINT ( 'NONE',  ( 9.699016383038308931, 101.8236182855165453, 2.444973590251038775 ) ) ;
#37370 =( LENGTH_UNIT ( ) NAMED_UNIT ( * ) SI_UNIT ( .MILLI., .METRE. ) );
#37371 = UNCERTAINTY_MEASURE_WITH_UNIT (LENGTH_MEASURE( 1.000000000000000082E-05 ), #63636, 'distance_accuracy_value', 'NONE');
#37372 = CARTESIAN_POINT ( 'NONE',  ( -92.52372448017906947, -60.00000000000000000, 202.4166223421563018 ) ) ;
#37373 = PRODUCT_DEFINITION_SHAPE ( 'NONE', 'NONE',  #106811 ) ;
#37374 = VECTOR ( 'NONE', #3861, 1000.000000000000341 ) ;
#37375 = CARTESIAN_POINT ( 'NONE',  ( 17.50000000000004974, 48.00000000000341771, 64.09949417230997426 ) ) ;
#37376 = AXIS2_PLACEMENT_3D ( 'NONE', #66651, #18121, #27304 ) ;
#37377 = CARTESIAN_POINT ( 'NONE',  ( 88.20199406385988539, 5.000000000000021316, 0.000000000000000000 ) ) ;
#37378 = CARTESIAN_POINT ( 'NONE',  ( -13.00000000000003730, 249.9999999999999432, 4.000000000000002665 ) ) ;
#37379 = SURFACE_STYLE_USAGE ( .BOTH. , #102606 ) ;
#37380 = CARTESIAN_POINT ( 'NONE',  ( -85.21723363474887947, -28.80621494017632145, 174.9461519470255837 ) ) ;
#37381 = CARTESIAN_POINT ( 'NONE',  ( 25.85123526981803010, 43.59342998289417892, -74.96042727038405928 ) ) ;
#37382 =( GEOMETRIC_REPRESENTATION_CONTEXT ( 3 ) GLOBAL_UNCERTAINTY_ASSIGNED_CONTEXT ( ( #14541 ) ) GLOBAL_UNIT_ASSIGNED_CONTEXT ( ( #65980, #40117, #7733 ) ) REPRESENTATION_CONTEXT ( 'NONE', 'WORKASPACE' ) );
#37383 = ORIENTED_EDGE ( 'NONE', *, *, #46202, .T. ) ;
#37384 = FILL_AREA_STYLE_COLOUR ( '', #2680 ) ;
#37385 = EDGE_CURVE ( 'NONE', #59167, #45575, #57106, .T. ) ;
#37386 = CARTESIAN_POINT ( 'NONE',  ( 5.092539576892241904, -67.44323467208434408, 3.177249149099056869 ) ) ;
#37387 = CARTESIAN_POINT ( 'NONE',  ( -85.81038825978107809, -52.70812745589994108, 30.16071544517509651 ) ) ;
#37388 = CARTESIAN_POINT ( 'NONE',  ( -1.916513513606918240, -7.172711491781471160, -13.28747680017342248 ) ) ;
#37389 = CARTESIAN_POINT ( 'NONE',  ( -3.983822851467989423, 136.6779518951960881, -5.000000000000000888 ) ) ;
#37390 = CARTESIAN_POINT ( 'NONE',  ( 4.474494503601499140, 142.5181942220502833, -4.999999999999999112 ) ) ;
#37391 =( NAMED_UNIT ( * ) PLANE_ANGLE_UNIT ( ) SI_UNIT ( $, .RADIAN. ) );
#37392 = CARTESIAN_POINT ( 'NONE',  ( -1.905220702120325443E-14, 42.00000000000000711, -59.23741894013591036 ) ) ;
#37393 = CARTESIAN_POINT ( 'NONE',  ( 78.25600647866326653, -14.21045842199443499, 182.3349015425907851 ) ) ;
#37394 = CARTESIAN_POINT ( 'NONE',  ( -39.18206537991729022, 57.18445727710330573, 19.59103268995864511 ) ) ;
#37395 = CARTESIAN_POINT ( 'NONE',  ( -89.06819603267832974, -14.21045842199437637, 44.46121640280500031 ) ) ;
#37396 = EDGE_CURVE ( 'NONE', #12734, #65330, #56328, .T. ) ;
#37397 = CARTESIAN_POINT ( 'NONE',  ( -63.69277339041742891, -39.48556901039047062, 82.38618134814525718 ) ) ;
#37398 = EDGE_LOOP ( 'NONE', ( #53412, #23496, #46157, #20704 ) ) ;
#37399 = CARTESIAN_POINT ( 'NONE',  ( 99.10782808284749024, -14.21045842199446163, 197.1815751231716263 ) ) ;
#37400 = CARTESIAN_POINT ( 'NONE',  ( -51.48757442383521266, 38.95383793070303113, -37.45149417477429665 ) ) ;
#37401 = CARTESIAN_POINT ( 'NONE',  ( 79.10866139746512715, -59.99999999997309175, 198.8830511339313318 ) ) ;
#37402 = ORIENTED_EDGE ( 'NONE', *, *, #99307, .F. ) ;
#37403 = CARTESIAN_POINT ( 'NONE',  ( -33.95156263172587785, 464.5083255208627406, 6.608064661821428487 ) ) ;
#37404 = CARTESIAN_POINT ( 'NONE',  ( -7.188101187500002709, -18.68750000204838457, 2.977408999572647819 ) ) ;
#37405 =( NAMED_UNIT ( * ) PLANE_ANGLE_UNIT ( ) SI_UNIT ( $, .RADIAN. ) );
#37406 = EDGE_LOOP ( 'NONE', ( #59145, #84021, #105152, #5385, #90339, #11559 ) ) ;
#37407 = CARTESIAN_POINT ( 'NONE',  ( -10.45066360978664122, 46.08369782028256623, 12.90779740156196986 ) ) ;
#37408 = VERTEX_POINT ( 'NONE', #22664 ) ;
#37409 = CARTESIAN_POINT ( 'NONE',  ( -7.135888613856518958, 39.99999999999999289, -71.74865085751089566 ) ) ;
#37410 =( NAMED_UNIT ( * ) SI_UNIT ( $, .STERADIAN. ) SOLID_ANGLE_UNIT ( ) );
#37411 = CARTESIAN_POINT ( 'NONE',  ( -90.96217874645275003, -59.99999999999998579, -17.00786546406066435 ) ) ;
#37412 = CARTESIAN_POINT ( 'NONE',  ( -30.00000000000000000, 450.0000000000002274, 13.20242257375370976 ) ) ;
#37413 = CARTESIAN_POINT ( 'NONE',  ( 7.188101187499999156, -33.12500000204838813, 2.977408999572654924 ) ) ;
#37414 = CARTESIAN_POINT ( 'NONE',  ( 0.000000000000000000, 3.500000000000000000, 3.500000000000000000 ) ) ;
#37415 = CARTESIAN_POINT ( 'NONE',  ( 15.38541618194248350, -4.285714285714296246, 20.05453516056601515 ) ) ;
#37416 = CARTESIAN_POINT ( 'NONE',  ( 5.036189802310915731, 48.00000000000000000, -76.26213611587833441 ) ) ;
#37417 = FACE_OUTER_BOUND ( 'NONE', #20713, .T. ) ;
#37418 = EDGE_CURVE ( 'NONE', #36282, #39760, #15935, .T. ) ;
#37419 = CARTESIAN_POINT ( 'NONE',  ( 20.11650669486618881, -3.999999999999998224, 0.000000000000000000 ) ) ;
#37420 = FACE_OUTER_BOUND ( 'NONE', #86244, .T. ) ;
#37421 = ORIENTED_EDGE ( 'NONE', *, *, #76903, .T. ) ;
#37422 = CARTESIAN_POINT ( 'NONE',  ( 33.00000000000000000, 500.0000000000002274, -12.00000000000000711 ) ) ;
#37423 = CARTESIAN_POINT ( 'NONE',  ( 4.973317752991476048, -3.468598768254688380, 102.2736751349651456 ) ) ;
#37425 = CARTESIAN_POINT ( 'NONE',  ( 37.51919295870404625, -49.89018639253918508, 39.00778217076621956 ) ) ;
#37424 = CARTESIAN_POINT ( 'NONE',  ( -3.405129524108836847, -48.85126520984761811, 104.5473292661494753 ) ) ;
#37426 = CARTESIAN_POINT ( 'NONE',  ( -6.601913983209747983, -4.285714285713511096, 24.56594385547482418 ) ) ;
#37427 = VERTEX_POINT ( 'NONE', #6428 ) ;
#37428 = CARTESIAN_POINT ( 'NONE',  ( -43.03265099499957813, 484.2747968070553384, -0.8099405866661226749 ) ) ;
#37430 = LINE ( 'NONE', #54081, #44040 ) ;
#37429 = CARTESIAN_POINT ( 'NONE',  ( 9.363581568756892182, -5.000000000000000000, -18.67428222363854218 ) ) ;
#37431 = LINE ( 'NONE', #85417, #35459 ) ;
#37432 = DIRECTION ( 'NONE',  ( 0.000000000000000000, -1.000000000000000000, 0.000000000000000000 ) ) ;
#37433 = CARTESIAN_POINT ( 'NONE',  ( -9.500000000000000000, -5.000000000000000000, -20.99851272547259384 ) ) ;
#37434 = CARTESIAN_POINT ( 'NONE',  ( 0.000000000000000000, -79.93083296558610584, -85.00000000000000000 ) ) ;
#37435 = LINE ( 'NONE', #64340, #43145 ) ;
#37436 = EDGE_LOOP ( 'NONE', ( #104189, #28945, #105200, #60602, #11513, #62854, #105351, #29157, #66308, #62986 ) ) ;
#37437 = CARTESIAN_POINT ( 'NONE',  ( 92.42316227055287925, -60.00000000000002132, -0.1668662530303857139 ) ) ;
#37438 = DIRECTION ( 'NONE',  ( -1.000000000000000000, -1.224606353822377258E-16, -0.000000000000000000 ) ) ;
#37439 = CARTESIAN_POINT ( 'NONE',  ( 0.000000000000000000, 34.19642918197134662, -12.16579798332631945 ) ) ;
#37440 = CARTESIAN_POINT ( 'NONE',  ( -6.472170351928723697, 40.92674623573195447, -71.09138923453632231 ) ) ;
#37441 = CARTESIAN_POINT ( 'NONE',  ( -11.79370259999046411, 11.30362766250548034, -9.861606943826988214 ) ) ;
#37442 = ORIENTED_EDGE ( 'NONE', *, *, #79650, .F. ) ;
#37443 = EDGE_CURVE ( 'NONE', #99943, #48231, #105144, .T. ) ;
#37444 = CARTESIAN_POINT ( 'NONE',  ( -88.81473527931045453, -30.00000000002773604, 198.9409494650124657 ) ) ;
#37445 = ORIENTED_EDGE ( 'NONE', *, *, #65246, .T. ) ;
#37446 = CARTESIAN_POINT ( 'NONE',  ( 33.00000000000000000, 464.3970849722209095, 17.41240408234224191 ) ) ;
#37447 = CARTESIAN_POINT ( 'NONE',  ( 21.84999999999999787, -3.309499999999999886, 4.475777889183790779E-16 ) ) ;
#37448 = CARTESIAN_POINT ( 'NONE',  ( 48.10000000000000142, 0.000000000000000000, 3.309499999999999886 ) ) ;
#37449 = CARTESIAN_POINT ( 'NONE',  ( 16.12871211736549881, 21.28428926968472723, 2.982820907299407853 ) ) ;
#37451 = CARTESIAN_POINT ( 'NONE',  ( -6.500000000000000000, 1.602771114417260501, -0.1495523863686117338 ) ) ;
#37450 = AXIS2_PLACEMENT_3D ( 'NONE', #38804, #30186, #79776 ) ;
#37452 = VECTOR ( 'NONE', #101553, 1000.000000000000114 ) ;
#37453 = CARTESIAN_POINT ( 'NONE',  ( 7.188101187499999156, -33.12500000204838813, 2.977408999572654924 ) ) ;
#37454 = CARTESIAN_POINT ( 'NONE',  ( -18.00372896877115636, 34.34010858039469127, 23.10073396340781215 ) ) ;
#37455 = CARTESIAN_POINT ( 'NONE',  ( 0.000000000000000000, 304.8518027762758038, 8.936999415352287812 ) ) ;
#37457 = ADVANCED_FACE ( 'NONE', ( #40936 ), #6643, .F. ) ;
#37456 = CARTESIAN_POINT ( 'NONE',  ( 0.000000000000000000, -1.500000000000000000, 0.000000000000000000 ) ) ;
#37458 = ORIENTED_EDGE ( 'NONE', *, *, #61657, .T. ) ;
#37459 = VECTOR ( 'NONE', #11390, 1000.000000000000000 ) ;
#37460 = CONICAL_SURFACE ( 'NONE', #13225, 4.000000000000007105, 0.9599310885968835860 ) ;
#37461 = VECTOR ( 'NONE', #32455, 1000.000000000000000 ) ;
#37462 = VECTOR ( 'NONE', #6302, 1000.000000000000000 ) ;
#37464 = VERTEX_POINT ( 'NONE', #17740 ) ;
#37463 = FACE_OUTER_BOUND ( 'NONE', #2949, .T. ) ;
#37465 = CARTESIAN_POINT ( 'NONE',  ( 77.91231580246096655, -46.43304605102353122, 140.2301567752059270 ) ) ;
#37466 = CARTESIAN_POINT ( 'NONE',  ( 14.90280835358713318, 2.161282233155129795, 1.653369514896020576 ) ) ;
#37467 = ORIENTED_EDGE ( 'NONE', *, *, #4151, .F. ) ;
#37468 = EDGE_CURVE ( 'NONE', #78006, #56185, #76485, .T. ) ;
#37469 = CARTESIAN_POINT ( 'NONE',  ( -12.50000000000000178, 37.35939052609327859, -58.38223258370340574 ) ) ;
#37470 = CIRCLE ( 'NONE', #4708, 3.309500000000001663 ) ;
#37471 = CARTESIAN_POINT ( 'NONE',  ( 5.082755093536324154, -16.34375000204838813, 5.082755093536326818 ) ) ;
#37472 = AXIS2_PLACEMENT_3D ( 'NONE', #11590, #66792, #78463 ) ;
#37473 = CARTESIAN_POINT ( 'NONE',  ( -81.37675186042847031, -57.51598868027654987, 200.0426579070166895 ) ) ;
#37474 = ORIENTED_EDGE ( 'NONE', *, *, #54002, .T. ) ;
#37475 =( NAMED_UNIT ( * ) SI_UNIT ( $, .STERADIAN. ) SOLID_ANGLE_UNIT ( ) );
#37476 = DIRECTION ( 'NONE',  ( 1.000000000000000000, 1.224606353822377258E-16, 0.000000000000000000 ) ) ;
#37477 = CARTESIAN_POINT ( 'NONE',  ( 6.907083959255991168, 41.55068448857264229, -58.85924345847777062 ) ) ;
#37478 = CARTESIAN_POINT ( 'NONE',  ( 49.19536753089936099, 12.91488588853587061, -16.05939653828881220 ) ) ;
#37479 = CONICAL_SURFACE ( 'NONE', #39219, 7.000000000000000000, 0.9599310885968753704 ) ;
#37480 = CARTESIAN_POINT ( 'NONE',  ( -8.000000000000001776, -17.84375000409677270, 3.313708498984758943 ) ) ;
#37481 = CARTESIAN_POINT ( 'NONE',  ( -51.05793882480850243, -29.86182477906456256, 48.38375129339014791 ) ) ;
#37482 = DIRECTION ( 'NONE',  ( 0.000000000000000000, 0.000000000000000000, 1.000000000000000000 ) ) ;
#37483 = DIRECTION ( 'NONE',  ( 0.000000000000000000, -1.000000000000000000, 0.000000000000000000 ) ) ;
#37484 = CARTESIAN_POINT ( 'NONE',  ( 6.931554132376503752, -2.999999999999883649, -71.13906995425703883 ) ) ;
#37485 = CARTESIAN_POINT ( 'NONE',  ( 0.000000000000000000, 16.00000000000000000, 0.000000000000000000 ) ) ;
#37486 =( NAMED_UNIT ( * ) SI_UNIT ( $, .STERADIAN. ) SOLID_ANGLE_UNIT ( ) );
#37487 = CARTESIAN_POINT ( 'NONE',  ( 5.561881810733785514, -30.00000000000001421, -4.944729227524142345 ) ) ;
#37488 = VERTEX_POINT ( 'NONE', #101312 ) ;
#37489 = CARTESIAN_POINT ( 'NONE',  ( -1.000000000000000666, -50.00000000000000000, 44.97220075561143204 ) ) ;
#37490 = DIRECTION ( 'NONE',  ( 0.000000000000000000, -1.000000000000000000, 0.000000000000000000 ) ) ;
#37491 = AXIS2_PLACEMENT_3D ( 'NONE', #41252, #90338, #97894 ) ;
#37492 = CARTESIAN_POINT ( 'NONE',  ( -40.60713025163710910, 436.1947416310474068, 6.060763751012204992 ) ) ;
#37493 = CARTESIAN_POINT ( 'NONE',  ( -71.80342408229671491, -29.99999999999998579, -19.71767938363507255 ) ) ;
#37494 = CARTESIAN_POINT ( 'NONE',  ( -61.79326048008234551, -30.00000000000000711, 71.46593052723335404 ) ) ;
#37495 = DIRECTION ( 'NONE',  ( 0.000000000000000000, 0.000000000000000000, 1.000000000000000000 ) ) ;
#37496 = EDGE_CURVE ( 'NONE', #87130, #73965, #2593, .T. ) ;
#37497 = ORIENTED_EDGE ( 'NONE', *, *, #50118, .T. ) ;
#37498 = CARTESIAN_POINT ( 'NONE',  ( -26.10828281006072871, 37.18604047991734518, -8.034813406053556761 ) ) ;
#37499 = CARTESIAN_POINT ( 'NONE',  ( 76.92828183364126460, -57.52628917366442352, 194.9584416617772149 ) ) ;
#37500 = FACE_OUTER_BOUND ( 'NONE', #87098, .T. ) ;
#37501 = EDGE_CURVE ( 'NONE', #40136, #77127, #8073, .T. ) ;
#37502 = ADVANCED_FACE ( 'NONE', ( #41998, #74877, #93214, #33945, #100232 ), #68379, .T. ) ;
#37503 = CARTESIAN_POINT ( 'NONE',  ( -10.28624191511830155, 43.99263840937192782, -12.90779740156156841 ) ) ;
#37504 = CARTESIAN_POINT ( 'NONE',  ( -14.66373388272641520, 22.41296547519206328, 3.537915336770097952 ) ) ;
#37505 = CARTESIAN_POINT ( 'NONE',  ( 6.936184427528457874, 1.053834543709838281E-15, 8.605212085995399107 ) ) ;
#37506 = CARTESIAN_POINT ( 'NONE',  ( -63.35497338199800055, -60.00000000000000000, 112.0391477965111022 ) ) ;
#37507 = AXIS2_PLACEMENT_3D ( 'NONE', #50435, #65040, #24088 ) ;
#37508 = CARTESIAN_POINT ( 'NONE',  ( -0.9108756637670308853, 6.979659189795754060, -6.219623095964492698 ) ) ;
#37509 = CARTESIAN_POINT ( 'NONE',  ( -13.00000000000003730, -10.00000000000000888, 0.000000000000000000 ) ) ;
#37510 = CARTESIAN_POINT ( 'NONE',  ( -64.32759900501736183, 49.99999999999999289, -11.06576400629343659 ) ) ;
#37511 = CARTESIAN_POINT ( 'NONE',  ( -85.78111746350951705, -35.63734805798310390, 184.6310799642125460 ) ) ;
#37512 = ORIENTED_EDGE ( 'NONE', *, *, #66692, .T. ) ;
#37513 = CARTESIAN_POINT ( 'NONE',  ( 34.02514208821929032, 329.8602221817346276, -3.866232146452765139 ) ) ;
#37514 = CARTESIAN_POINT ( 'NONE',  ( 4.938669310872844932E-05, -53.40265726396589940, 32.79009283693002175 ) ) ;
#37515 = CARTESIAN_POINT ( 'NONE',  ( -6.583805027033739599, 41.87230883119009661, -59.35876460053138715 ) ) ;
#37516 =( NAMED_UNIT ( * ) PLANE_ANGLE_UNIT ( ) SI_UNIT ( $, .RADIAN. ) );
#37517 = EDGE_CURVE ( 'NONE', #958, #5935, #55835, .T. ) ;
#37518 = DIRECTION ( 'NONE',  ( -1.000000000000000000, 0.000000000000000000, 0.000000000000000000 ) ) ;
#37519 = DIRECTION ( 'NONE',  ( -0.000000000000000000, 0.8660254037844387076, 0.5000000000000000000 ) ) ;
#37520 = DIRECTION ( 'NONE',  ( -0.5735764363510512664, 0.8191520442889881348, 1.003171929053520309E-16 ) ) ;
#37521 = ORIENTED_EDGE ( 'NONE', *, *, #101178, .F. ) ;
#37522 = AXIS2_PLACEMENT_3D ( 'NONE', #34603, #84182, #17333 ) ;
#37523 = CARTESIAN_POINT ( 'NONE',  ( 17.93387092058976151, 50.00000000000000711, 61.97722397227583713 ) ) ;
#37524 = CARTESIAN_POINT ( 'NONE',  ( 10.37426823381935570, 10.87037927388256087, 10.42851533226476235 ) ) ;
#37525 = ADVANCED_FACE ( 'NONE', ( #27993 ), #37676, .F. ) ;
#37526 =( LENGTH_UNIT ( ) NAMED_UNIT ( * ) SI_UNIT ( .MILLI., .METRE. ) );
#37527 = CARTESIAN_POINT ( 'NONE',  ( 8.718495747319281008, 53.90653400547435581, -1.531152949374520622 ) ) ;
#37528 = CARTESIAN_POINT ( 'NONE',  ( 86.99610535363679276, -14.21045842199441012, 24.11248255592787615 ) ) ;
#37529 = CARTESIAN_POINT ( 'NONE',  ( -77.74926328355248017, -60.31560680552357212, 154.2294776400503622 ) ) ;
#37530 = VERTEX_POINT ( 'NONE', #70538 ) ;
#37531 = CARTESIAN_POINT ( 'NONE',  ( -3.733787657005604999, 42.00000000000000000, -68.31039150692600970 ) ) ;
#37532 = VECTOR ( 'NONE', #26624, 1000.000000000000000 ) ;
#37533 = FILL_AREA_STYLE ('',( #19765 ) ) ;
#37534 = AXIS2_PLACEMENT_3D ( 'NONE', #12636, #38032, #45570 ) ;
#37535 = CARTESIAN_POINT ( 'NONE',  ( 61.31082008514584913, 50.00000000000000000, 14.70291697493483696 ) ) ;
#37536 = CARTESIAN_POINT ( 'NONE',  ( 44.33761176843466956, 336.2903648585140672, 0.003362554233744022205 ) ) ;
#37537 = FACE_OUTER_BOUND ( 'NONE', #731, .T. ) ;
#37538 = ORIENTED_EDGE ( 'NONE', *, *, #96907, .F. ) ;
#37539 = CARTESIAN_POINT ( 'NONE',  ( -6.953930663124324063, 304.7325910270068334, -10.02533923955978779 ) ) ;
#37540 = DIRECTION ( 'NONE',  ( 0.1659550938519105956, -0.9861333108787085910, -0.000000000000000000 ) ) ;
#37541 = CARTESIAN_POINT ( 'NONE',  ( -7.188101187500001821, -27.50000000204838813, -2.977408999572651371 ) ) ;
#37542 = ORIENTED_EDGE ( 'NONE', *, *, #62779, .F. ) ;
#37543 = DIRECTION ( 'NONE',  ( -1.000000000000000000, -1.224606353822377258E-16, -0.000000000000000000 ) ) ;
#37544 = DIRECTION ( 'NONE',  ( -1.000000000000000000, -1.224606353822377258E-16, -0.000000000000000000 ) ) ;
#37545 = CARTESIAN_POINT ( 'NONE',  ( 5.652564027754396925, 41.79847498694749675, -70.46163205703543042 ) ) ;
#37546 = CARTESIAN_POINT ( 'NONE',  ( -17.03955750629483745, 45.47802236175360235, -6.596165372994933662 ) ) ;
#37547 = DIRECTION ( 'NONE',  ( 0.5735764363510466035, -0.8191520442889914655, 1.003171929053524500E-16 ) ) ;
#37548 = VECTOR ( 'NONE', #104700, 1000.000000000000000 ) ;
#37549 = CARTESIAN_POINT ( 'NONE',  ( -34.38981283644526599, 463.7396323591523242, 19.22682496774974226 ) ) ;
#37550 = ORIENTED_EDGE ( 'NONE', *, *, #67786, .T. ) ;
#37551 = CARTESIAN_POINT ( 'NONE',  ( 92.72480697121025628, -60.00000000000000000, -5.027149249431430711 ) ) ;
#37553 = CARTESIAN_POINT ( 'NONE',  ( 27.79149109135314788, -36.00466587923170181, 31.83270667620929828 ) ) ;
#37552 = CARTESIAN_POINT ( 'NONE',  ( -54.44990204170284898, -30.00000000000008882, 75.82925260777241760 ) ) ;
#37554 = CARTESIAN_POINT ( 'NONE',  ( 66.76860190796567451, 46.03420836107012093, 33.38430095398285857 ) ) ;
#37555 = ORIENTED_EDGE ( 'NONE', *, *, #166, .T. ) ;
#37556 = VECTOR ( 'NONE', #26027, 1000.000000000000000 ) ;
#37557 = UNCERTAINTY_MEASURE_WITH_UNIT (LENGTH_MEASURE( 1.000000000000000082E-05 ), #24732, 'distance_accuracy_value', 'NONE');
#37558 = B_SPLINE_CURVE_WITH_KNOTS ( 'NONE', 3,
 ( #100428, #77762, #3875, #43790, #21677, #62133, #63175, #22734, #5971, #38902, #80391, #6500, #55573, #95023, #22200, #86928, #20645, #96069, #30287, #5461, #62647, #4397, #13535, #70195, #21160, #95531, #55051, #38384, #103103, #71245, #70727, #53987, #14586, #29252, #78804, #45403, #72312, #103621, #54511, #87981, #29769, #46966, #104143, #87455, #14061, #30829, #46452, #79864 ),
 .UNSPECIFIED., .F., .F.,
 ( 4, 2, 2, 2, 2, 2, 2, 2, 2, 2, 2, 2, 2, 2, 2, 2, 2, 2, 2, 2, 2, 2, 2, 4 ),
 ( -6.000000001300036219E-08, 0.001124634766771550340, 0.002249329533543113768, 0.003374024300314676979, 0.004498719067086241058, 0.006748108600629357939, 0.007872803367400916380, 0.008997498134172474821, 0.01124688766771547895, 0.01349627720125848480, 0.01799505626834449479, 0.02024444580188758044, 0.02249383533543066610, 0.02699261440251668129, 0.03149139346960269648, 0.03599017253668870819, 0.04498773067086057204, 0.05398528880503244282, 0.07198040507337616356, 0.08097796320754802046, 0.08997552134171989124, 0.1079706376100636189, 0.1259657538784073327, 0.1439608701467510743 ),
 .UNSPECIFIED. ) ;
#37559 = ORIENTED_EDGE ( 'NONE', *, *, #7213, .T. ) ;
#37560 = SURFACE_STYLE_USAGE ( .BOTH. , #46665 ) ;
#37561 = CARTESIAN_POINT ( 'NONE',  ( 13.99999999999998401, 59.99999999999999289, -6.999999999999989342 ) ) ;
#37562 = DIRECTION ( 'NONE',  ( 0.000000000000000000, -1.000000000000000000, 0.000000000000000000 ) ) ;
#37563 = CARTESIAN_POINT ( 'NONE',  ( 0.000000000000000000, -30.00000000000000000, 0.000000000000000000 ) ) ;
#37564 = DIRECTION ( 'NONE',  ( 0.000000000000000000, 0.000000000000000000, -1.000000000000000000 ) ) ;
#37565 = CARTESIAN_POINT ( 'NONE',  ( 0.4037800551813762184, -7.199367570657610571, -0.5303295852573148839 ) ) ;
#37567 = ORIENTED_EDGE ( 'NONE', *, *, #80933, .T. ) ;
#37566 = TOROIDAL_SURFACE ( 'NONE', #78847, 66.00000000000000000, 0.5000000000000000000 ) ;
#37568 = B_SPLINE_CURVE_WITH_KNOTS ( 'NONE', 3,
 ( #10835, #93911, #100926, #61024, #18998, #20614, #68587, #68032, #101470, #44844, #93388, #92293, #52916, #27622, #51302, #84223 ),
 .UNSPECIFIED., .F., .F.,
 ( 4, 2, 2, 2, 2, 2, 2, 4 ),
 ( 0.000000000000000000, 0.002625638288314691149, 0.003938457432472034989, 0.004594867004550707776, 0.005251276576629379696, 0.006564095720786724403, 0.007876914864944068242, 0.01050255315325875766 ),
 .UNSPECIFIED. ) ;
#37569 = CARTESIAN_POINT ( 'NONE',  ( 17.50000000000002487, 48.00000000000000000, 62.61746187599675295 ) ) ;
#37570 = CARTESIAN_POINT ( 'NONE',  ( 100.7707649814656747, -30.00000000000000355, 180.9804943645408457 ) ) ;
#37571 = CARTESIAN_POINT ( 'NONE',  ( -11.38602198108772434, 20.27704874433871396, -8.239207418153725371 ) ) ;
#37572 = CARTESIAN_POINT ( 'NONE',  ( -29.68315524076956891, -1.200000000000000030E-05, 42.10535821593508388 ) ) ;
#37573 = CIRCLE ( 'NONE', #1307, 15.43455230191221261 ) ;
#37574 = CARTESIAN_POINT ( 'NONE',  ( 80.77803734578861850, -30.00000000000000000, -12.46495713760978852 ) ) ;
#37575 = FACE_OUTER_BOUND ( 'NONE', #46509, .T. ) ;
#37576 = ORIENTED_EDGE ( 'NONE', *, *, #64149, .F. ) ;
#37577 = EDGE_CURVE ( 'NONE', #88824, #48298, #50677, .T. ) ;
#37578 = ORIENTED_EDGE ( 'NONE', *, *, #55874, .F. ) ;
#37579 = CIRCLE ( 'NONE', #6551, 4.172000000000001485 ) ;
#37580 = ORIENTED_EDGE ( 'NONE', *, *, #7852, .T. ) ;
#37581 = CARTESIAN_POINT ( 'NONE',  ( 96.28888888888889142, -4.171999999999998820, 0.000000000000000000 ) ) ;
#37582 = CARTESIAN_POINT ( 'NONE',  ( 9.797174393178809880E-16, 274.9999999999999432, 7.999999999999986677 ) ) ;
#37583 = CARTESIAN_POINT ( 'NONE',  ( -36.95419080661243783, 25.70428587859928982, -13.30723349455869098 ) ) ;
#37584 = DIRECTION ( 'NONE',  ( -0.000000000000000000, 1.000000000000000000, 0.000000000000000000 ) ) ;
#37585 = CARTESIAN_POINT ( 'NONE',  ( -1.910791319121646126, -69.56563210985819978, 12.86688064138004961 ) ) ;
#37586 = EDGE_CURVE ( 'NONE', #72256, #89827, #78606, .T. ) ;
#37587 = CARTESIAN_POINT ( 'NONE',  ( 5.454472066463755375, 54.16644935941751271, 6.039397278010941505 ) ) ;
#37588 = AXIS2_PLACEMENT_3D ( 'NONE', #66833, #25893, #25335 ) ;
#37589 = ORIENTED_EDGE ( 'NONE', *, *, #60688, .F. ) ;
#37590 = CARTESIAN_POINT ( 'NONE',  ( -29.68315524077004497, 8.302504244945346557, -42.10535821593474282 ) ) ;
#37591 = VERTEX_POINT ( 'NONE', #61394 ) ;
#37592 = CARTESIAN_POINT ( 'NONE',  ( -1.749814335632529083, 15.56087475005694643, -9.852235012526419311 ) ) ;
#37593 = CARTESIAN_POINT ( 'NONE',  ( 60.52345103412395844, -38.34237732095000695, 98.06192674467523318 ) ) ;
#37594 = CARTESIAN_POINT ( 'NONE',  ( 3.313708498984761608, -10.90625000409677092, -8.000000000000000000 ) ) ;
#37595 = CARTESIAN_POINT ( 'NONE',  ( 24.83179908432460081, 295.6082205264385721, 2.099364176556762995 ) ) ;
#37596 = CARTESIAN_POINT ( 'NONE',  ( 8.844474929605143032, 302.6213362138051934, -10.03676381922342564 ) ) ;
#37597 = CARTESIAN_POINT ( 'NONE',  ( 64.00467378430177234, -29.05420584686936891, 77.96572560711764766 ) ) ;
#37598 = CIRCLE ( 'NONE', #97813, 7.999999999999989342 ) ;
#37599 = ORIENTED_EDGE ( 'NONE', *, *, #55028, .F. ) ;
#37600 = EDGE_CURVE ( 'NONE', #87833, #43519, #49406, .T. ) ;
#37601 = CARTESIAN_POINT ( 'NONE',  ( 17.61650669486618881, 1.474610560812782335E-15, 0.000000000000000000 ) ) ;
#37602 = CARTESIAN_POINT ( 'NONE',  ( -46.42533371640924855, -34.72140787405426465, -36.69163149917219613 ) ) ;
#37603 = CARTESIAN_POINT ( 'NONE',  ( -38.38188837495462735, 437.9257690784074839, 4.300778830038868961 ) ) ;
#37604 = CARTESIAN_POINT ( 'NONE',  ( -9.169258015245434379, 51.60721829683665618, 1.678621333424785700 ) ) ;
#37605 = ORIENTED_EDGE ( 'NONE', *, *, #31670, .T. ) ;
#37606 = CARTESIAN_POINT ( 'NONE',  ( 7.150053860865852151, 28.21734546086023343, 3.590189269391290239 ) ) ;
#37607 = LINE ( 'NONE', #45146, #5728 ) ;
#37608 = CARTESIAN_POINT ( 'NONE',  ( 43.64531880380447149, 464.9151967207193366, 12.30391130301436142 ) ) ;
#37609 = AXIS2_PLACEMENT_3D ( 'NONE', #16657, #42521, #91624 ) ;
#37610 = AXIS2_PLACEMENT_3D ( 'NONE', #83256, #91884, #92945 ) ;
#37611 = VECTOR ( 'NONE', #102754, 1000.000000000000000 ) ;
#37612 = CARTESIAN_POINT ( 'NONE',  ( -18.00000000000001421, -20.00000000000001776, 9.000000000000008882 ) ) ;
#37613 = CARTESIAN_POINT ( 'NONE',  ( 9.607612890400023531, 15.83452282593334637, 2.797297131808757165 ) ) ;
#37614 = VECTOR ( 'NONE', #52511, 999.9999999999998863 ) ;
#37615 = CARTESIAN_POINT ( 'NONE',  ( 85.27851683770271052, -57.46677582188632272, 192.4431409699905089 ) ) ;
#37616 = B_SPLINE_CURVE_WITH_KNOTS ( 'NONE', 3,
 ( #34175, #67053, #64921, #40634, #7204, #32040, #99930, #26105, #58962, #81091, #106420, #40112, #72988, #105894, #48713, #81601, #7728, #73519, #20132, #68658, #68097, #17973 ),
 .UNSPECIFIED., .F., .F.,
 ( 4, 2, 2, 2, 2, 2, 2, 2, 2, 2, 4 ),
 ( 0.007323666553981427081, 0.007826507932084076496, 0.008329349310186726779, 0.008580769999238053655, 0.008832190688289378797, 0.009335032066392032549, 0.009586452755443361159, 0.009837873444494689770, 0.01034071482259735220, 0.01084355620070001636, 0.01134639757880268052 ),
 .UNSPECIFIED. ) ;
#37617 = CARTESIAN_POINT ( 'NONE',  ( 23.86650669486618881, 1.474610560812782335E-15, 0.000000000000000000 ) ) ;
#37618 = CARTESIAN_POINT ( 'NONE',  ( -5.452425833994689164, 5.376849860293315686, 5.000000000000000000 ) ) ;
#37619 = CARTESIAN_POINT ( 'NONE',  ( 7.800703710507055355, -6.414043073420603314, 1.791736796405271281 ) ) ;
#37620 = CARTESIAN_POINT ( 'NONE',  ( -43.03265099499981972, 484.2747968070553952, -0.8099405866661884001 ) ) ;
#37621 = CARTESIAN_POINT ( 'NONE',  ( 13.93078765908243710, -50.20613146654194736, 28.41172023899451560 ) ) ;
#37622 = CARTESIAN_POINT ( 'NONE',  ( 34.99225395455989940, 435.2420463162160900, 7.288472211092408060 ) ) ;
#37623 = CARTESIAN_POINT ( 'NONE',  ( -100.3777161340725712, -29.99999999999999289, 157.7761675202767151 ) ) ;
#37624 = EDGE_CURVE ( 'NONE', #7789, #11792, #21901, .T. ) ;
#37625 =( GEOMETRIC_REPRESENTATION_CONTEXT ( 3 ) GLOBAL_UNCERTAINTY_ASSIGNED_CONTEXT ( ( #65677 ) ) GLOBAL_UNIT_ASSIGNED_CONTEXT ( ( #83082, #101918, #91196 ) ) REPRESENTATION_CONTEXT ( 'NONE', 'WORKASPACE' ) );
#37626 = DIRECTION ( 'NONE',  ( 0.000000000000000000, 1.000000000000000000, 0.000000000000000000 ) ) ;
#37627 = CARTESIAN_POINT ( 'NONE',  ( 1.031133051057990135, -57.67120256293672043, 41.61115920477558916 ) ) ;
#37629 = FACE_BOUND ( 'NONE', #237, .T. ) ;
#37628 = CARTESIAN_POINT ( 'NONE',  ( -9.333079356992119102, 248.2216691992512381, 3.592383266237786366 ) ) ;
#37630 = EDGE_CURVE ( 'NONE', #69611, #75902, #71811, .T. ) ;
#37631 = MECHANICAL_DESIGN_GEOMETRIC_PRESENTATION_REPRESENTATION (  '', ( #44528 ), #53147 ) ;
#37632 = CARTESIAN_POINT ( 'NONE',  ( -40.54980470635882028, 41.80014700451209109, -54.75323515523022877 ) ) ;
#37633 = CARTESIAN_POINT ( 'NONE',  ( -17.92955758770686003, 50.00000000000000711, 61.98266528452947455 ) ) ;
#37634 = CARTESIAN_POINT ( 'NONE',  ( -9.090909090909089940, 15.00000000000000000, 4.165977904505306917 ) ) ;
#37635 = DIRECTION ( 'NONE',  ( -0.000000000000000000, -1.000000000000000000, -0.000000000000000000 ) ) ;
#37636 = CARTESIAN_POINT ( 'NONE',  ( 0.9330442100808740147, -70.05675763226145136, 13.03100537459354413 ) ) ;
#37637 = CIRCLE ( 'NONE', #78934, 5.000000000000010658 ) ;
#37638 = FACE_OUTER_BOUND ( 'NONE', #5043, .T. ) ;
#37639 = CARTESIAN_POINT ( 'NONE',  ( 0.000000000000000000, -14.49999999999999822, 0.000000000000000000 ) ) ;
#37640 = ORIENTED_EDGE ( 'NONE', *, *, #50996, .F. ) ;
#37641 = CARTESIAN_POINT ( 'NONE',  ( 5.744562646538028616, 12.99999999999999289, 4.000000000000000000 ) ) ;
#37642 = CARTESIAN_POINT ( 'NONE',  ( -2.106572258996926905, -49.79055979746641469, 102.5319188847123542 ) ) ;
#37643 = CARTESIAN_POINT ( 'NONE',  ( -15.54353313750226206, -32.51340815750653945, 29.48048180118074413 ) ) ;
#37644 =( BOUNDED_SURFACE ( )  B_SPLINE_SURFACE ( 3, 2, ( 
 ( #77393, #77926, #100593 ),
 ( #36967, #26752, #102733 ),
 ( #60696, #28892, #20807 ),
 ( #11041, #35914, #12635 ),
 ( #68786, #101667, #92499 ),
 ( #75791, #59629, #68239 ),
 ( #56265, #46092, #87617 ),
 ( #88668, #63349, #104854 ),
 ( #47659, #95700, #55220 ),
 ( #80555, #96249, #6140 ),
 ( #72476, #30455, #71407 ),
 ( #47132, #38542, #104305 ),
 ( #21312, #29924, #78977 ),
 ( #13701, #39603, #54149 ),
 ( #46612, #89202, #80027 ),
 ( #79509, #70891, #37504 ),
 ( #22375, #39069, #88146 ),
 ( #71950, #87089, #105382 ),
 ( #5619, #30997, #62290 ),
 ( #31521, #14226, #95180 ) ),
 .UNSPECIFIED., .F., .F., .T. ) 
 B_SPLINE_SURFACE_WITH_KNOTS ( ( 4, 2, 2, 2, 2, 2, 2, 2, 2, 4 ),
 ( 3, 3 ),
 ( 3.184952301893417825E-15, 0.001208125624086961360, 0.002416251248170737768, 0.003624376872254514177, 0.004832502496338290585, 0.005436565308380179005, 0.006040628120422067426, 0.007248753744505843401, 0.008456879368589619375, 0.009665004992673396217 ),
 ( 0.000000000000000000, 1.000000000000000000 ),
 .UNSPECIFIED. ) 
 GEOMETRIC_REPRESENTATION_ITEM ( )  RATIONAL_B_SPLINE_SURFACE ( (
 ( 1.000000000000000000, 0.8291561975880743507, 1.000000000000000000),
 ( 1.000000000000000000, 0.8411444448774373361, 1.000000000000000000),
 ( 1.000000000000000000, 0.8513107778592109431, 1.000000000000000000),
 ( 1.000000000000000000, 0.8686991428040923280, 1.000000000000000000),
 ( 1.000000000000000000, 0.8759367825447341716, 1.000000000000000000),
 ( 1.000000000000000000, 0.8878384569986785824, 1.000000000000000000),
 ( 1.000000000000000000, 0.8925163270234079960, 1.000000000000000000),
 ( 1.000000000000000000, 0.8988019894165557577, 1.000000000000000000),
 ( 1.000000000000000000, 0.9004488336118289249, 1.000000000000000000),
 ( 1.000000000000000000, 0.9004787869545520795, 1.000000000000000000),
 ( 1.000000000000000000, 0.9000741598243899855, 1.000000000000000000),
 ( 1.000000000000000000, 0.8984769429442731603, 1.000000000000000000),
 ( 1.000000000000000000, 0.8972871579692907051, 1.000000000000000000),
 ( 1.000000000000000000, 0.8926126616870123653, 1.000000000000000000),
 ( 1.000000000000000000, 0.8880148073974446499, 1.000000000000000000),
 ( 1.000000000000000000, 0.8760712452968238972, 1.000000000000000000),
 ( 1.000000000000000000, 0.8688049777777138161, 1.000000000000000000),
 ( 1.000000000000000000, 0.8513604698959409411, 1.000000000000000000),
 ( 1.000000000000000000, 0.8411660073561874063, 1.000000000000000000),
 ( 1.000000000000000000, 0.8291561975891263980, 1.000000000000000000) ) ) 
 REPRESENTATION_ITEM ( '' )  SURFACE ( )  );
#37646 = DIRECTION ( 'NONE',  ( 0.000000000000000000, 0.000000000000000000, -1.000000000000000000 ) ) ;
#37645 = CARTESIAN_POINT ( 'NONE',  ( -85.70835096055856184, -60.00000000000002132, -14.66632915116390734 ) ) ;
#37647 = ORIENTED_EDGE ( 'NONE', *, *, #60166, .F. ) ;
#37648 = EDGE_CURVE ( 'NONE', #9279, #78066, #5272, .T. ) ;
#37649 = AXIS2_PLACEMENT_3D ( 'NONE', #60439, #93315, #19471 ) ;
#37650 = CARTESIAN_POINT ( 'NONE',  ( -89.99999999999997158, -52.00000000000000000, 194.0238439516549818 ) ) ;
#37651 = DIRECTION ( 'NONE',  ( -1.000000000000000000, -1.224606353822377258E-16, -0.000000000000000000 ) ) ;
#37652 = CIRCLE ( 'NONE', #82412, 5.000000000000000000 ) ;
#37653 = CARTESIAN_POINT ( 'NONE',  ( 15.86714682456667092, 3.932109987699209164, -3.945841262946509609 ) ) ;
#37654 = CARTESIAN_POINT ( 'NONE',  ( -35.96492786661492858, 302.4488314805894902, -8.278427239162008178 ) ) ;
#37655 = ORIENTED_EDGE ( 'NONE', *, *, #40858, .T. ) ;
#37656 = DIRECTION ( 'NONE',  ( 0.000000000000000000, 0.000000000000000000, 1.000000000000000000 ) ) ;
#37657 = DIRECTION ( 'NONE',  ( -1.000000000000000000, 0.000000000000000000, 0.000000000000000000 ) ) ;
#37659 = CARTESIAN_POINT ( 'NONE',  ( 0.000000000000000000, 0.000000000000000000, 15.00000000000000000 ) ) ;
#37658 = CARTESIAN_POINT ( 'NONE',  ( -13.50000000000000000, 5.257130651325558013, -0.5389759092231611870 ) ) ;
#37660 = EDGE_CURVE ( 'NONE', #64333, #1743, #72116, .T. ) ;
#37661 = CIRCLE ( 'NONE', #41006, 3.309500000000007880 ) ;
#37662 = ORIENTED_EDGE ( 'NONE', *, *, #66628, .T. ) ;
#37663 = ORIENTED_EDGE ( 'NONE', *, *, #96954, .F. ) ;
#37664 = ORIENTED_EDGE ( 'NONE', *, *, #3776, .F. ) ;
#37665 = CARTESIAN_POINT ( 'NONE',  ( 58.92761780597729881, 6.856755485862130937E-15, 0.000000000000000000 ) ) ;
#37666 = CARTESIAN_POINT ( 'NONE',  ( 7.500000000000007105, 40.00000000000069633, -70.73267643392320281 ) ) ;
#37667 = CARTESIAN_POINT ( 'NONE',  ( 44.83349330513380693, 1.593028355512270567E-15, 0.000000000000000000 ) ) ;
#37668 = ORIENTED_EDGE ( 'NONE', *, *, #19932, .F. ) ;
#37669 = B_SPLINE_CURVE_WITH_KNOTS ( 'NONE', 3,
 ( #76127, #93918, #77740, #51850, #43763, #11921, #85847, #18455, #52379 ),
 .UNSPECIFIED., .F., .F.,
 ( 4, 2, 1, 2, 4 ),
 ( 0.000000000000000000, 0.002165063509461097498, 0.004330127018922194995, 0.006495190528383292493, 0.008660254037844389990 ),
 .UNSPECIFIED. ) ;
#37670 = SURFACE_STYLE_FILL_AREA ( #96407 ) ;
#37671 = CARTESIAN_POINT ( 'NONE',  ( -6.804095716565868202, 41.75280174922988152, -69.96721254779907895 ) ) ;
#37672 = CARTESIAN_POINT ( 'NONE',  ( -87.54930676208033447, -60.00000000002437872, -25.45872903247207475 ) ) ;
#37673 = CARTESIAN_POINT ( 'NONE',  ( -20.37278541768183615, 303.8378246129572631, -10.00297115033342266 ) ) ;
#37674 = CIRCLE ( 'NONE', #51391, 3.400000000000000355 ) ;
#37675 = CARTESIAN_POINT ( 'NONE',  ( 37.31558637970096015, -60.00000000000000000, 48.70948680922666085 ) ) ;
#37676 = CYLINDRICAL_SURFACE ( 'NONE', #23658, 4.000000000000000000 ) ;
#37677 = CARTESIAN_POINT ( 'NONE',  ( -5.902962327514317487, 41.87327319969161010, -59.02279321040224147 ) ) ;
#37678 = CIRCLE ( 'NONE', #35993, 15.00000000000000000 ) ;
#37680 = CARTESIAN_POINT ( 'NONE',  ( 11.16551004579882189, -25.54854244899442506, 28.17187544474615635 ) ) ;
#37679 = CARTESIAN_POINT ( 'NONE',  ( -101.2960459709432826, -29.99999999999998579, 104.2733491104911963 ) ) ;
#37681 = AXIS2_PLACEMENT_3D ( 'NONE', #69651, #94467, #14567 ) ;
#37682 =( NAMED_UNIT ( * ) PLANE_ANGLE_UNIT ( ) SI_UNIT ( $, .RADIAN. ) );
#37683 = CARTESIAN_POINT ( 'NONE',  ( -47.68213074599328394, -42.98560256933807722, 48.22320990812892205 ) ) ;
#37684 = CARTESIAN_POINT ( 'NONE',  ( -3.465069528698219603, 19.86757101636677447, 6.084398292909884987 ) ) ;
#37685 = EDGE_LOOP ( 'NONE', ( #35880, #26888, #20901, #77031, #37647, #98021 ) ) ;
#37686 = CARTESIAN_POINT ( 'NONE',  ( 0.2952253681877878844, 13.62314717402266062, -49.28328918176131879 ) ) ;
#37687 = VECTOR ( 'NONE', #14188, 1000.000000000000000 ) ;
#37688 = DIRECTION ( 'NONE',  ( 0.000000000000000000, -1.000000000000000000, 0.000000000000000000 ) ) ;
#37689 = FACE_OUTER_BOUND ( 'NONE', #18846, .T. ) ;
#37690 = EDGE_LOOP ( 'NONE', ( #70194, #92761, #8550, #25656 ) ) ;
#37691 = FILL_AREA_STYLE ('',( #79160 ) ) ;
#37692 = ORIENTED_EDGE ( 'NONE', *, *, #36716, .F. ) ;
#37693 = CARTESIAN_POINT ( 'NONE',  ( 44.47534377888502632, -38.31160956920666649, 57.00192013341538910 ) ) ;
#37694 = CARTESIAN_POINT ( 'NONE',  ( 3.787335548944762209, -48.90784695950119243, 104.1352136098573453 ) ) ;
#37695 = CARTESIAN_POINT ( 'NONE',  ( 0.8750000000000016653, -70.58759490697437400, 13.02737050516260098 ) ) ;
#37696 = CARTESIAN_POINT ( 'NONE',  ( -15.50526908257195835, 42.00000000000000000, -57.69562748404377572 ) ) ;
#37697 = CARTESIAN_POINT ( 'NONE',  ( 98.09172150708243976, -29.99999999999999645, 190.4342177531940763 ) ) ;
#37698 = CARTESIAN_POINT ( 'NONE',  ( 0.1317522424472098164, 1.959574484719855292, 7.999999999999998224 ) ) ;
#37699 = VERTEX_POINT ( 'NONE', #7368 ) ;
#37700 = EDGE_CURVE ( 'NONE', #48471, #2695, #98276, .T. ) ;
#37701 = AXIS2_PLACEMENT_3D ( 'NONE', #34050, #51239, #10262 ) ;
#37702 = ORIENTED_EDGE ( 'NONE', *, *, #44672, .T. ) ;
#37703 = EDGE_LOOP ( 'NONE', ( #92981, #2728, #22262, #105576, #40663 ) ) ;
#37704 = CARTESIAN_POINT ( 'NONE',  ( 54.02217166477871757, -36.03114398899570858, 56.87927286532268312 ) ) ;
#37705 = CARTESIAN_POINT ( 'NONE',  ( 0.9654893961777153422, -30.00000000000000355, 7.122964895856731538 ) ) ;
#37706 = FACE_OUTER_BOUND ( 'NONE', #3002, .T. ) ;
#37707 = ADVANCED_FACE ( 'NONE', ( #48361 ), #23597, .F. ) ;
#37709 = ORIENTED_EDGE ( 'NONE', *, *, #86157, .T. ) ;
#37708 = CIRCLE ( 'NONE', #67158, 5.000000000000010658 ) ;
#37711 = EDGE_CURVE ( 'NONE', #85984, #75882, #1250, .T. ) ;
#37710 = CARTESIAN_POINT ( 'NONE',  ( -16.03934073995868204, 4.450581328283826466, 3.145353196842342935 ) ) ;
#37712 = VERTEX_POINT ( 'NONE', #39768 ) ;
#37713 = CARTESIAN_POINT ( 'NONE',  ( 5.908054807098742893E-16, -0.6346842323187772417, -6.500000000000000000 ) ) ;
#37714 = CARTESIAN_POINT ( 'NONE',  ( 102.1500853529942106, -38.44127923276875691, 199.6050571543175067 ) ) ;
#37715 = CARTESIAN_POINT ( 'NONE',  ( 10.07739987653159908, 15.02570658418118121, 10.37755588292369247 ) ) ;
#37716 = CARTESIAN_POINT ( 'NONE',  ( 86.46873085151457872, -60.13455952585971431, 2.723771532636757531 ) ) ;
#37717 = DIRECTION ( 'NONE',  ( 0.000000000000000000, 0.000000000000000000, -1.000000000000000000 ) ) ;
#37718 = CARTESIAN_POINT ( 'NONE',  ( -42.88690404150482038, 465.8389234274137607, 12.02232841050726897 ) ) ;
#37719 = B_SPLINE_CURVE_WITH_KNOTS ( 'NONE', 3,
 ( #63920, #14804, #48751, #73026, #98897, #183, #23470, #25058, #32082, #73562, #66017, #106464, #33149, #55776, #96808, #105936, #88712, #24008, #56852, #47698, #15877, #97318, #64957, #80598, #16951, #7240, #57381, #90294, #57912, #7771, #89774, #6720, #16404, #32622 ),
 .UNSPECIFIED., .F., .F.,
 ( 4, 2, 2, 2, 2, 2, 2, 2, 2, 2, 2, 2, 2, 2, 2, 2, 4 ),
 ( 1.409296014025916843E-17, 0.0007899309203816181355, 0.001579861840763222176, 0.002369792761144825892, 0.003159723681526430041, 0.003949654601908034190, 0.004739585522289637906, 0.005529516442671242489, 0.006319447363052846205, 0.007109378283434449920, 0.007899309203816054503, 0.008689240124197658219, 0.009479171044579261934, 0.01026910196496086565, 0.01105903288534247110, 0.01184896380572407482, 0.01263889472610567853 ),
 .UNSPECIFIED. ) ;
#37720 = DIRECTION ( 'NONE',  ( -0.000000000000000000, 1.000000000000000000, -0.000000000000000000 ) ) ;
#37721 = EDGE_CURVE ( 'NONE', #99675, #88535, #88836, .T. ) ;
#37722 = CARTESIAN_POINT ( 'NONE',  ( 9.518114778805811582, 142.5485589762550092, 5.000000000000000888 ) ) ;
#37723 = ORIENTED_EDGE ( 'NONE', *, *, #24505, .F. ) ;
#37724 =( NAMED_UNIT ( * ) SI_UNIT ( $, .STERADIAN. ) SOLID_ANGLE_UNIT ( ) );
#37725 = CARTESIAN_POINT ( 'NONE',  ( -38.26552733536168915, 461.1050587587353107, 2.389481650175799832 ) ) ;
#37726 = DIRECTION ( 'NONE',  ( -1.224646799147353207E-16, 1.000000000000000000, 0.000000000000000000 ) ) ;
#37727 = B_SPLINE_CURVE_WITH_KNOTS ( 'NONE', 3,
 ( #48587, #11, #95191, #39990, #86582, #106288, #16227, #81475, #5110, #65849 ),
 .UNSPECIFIED., .F., .F.,
 ( 4, 2, 2, 2, 4 ),
 ( 5.679895013065603427E-17, 0.002488089381717967750, 0.003110111727147444292, 0.003732134072576921702, 0.004976178763435875653 ),
 .UNSPECIFIED. ) ;
#37728 = EDGE_LOOP ( 'NONE', ( #9460, #36932, #10289 ) ) ;
#37729 = CYLINDRICAL_SURFACE ( 'NONE', #71670, 15.00000000000000000 ) ;
#37730 = STYLED_ITEM ( 'NONE', ( #17938 ), #76671 ) ;
#37731 = CARTESIAN_POINT ( 'NONE',  ( -38.19214260828640306, 317.3320220044833491, 15.41122486417729931 ) ) ;
#37732 = CARTESIAN_POINT ( 'NONE',  ( -11.60474022310126152, -4.919048487763364008, -76.97896355671299773 ) ) ;
#37733 = CARTESIAN_POINT ( 'NONE',  ( 0.000000000000000000, -4.000000000000003553, 27.00000000000000000 ) ) ;
#37734 = CARTESIAN_POINT ( 'NONE',  ( 3.313708498984762496, -18.78124999999998934, 7.999999999999998224 ) ) ;
#37735 = CARTESIAN_POINT ( 'NONE',  ( 53.08934989192470510, -29.99999999999999289, 52.21148837440654944 ) ) ;
#37736 = DIRECTION ( 'NONE',  ( 0.000000000000000000, 1.000000000000000000, 0.000000000000000000 ) ) ;
#37737 = ORIENTED_EDGE ( 'NONE', *, *, #29916, .T. ) ;
#37738 = CARTESIAN_POINT ( 'NONE',  ( 85.27564894550540942, -32.22278697073298304, 179.6136003457102106 ) ) ;
#37739 = CARTESIAN_POINT ( 'NONE',  ( -49.13349184603291775, 7.785586125543571434, 16.19411946323684859 ) ) ;
#37740 = AXIS2_PLACEMENT_3D ( 'NONE', #53632, #86566, #37495 ) ;
#37741 = ORIENTED_EDGE ( 'NONE', *, *, #27122, .F. ) ;
#37742 = CARTESIAN_POINT ( 'NONE',  ( -100.8220720648846225, -60.15490406098927423, 120.1837212289833019 ) ) ;
#37743 = DIRECTION ( 'NONE',  ( 0.000000000000000000, 0.000000000000000000, 1.000000000000000000 ) ) ;
#37744 = CARTESIAN_POINT ( 'NONE',  ( -8.572890873561306080, -5.000000000000002665, -75.22730630429823862 ) ) ;
#37745 = CARTESIAN_POINT ( 'NONE',  ( 8.480908980104139516, -4.333298119783806968, 15.78559285094131148 ) ) ;
#37746 = CARTESIAN_POINT ( 'NONE',  ( -5.687071598576536324, -21.74269005626036844, -38.54672360651682084 ) ) ;
#37747 =( NAMED_UNIT ( * ) SI_UNIT ( $, .STERADIAN. ) SOLID_ANGLE_UNIT ( ) );
#37748 = CARTESIAN_POINT ( 'NONE',  ( 12.43567954112019969, -21.33041175957170310, 35.61117015663748475 ) ) ;
#37749 = CARTESIAN_POINT ( 'NONE',  ( 1.910332202385262690, -0.1361670080387644977, 102.2504571675851963 ) ) ;
#37750 = CARTESIAN_POINT ( 'NONE',  ( 39.77890293349060613, -26.23074748553104385, 35.82129514820142191 ) ) ;
#37751 = AXIS2_PLACEMENT_3D ( 'NONE', #60272, #25801, #52136 ) ;
#37753 = CARTESIAN_POINT ( 'NONE',  ( -10.60777364585932681, 14.22653809302268080, 9.944243933998073715 ) ) ;
#37752 = CARTESIAN_POINT ( 'NONE',  ( 42.61862771095000824, 462.7773917227530092, 13.89716710540371736 ) ) ;
#37754 = EDGE_CURVE ( 'NONE', #24908, #3711, #71573, .T. ) ;
#37755 = CARTESIAN_POINT ( 'NONE',  ( 42.01176354208753594, 328.3689192229740001, 6.166223753866878710 ) ) ;
#37756 = CARTESIAN_POINT ( 'NONE',  ( 2.602085213965210642E-15, 15.58845726811991561, -11.79422863405993382 ) ) ;
#37757 = CARTESIAN_POINT ( 'NONE',  ( -83.17009416728905080, -38.00000000000003553, -3.028942620234869931 ) ) ;
#37758 = B_SPLINE_CURVE_WITH_KNOTS ( 'NONE', 3,
 ( #79957, #62229, #103714, #47057, #56190, #55145, #104775, #103193, #39529, #21245, #23351, #89128, #22829, #15229, #47586, #54604, #48115, #29860, #38993, #55661, #71870, #87545, #71339, #80482, #46542, #72406, #79435, #81014, #63271, #21768, #88075, #105310, #63804, #54080, #37429, #14153, #46020, #87021, #37961 ),
 .UNSPECIFIED., .F., .F.,
 ( 4, 1, 1, 1, 2, 2, 1, 1, 1, 1, 1, 2, 2, 1, 1, 1, 1, 1, 2, 2, 1, 1, 1, 1, 1, 1, 2, 2, 4 ),
 ( 0.000000000000000000, 0.06250000000000072164, 0.09375000000000111022, 0.1093750000000013323, 0.1171875000000015682, 0.1250000000000017764, 0.1875000000000041633, 0.2187500000000052180, 0.2343750000000056621, 0.2421875000000059674, 0.2460937500000059674, 0.2480468750000058564, 0.2500000000000057176, 0.3750000000000043854, 0.4375000000000034972, 0.4687500000000037748, 0.4843750000000037748, 0.4921875000000037192, 0.4960937500000044409, 0.5000000000000051070, 0.6250000000000281997, 0.6875000000000405231, 0.7187500000000471845, 0.7343750000000498490, 0.7421875000000507372, 0.7460937500000517364, 0.7480468750000521805, 0.7500000000000526246, 1.000000000000000000 ),
 .UNSPECIFIED. ) ;
#37759 = VERTEX_POINT ( 'NONE', #75159 ) ;
#37760 = CARTESIAN_POINT ( 'NONE',  ( -12.16150765691225999, -2.480561230130143624, 20.68473351390147386 ) ) ;
#37761 = SURFACE_STYLE_USAGE ( .BOTH. , #38282 ) ;
#37762 = CARTESIAN_POINT ( 'NONE',  ( 38.54515645702225868, 5.000000000000002665, 0.000000000000000000 ) ) ;
#37763 = ADVANCED_FACE ( 'NONE', ( #6844 ), #2915, .T. ) ;
#37764 = CARTESIAN_POINT ( 'NONE',  ( -6.281393465144616606, -34.58963968333188888, -32.56267242852022292 ) ) ;
#37765 = ORIENTED_EDGE ( 'NONE', *, *, #4284, .F. ) ;
#37766 = CONICAL_SURFACE ( 'NONE', #5019, 8.900000000000000355, 0.7853981633974418397 ) ;
#37767 = CYLINDRICAL_SURFACE ( 'NONE', #22100, 4.000000000000000000 ) ;
#37768 = CARTESIAN_POINT ( 'NONE',  ( 0.4033376246892518835, -4.059728990630813605, -5.968343123267134231 ) ) ;
#37769 = AXIS2_PLACEMENT_3D ( 'NONE', #4154, #85069, #102846 ) ;
#37770 = EDGE_LOOP ( 'NONE', ( #61180, #58634, #95445, #29448, #19726, #59060 ) ) ;
#37771 = AXIS2_PLACEMENT_3D ( 'NONE', #16843, #82632, #80487 ) ;
#37772 = DIRECTION ( 'NONE',  ( -1.000000000000000000, -0.000000000000000000, -0.000000000000000000 ) ) ;
#37773 = DIRECTION ( 'NONE',  ( 1.000000000000000000, 0.000000000000000000, -0.000000000000000000 ) ) ;
#37774 = CARTESIAN_POINT ( 'NONE',  ( -92.24153208330554321, -59.99999999999999289, 2.317352427123469560 ) ) ;
#37775 = EDGE_LOOP ( 'NONE', ( #65968, #1441, #104640, #96992, #51574, #14613 ) ) ;
#37776 = CARTESIAN_POINT ( 'NONE',  ( 8.162336134653109809, 41.33266196706049556, -58.07023218170494516 ) ) ;
#37777 = FACE_OUTER_BOUND ( 'NONE', #40657, .T. ) ;
#37778 = CARTESIAN_POINT ( 'NONE',  ( -9.253800200985683233, 28.69989668911828318, -3.791983798715485410 ) ) ;
#37779 = EDGE_CURVE ( 'NONE', #58408, #19689, #67092, .T. ) ;
#37781 = DIRECTION ( 'NONE',  ( 0.5735764363510468256, 0.8191520442889913545, 0.000000000000000000 ) ) ;
#37780 =( NAMED_UNIT ( * ) SI_UNIT ( $, .STERADIAN. ) SOLID_ANGLE_UNIT ( ) );
#37782 = ADVANCED_FACE ( 'NONE', ( #55386 ), #88316, .F. ) ;
#37783 = CARTESIAN_POINT ( 'NONE',  ( -83.70341740888480331, -32.52351292720956621, 165.3169881577036620 ) ) ;
#37784 = ORIENTED_EDGE ( 'NONE', *, *, #27851, .F. ) ;
#37785 = CARTESIAN_POINT ( 'NONE',  ( 2.083846472846741813E-15, -8.673617379884035472E-16, 17.01589776168603407 ) ) ;
#37786 = EDGE_LOOP ( 'NONE', ( #77873, #98403, #18681, #62074, #101212, #47815, #561 ) ) ;
#37787 = VERTEX_POINT ( 'NONE', #40280 ) ;
#37788 = CARTESIAN_POINT ( 'NONE',  ( -7.811152745362720751, -4.332661967060489339, -16.03212449091516945 ) ) ;
#37789 = DIRECTION ( 'NONE',  ( -1.000000000000000000, -1.224606353822377258E-16, -0.000000000000000000 ) ) ;
#37790 = SURFACE_STYLE_USAGE ( .BOTH. , #53411 ) ;
#37791 = ORIENTED_EDGE ( 'NONE', *, *, #92950, .F. ) ;
#37792 = CARTESIAN_POINT ( 'NONE',  ( 0.000000000000000000, 4.000000000000000000, 0.000000000000000000 ) ) ;
#37793 = DIRECTION ( 'NONE',  ( 0.000000000000000000, -0.9459915920727718364, 0.3241911592372968554 ) ) ;
#37794 = CARTESIAN_POINT ( 'NONE',  ( -109.3314759607053759, -57.67120315069445269, 124.6891463060778165 ) ) ;
#37795 = CARTESIAN_POINT ( 'NONE',  ( -5.982126593009819970, -68.97334227892932290, 0.5333292889181892038 ) ) ;
#37796 = CONICAL_SURFACE ( 'NONE', #15416, 4.000000000000001776, 0.9599310885968808105 ) ;
#37797 = CARTESIAN_POINT ( 'NONE',  ( 0.4969600502617521620, 8.860760056385744932, 0.6527133886630304138 ) ) ;
#37798 = FACE_OUTER_BOUND ( 'NONE', #92361, .T. ) ;
#37799 = CYLINDRICAL_SURFACE ( 'NONE', #40791, 15.00000000000000711 ) ;
#37800 = CARTESIAN_POINT ( 'NONE',  ( 3.997425403568004132, 15.99999999372935022, -9.168149550321022190 ) ) ;
#37801 = COLOUR_RGB ( '', 0.09019608, 0.27058824, 0.51372549) ;
#37802 = CARTESIAN_POINT ( 'NONE',  ( 88.18294634653494768, -59.99999999999992895, -24.85591942078231043 ) ) ;
#37803 =( BOUNDED_CURVE ( )  B_SPLINE_CURVE ( 2, ( #57956, #91419, #16446 ),
 .UNSPECIFIED., .F., .F. ) 
 B_SPLINE_CURVE_WITH_KNOTS ( ( 3, 3 ),
 ( 0.000000000000000000, 1.000000000000000000 ),
 .UNSPECIFIED. ) 
 CURVE ( )  GEOMETRIC_REPRESENTATION_ITEM ( )  RATIONAL_B_SPLINE_CURVE ( ( 1.428571428571429047, 1.428571428571408397, 1.000000000000000000 ) ) 
 REPRESENTATION_ITEM ( '' )  );
#37804 = CARTESIAN_POINT ( 'NONE',  ( -70.80424915565322408, -29.99999999999997513, 131.6008933728038528 ) ) ;
#37805 = CARTESIAN_POINT ( 'NONE',  ( -54.32531917774948482, -60.32353084016035893, 67.31808107234573413 ) ) ;
#37806 = ORIENTED_EDGE ( 'NONE', *, *, #35063, .T. ) ;
#37807 = CARTESIAN_POINT ( 'NONE',  ( 43.87115969799069148, 464.7386531662421589, 11.09928998703298397 ) ) ;
#37808 = ORIENTED_EDGE ( 'NONE', *, *, #78575, .F. ) ;
#37809 = CARTESIAN_POINT ( 'NONE',  ( -99.49925588239455010, -37.80182837650123417, 191.3413508579977531 ) ) ;
#37810 =( BOUNDED_SURFACE ( )  B_SPLINE_SURFACE ( 2, 3, ( 
 ( #97359, #7813, #89820, #48273 ),
 ( #90341, #47743, #22981, #23513 ),
 ( #88754, #14847, #24052, #47216 ) ),
 .UNSPECIFIED., .F., .F., .F. ) 
 B_SPLINE_SURFACE_WITH_KNOTS ( ( 3, 3 ),
 ( 4, 4 ),
 ( 0.000000000000000000, 1.000000000000000000 ),
 ( -1.530452813897690353E-17, 0.06873863542433759910 ),
 .UNSPECIFIED. ) 
 GEOMETRIC_REPRESENTATION_ITEM ( )  RATIONAL_B_SPLINE_SURFACE ( (
 ( 1.000000000000000000, 1.000000000000000000, 1.000000000000000000, 1.000000000000000000),
 ( 1.857142857142858317, 1.857142857142858317, 1.857142857142858317, 1.857142857142858317),
 ( 1.000000000000000000, 1.000000000000000000, 1.000000000000000000, 1.000000000000000000) ) ) 
 REPRESENTATION_ITEM ( '' )  SURFACE ( )  );
#37811 = CARTESIAN_POINT ( 'NONE',  ( -1.102331679451517221, 51.47917464568522661, 9.610681418731136461 ) ) ;
#37812 = VECTOR ( 'NONE', #86956, 1000.000000000000000 ) ;
#37813 = ORIENTED_EDGE ( 'NONE', *, *, #57500, .T. ) ;
#37814 = CARTESIAN_POINT ( 'NONE',  ( 18.91765080832239221, 48.32805959737323320, 62.18241223506090165 ) ) ;
#37815 = FACE_OUTER_BOUND ( 'NONE', #27468, .T. ) ;
#37816 = SURFACE_SIDE_STYLE ('',( #71193 ) ) ;
#37817 = CARTESIAN_POINT ( 'NONE',  ( 7.188101187500000044, -15.03125000204838457, 0.000000000000000000 ) ) ;
#37818 = CARTESIAN_POINT ( 'NONE',  ( 32.35336999986095208, 300.6590557721156642, 11.25190399080426751 ) ) ;
#37819 = CARTESIAN_POINT ( 'NONE',  ( 14.83349330513380693, -4.000000000000000000, 4.898587196589415787E-16 ) ) ;
#37820 = FILL_AREA_STYLE ('',( #61548 ) ) ;
#37821 = CARTESIAN_POINT ( 'NONE',  ( 69.53704851309812796, -30.00000000000000000, 93.84895101583573762 ) ) ;
#37822 = CARTESIAN_POINT ( 'NONE',  ( -9.411401105578752535, 141.6908105720070239, -0.000000000000000000 ) ) ;
#37823 = DIRECTION ( 'NONE',  ( 0.000000000000000000, -0.9405207353770878020, 0.3397362893859623423 ) ) ;
#37824 = CARTESIAN_POINT ( 'NONE',  ( 43.10000000000000142, 1.533819458162526451E-15, 0.000000000000000000 ) ) ;
#37825 = CARTESIAN_POINT ( 'NONE',  ( -26.74884781052236704, -25.57352610173401430, 29.74563790467716728 ) ) ;
#37826 = ORIENTED_EDGE ( 'NONE', *, *, #99418, .F. ) ;
#37827 = ORIENTED_EDGE ( 'NONE', *, *, #89470, .T. ) ;
#37828 = CARTESIAN_POINT ( 'NONE',  ( 48.09347440250294881, -32.60269077776137436, 45.64648356772737259 ) ) ;
#37829 = CARTESIAN_POINT ( 'NONE',  ( -0.8583531473660760414, 8.496822302985666653, 51.42805900925117868 ) ) ;
#37830 = CARTESIAN_POINT ( 'NONE',  ( -6.879475648205854554, 16.78609259491953409, 1.316666052250859753 ) ) ;
#37831 = CARTESIAN_POINT ( 'NONE',  ( -108.6452951072574820, -38.35698101357876055, 191.2191590237300147 ) ) ;
#37832 = ORIENTED_EDGE ( 'NONE', *, *, #43975, .T. ) ;
#37833 = CARTESIAN_POINT ( 'NONE',  ( 91.19386398214668077, -38.35691295928401701, -0.5933418896404458742 ) ) ;
#37834 = CARTESIAN_POINT ( 'NONE',  ( 13.35126306661430995, 5.573441611265049112, -6.725115378757728912 ) ) ;
#37835 = CARTESIAN_POINT ( 'NONE',  ( -19.05430908020328573, 49.61020930493598513, 61.81757898065636425 ) ) ;
#37836 = CARTESIAN_POINT ( 'NONE',  ( 5.597109213676861650, 41.52722297769237514, -70.77038839093803801 ) ) ;
#37837 = VECTOR ( 'NONE', #19671, 999.9999999999998863 ) ;
#37838 = CARTESIAN_POINT ( 'NONE',  ( -33.51637563653506646, 434.0198191192274066, 13.77959778571810290 ) ) ;
#37839 = CARTESIAN_POINT ( 'NONE',  ( -33.38504658724071561, 488.8572893497079122, 10.16177171491941422 ) ) ;
#37840 = CARTESIAN_POINT ( 'NONE',  ( -32.21290004233181037, 485.9817488812122406, 5.040586218662800988 ) ) ;
#37841 = CARTESIAN_POINT ( 'NONE',  ( 103.3672439911610468, -59.99999999999999289, 200.3982682180039490 ) ) ;
#37842 = EDGE_CURVE ( 'NONE', #2138, #53725, #26146, .T. ) ;
#37843 = CARTESIAN_POINT ( 'NONE',  ( -16.34139928092842098, 35.06236595198802775, 21.87332501390299555 ) ) ;
#37844 = EDGE_LOOP ( 'NONE', ( #95355, #29469, #17175, #52738, #37467 ) ) ;
#37845 = EDGE_CURVE ( 'NONE', #48387, #90863, #30100, .T. ) ;
#37846 = CARTESIAN_POINT ( 'NONE',  ( -34.60124782188066206, 301.9306886739316838, -0.3923369183991654574 ) ) ;
#37847 = CARTESIAN_POINT ( 'NONE',  ( -2.500000000000001332, 0.000000000000000000, 0.000000000000000000 ) ) ;
#37848 = VECTOR ( 'NONE', #69343, 1000.000000000000000 ) ;
#37849 = CARTESIAN_POINT ( 'NONE',  ( 8.999999999999996447, 0.000000000000000000, 42.58845726811989607 ) ) ;
#37850 = ORIENTED_EDGE ( 'NONE', *, *, #41725, .T. ) ;
#37852 = DIRECTION ( 'NONE',  ( -0.000000000000000000, -0.000000000000000000, -1.000000000000000000 ) ) ;
#37851 = CARTESIAN_POINT ( 'NONE',  ( -103.7550299252929591, -38.41758574445464802, 198.5926835292501949 ) ) ;
#37853 = DIRECTION ( 'NONE',  ( -1.000000000000000000, -0.000000000000000000, -0.000000000000000000 ) ) ;
#37854 = CARTESIAN_POINT ( 'NONE',  ( 43.51084452654469459, 465.2903130129626561, 9.421687747985401984 ) ) ;
#37855 = SURFACE_SIDE_STYLE ('',( #78790 ) ) ;
#37856 = AXIS2_PLACEMENT_3D ( 'NONE', #3490, #26737, #77374 ) ;
#37857 = CARTESIAN_POINT ( 'NONE',  ( -7.188101187500002709, -14.18750000204838280, 2.977408999572648707 ) ) ;
#37858 = CARTESIAN_POINT ( 'NONE',  ( 5.036189802311931807, -3.000000000000002665, -76.26213611587876073 ) ) ;
#37859 = AXIS2_PLACEMENT_3D ( 'NONE', #3888, #79353, #36820 ) ;
#37860 = CARTESIAN_POINT ( 'NONE',  ( 30.00000000000000000, 461.8163627757383551, 11.11111419091032460 ) ) ;
#37861 = AXIS2_PLACEMENT_3D ( 'NONE', #92410, #84866, #10948 ) ;
#37863 = ORIENTED_EDGE ( 'NONE', *, *, #98299, .T. ) ;
#37862 = CARTESIAN_POINT ( 'NONE',  ( -51.48757442383523397, 38.95383793070303113, -37.45149417477429665 ) ) ;
#37864 = CARTESIAN_POINT ( 'NONE',  ( 80.87169800746870862, -60.48560008594591153, 182.4047845298172206 ) ) ;
#37865 = CARTESIAN_POINT ( 'NONE',  ( -44.27202126170846697, 463.8287145583149709, 7.882879088893235853 ) ) ;
#37866 = CARTESIAN_POINT ( 'NONE',  ( -38.13233550252180493, 438.4599495265808855, 23.49086985287510743 ) ) ;
#37867 = VERTEX_POINT ( 'NONE', #104481 ) ;
#37868 = DIRECTION ( 'NONE',  ( 0.000000000000000000, -1.000000000000000000, 0.000000000000000000 ) ) ;
#37869 = CARTESIAN_POINT ( 'NONE',  ( -4.250000000000000000, 5.204748896376250699E-16, -3.393184225085859929 ) ) ;
#37870 = DIRECTION ( 'NONE',  ( -1.000000000000000000, -1.224606353822377258E-16, -0.000000000000000000 ) ) ;
#37871 = SURFACE_STYLE_USAGE ( .BOTH. , #4939 ) ;
#37872 =( NAMED_UNIT ( * ) SI_UNIT ( $, .STERADIAN. ) SOLID_ANGLE_UNIT ( ) );
#37873 = VERTEX_POINT ( 'NONE', #72643 ) ;
#37874 = MECHANICAL_DESIGN_GEOMETRIC_PRESENTATION_REPRESENTATION (  '', ( #80935 ), #44776 ) ;
#37875 = CARTESIAN_POINT ( 'NONE',  ( -76.72470682087703153, -30.00000000000000355, -16.84832387072587778 ) ) ;
#37876 = DIRECTION ( 'NONE',  ( 0.000000000000000000, -1.000000000000000000, 0.000000000000000000 ) ) ;
#37877 = CARTESIAN_POINT ( 'NONE',  ( 14.46738925856536540, 21.80453881764446322, -4.782842684419118306 ) ) ;
#37879 = CARTESIAN_POINT ( 'NONE',  ( -43.50721599125494521, 484.7945671711814271, 4.126833950652403438 ) ) ;
#37878 = CARTESIAN_POINT ( 'NONE',  ( 7.320748848010288690, 41.41789156490656154, -68.91429206068630720 ) ) ;
#37880 = EDGE_CURVE ( 'NONE', #22977, #65105, #44275, .T. ) ;
#37881 = AXIS2_PLACEMENT_3D ( 'NONE', #78231, #32219, #39781 ) ;
#37882 = CARTESIAN_POINT ( 'NONE',  ( 2.977408999572651815, -19.43750000204838457, 7.188101187500000933 ) ) ;
#37883 = CARTESIAN_POINT ( 'NONE',  ( 35.11650669486618170, 4.898587196589413815E-16, -4.000000000000000888 ) ) ;
#37884 = CARTESIAN_POINT ( 'NONE',  ( -38.47428897411860760, 484.8307741943502833, -5.088672563356786860 ) ) ;
#37885 = AXIS2_PLACEMENT_3D ( 'NONE', #37180, #6344, #71101 ) ;
#37886 = CONTEXT_DEPENDENT_SHAPE_REPRESENTATION ( #65225, #61453 ) ;
#37887 = ORIENTED_EDGE ( 'NONE', *, *, #10500, .F. ) ;
#37888 = CARTESIAN_POINT ( 'NONE',  ( 24.05868969682389036, 1.340359594676612611E-15, 0.000000000000000000 ) ) ;
#37889 = DIRECTION ( 'NONE',  ( -0.000000000000000000, -1.000000000000000000, -0.000000000000000000 ) ) ;
#37890 = CARTESIAN_POINT ( 'NONE',  ( -8.985503746895339816, 15.44863866162878452, 0.000000000000000000 ) ) ;
#37891 = ADVANCED_FACE ( 'NONE', ( #91374 ), #50351, .F. ) ;
#37892 = EDGE_CURVE ( 'NONE', #84395, #39378, #9917, .T. ) ;
#37893 = DIRECTION ( 'NONE',  ( -1.000000000000000000, 0.000000000000000000, 0.000000000000000000 ) ) ;
#37894 = ORIENTED_EDGE ( 'NONE', *, *, #73094, .F. ) ;
#37895 = CARTESIAN_POINT ( 'NONE',  ( -34.15253942429701084, 465.0582672257402805, 17.72214182034827346 ) ) ;
#37896 = ORIENTED_EDGE ( 'NONE', *, *, #41302, .F. ) ;
#37897 = AXIS2_PLACEMENT_3D ( 'NONE', #54256, #21416, #44619 ) ;
#37898 = CARTESIAN_POINT ( 'NONE',  ( -28.35175412354155355, 34.21502232083763317, 8.615583304109071250 ) ) ;
#37899 = CARTESIAN_POINT ( 'NONE',  ( -40.93388221928996984, 39.67581419069122717, -51.72194110475966511 ) ) ;
#37900 = CARTESIAN_POINT ( 'NONE',  ( -48.02835407290534420, -1.200000000000000030E-05, -15.60535821593460248 ) ) ;
#37901 = CARTESIAN_POINT ( 'NONE',  ( -102.7322205242310247, -60.00000000000000000, 200.7630764697867960 ) ) ;
#37902 = CARTESIAN_POINT ( 'NONE',  ( 6.849999999999999645, 9.797174393178825657E-16, -8.000000000000000000 ) ) ;
#37903 = CARTESIAN_POINT ( 'NONE',  ( -3.460411933849569239E-15, -7.124194613927627984, -3.660532965668814143 ) ) ;
#37904 = CARTESIAN_POINT ( 'NONE',  ( -10.00000000000000178, -15.00000000000000000, -9.999999999999998224 ) ) ;
#37905 = DIRECTION ( 'NONE',  ( 0.000000000000000000, -1.000000000000000000, 0.000000000000000000 ) ) ;
#37906 = EDGE_CURVE ( 'NONE', #39330, #83609, #89156, .T. ) ;
#37907 = CARTESIAN_POINT ( 'NONE',  ( -85.12052891753060635, -28.84667419981521874, 173.9529900625116454 ) ) ;
#37908 = CARTESIAN_POINT ( 'NONE',  ( 39.05596081242668305, 42.03682209387911684, -56.80693097134772529 ) ) ;
#37909 = ORIENTED_EDGE ( 'NONE', *, *, #62711, .F. ) ;
#37910 = CARTESIAN_POINT ( 'NONE',  ( 6.400000000000000355, 0.000000000000000000, 8.000000000000000000 ) ) ;
#37911 = EDGE_CURVE ( 'NONE', #51816, #69452, #52967, .T. ) ;
#37912 = CARTESIAN_POINT ( 'NONE',  ( 4.472135954999576946, -65.27329903512642773, -4.000000000000004441 ) ) ;
#37913 = CARTESIAN_POINT ( 'NONE',  ( -83.68684263103561705, -45.26603780466695071, 9.535851223383053465 ) ) ;
#37914 = CIRCLE ( 'NONE', #99923, 5.000000000000000000 ) ;
#37915 = B_SPLINE_CURVE_WITH_KNOTS ( 'NONE', 3,
 ( #63290, #73470, #96190, #22320, #55165, #14174, #47078, #30946, #96713, #22849, #49738, #24964, #57819, #9799, #76667, #33580, #76137, #25510, #99887, #34664, #67004, #65931, #617, #1711, #58366, #92317, #91287, #34130, #26058, #17396, #67537, #90742, #16858, #82647, #59995, #10338, #33061, #75065, #58914, #42716, #91808, #19021, #66459, #1158, #17929, #75611, #50271, #50782, #99335, #100417 ),
 .UNSPECIFIED., .F., .F.,
 ( 4, 2, 2, 2, 2, 2, 2, 2, 2, 2, 2, 2, 2, 2, 2, 2, 2, 2, 2, 2, 2, 2, 2, 2, 4 ),
 ( 0.0002970904109619049312, 0.009133031734025364584, 0.01796897305708882245, 0.03564085570321574165, 0.05331273834934266431, 0.07098462099546958004, 0.08865650364159649577, 0.09749244496466002996, 0.1063283862877235642, 0.1107463569492554284, 0.1151643276107872926, 0.1195822982723191430, 0.1240002689338510072, 0.1284182395953828437, 0.1306272249261486995, 0.1328362102569145553, 0.1339407029222974832, 0.1350451955876804111, 0.1361496882530633390, 0.1372541809184462669, 0.1383586735838292225, 0.1394631662492121504, 0.1405676589145950783, 0.1411199052472865145, 0.1416721515799779785 ),
 .UNSPECIFIED. ) ;
#37916 = CARTESIAN_POINT ( 'NONE',  ( 33.82591814952031939, 464.6968131430474500, 6.992934999028691756 ) ) ;
#37917 = AXIS2_PLACEMENT_3D ( 'NONE', #69300, #28322, #35354 ) ;
#37918 = SURFACE_SIDE_STYLE ('',( #52456 ) ) ;
#37919 = CARTESIAN_POINT ( 'NONE',  ( 8.642223818570965221, 129.6034357518176989, 0.000000000000000000 ) ) ;
#37920 = CARTESIAN_POINT ( 'NONE',  ( 57.69562748396144514, 41.99999999999999289, 15.50526908259264225 ) ) ;
#37921 = CARTESIAN_POINT ( 'NONE',  ( 86.51021125171571668, -60.00000000000013500, 203.5141634203183685 ) ) ;
#37922 = MECHANICAL_DESIGN_GEOMETRIC_PRESENTATION_REPRESENTATION (  '', ( #48185 ), #98166 ) ;
#37923 = CARTESIAN_POINT ( 'NONE',  ( -4.425930005958663723E-15, 43.22324503868515677, 36.14046114390016839 ) ) ;
#37924 = CARTESIAN_POINT ( 'NONE',  ( -98.48977711285814962, -30.00000000000000355, 87.89215492326917456 ) ) ;
#37925 = CARTESIAN_POINT ( 'NONE',  ( -64.36786927653166401, -39.48549010098479073, 84.34220923411332649 ) ) ;
#37926 = ORIENTED_EDGE ( 'NONE', *, *, #105675, .F. ) ;
#37927 = CARTESIAN_POINT ( 'NONE',  ( -64.33156063945668279, 39.42582946629362084, 9.759223879856712358 ) ) ;
#37928 = CARTESIAN_POINT ( 'NONE',  ( 77.52758066070661869, -59.99999999999010214, 196.9906909439896765 ) ) ;
#37929 = ADVANCED_FACE ( 'NONE', ( #61684 ), #42635, .T. ) ;
#37930 = ORIENTED_EDGE ( 'NONE', *, *, #40352, .T. ) ;
#37931 = DIRECTION ( 'NONE',  ( -1.000000000000000000, -1.224606353822377258E-16, -0.000000000000000000 ) ) ;
#37932 = CARTESIAN_POINT ( 'NONE',  ( -7.188101187500002709, -17.18750000204838813, 2.977408999572647819 ) ) ;
#37933 = CARTESIAN_POINT ( 'NONE',  ( -4.814352310392310486, -8.203214058964258371, -3.583053941560742750 ) ) ;
#37934 = VERTEX_POINT ( 'NONE', #60613 ) ;
#37935 = CARTESIAN_POINT ( 'NONE',  ( 3.386166871500281950, -49.13792346205087114, 104.0373179439116882 ) ) ;
#37936 = VERTEX_POINT ( 'NONE', #85954 ) ;
#37937 = DIRECTION ( 'NONE',  ( 0.000000000000000000, -0.000000000000000000, 1.000000000000000000 ) ) ;
#37938 = EDGE_CURVE ( 'NONE', #16303, #87076, #83993, .T. ) ;
#37939 = FACE_OUTER_BOUND ( 'NONE', #33517, .T. ) ;
#37940 = CARTESIAN_POINT ( 'NONE',  ( -76.56013186602308451, -60.00000000000000000, -29.77863996211247510 ) ) ;
#37941 = CARTESIAN_POINT ( 'NONE',  ( 71.63333333333333997, 6.915964383211875250E-15, 0.000000000000000000 ) ) ;
#37942 = CARTESIAN_POINT ( 'NONE',  ( 5.082755093536325930, -9.968750002048384573, -5.082755093536325042 ) ) ;
#37943 = VECTOR ( 'NONE', #72084, 1000.000000000000000 ) ;
#37944 = LINE ( 'NONE', #103698, #79104 ) ;
#37945 =( BOUNDED_SURFACE ( )  B_SPLINE_SURFACE ( 3, 2, ( 
 ( #62288, #29923, #22374 ),
 ( #14755, #95179, #21311 ),
 ( #55734, #70365, #69831 ),
 ( #62810, #87616, #77925 ),
 ( #54682, #21840, #29409 ),
 ( #12634, #54148, #36966 ) ),
 .UNSPECIFIED., .F., .F., .F. ) 
 B_SPLINE_SURFACE_WITH_KNOTS ( ( 4, 2, 4 ),
 ( 3, 3 ),
 ( 0.003190620565844245072, 0.007281897438794512727, 0.01137317431174478082 ),
 ( 0.000000000000000000, 1.000000000000000000 ),
 .UNSPECIFIED. ) 
 GEOMETRIC_REPRESENTATION_ITEM ( )  RATIONAL_B_SPLINE_SURFACE ( (
 ( 1.000000000000000000, 0.8047731410850402778, 1.000000000000000000),
 ( 1.000000000000000000, 0.8125552299157379199, 1.000000000000000000),
 ( 1.000000000000000000, 0.8191520442888340359, 1.000000000000000000),
 ( 1.000000000000000000, 0.8191520442891404574, 1.000000000000000000),
 ( 1.000000000000000000, 0.8125552299155076597, 1.000000000000000000),
 ( 1.000000000000000000, 0.8047731410850398337, 1.000000000000000000) ) ) 
 REPRESENTATION_ITEM ( '' )  SURFACE ( )  );
#37946 = LINE ( 'NONE', #87006, #70551 ) ;
#37947 = CARTESIAN_POINT ( 'NONE',  ( 5.000000000000000888, -43.08885284240903957, 0.3536648518834484278 ) ) ;
#37948 = VECTOR ( 'NONE', #32766, 1000.000000000000000 ) ;
#37949 = CARTESIAN_POINT ( 'NONE',  ( -8.737863884121635394, 48.00000000000000000, -90.03618980231102853 ) ) ;
#37950 = CARTESIAN_POINT ( 'NONE',  ( 20.11650669486618881, -3.999999999999998224, 0.000000000000000000 ) ) ;
#37951 = CARTESIAN_POINT ( 'NONE',  ( -43.63597198433378566, 421.7854419661105112, 15.67568856678759204 ) ) ;
#37952 = CARTESIAN_POINT ( 'NONE',  ( 32.73643714039037889, 313.1396241591655212, -7.563205551003425064 ) ) ;
#37953 = VECTOR ( 'NONE', #79352, 1000.000000000000114 ) ;
#37954 = EDGE_LOOP ( 'NONE', ( #98817, #67469, #94579, #4850, #8681 ) ) ;
#37955 = CARTESIAN_POINT ( 'NONE',  ( 74.60950000000003968, 0.000000000000000000, 0.000000000000000000 ) ) ;
#37956 = CARTESIAN_POINT ( 'NONE',  ( 36.03585763630033512, -42.96736410595855915, 36.59562221089151990 ) ) ;
#37957 = CARTESIAN_POINT ( 'NONE',  ( -4.453875240779026079, -1.734723475976807094E-15, 16.57301948836938621 ) ) ;
#37958 = ORIENTED_EDGE ( 'NONE', *, *, #6227, .T. ) ;
#37959 = CARTESIAN_POINT ( 'NONE',  ( 6.333820801330181993, -6.982605850970108108, 0.9057718968895951406 ) ) ;
#37960 = CONICAL_SURFACE ( 'NONE', #74081, 3.309500000000001663, 0.9599310885968770357 ) ;
#37962 = CARTESIAN_POINT ( 'NONE',  ( 7.263825692932301514, 4.945657111639576442, -7.907570769506051533 ) ) ;
#37961 = CARTESIAN_POINT ( 'NONE',  ( 9.500000000000000000, -5.000000000000000000, -20.99851272547260095 ) ) ;
#37963 = DIRECTION ( 'NONE',  ( 0.000000000000000000, 0.000000000000000000, -1.000000000000000000 ) ) ;
#37964 = CARTESIAN_POINT ( 'NONE',  ( -4.852941176470590534, 25.66666666666755248, -70.80672828634229177 ) ) ;
#37965 = CARTESIAN_POINT ( 'NONE',  ( 32.94330508143927716, 4.999999999999994671, 6.123233995736758394E-16 ) ) ;
#37966 = DIRECTION ( 'NONE',  ( 0.000000000000000000, 0.000000000000000000, 1.000000000000000000 ) ) ;
#37967 = CARTESIAN_POINT ( 'NONE',  ( 8.929771841637641927, 1.482358050883964840E-15, 0.000000000000000000 ) ) ;
#37968 = ORIENTED_EDGE ( 'NONE', *, *, #61429, .T. ) ;
#37969 = AXIS2_PLACEMENT_3D ( 'NONE', #29943, #63894, #20825 ) ;
#37970 = CARTESIAN_POINT ( 'NONE',  ( 92.44495282290664306, -59.99999999999999289, -0.4686678803088884515 ) ) ;
#37971 = DIRECTION ( 'NONE',  ( -1.000000000000000000, -1.224606353822377258E-16, -0.000000000000000000 ) ) ;
#37972 = B_SPLINE_CURVE_WITH_KNOTS ( 'NONE', 3,
 ( #86021, #45549, #79489, #20785 ),
 .UNSPECIFIED., .F., .F.,
 ( 4, 4 ),
 ( 1.734723475976807094E-18, 0.001327912649060388655 ),
 .UNSPECIFIED. ) ;
#37973 = LINE ( 'NONE', #13104, #6556 ) ;
#37974 = DIRECTION ( 'NONE',  ( -0.000000000000000000, 1.000000000000000000, -0.000000000000000000 ) ) ;
#37975 = CARTESIAN_POINT ( 'NONE',  ( -13.12019779049608026, 19.43057441571500377, -7.665946815556264227 ) ) ;
#37976 = ORIENTED_EDGE ( 'NONE', *, *, #3982, .F. ) ;
#37977 = ADVANCED_FACE ( 'NONE', ( #3421 ), #67629, .F. ) ;
#37978 = CARTESIAN_POINT ( 'NONE',  ( -84.32296871598593668, -29.99999999998828670, -21.60099904174990115 ) ) ;
#37979 = VERTEX_POINT ( 'NONE', #20182 ) ;
#37980 = DIRECTION ( 'NONE',  ( 1.000000000000000000, 0.000000000000000000, 0.000000000000000000 ) ) ;
#37981 = CARTESIAN_POINT ( 'NONE',  ( 6.177150199754222193, -12.02207793746709008, -12.99999999999998757 ) ) ;
#37982 = LINE ( 'NONE', #54102, #47067 ) ;
#37983 = CARTESIAN_POINT ( 'NONE',  ( 16.10155139016696069, 21.86297139503093589, 0.4316986452390899065 ) ) ;
#37984 = CARTESIAN_POINT ( 'NONE',  ( -6.500000000000000000, 0.3213925021621101830, 3.146515640812911001E-15 ) ) ;
#37985 = CARTESIAN_POINT ( 'NONE',  ( 7.188101187500001821, -29.93750000204839523, -2.977408999572650483 ) ) ;
#37986 = AXIS2_PLACEMENT_3D ( 'NONE', #37884, #54527, #101521 ) ;
#37988 = EDGE_CURVE ( 'NONE', #40622, #57919, #93132, .T. ) ;
#37987 = CARTESIAN_POINT ( 'NONE',  ( -44.24141271893151384, 485.5284546383997508, 3.135518353093314392 ) ) ;
#37989 = CARTESIAN_POINT ( 'NONE',  ( 9.177423055815349784, 46.16989776044872684, -13.55706802408399980 ) ) ;
#37990 = DIRECTION ( 'NONE',  ( -0.000000000000000000, -1.000000000000000000, -0.000000000000000000 ) ) ;
#37991 = VERTEX_POINT ( 'NONE', #27742 ) ;
#37992 = EDGE_CURVE ( 'NONE', #27209, #30721, #43346, .T. ) ;
#37993 = ORIENTED_EDGE ( 'NONE', *, *, #92857, .F. ) ;
#37994 = CARTESIAN_POINT ( 'NONE',  ( 81.08675078009645176, -29.09168970534348020, 141.3822325320448101 ) ) ;
#37995 = CARTESIAN_POINT ( 'NONE',  ( -3.313708498984726969, -20.46874999999999289, 8.000000000000039080 ) ) ;
#37996 = VERTEX_POINT ( 'NONE', #101043 ) ;
#37997 = DIRECTION ( 'NONE',  ( 0.000000000000000000, -1.000000000000000000, 0.000000000000000000 ) ) ;
#37998 = CARTESIAN_POINT ( 'NONE',  ( 5.082755093536324154, -20.84375000204838813, 5.082755093536326818 ) ) ;
#37999 = CARTESIAN_POINT ( 'NONE',  ( -78.78539465073522763, -57.50642106797575082, 197.5849804933186817 ) ) ;
#38000 = VERTEX_POINT ( 'NONE', #84867 ) ;
#38001 = VECTOR ( 'NONE', #42950, 999.9999999999998863 ) ;
#38002 = FACE_OUTER_BOUND ( 'NONE', #34250, .T. ) ;
#38003 = CARTESIAN_POINT ( 'NONE',  ( -4.590682673078522846, -11.06791757312157465, 3.864023243754608039 ) ) ;
#38004 = VECTOR ( 'NONE', #80552, 1000.000000000000000 ) ;
#38005 = CARTESIAN_POINT ( 'NONE',  ( -9.482993638194541219, 82.55651279746325599, -3.177441187500463116 ) ) ;
#38006 = CARTESIAN_POINT ( 'NONE',  ( -6.500000000000002665, -2.501851166488398892, -5.848636054922038419 ) ) ;
#38007 = EDGE_CURVE ( 'NONE', #28004, #50935, #96674, .T. ) ;
#38008 = CARTESIAN_POINT ( 'NONE',  ( -3.313708498984760720, -10.71875000409676915, -8.000000000000000000 ) ) ;
#38009 = AXIS2_PLACEMENT_3D ( 'NONE', #69055, #51235, #20008 ) ;
#38010 = CARTESIAN_POINT ( 'NONE',  ( -5.638837409264774614, -12.95953527002633976, 32.08345554597801197 ) ) ;
#38011 = CARTESIAN_POINT ( 'NONE',  ( 9.700350089084166072, 15.75268258782372754, 2.455962139888934193 ) ) ;
#38012 = CARTESIAN_POINT ( 'NONE',  ( -46.00000000000000000, 488.9831568219306064, 4.757012338623855641 ) ) ;
#38013 = CARTESIAN_POINT ( 'NONE',  ( 7.230783165913826416, -2.999999999999999112, -70.90935356275363688 ) ) ;
#38014 = CARTESIAN_POINT ( 'NONE',  ( 3.313708498984722972, -19.71874999999999289, -8.000000000000040856 ) ) ;
#38015 = CARTESIAN_POINT ( 'NONE',  ( -9.989285784994811124, 33.97342427445700963, 0.5301777604595827587 ) ) ;
#38016 = VERTEX_POINT ( 'NONE', #62724 ) ;
#38017 = SURFACE_STYLE_USAGE ( .BOTH. , #26217 ) ;
#38018 = AXIS2_PLACEMENT_3D ( 'NONE', #38109, #79584, #13245 ) ;
#38019 = CARTESIAN_POINT ( 'NONE',  ( 11.21300718243333883, -4.973729321444529283, -12.57639419883998855 ) ) ;
#38020 = DIRECTION ( 'NONE',  ( 0.000000000000000000, -1.000000000000000000, 0.000000000000000000 ) ) ;
#38021 = CARTESIAN_POINT ( 'NONE',  ( -1.445468217397182231, -17.74378107465255283, -37.96072284730425395 ) ) ;
#38022 = CARTESIAN_POINT ( 'NONE',  ( -83.04267475782658892, -30.00000000000000711, 153.2271410443097182 ) ) ;
#38023 = ADVANCED_FACE ( 'NONE', ( #54590 ), #54637, .T. ) ;
#38024 = DIRECTION ( 'NONE',  ( 0.000000000000000000, 0.000000000000000000, 1.000000000000000000 ) ) ;
#38025 = ORIENTED_EDGE ( 'NONE', *, *, #46714, .F. ) ;
#38026 = CARTESIAN_POINT ( 'NONE',  ( 14.34999999999999787, -3.309499999999999886, 0.000000000000000000 ) ) ;
#38027 = CARTESIAN_POINT ( 'NONE',  ( 91.21504626101743440, -57.61349245510880479, 204.2098318074243366 ) ) ;
#38028 = CARTESIAN_POINT ( 'NONE',  ( 3.400000000000000355, 0.000000000000000000, -0.7408754770741831086 ) ) ;
#38030 = CARTESIAN_POINT ( 'NONE',  ( 32.93513049338658760, 465.6726574193327792, 10.66039033145146142 ) ) ;
#38029 = AXIS2_PLACEMENT_3D ( 'NONE', #67543, #34138, #99892 ) ;
#38031 = FACE_BOUND ( 'NONE', #36680, .T. ) ;
#38032 = DIRECTION ( 'NONE',  ( -1.000000000000000000, -1.224606353822377258E-16, -0.000000000000000000 ) ) ;
#38033 = CARTESIAN_POINT ( 'NONE',  ( -53.97748731286613832, -60.00000000000002842, 82.35806573917696483 ) ) ;
#38034 = CARTESIAN_POINT ( 'NONE',  ( 0.2259792476677729700, 7.636022678937404606, -6.470294263593366679 ) ) ;
#38035 = CARTESIAN_POINT ( 'NONE',  ( -32.17608548772882671, 486.0066403424740997, 5.076835838891838648 ) ) ;
#38036 = STYLED_ITEM ( 'NONE', ( #54302 ), #70720 ) ;
#38037 = CARTESIAN_POINT ( 'NONE',  ( 51.78317192861597107, 50.00000000002003731, 39.73656039222791492 ) ) ;
#38038 = CARTESIAN_POINT ( 'NONE',  ( -84.08473047087470320, -61.05543080211507601, 192.4300456549544833 ) ) ;
#38039 = ORIENTED_EDGE ( 'NONE', *, *, #28328, .F. ) ;
#38040 = CARTESIAN_POINT ( 'NONE',  ( 35.75530239586758796, 408.8884727095264111, 6.061804817591524674 ) ) ;
#38041 = DIRECTION ( 'NONE',  ( 0.000000000000000000, 0.000000000000000000, 1.000000000000000000 ) ) ;
#38042 = CARTESIAN_POINT ( 'NONE',  ( -6.394717965045618513, 41.92174107680550321, -59.37671525613893664 ) ) ;
#38043 = CARTESIAN_POINT ( 'NONE',  ( 0.000000000000000000, 15.00000000000000000, -10.00000000000000000 ) ) ;
#38044 = CARTESIAN_POINT ( 'NONE',  ( 12.32841007366230635, -4.394465204956419235, -76.76276077223143091 ) ) ;
#38045 = EDGE_CURVE ( 'NONE', #91737, #16098, #51241, .T. ) ;
#38046 = B_SPLINE_CURVE_WITH_KNOTS ( 'NONE', 3,
 ( #89961, #40344, #88900, #65685, #95536, #14998 ),
 .UNSPECIFIED., .F., .F.,
 ( 4, 1, 1, 4 ),
 ( 0.000000000000000000, 0.4213833399777465738, 0.5213833399777465516, 0.9843640123765010630 ),
 .UNSPECIFIED. ) ;
#38047 = CARTESIAN_POINT ( 'NONE',  ( -84.67955570590166303, -52.73943624728606494, -13.91631340859395571 ) ) ;
#38048 = DIRECTION ( 'NONE',  ( -1.000000000000000000, -1.224606353822377258E-16, -0.000000000000000000 ) ) ;
#38049 = CARTESIAN_POINT ( 'NONE',  ( -43.49620567743568955, 471.8615734360724332, 7.936790638083616400 ) ) ;
#38050 = ORIENTED_EDGE ( 'NONE', *, *, #90922, .F. ) ;
#38051 = CIRCLE ( 'NONE', #51775, 5.000000000000002665 ) ;
#38052 =( LENGTH_UNIT ( ) NAMED_UNIT ( * ) SI_UNIT ( .MILLI., .METRE. ) );
#38053 = CARTESIAN_POINT ( 'NONE',  ( 13.25615415199737335, 3.883583888817405239, 6.949209056975313992 ) ) ;
#38054 = ADVANCED_FACE ( 'NONE', ( #78886 ), #60611, .T. ) ;
#38055 = CARTESIAN_POINT ( 'NONE',  ( -22.23822744035697241, -8.673617379884035472E-16, -2.910977163147234759 ) ) ;
#38056 = CARTESIAN_POINT ( 'NONE',  ( -32.62734573167237073, 485.2399387473970478, 2.793905986283565568 ) ) ;
#38057 = CARTESIAN_POINT ( 'NONE',  ( 94.38107034336813683, -59.99999999999990763, 5.298252861571447703 ) ) ;
#38058 = MECHANICAL_DESIGN_GEOMETRIC_PRESENTATION_REPRESENTATION (  '', ( #51779 ), #65574 ) ;
#38059 = CARTESIAN_POINT ( 'NONE',  ( -78.23876340934074847, -49.90743072093854948, 145.7851689650335061 ) ) ;
#38060 = EDGE_LOOP ( 'NONE', ( #25298, #16514, #21991, #76964 ) ) ;
#38061 = CARTESIAN_POINT ( 'NONE',  ( 10.59999999999999609, 3.309500000000003439, 0.000000000000000000 ) ) ;
#38062 = CARTESIAN_POINT ( 'NONE',  ( 55.00571552735602410, -4.000000000000000000, 4.898587196589421703E-16 ) ) ;
#38063 = CARTESIAN_POINT ( 'NONE',  ( 87.55754732123112660, -57.59262797547410173, 203.3067698811781838 ) ) ;
#38064 = UNCERTAINTY_MEASURE_WITH_UNIT (LENGTH_MEASURE( 1.000000000000000082E-05 ), #56485, 'distance_accuracy_value', 'NONE');
#38065 = CARTESIAN_POINT ( 'NONE',  ( 37.66863543806578463, 305.0556223276453807, -7.649085916423524090 ) ) ;
#38066 = CARTESIAN_POINT ( 'NONE',  ( -5.641239428713638286E-16, -0.6346842323199932689, -6.500000000000000000 ) ) ;
#38067 = ORIENTED_EDGE ( 'NONE', *, *, #33326, .F. ) ;
#38068 = FILL_AREA_STYLE ('',( #79017 ) ) ;
#38069 = EDGE_CURVE ( 'NONE', #33365, #39498, #18653, .T. ) ;
#38070 = CARTESIAN_POINT ( 'NONE',  ( 31.95183731899507862, 438.9709496923862844, 23.61699702108921528 ) ) ;
#38071 = DIRECTION ( 'NONE',  ( 0.000000000000000000, -1.000000000000000000, 0.000000000000000000 ) ) ;
#38072 = CARTESIAN_POINT ( 'NONE',  ( 7.188101187500001821, -28.06250000204838813, -2.977408999572650483 ) ) ;
#38073 = ORIENTED_EDGE ( 'NONE', *, *, #23747, .T. ) ;
#38074 = CARTESIAN_POINT ( 'NONE',  ( 0.000000000000000000, 0.000000000000000000, 0.000000000000000000 ) ) ;
#38075 = FACE_OUTER_BOUND ( 'NONE', #81715, .T. ) ;
#38076 = DIRECTION ( 'NONE',  ( -1.000000000000000000, -1.224606353822377258E-16, -0.000000000000000000 ) ) ;
#38077 = DIRECTION ( 'NONE',  ( 0.000000000000000000, 0.000000000000000000, 1.000000000000000000 ) ) ;
#38078 = CARTESIAN_POINT ( 'NONE',  ( 8.099999999999999645, 0.000000000000000000, 0.000000000000000000 ) ) ;
#38079 = AXIS2_PLACEMENT_3D ( 'NONE', #77589, #34509, #43618 ) ;
#38080 = CARTESIAN_POINT ( 'NONE',  ( -37.72536826884616090, 463.3861702155473381, 19.97111768659724973 ) ) ;
#38081 = ORIENTED_EDGE ( 'NONE', *, *, #60495, .T. ) ;
#38082 = CARTESIAN_POINT ( 'NONE',  ( -7.004291982367333524, 40.56179000230169862, -71.01843131766943884 ) ) ;
#38084 = CARTESIAN_POINT ( 'NONE',  ( 26.88634610105399858, -60.34360723818206651, 35.78200920591456935 ) ) ;
#38083 = CARTESIAN_POINT ( 'NONE',  ( -75.56794833712217496, -14.21045842199431597, 141.5492349273399952 ) ) ;
#38085 = CARTESIAN_POINT ( 'NONE',  ( 23.54225815529381904, 28.03385386361088649, -30.74635459162673357 ) ) ;
#38086 = ORIENTED_EDGE ( 'NONE', *, *, #12758, .F. ) ;
#38087 = ORIENTED_EDGE ( 'NONE', *, *, #49370, .F. ) ;
#38088 =( NAMED_UNIT ( * ) SI_UNIT ( $, .STERADIAN. ) SOLID_ANGLE_UNIT ( ) );
#38089 = CARTESIAN_POINT ( 'NONE',  ( 111.8964183755431918, 22.97884757028484870, 55.94820918777161722 ) ) ;
#38090 = CARTESIAN_POINT ( 'NONE',  ( 7.439207106853293894, 40.67211991679438654, -59.07662331495946262 ) ) ;
#38091 = CARTESIAN_POINT ( 'NONE',  ( 5.947762761376481855, -6.880090707843056208, -1.083333333333333259 ) ) ;
#38092 = CARTESIAN_POINT ( 'NONE',  ( 12.13034742782427955, 48.00000000000000000, -93.82352941176471006 ) ) ;
#38093 = ORIENTED_EDGE ( 'NONE', *, *, #53491, .F. ) ;
#38094 = CARTESIAN_POINT ( 'NONE',  ( -1.469576158976823947E-15, -14.37499999999999112, 8.000000000000000000 ) ) ;
#38095 = CARTESIAN_POINT ( 'NONE',  ( 64.99863289610547668, -29.99999999999999289, 80.18763367229007599 ) ) ;
#38096 = CARTESIAN_POINT ( 'NONE',  ( -12.49438147519285813, 22.71955599834702966, -5.903923697086765898 ) ) ;
#38098 = CARTESIAN_POINT ( 'NONE',  ( 44.08840282922849241, 485.7747746244180007, 4.178803824087734320 ) ) ;
#38097 = VECTOR ( 'NONE', #64230, 1000.000000000000227 ) ;
#38099 = CARTESIAN_POINT ( 'NONE',  ( 76.87505874220391888, -29.99999999999999645, -16.73993432065925546 ) ) ;
#38100 =( GEOMETRIC_REPRESENTATION_CONTEXT ( 3 ) GLOBAL_UNCERTAINTY_ASSIGNED_CONTEXT ( ( #8494 ) ) GLOBAL_UNIT_ASSIGNED_CONTEXT ( ( #12194, #3047, #20360 ) ) REPRESENTATION_CONTEXT ( 'NONE', 'WORKASPACE' ) );
#38101 = DIRECTION ( 'NONE',  ( -0.000000000000000000, -1.000000000000000000, -0.000000000000000000 ) ) ;
#38102 = ORIENTED_EDGE ( 'NONE', *, *, #1086, .T. ) ;
#38103 = ADVANCED_FACE ( 'NONE', ( #16274 ), #65044, .T. ) ;
#38104 = VECTOR ( 'NONE', #51633, 1000.000000000000000 ) ;
#38105 = ORIENTED_EDGE ( 'NONE', *, *, #31173, .F. ) ;
#38106 = ORIENTED_EDGE ( 'NONE', *, *, #16832, .F. ) ;
#38107 = CARTESIAN_POINT ( 'NONE',  ( -9.035703905990970952, 10.37169118567824810, -0.1149164202474761975 ) ) ;
#38108 = DIRECTION ( 'NONE',  ( -0.000000000000000000, -0.000000000000000000, 1.000000000000000000 ) ) ;
#38109 = CARTESIAN_POINT ( 'NONE',  ( 19.00000000000001066, -4.000000000000000000, 0.000000000000000000 ) ) ;
#38111 = COLOUR_RGB ( '', 0.08235294, 0.09019608, 0.10196078) ;
#38110 = DIRECTION ( 'NONE',  ( 0.000000000000000000, 0.000000000000000000, -1.000000000000000000 ) ) ;
#38112 = CARTESIAN_POINT ( 'NONE',  ( 48.10000000000000142, 0.000000000000000000, 0.000000000000000000 ) ) ;
#38114 = EDGE_CURVE ( 'NONE', #56403, #100438, #49158, .T. ) ;
#38113 = DIRECTION ( 'NONE',  ( -1.000000000000000000, -0.000000000000000000, -0.000000000000000000 ) ) ;
#38115 = ORIENTED_EDGE ( 'NONE', *, *, #24728, .F. ) ;
#38116 = DIRECTION ( 'NONE',  ( -0.000000000000000000, 1.000000000000000000, -0.000000000000000000 ) ) ;
#38117 = AXIS2_PLACEMENT_3D ( 'NONE', #87974, #63167, #45917 ) ;
#38118 = B_SPLINE_CURVE_WITH_KNOTS ( 'NONE', 3,
 ( #72548, #16438, #23501, #31077, #48787, #7802, #105453, #40710, #97886, #73059, #14836, #14301, #15375, #63956, #31594, #73598, #96842, #22971, #32111, #55295 ),
 .UNSPECIFIED., .F., .F.,
 ( 4, 2, 2, 2, 2, 2, 2, 2, 2, 4 ),
 ( 0.000000000000000000, 0.001397185393360531221, 0.002095778090040806806, 0.002794370786721082391, 0.004191556180081631826, 0.005588741573442182128, 0.006985926966802732431, 0.008383112360163280999, 0.009780297753523832169, 0.01117748314688438160 ),
 .UNSPECIFIED. ) ;
#38119 = VERTEX_POINT ( 'NONE', #8714 ) ;
#38120 = FACE_OUTER_BOUND ( 'NONE', #23324, .T. ) ;
#38121 = DIRECTION ( 'NONE',  ( 0.9077394194975960673, 0.1875825441113498915, -0.3752624887127422038 ) ) ;
#38122 = CARTESIAN_POINT ( 'NONE',  ( -16.64348903516521005, 43.47556584774768140, -6.657797401561535544 ) ) ;
#38123 = CARTESIAN_POINT ( 'NONE',  ( -83.88445482477082749, -59.99999999999995737, 191.6821729358339610 ) ) ;
#38124 = CARTESIAN_POINT ( 'NONE',  ( 63.25588472527466877, -46.43434427221221483, 84.68567794870051557 ) ) ;
#38125 = ORIENTED_EDGE ( 'NONE', *, *, #98804, .F. ) ;
#38126 = CARTESIAN_POINT ( 'NONE',  ( 38.54943464502932926, 464.3877170423162397, 18.94545795437182178 ) ) ;
#38127 = CARTESIAN_POINT ( 'NONE',  ( -46.13793940742458233, -34.64890882579388887, -36.73075005924651748 ) ) ;
#38128 = CARTESIAN_POINT ( 'NONE',  ( -39.84523985364283050, 437.5033382181499633, 4.901783744328629844 ) ) ;
#38129 = DIRECTION ( 'NONE',  ( 0.1792365085106985001, 0.7133058216310638189, 0.6775463665640362176 ) ) ;
#38130 = EDGE_CURVE ( 'NONE', #85882, #83030, #105814, .T. ) ;
#38131 = ORIENTED_EDGE ( 'NONE', *, *, #47726, .T. ) ;
#38132 = AXIS2_PLACEMENT_3D ( 'NONE', #64543, #74204, #8943 ) ;
#38133 =( LENGTH_UNIT ( ) NAMED_UNIT ( * ) SI_UNIT ( .MILLI., .METRE. ) );
#38134 = DIRECTION ( 'NONE',  ( 0.9738156377458878632, 0.000000000000000000, -0.2273391820201038915 ) ) ;
#38135 = CARTESIAN_POINT ( 'NONE',  ( 70.89460441624491693, 4.000000000000013323, 0.000000000000000000 ) ) ;
#38136 = CONICAL_SURFACE ( 'NONE', #39798, 5.000000000000000000, 0.9599310885968913576 ) ;
#38137 = DIRECTION ( 'NONE',  ( -1.000000000000000000, -1.224606353822377258E-16, -0.000000000000000000 ) ) ;
#38138 = CIRCLE ( 'NONE', #15675, 4.000000000000007105 ) ;
#38139 = CARTESIAN_POINT ( 'NONE',  ( 3.313708498984762496, -29.46875000409677625, 7.999999999999998224 ) ) ;
#38140 = CARTESIAN_POINT ( 'NONE',  ( 7.086921372259695358E-15, 43.50000000000000711, -57.86910460382442523 ) ) ;
#38141 = CARTESIAN_POINT ( 'NONE',  ( 86.76698164667543267, -35.43929735535429870, 187.6249619233078363 ) ) ;
#38142 = CARTESIAN_POINT ( 'NONE',  ( -5.219506489253183723, 6.759691074813323652, -27.25072272683319952 ) ) ;
#38143 = CARTESIAN_POINT ( 'NONE',  ( -3.477260921866647703, 26.80326629624875423, 5.000000000000000000 ) ) ;
#38144 = DIRECTION ( 'NONE',  ( -1.000000000000000000, -1.224606353822377258E-16, -0.000000000000000000 ) ) ;
#38145 = CARTESIAN_POINT ( 'NONE',  ( 19.02088688056375787, 303.6992897676895495, 9.904581773955044355 ) ) ;
#38146 = CARTESIAN_POINT ( 'NONE',  ( 13.98736753405778543, -50.02671451802293490, 27.64795516495958339 ) ) ;
#38147 = CARTESIAN_POINT ( 'NONE',  ( 5.000000000000000000, -13.85537367056137192, 10.16084852768616997 ) ) ;
#38148 = CARTESIAN_POINT ( 'NONE',  ( -99.88944901110127716, -30.00000000000000355, 186.0585768036329739 ) ) ;
#38149 = VECTOR ( 'NONE', #103334, 1000.000000000000000 ) ;
#38150 = CARTESIAN_POINT ( 'NONE',  ( -3.250000000000013767, -5.629165124598844550, 1.734723475976807094E-15 ) ) ;
#38151 = CARTESIAN_POINT ( 'NONE',  ( 30.90980334511036176, -57.68590788500401345, 45.77300714667035919 ) ) ;
#38153 = LINE ( 'NONE', #14348, #55107 ) ;
#38152 = CARTESIAN_POINT ( 'NONE',  ( 11.52978300598590700, 12.35134215813147485, -9.999999999999882760 ) ) ;
#38154 = DIRECTION ( 'NONE',  ( 0.5000000000000008882, 0.8660254037844382635, -0.000000000000000000 ) ) ;
#38155 = CARTESIAN_POINT ( 'NONE',  ( -18.85365065124617701, 50.00000000000001421, 60.78410979961230964 ) ) ;
#38156 = CARTESIAN_POINT ( 'NONE',  ( -9.999999999999998224, 15.00000000000000000, 0.7768758660237131686 ) ) ;
#38157 = CARTESIAN_POINT ( 'NONE',  ( 30.00000000000000000, 0.000000000000000000, 8.000000000000007105 ) ) ;
#38158 = CARTESIAN_POINT ( 'NONE',  ( 9.452785795943286828, -16.11909601877263754, -34.86652532129186710 ) ) ;
#38159 = SURFACE_SIDE_STYLE ('',( #97806 ) ) ;
#38160 = CARTESIAN_POINT ( 'NONE',  ( -86.93315611284394606, -53.75507749461908702, 192.8295728004336240 ) ) ;
#38161 = ORIENTED_EDGE ( 'NONE', *, *, #61906, .T. ) ;
#38162 = CARTESIAN_POINT ( 'NONE',  ( 41.50869271557970563, 485.4378639541095595, -3.633045570236669519 ) ) ;
#38163 = CARTESIAN_POINT ( 'NONE',  ( 33.21102376836596193, 438.9613914113129454, 23.92328486949907784 ) ) ;
#38164 = CARTESIAN_POINT ( 'NONE',  ( -12.13119334609016065, -18.58662857061450069, 27.03411493363265450 ) ) ;
#38165 = AXIS2_PLACEMENT_3D ( 'NONE', #104799, #6626, #95136 ) ;
#38167 = DIRECTION ( 'NONE',  ( -0.000000000000000000, -0.000000000000000000, -1.000000000000000000 ) ) ;
#38166 = CARTESIAN_POINT ( 'NONE',  ( -86.95270011918000819, -60.00000000000005684, -4.645723306006363629 ) ) ;
#38168 = ADVANCED_FACE ( 'NONE', ( #73438 ), #41621, .F. ) ;
#38169 = ORIENTED_EDGE ( 'NONE', *, *, #89227, .T. ) ;
#38170 = CARTESIAN_POINT ( 'NONE',  ( 67.96666666666666856, 6.915964383211875250E-15, 0.000000000000000000 ) ) ;
#38171 = AXIS2_PLACEMENT_3D ( 'NONE', #13428, #5366, #105117 ) ;
#38172 = EDGE_CURVE ( 'NONE', #30465, #42532, #65891, .T. ) ;
#38173 = CARTESIAN_POINT ( 'NONE',  ( -13.38606538552758884, 42.81373475612566182, -92.09720263395749384 ) ) ;
#38174 = CIRCLE ( 'NONE', #19261, 1.999999999999999556 ) ;
#38175 = EDGE_CURVE ( 'NONE', #64739, #45575, #46050, .T. ) ;
#38176 = CIRCLE ( 'NONE', #98425, 2.000000000000000000 ) ;
#38177 = LINE ( 'NONE', #39217, #90765 ) ;
#38178 = CARTESIAN_POINT ( 'NONE',  ( -36.91281931599076671, 303.7809130842520631, -7.959270006439831846 ) ) ;
#38179 = VERTEX_POINT ( 'NONE', #97714 ) ;
#38180 = DIRECTION ( 'NONE',  ( 0.000000000000000000, 0.000000000000000000, 1.000000000000000000 ) ) ;
#38181 = CARTESIAN_POINT ( 'NONE',  ( 6.243930039575695118E-05, -60.00000000000000000, 42.00000000000000711 ) ) ;
#38182 = CARTESIAN_POINT ( 'NONE',  ( 91.95555555555554861, -4.171999999999998820, 0.000000000000000000 ) ) ;
#38183 = ORIENTED_EDGE ( 'NONE', *, *, #29269, .F. ) ;
#38184 = EDGE_CURVE ( 'NONE', #64513, #71627, #66970, .T. ) ;
#38185 = ORIENTED_EDGE ( 'NONE', *, *, #30875, .T. ) ;
#38186 = CARTESIAN_POINT ( 'NONE',  ( -26.26318723337799454, 307.7053845768774067, 10.82856312047318426 ) ) ;
#38187 = ORIENTED_EDGE ( 'NONE', *, *, #89542, .T. ) ;
#38188 =( NAMED_UNIT ( * ) SI_UNIT ( $, .STERADIAN. ) SOLID_ANGLE_UNIT ( ) );
#38189 = CARTESIAN_POINT ( 'NONE',  ( -40.21603221112191306, 460.7694907478774553, 2.143794914364798743 ) ) ;
#38190 = CARTESIAN_POINT ( 'NONE',  ( 5.656854249492378806, -12.87500000409676915, 5.656854249492381470 ) ) ;
#38191 = ORIENTED_EDGE ( 'NONE', *, *, #525, .F. ) ;
#38192 = FACE_OUTER_BOUND ( 'NONE', #8684, .T. ) ;
#38193 = CARTESIAN_POINT ( 'NONE',  ( -5.504991060908163369, 41.95607664920181179, -69.87069165643147528 ) ) ;
#38195 = CARTESIAN_POINT ( 'NONE',  ( -109.2418094552294718, -60.00000000000121503, 198.0553673896860687 ) ) ;
#38194 = AXIS2_PLACEMENT_3D ( 'NONE', #45313, #52857, #55360 ) ;
#38196 = CARTESIAN_POINT ( 'NONE',  ( 30.78144837821654889, -60.00000000000000000, -43.20504364394649599 ) ) ;
#38197 = CARTESIAN_POINT ( 'NONE',  ( 16.24800036964924388, -5.000000000000000000, 2.396130137889210587 ) ) ;
#38198 = CARTESIAN_POINT ( 'NONE',  ( -5.903045970190874847, 41.64520878214334232, -58.65814377447863137 ) ) ;
#38199 =( GEOMETRIC_REPRESENTATION_CONTEXT ( 3 ) GLOBAL_UNCERTAINTY_ASSIGNED_CONTEXT ( ( #31309 ) ) GLOBAL_UNIT_ASSIGNED_CONTEXT ( ( #15740, #90704, #66414 ) ) REPRESENTATION_CONTEXT ( 'NONE', 'WORKASPACE' ) );
#38201 = CARTESIAN_POINT ( 'NONE',  ( 9.184983414718331574, -35.99160910021836202, 29.89037362904370099 ) ) ;
#38200 = CARTESIAN_POINT ( 'NONE',  ( -88.56648999577124926, -14.21045842199433018, 40.40162738224969274 ) ) ;
#38202 = CARTESIAN_POINT ( 'NONE',  ( -49.20447750785626084, -25.67215719499521143, 45.04643150312214317 ) ) ;
#38203 = CONICAL_SURFACE ( 'NONE', #5454, 3.309500000000001663, 0.9599310885968770357 ) ;
#38204 = CARTESIAN_POINT ( 'NONE',  ( 0.8750000000000016653, -70.58759490697437400, 13.02737050516260098 ) ) ;
#38205 = PRODUCT ( '7. Anchor', '7. Anchor', '', ( #40099 ) ) ;
#38206 = VERTEX_POINT ( 'NONE', #42142 ) ;
#38207 = CARTESIAN_POINT ( 'NONE',  ( 36.56554981725791720, 437.5759650626826556, 4.257361216054158071 ) ) ;
#38208 = CARTESIAN_POINT ( 'NONE',  ( 16.91657744243869743, 36.34978592707985712, 24.30698433968583672 ) ) ;
#38209 = ORIENTED_EDGE ( 'NONE', *, *, #7559, .T. ) ;
#38210 = CARTESIAN_POINT ( 'NONE',  ( -7.819788844806560668, -14.69552936754710792, 15.37580215694229224 ) ) ;
#38211 = ORIENTED_EDGE ( 'NONE', *, *, #8544, .T. ) ;
#38212 = CARTESIAN_POINT ( 'NONE',  ( 93.19143838610155228, -29.99999999999330669, 199.8529442901022151 ) ) ;
#38213 = CARTESIAN_POINT ( 'NONE',  ( 6.245851208105055896, 41.90677386778757096, -59.22337204205300054 ) ) ;
#38214 = CARTESIAN_POINT ( 'NONE',  ( 102.6464385083043283, 1.030564683017419500E-14, 0.000000000000000000 ) ) ;
#38215 = CARTESIAN_POINT ( 'NONE',  ( 97.95297396224403030, -30.00000000000000711, 190.5773321744065925 ) ) ;
#38216 = DIRECTION ( 'NONE',  ( 0.000000000000000000, 0.000000000000000000, -1.000000000000000000 ) ) ;
#38217 = VERTEX_POINT ( 'NONE', #80999 ) ;
#38218 = EDGE_CURVE ( 'NONE', #48298, #53479, #83936, .T. ) ;
#38219 = VERTEX_POINT ( 'NONE', #51288 ) ;
#38220 = VERTEX_POINT ( 'NONE', #50748 ) ;
#38221 = DIRECTION ( 'NONE',  ( 0.000000000000000000, -1.000000000000000000, 0.000000000000000000 ) ) ;
#38222 = DIRECTION ( 'NONE',  ( -1.000000000000000000, -1.224606353822377258E-16, -0.000000000000000000 ) ) ;
#38223 = CARTESIAN_POINT ( 'NONE',  ( 63.07777777777777573, 6.915964383211875250E-15, 0.000000000000000000 ) ) ;
#38224 = EDGE_CURVE ( 'NONE', #41320, #27731, #100381, .T. ) ;
#38225 = EDGE_CURVE ( 'NONE', #44057, #93631, #59842, .T. ) ;
#38226 = VERTEX_POINT ( 'NONE', #2742 ) ;
#38227 = DIRECTION ( 'NONE',  ( -1.000000000000000000, -1.224606353822377258E-16, -0.000000000000000000 ) ) ;
#38228 = ORIENTED_EDGE ( 'NONE', *, *, #13122, .F. ) ;
#38229 = DIRECTION ( 'NONE',  ( 0.000000000000000000, -1.000000000000000000, 0.000000000000000000 ) ) ;
#38230 = CARTESIAN_POINT ( 'NONE',  ( 101.5753516748054750, -38.45075819519839655, 199.8879498216157344 ) ) ;
#38231 = CARTESIAN_POINT ( 'NONE',  ( 10.51501260721461151, 10.28692437246665214, 10.32948041498278435 ) ) ;
#38232 = CARTESIAN_POINT ( 'NONE',  ( 82.47009247757118544, -37.85521738824169091, 15.76104204749702653 ) ) ;
#38233 = CARTESIAN_POINT ( 'NONE',  ( 5.975663821522314123, -7.000939006314191637, 0.8740179403730684582 ) ) ;
#38234 = CARTESIAN_POINT ( 'NONE',  ( 42.75526354329229406, 382.2722604821533992, 18.98976758742777804 ) ) ;
#38235 = CARTESIAN_POINT ( 'NONE',  ( 22.33349330513380337, -4.000000000000000000, 4.898587196589415787E-16 ) ) ;
#38236 = FACE_OUTER_BOUND ( 'NONE', #64990, .T. ) ;
#38238 = B_SPLINE_CURVE_WITH_KNOTS ( 'NONE', 3,
 ( #85491, #2953, #77390, #77924, #12110, #68783, #36963, #19729, #36445, #68236, #28338, #101664, #69830, #28890, #61763, #61214, #69312, #94102 ),
 .UNSPECIFIED., .F., .F.,
 ( 4, 2, 2, 2, 2, 2, 2, 2, 4 ),
 ( 0.000000000000000000, 0.06250000000000000000, 0.1250000000000000000, 0.1875000000000000000, 0.2500000000000000000, 0.3125000000000000000, 0.3750000000000000000, 0.4375000000000000000, 0.5000000000000000000 ),
 .UNSPECIFIED. ) ;
#38237 = AXIS2_PLACEMENT_3D ( 'NONE', #94213, #10615, #69415 ) ;
#38239 = FACE_OUTER_BOUND ( 'NONE', #35520, .T. ) ;
#38240 =( GEOMETRIC_REPRESENTATION_CONTEXT ( 3 ) GLOBAL_UNCERTAINTY_ASSIGNED_CONTEXT ( ( #17141 ) ) GLOBAL_UNIT_ASSIGNED_CONTEXT ( ( #9670, #69012, #2651 ) ) REPRESENTATION_CONTEXT ( 'NONE', 'WORKASPACE' ) );
#38241 = CARTESIAN_POINT ( 'NONE',  ( 0.000000000000000000, 0.000000000000000000, -8.000000000000000000 ) ) ;
#38242 = ORIENTED_EDGE ( 'NONE', *, *, #106429, .T. ) ;
#38243 = EDGE_CURVE ( 'NONE', #37867, #69966, #74941, .T. ) ;
#38244 = CARTESIAN_POINT ( 'NONE',  ( -37.72254196851303476, 461.3702377715575835, 2.610691308934373289 ) ) ;
#38245 = LINE ( 'NONE', #46829, #48758 ) ;
#38246 = ORIENTED_EDGE ( 'NONE', *, *, #56545, .F. ) ;
#38247 = FACE_BOUND ( 'NONE', #82341, .T. ) ;
#38248 = CARTESIAN_POINT ( 'NONE',  ( -35.22718675236506414, 303.5445495247209919, 3.938089295098547549 ) ) ;
#38249 = CARTESIAN_POINT ( 'NONE',  ( 20.49977525862259142, 302.8459220885798686, -10.00124997875687427 ) ) ;
#38250 = CARTESIAN_POINT ( 'NONE',  ( 0.2578475836320665016, -4.367703157927319779, 5.434916218090832807 ) ) ;
#38251 = CARTESIAN_POINT ( 'NONE',  ( 7.999999999999998224, -17.09374999999999289, 3.313708498984766493 ) ) ;
#38252 = CARTESIAN_POINT ( 'NONE',  ( 2.680339019791157629, -14.91472760605375036, 34.48196116050767301 ) ) ;
#38253 = ADVANCED_FACE ( 'NONE', ( #83653 ), #7506, .F. ) ;
#38254 = CIRCLE ( 'NONE', #3743, 14.00000000000000178 ) ;
#38255 = DIRECTION ( 'NONE',  ( -1.000000000000000000, -1.224606353822377258E-16, -0.000000000000000000 ) ) ;
#38256 = ORIENTED_EDGE ( 'NONE', *, *, #11495, .F. ) ;
#38257 = CARTESIAN_POINT ( 'NONE',  ( 85.67508185048706082, -28.57312383954360868, 179.3342417396961253 ) ) ;
#38258 = EDGE_CURVE ( 'NONE', #21702, #85790, #94263, .T. ) ;
#38259 = CARTESIAN_POINT ( 'NONE',  ( -48.55208739724533729, 8.680497950467669810, 16.74317141725358127 ) ) ;
#38260 = CARTESIAN_POINT ( 'NONE',  ( -8.542937654374686218, 0.000000000000000000, -6.800000000000000711 ) ) ;
#38261 = ORIENTED_EDGE ( 'NONE', *, *, #92199, .F. ) ;
#38262 = CARTESIAN_POINT ( 'NONE',  ( 93.83510257185203329, -57.67426556498583778, 12.53502779676051304 ) ) ;
#38263 = CARTESIAN_POINT ( 'NONE',  ( 42.59614121018028499, 472.7198067255873184, 11.67823714611269104 ) ) ;
#38264 = CARTESIAN_POINT ( 'NONE',  ( -13.24502500595601795, -3.000000000000003553, -77.83160543687115762 ) ) ;
#38265 = CARTESIAN_POINT ( 'NONE',  ( 29.68315524077034340, 13.12249633091093415, 39.60535821593451544 ) ) ;
#38266 =( BOUNDED_CURVE ( )  B_SPLINE_CURVE ( 2, ( #101364, #35060, #51733, #91164, #76538, #58235, #67928, #75481, #25930 ),
 .UNSPECIFIED., .F., .F. ) 
 B_SPLINE_CURVE_WITH_KNOTS ( ( 3, 2, 2, 2, 3 ),
 ( 0.4558823529411765718, 0.4632352941176471894, 0.4705882352941177516, 0.4779411764705884247, 0.4852941176470589868 ),
 .UNSPECIFIED. ) 
 CURVE ( )  GEOMETRIC_REPRESENTATION_ITEM ( )  RATIONAL_B_SPLINE_CURVE ( ( 0.9999999999999988898, 0.9238795325112878487, 1.000000000000000000, 0.9238795325112867385, 1.000000000000000000, 0.9238795325112867385, 1.000000000000000000, 0.9238795325112849621, 1.000000000000001776 ) ) 
 REPRESENTATION_ITEM ( '' )  );
#38267 =( LENGTH_UNIT ( ) NAMED_UNIT ( * ) SI_UNIT ( .MILLI., .METRE. ) );
#38268 = AXIS2_PLACEMENT_3D ( 'NONE', #69081, #45855, #87388 ) ;
#38269 = PRESENTATION_LAYER_ASSIGNMENT (  '', '', ( #89896 ) ) ;
#38270 = DIRECTION ( 'NONE',  ( 1.000000000000000000, -0.000000000000000000, -0.000000000000000000 ) ) ;
#38271 = CARTESIAN_POINT ( 'NONE',  ( 3.871024465589348207, -1.214821636234518998, 104.2728733527511906 ) ) ;
#38272 = CARTESIAN_POINT ( 'NONE',  ( 39.96643535430156646, -26.31157452080049808, 35.93915362622938403 ) ) ;
#38274 = FACE_OUTER_BOUND ( 'NONE', #86079, .T. ) ;
#38273 = CARTESIAN_POINT ( 'NONE',  ( -30.00000000000000000, -54.00000000000000711, 27.11721482942554928 ) ) ;
#38275 = CARTESIAN_POINT ( 'NONE',  ( 42.51080986292980413, 487.1495428172316906, 7.889844863796903418 ) ) ;
#38276 =( LENGTH_UNIT ( ) NAMED_UNIT ( * ) SI_UNIT ( .MILLI., .METRE. ) );
#38277 = CARTESIAN_POINT ( 'NONE',  ( 43.47475788941068942, 362.3245890593326521, 12.84241293556198649 ) ) ;
#38278 = CARTESIAN_POINT ( 'NONE',  ( -17.41231411112303107, 294.5863894558068523, 1.881106854385071303 ) ) ;
#38279 = DIRECTION ( 'NONE',  ( 0.000000000000000000, 0.000000000000000000, 1.000000000000000000 ) ) ;
#38280 = ORIENTED_EDGE ( 'NONE', *, *, #42042, .T. ) ;
#38281 = CARTESIAN_POINT ( 'NONE',  ( -13.80956423950918754, 1.042457166890826903, 14.96477920397855854 ) ) ;
#38282 = SURFACE_SIDE_STYLE ('',( #38793 ) ) ;
#38283 = CARTESIAN_POINT ( 'NONE',  ( 4.813555570991610466, -63.20526203482679506, -3.584128953194789968 ) ) ;
#38285 = CARTESIAN_POINT ( 'NONE',  ( 6.197033621690949623, -21.77038157703285037, -30.42749805555791198 ) ) ;
#38284 = SURFACE_STYLE_USAGE ( .BOTH. , #6936 ) ;
#38286 = EDGE_CURVE ( 'NONE', #105826, #26612, #32581, .T. ) ;
#38287 = ORIENTED_EDGE ( 'NONE', *, *, #29291, .F. ) ;
#38288 = FILL_AREA_STYLE_COLOUR ( '', #9987 ) ;
#38289 = ORIENTED_EDGE ( 'NONE', *, *, #72519, .T. ) ;
#38290 = EDGE_CURVE ( 'NONE', #26814, #95526, #90853, .T. ) ;
#38291 = EDGE_CURVE ( 'NONE', #98079, #98690, #31249, .T. ) ;
#38292 = CARTESIAN_POINT ( 'NONE',  ( 6.333820801329741457, 6.982605850968585770, 0.9057718968909901358 ) ) ;
#38293 = DIRECTION ( 'NONE',  ( -1.000000000000000000, -1.224606353822377258E-16, -0.000000000000000000 ) ) ;
#38294 = CARTESIAN_POINT ( 'NONE',  ( -92.53755267726359079, -60.00000000000000711, -1.808094159106042653 ) ) ;
#38295 = VERTEX_POINT ( 'NONE', #15367 ) ;
#38296 = CARTESIAN_POINT ( 'NONE',  ( 8.000000000000000000, 9.797174393178825657E-16, -12.97459999999999525 ) ) ;
#38297 = CARTESIAN_POINT ( 'NONE',  ( 7.681258945454893382E-14, -1.200000000000000030E-05, 39.50000000000000000 ) ) ;
#38298 = CARTESIAN_POINT ( 'NONE',  ( -9.177080501238306098, 29.46653057145731580, -3.972956046786646489 ) ) ;
#38300 = DIRECTION ( 'NONE',  ( -1.000000000000000000, -1.224606353822377258E-16, -0.000000000000000000 ) ) ;
#38299 = CARTESIAN_POINT ( 'NONE',  ( 35.90484354297773706, 6.123233995736770227E-16, -5.000000000000002665 ) ) ;
#38301 = ADVANCED_FACE ( 'NONE', ( #23494, #39666 ), #88736, .T. ) ;
#38302 = CARTESIAN_POINT ( 'NONE',  ( -80.00123558984591909, -60.37367201449674070, 175.0854090040365065 ) ) ;
#38303 = EDGE_LOOP ( 'NONE', ( #54972, #74612, #93676, #78494 ) ) ;
#38304 = CARTESIAN_POINT ( 'NONE',  ( -15.29459302239368235, 0.000000000000000000, -7.540142361543696659 ) ) ;
#38305 = VECTOR ( 'NONE', #87458, 1000.000000000000114 ) ;
#38306 = EDGE_CURVE ( 'NONE', #103934, #74067, #58115, .T. ) ;
#38307 = EDGE_LOOP ( 'NONE', ( #19353, #6998, #17946, #89506 ) ) ;
#38308 = EDGE_LOOP ( 'NONE', ( #98871, #86644, #83318, #48577, #37361, #64629 ) ) ;
#38309 = CYLINDRICAL_SURFACE ( 'NONE', #24242, 4.000000000000000000 ) ;
#38310 = DIRECTION ( 'NONE',  ( 0.000000000000000000, 1.000000000000000000, 0.000000000000000000 ) ) ;
#38311 = EDGE_LOOP ( 'NONE', ( #97726, #66716, #32558, #79569, #53995 ) ) ;
#38312 = CARTESIAN_POINT ( 'NONE',  ( 15.89370886130898164, 45.88935169965960625, -6.420701231162496470 ) ) ;
#38313 = CARTESIAN_POINT ( 'NONE',  ( -84.33710589588049800, -57.55216090540037044, 201.9444809301270141 ) ) ;
#38314 = CARTESIAN_POINT ( 'NONE',  ( 1.561526116976854173, -49.96194285232682830, 101.5970966559196000 ) ) ;
#38315 = DIRECTION ( 'NONE',  ( 0.000000000000000000, 1.000000000000000000, 0.000000000000000000 ) ) ;
#38316 =( NAMED_UNIT ( * ) PLANE_ANGLE_UNIT ( ) SI_UNIT ( $, .RADIAN. ) );
#38317 =( LENGTH_UNIT ( ) NAMED_UNIT ( * ) SI_UNIT ( .MILLI., .METRE. ) );
#38318 = AXIS2_PLACEMENT_3D ( 'NONE', #39256, #55913, #72132 ) ;
#38319 = CARTESIAN_POINT ( 'NONE',  ( 87.78053949331578565, -14.21045842199421294, -8.623972743651103556 ) ) ;
#38320 = AXIS2_PLACEMENT_3D ( 'NONE', #80151, #48831, #7848 ) ;
#38321 = CARTESIAN_POINT ( 'NONE',  ( -67.17213121490354411, -60.00000000000000000, 138.9710117141604826 ) ) ;
#38322 = CARTESIAN_POINT ( 'NONE',  ( -54.89818758952581845, -56.85426884866628683, 67.23925021769613863 ) ) ;
#38323 = EDGE_LOOP ( 'NONE', ( #38444, #9808, #25734, #57591, #43930 ) ) ;
#38324 = CARTESIAN_POINT ( 'NONE',  ( -6.999999999999975131, -12.54465221550630183, 8.223849511754991681 ) ) ;
#38325 = ORIENTED_EDGE ( 'NONE', *, *, #43829, .T. ) ;
#38326 = CARTESIAN_POINT ( 'NONE',  ( -100.7112993965425147, -45.26202956731061278, 191.7609640039119370 ) ) ;
#38327 = APPLICATION_CONTEXT ( 'automotive_design' ) ;
#38328 = CARTESIAN_POINT ( 'NONE',  ( -30.63818566637198515, 16.09127295623279608, -40.04027533505464476 ) ) ;
#38329 = ORIENTED_EDGE ( 'NONE', *, *, #31070, .F. ) ;
#38330 = CARTESIAN_POINT ( 'NONE',  ( 19.11197997874395327, 49.68659357142563238, 61.71932382479903367 ) ) ;
#38331 = CARTESIAN_POINT ( 'NONE',  ( -15.51619600599612525, -60.00000000000000000, 39.81136932477215140 ) ) ;
#38332 = CARTESIAN_POINT ( 'NONE',  ( -42.48192783572968523, 485.4100919824712719, -3.499593777785077631 ) ) ;
#38333 = CARTESIAN_POINT ( 'NONE',  ( 85.31310517497098544, 1.030564683017419500E-14, 0.000000000000000000 ) ) ;
#38334 = DIRECTION ( 'NONE',  ( 0.000000000000000000, 1.000000000000000000, 0.000000000000000000 ) ) ;
#38335 = DIRECTION ( 'NONE',  ( -1.000000000000000000, 0.000000000000000000, 0.000000000000000000 ) ) ;
#38336 = CARTESIAN_POINT ( 'NONE',  ( -40.73878143178837519, 486.4834083601638213, 16.46716573231486436 ) ) ;
#38337 = CIRCLE ( 'NONE', #98580, 12.50000000000000533 ) ;
#38338 = CARTESIAN_POINT ( 'NONE',  ( -9.609486011791419813, 143.0915023496522736, 0.000000000000000000 ) ) ;
#38339 = DIRECTION ( 'NONE',  ( -1.000000000000000000, 0.000000000000000000, 0.000000000000000000 ) ) ;
#38340 = ADVANCED_BREP_SHAPE_REPRESENTATION ( '', ( #52984, #10728 ), #57385 ) ;
#38341 = UNCERTAINTY_MEASURE_WITH_UNIT (LENGTH_MEASURE( 1.000000000000000082E-05 ), #10449, 'distance_accuracy_value', 'NONE');
#38342 = CARTESIAN_POINT ( 'NONE',  ( -27.79213640563233767, -36.00755841895716003, 31.83339595010198408 ) ) ;
#38343 = MECHANICAL_DESIGN_GEOMETRIC_PRESENTATION_REPRESENTATION (  '', ( #84814 ), #65862 ) ;
#38344 = EDGE_LOOP ( 'NONE', ( #64597, #48670, #80215, #45234, #33120, #69664 ) ) ;
#38345 = ORIENTED_EDGE ( 'NONE', *, *, #79970, .F. ) ;
#38346 = CARTESIAN_POINT ( 'NONE',  ( 46.18361529899789275, -22.24103619873750404, 40.23939593157469119 ) ) ;
#38347 = CARTESIAN_POINT ( 'NONE',  ( 33.00000000000000000, 439.7597899781497972, 24.16317522621304192 ) ) ;
#38348 = CARTESIAN_POINT ( 'NONE',  ( -7.000111909206518490, 17.00019584125958616, -0.1284026198027884702 ) ) ;
#38349 = ADVANCED_FACE ( 'NONE', ( #40175 ), #48779, .F. ) ;
#38350 = CARTESIAN_POINT ( 'NONE',  ( -110.8441515072943986, -38.35618291059805074, 166.5699242065477677 ) ) ;
#38351 = ORIENTED_EDGE ( 'NONE', *, *, #28069, .F. ) ;
#38352 = CARTESIAN_POINT ( 'NONE',  ( 90.05187521117480287, -38.39608854082356970, -15.95136963641786920 ) ) ;
#38353 = CARTESIAN_POINT ( 'NONE',  ( 15.04093380808766867, 5.422855115928403968, -6.531324706886918463 ) ) ;
#38354 = CARTESIAN_POINT ( 'NONE',  ( -19.45095198684093063, 49.97783521840197807, 60.61741209756609550 ) ) ;
#38355 = FILL_AREA_STYLE_COLOUR ( '', #19009 ) ;
#38356 = PRESENTATION_STYLE_ASSIGNMENT (( #61564 ) ) ;
#38357 = FACE_OUTER_BOUND ( 'NONE', #16112, .T. ) ;
#38358 = CARTESIAN_POINT ( 'NONE',  ( 0.5805565836007701153, -7.505553499465148271, -1.383738442504732931E-16 ) ) ;
#38359 = CARTESIAN_POINT ( 'NONE',  ( 93.12889346891942921, -59.99999999999998579, 202.4813445689636922 ) ) ;
#38360 = CARTESIAN_POINT ( 'NONE',  ( 18.78726065216163477, 45.00000000000000000, 62.22585866237294994 ) ) ;
#38361 = VERTEX_POINT ( 'NONE', #73050 ) ;
#38362 = CARTESIAN_POINT ( 'NONE',  ( 56.92742074447681233, -32.55220054188133361, 61.62941135532160786 ) ) ;
#38363 = CARTESIAN_POINT ( 'NONE',  ( -30.10228782825764426, 308.0113986215986870, -8.824383475263772425 ) ) ;
#38364 = CARTESIAN_POINT ( 'NONE',  ( 7.986711519608433285, 33.97361903623433932, -0.5300249774147544057 ) ) ;
#38365 = CARTESIAN_POINT ( 'NONE',  ( -7.619753052866897747, 26.82548497192825465, -2.447276542590443249 ) ) ;
#38366 = ORIENTED_EDGE ( 'NONE', *, *, #88197, .T. ) ;
#38368 = CARTESIAN_POINT ( 'NONE',  ( 0.000000000000000000, 45.89575828009193259, 0.000000000000000000 ) ) ;
#38367 = CARTESIAN_POINT ( 'NONE',  ( -99.91270067421781675, -38.46799138967286780, 200.5326549990056151 ) ) ;
#38369 = DIRECTION ( 'NONE',  ( 0.000000000000000000, 0.000000000000000000, 1.000000000000000000 ) ) ;
#38370 = FACE_OUTER_BOUND ( 'NONE', #77844, .T. ) ;
#38371 =( NAMED_UNIT ( * ) SI_UNIT ( $, .STERADIAN. ) SOLID_ANGLE_UNIT ( ) );
#38372 = CARTESIAN_POINT ( 'NONE',  ( -7.188101187500000044, -11.28125000204838457, -8.802885111219163269E-16 ) ) ;
#38373 = CARTESIAN_POINT ( 'NONE',  ( 8.737863884122765157, -5.000000000000000888, -79.96381019769943066 ) ) ;
#38374 = EDGE_CURVE ( 'NONE', #20894, #68049, #98408, .T. ) ;
#38375 = PLANE ( 'NONE',  #65552 ) ;
#38377 = VERTEX_POINT ( 'NONE', #30527 ) ;
#38376 = FACE_OUTER_BOUND ( 'NONE', #56762, .T. ) ;
#38378 = CARTESIAN_POINT ( 'NONE',  ( 85.31446539190037015, -22.01966134143505371, 163.9754572180653440 ) ) ;
#38379 = ADVANCED_FACE ( 'NONE', ( #72018 ), #73653, .T. ) ;
#38380 = CARTESIAN_POINT ( 'NONE',  ( 8.731365433225425576, 20.06141188278254006, -2.602085213965209853E-15 ) ) ;
#38381 = CARTESIAN_POINT ( 'NONE',  ( -41.50820411079202188, 461.5963371455320612, 2.703439750996428081 ) ) ;
#38382 = EDGE_LOOP ( 'NONE', ( #53950, #76863, #12378, #21178 ) ) ;
#38383 = VECTOR ( 'NONE', #21420, 1000.000000000000000 ) ;
#38384 = CARTESIAN_POINT ( 'NONE',  ( -35.21460518038509235, 323.6916001596177352, -4.906611162513216051 ) ) ;
#38385 = CARTESIAN_POINT ( 'NONE',  ( 17.97922351027873589, 34.27503843121980509, 23.34624828125660656 ) ) ;
#38386 = DIRECTION ( 'NONE',  ( -0.000000000000000000, -1.000000000000000000, -0.000000000000000000 ) ) ;
#38387 = FILL_AREA_STYLE ('',( #69672 ) ) ;
#38388 = FACE_OUTER_BOUND ( 'NONE', #12981, .T. ) ;
#38389 = ORIENTED_EDGE ( 'NONE', *, *, #103598, .F. ) ;
#38390 = SURFACE_STYLE_USAGE ( .BOTH. , #15668 ) ;
#38392 = CARTESIAN_POINT ( 'NONE',  ( -6.342436232120165052, 297.2558017715909386, 7.735853733431446777 ) ) ;
#38391 = TOROIDAL_SURFACE ( 'NONE', #84873, 8.499999999999992895, 0.5000000000000000000 ) ;
#38393 = CARTESIAN_POINT ( 'NONE',  ( -1.000000000000000000, -26.68136363036562742, -6.178889730600807262 ) ) ;
#38394 = CARTESIAN_POINT ( 'NONE',  ( 6.800000000000000711, 6.613092715395708453E-16, 5.400000000000001243 ) ) ;
#38396 = CARTESIAN_POINT ( 'NONE',  ( -10.81758598141882644, 16.04212470968489868, -9.532093978217352159 ) ) ;
#38395 = CARTESIAN_POINT ( 'NONE',  ( -0.1795511817381551245, -18.03052986994432061, 35.00506736773241556 ) ) ;
#38397 = PRODUCT_RELATED_PRODUCT_CATEGORY ( 'part', '', ( #63166 ) ) ;
#38398 = CARTESIAN_POINT ( 'NONE',  ( -2.977408999572654480, -21.12500000204838813, 7.188101187499999156 ) ) ;
#38399 = CARTESIAN_POINT ( 'NONE',  ( 16.03995343662826656, 302.5635438422187917, -10.06125143394410237 ) ) ;
#38400 = DIRECTION ( 'NONE',  ( 0.000000000000000000, -1.000000000000000000, 0.000000000000000000 ) ) ;
#38401 = ORIENTED_EDGE ( 'NONE', *, *, #43117, .F. ) ;
#38402 = DIRECTION ( 'NONE',  ( 0.000000000000000000, -0.000000000000000000, 1.000000000000000000 ) ) ;
#38403 = CARTESIAN_POINT ( 'NONE',  ( 0.000000000000000000, 0.000000000000000000, -0.7256075382097185722 ) ) ;
#38404 = CARTESIAN_POINT ( 'NONE',  ( -9.737904753430131066, 8.235624462465031215, -5.000000000000000888 ) ) ;
#38405 = VECTOR ( 'NONE', #26212, 1000.000000000000000 ) ;
#38406 = FILL_AREA_STYLE ('',( #53509 ) ) ;
#38407 = DIRECTION ( 'NONE',  ( 0.000000000000000000, -1.000000000000000000, 0.000000000000000000 ) ) ;
#38408 = ORIENTED_EDGE ( 'NONE', *, *, #25287, .F. ) ;
#38409 = CARTESIAN_POINT ( 'NONE',  ( 10.59999999999999609, 3.309500000000003439, 4.052968581778167743E-16 ) ) ;
#38410 = CARTESIAN_POINT ( 'NONE',  ( 4.898587196589412829E-16, -21.31250000409676915, -8.000000000000000000 ) ) ;
#38411 = PRESENTATION_LAYER_ASSIGNMENT (  '', '', ( #22871 ) ) ;
#38412 = EDGE_LOOP ( 'NONE', ( #44222, #90043, #51472, #5886 ) ) ;
#38413 = SHAPE_REPRESENTATION ( '11. Strainer', ( #10728 ), #105516 ) ;
#38414 = EDGE_CURVE ( 'NONE', #90133, #15190, #96934, .T. ) ;
#38415 = PRESENTATION_STYLE_ASSIGNMENT (( #86442 ) ) ;
#38416 = CARTESIAN_POINT ( 'NONE',  ( -3.678498789086714016, -1.016373932518044532, 104.0112638849122959 ) ) ;
#38417 = DIRECTION ( 'NONE',  ( 0.000000000000000000, 0.000000000000000000, 1.000000000000000000 ) ) ;
#38418 = SURFACE_STYLE_FILL_AREA ( #6536 ) ;
#38419 = UNCERTAINTY_MEASURE_WITH_UNIT (LENGTH_MEASURE( 1.000000000000000082E-05 ), #31035, 'distance_accuracy_value', 'NONE');
#38420 = CARTESIAN_POINT ( 'NONE',  ( -111.0763646976983381, -60.00000000000000000, 152.8868246609566484 ) ) ;
#38421 = DIRECTION ( 'NONE',  ( 0.000000000000000000, 0.000000000000000000, -1.000000000000000000 ) ) ;
#38422 = FILL_AREA_STYLE ('',( #20682 ) ) ;
#38423 = CARTESIAN_POINT ( 'NONE',  ( 44.03570364123596192, 435.3116947630522873, 15.43179346459484513 ) ) ;
#38424 = CARTESIAN_POINT ( 'NONE',  ( 16.91742856729430855, 34.95464097504886780, -21.80698433968623462 ) ) ;
#38425 = CARTESIAN_POINT ( 'NONE',  ( -86.13551971958956699, -21.45869068250014067, 175.8984454080961370 ) ) ;
#38426 = ORIENTED_EDGE ( 'NONE', *, *, #46903, .F. ) ;
#38427 = CARTESIAN_POINT ( 'NONE',  ( 44.98274357202011231, 41.27416156066848885, -48.65895178432889168 ) ) ;
#38428 = EDGE_CURVE ( 'NONE', #69383, #51961, #65976, .T. ) ;
#38429 = ORIENTED_EDGE ( 'NONE', *, *, #81648, .F. ) ;
#38430 = CARTESIAN_POINT ( 'NONE',  ( 0.000000000000000000, 0.000000000000000000, -4.289342857142857568 ) ) ;
#38431 = ADVANCED_FACE ( 'NONE', ( #105447 ), #34137, .T. ) ;
#38432 = CARTESIAN_POINT ( 'NONE',  ( 5.999787407977320797, -68.99968111184449526, 0.2740427891043017983 ) ) ;
#38433 = CARTESIAN_POINT ( 'NONE',  ( -84.93247734541225213, -52.70439048363899559, 14.92132537576424589 ) ) ;
#38434 = CARTESIAN_POINT ( 'NONE',  ( -3.339336928304093011, 304.8518027742523486, 9.936999414809044140 ) ) ;
#38435 = CARTESIAN_POINT ( 'NONE',  ( 7.869427812662811661, 87.30462500886650901, 0.000000000000000000 ) ) ;
#38436 = CARTESIAN_POINT ( 'NONE',  ( 0.000000000000000000, 0.000000000000000000, 0.000000000000000000 ) ) ;
#38437 = CARTESIAN_POINT ( 'NONE',  ( 47.37019975555959661, 42.00000000000001421, -36.40416150955741870 ) ) ;
#38438 = CARTESIAN_POINT ( 'NONE',  ( 97.75109942996037660, -59.99999999999985789, 204.9114775063931120 ) ) ;
#38439 = CARTESIAN_POINT ( 'NONE',  ( -110.2447566669111154, -59.99999999999998579, 128.1452744908969521 ) ) ;
#38440 = CARTESIAN_POINT ( 'NONE',  ( -63.15306896468232623, -53.39223773315245580, 87.98131365993890540 ) ) ;
#38441 = EDGE_LOOP ( 'NONE', ( #66088, #51184, #16409, #45236 ) ) ;
#38442 = CARTESIAN_POINT ( 'NONE',  ( -63.17583207858296390, 39.42583197079326851, 15.57582698347478001 ) ) ;
#38443 = CARTESIAN_POINT ( 'NONE',  ( 76.19937483932648092, -59.99999999999009503, 194.9015389639207285 ) ) ;
#38444 = ORIENTED_EDGE ( 'NONE', *, *, #41000, .F. ) ;
#38445 = CARTESIAN_POINT ( 'NONE',  ( 13.60728112438141402, -56.44183047709488221, 30.29609480636782592 ) ) ;
#38446 = CARTESIAN_POINT ( 'NONE',  ( 5.082755093536325930, -22.34375000204838457, -5.082755093536325042 ) ) ;
#38447 = CARTESIAN_POINT ( 'NONE',  ( 43.00000000000000000, 500.0000000000002274, 12.00000000000000711 ) ) ;
#38448 = ORIENTED_EDGE ( 'NONE', *, *, #31356, .T. ) ;
#38449 = CARTESIAN_POINT ( 'NONE',  ( 96.28888888888889142, 1.023464760207051730E-14, 0.000000000000000000 ) ) ;
#38450 = ORIENTED_EDGE ( 'NONE', *, *, #45010, .F. ) ;
#38451 = CARTESIAN_POINT ( 'NONE',  ( 11.48443175375249048, 45.38933445805910338, -14.52341122396187423 ) ) ;
#38452 = VECTOR ( 'NONE', #5234, 1000.000000000000000 ) ;
#38453 = CARTESIAN_POINT ( 'NONE',  ( 47.06916318994454684, 18.66170694578125477, -14.79344423761990512 ) ) ;
#38454 = CARTESIAN_POINT ( 'NONE',  ( -52.60051048173597366, -60.00000000000000000, -37.38023807311972746 ) ) ;
#38455 = CARTESIAN_POINT ( 'NONE',  ( 8.143901214329899974E-15, 0.000000000000000000, -66.50000000000000000 ) ) ;
#38456 = CARTESIAN_POINT ( 'NONE',  ( -5.082755093536326818, -30.59375000204838813, 5.082755093536325042 ) ) ;
#38457 = VECTOR ( 'NONE', #91979, 1000.000000000000227 ) ;
#38458 = CARTESIAN_POINT ( 'NONE',  ( 23.93420880016849139, -4.285714285714295357, 8.127057321558249114 ) ) ;
#38459 = CARTESIAN_POINT ( 'NONE',  ( 5.000000000000000888, -40.36147667352133084, -0.7651093971659219672 ) ) ;
#38460 = CARTESIAN_POINT ( 'NONE',  ( -5.036189802311180408, 48.00000000000000000, -76.26213611587843388 ) ) ;
#38461 = CARTESIAN_POINT ( 'NONE',  ( -34.12349128637492157, 490.8027302422244134, 11.84948222508912252 ) ) ;
#38462 = CARTESIAN_POINT ( 'NONE',  ( -38.79167372577270356, 310.2940712511280026, 1.667255102746370454 ) ) ;
#38463 = CARTESIAN_POINT ( 'NONE',  ( 26.21593877366845504, 304.5184713299540817, -9.636447512346801858 ) ) ;
#38464 = VERTEX_POINT ( 'NONE', #75182 ) ;
#38465 = CARTESIAN_POINT ( 'NONE',  ( 91.37578371391791165, 5.000000000000023093, 6.123233995736781074E-16 ) ) ;
#38466 = FACE_OUTER_BOUND ( 'NONE', #30293, .T. ) ;
#38467 = CARTESIAN_POINT ( 'NONE',  ( 33.46736520451723607, -39.49419924740560361, 34.56458480083048102 ) ) ;
#38468 = CARTESIAN_POINT ( 'NONE',  ( -17.01589776168603407, -1.734723475976807094E-15, 2.227375807157432774 ) ) ;
#38469 = ORIENTED_EDGE ( 'NONE', *, *, #3634, .T. ) ;
#38470 = CARTESIAN_POINT ( 'NONE',  ( 5.975663821521392194, -7.000939006314269797, 0.8740179403729263496 ) ) ;
#38471 = EDGE_CURVE ( 'NONE', #42319, #98662, #85784, .T. ) ;
#38472 = VERTEX_POINT ( 'NONE', #50375 ) ;
#38474 = CARTESIAN_POINT ( 'NONE',  ( 45.29905483860081716, 480.9466865490944656, -2.171671249451534003 ) ) ;
#38473 = LINE ( 'NONE', #70823, #52089 ) ;
#38475 = CARTESIAN_POINT ( 'NONE',  ( 0.000000000000000000, 60.00000000000000000, 6.999999999999992895 ) ) ;
#38476 = LINE ( 'NONE', #87024, #94834 ) ;
#38477 = CARTESIAN_POINT ( 'NONE',  ( -30.00000000000000000, 0.000000000000000000, 0.000000000000000000 ) ) ;
#38478 = FACE_OUTER_BOUND ( 'NONE', #97423, .T. ) ;
#38479 = CARTESIAN_POINT ( 'NONE',  ( -48.02835407290534420, 16.78162100668604495, -14.35535821593460248 ) ) ;
#38480 = CARTESIAN_POINT ( 'NONE',  ( -44.00013453485239268, 465.7974093566494957, 11.65569858486088606 ) ) ;
#38481 = CARTESIAN_POINT ( 'NONE',  ( 95.46109593427335938, -60.00000000000002132, 52.32479805523267657 ) ) ;
#38482 = CARTESIAN_POINT ( 'NONE',  ( 28.09972863518510877, 34.19584976912102547, -9.568757885759717752 ) ) ;
#38483 = CARTESIAN_POINT ( 'NONE',  ( 19.00000000000001066, -4.000000000000000000, 25.00000000000000000 ) ) ;
#38484 = VECTOR ( 'NONE', #25808, 999.9999999999998863 ) ;
#38485 = CIRCLE ( 'NONE', #74560, 4.000000000000000888 ) ;
#38486 = DIRECTION ( 'NONE',  ( 0.000000000000000000, 0.000000000000000000, 1.000000000000000000 ) ) ;
#38487 = FACE_OUTER_BOUND ( 'NONE', #105089, .T. ) ;
#38488 = EDGE_CURVE ( 'NONE', #1105, #12701, #15151, .T. ) ;
#38489 = ORIENTED_EDGE ( 'NONE', *, *, #19941, .T. ) ;
#38490 =( GEOMETRIC_REPRESENTATION_CONTEXT ( 3 ) GLOBAL_UNCERTAINTY_ASSIGNED_CONTEXT ( ( #9291 ) ) GLOBAL_UNIT_ASSIGNED_CONTEXT ( ( #43931, #18619, #17547 ) ) REPRESENTATION_CONTEXT ( 'NONE', 'WORKASPACE' ) );
#38491 = CARTESIAN_POINT ( 'NONE',  ( -89.95007437634640723, -30.00000000001658762, -2.808103800467800948 ) ) ;
#38492 = ORIENTED_EDGE ( 'NONE', *, *, #87129, .F. ) ;
#38493 = CARTESIAN_POINT ( 'NONE',  ( 0.000000000000000000, 43.50000000000000711, 0.000000000000000000 ) ) ;
#38494 = CARTESIAN_POINT ( 'NONE',  ( 15.79700980112376918, 22.78020937716664562, 0.4986931010921795693 ) ) ;
#38495 = CARTESIAN_POINT ( 'NONE',  ( -6.500000000000000000, 2.536640449112266271, -0.3753468889000121100 ) ) ;
#38496 = CIRCLE ( 'NONE', #74635, 0.9999999999999742428 ) ;
#38497 = CARTESIAN_POINT ( 'NONE',  ( 4.401442555609581635E-16, -32.65625000204838813, -7.188101187500000044 ) ) ;
#38498 = DIRECTION ( 'NONE',  ( 0.8400944247696998657, 0.000000000000000000, 0.5424401879201679044 ) ) ;
#38499 = DIRECTION ( 'NONE',  ( 0.000000000000000000, 0.000000000000000000, -1.000000000000000000 ) ) ;
#38500 = VERTEX_POINT ( 'NONE', #18047 ) ;
#38502 = ORIENTED_EDGE ( 'NONE', *, *, #104431, .T. ) ;
#38501 = FACE_OUTER_BOUND ( 'NONE', #15709, .T. ) ;
#38503 = CARTESIAN_POINT ( 'NONE',  ( 80.71697465536873040, -32.56001387452523943, 142.8104254745445871 ) ) ;
#38504 = EDGE_CURVE ( 'NONE', #68326, #17636, #45368, .T. ) ;
#38505 = CARTESIAN_POINT ( 'NONE',  ( -38.50768004163307978, 27.33171274800497130, -13.03328602146359039 ) ) ;
#38506 = ORIENTED_EDGE ( 'NONE', *, *, #37020, .T. ) ;
#38507 = CARTESIAN_POINT ( 'NONE',  ( -12.50000000000000711, 39.48967685716225873, -64.09116616746609907 ) ) ;
#38508 = CARTESIAN_POINT ( 'NONE',  ( 7.188101187500000044, -17.65625000204838457, 0.000000000000000000 ) ) ;
#38509 = CARTESIAN_POINT ( 'NONE',  ( 11.24762705481944813, 45.31580660681511574, 14.96115168073759705 ) ) ;
#38510 = EDGE_CURVE ( 'NONE', #44939, #87130, #78906, .T. ) ;
#38511 = B_SPLINE_SURFACE_WITH_KNOTS ( 'NONE', 3, 1, ( 
 ( #77951, #5646, #48215 ),
 ( #22925, #40137, #80055 ),
 ( #64432, #14789, #73014 ),
 ( #22402, #47159, #6165 ),
 ( #55762, #55246, #104332 ),
 ( #71977, #30481, #24524 ),
 ( #80582, #23998, #7227 ),
 ( #39097, #15860, #96276 ),
 ( #57364, #79533, #88170 ),
 ( #73547, #16387, #14254 ),
 ( #105919, #97302, #23457 ),
 ( #65482, #104887, #31026 ),
 ( #90283, #6704, #98371 ),
 ( #106451, #39631, #71431 ),
 ( #63907, #96793, #64945 ),
 ( #88694, #56293, #48738 ),
 ( #47684, #105407, #32071 ),
 ( #89231, #38570, #97837 ),
 ( #89763, #81631, #7755 ),
 ( #32609, #74613, #91360 ),
 ( #83247, #68129, #90822 ),
 ( #92393, #18541, #17475 ),
 ( #34740, #25042, #16938 ),
 ( #51406, #33134, #76210 ),
 ( #9880, #42791, #59523 ),
 ( #42250, #50338, #9340 ),
 ( #693, #75141, #49816 ),
 ( #10414, #100491, #26647 ),
 ( #101025, #27179, #41729 ),
 ( #75684, #1236, #1783 ),
 ( #67611, #84317, #43329 ),
 ( #58988, #49273, #60069 ),
 ( #34206, #82721, #8825 ),
 ( #33658, #92932, #67078 ),
 ( #57898, #66537, #82177 ),
 ( #2315, #35261, #8293 ),
 ( #41199, #74085, #171 ),
 ( #66004, #50864, #98881 ),
 ( #99411, #25593, #91876 ),
 ( #99961, #58451, #18003 ),
 ( #26134, #83769, #60595 ),
 ( #70260, #93483, #20162 ),
 ( #44394, #36344, #76741 ),
 ( #20705, #102624, #69215 ),
 ( #3402, #68683, #77290 ),
 ( #28782, #101564, #35805 ),
 ( #43851, #27721, #12007 ),
 ( #77824, #53543, #86474 ),
 ( #102081, #62196, #45465 ),
 ( #28243, #21214, #12530 ),
 ( #19632, #52465, #54044 ),
 ( #94553, #84847, #78338 ),
 ( #61113, #19094, #94000 ),
 ( #95082, #4456, #37399 ),
 ( #85384, #51935, #61664 ),
 ( #2851, #10930, #11467 ),
 ( #44940, #53012, #85936 ),
 ( #3934, #36865, #69733 ),
 ( #103161, #29306, #59116 ),
 ( #33788, #33252, #58024 ),
 ( #7876, #34334, #83370 ),
 ( #8417, #73677, #67732 ),
 ( #17059, #67209, #91483 ),
 ( #106579, #24637, #66663 ),
 ( #100616, #26253, #75270 ),
 ( #83902, #59648, #57484 ),
 ( #58582, #818, #99548 ),
 ( #81754, #48861, #40783 ),
 ( #25724, #286, #50988 ),
 ( #91996, #42923, #18132 ),
 ( #90952, #65598, #90409 ),
 ( #16512, #17598, #10016 ),
 ( #75815, #66125, #9467 ),
 ( #1910, #50460, #8946 ),
 ( #49938, #42379, #74207 ),
 ( #49398, #1368, #34863 ),
 ( #100083, #26779, #15984 ),
 ( #32731, #98484, #99004 ),
 ( #82307, #41317, #25169 ),
 ( #82843, #41849, #74735 ),
 ( #36991, #61792, #68810 ),
 ( #92524, #103292, #69340 ),
 ( #19234, #93068, #27319 ),
 ( #29437, #19759, #18679 ),
 ( #68264, #51535, #84449 ),
 ( #53664, #86066, #77417 ),
 ( #10542, #94686, #20833 ),
 ( #3532, #12137, #86598 ),
 ( #43460, #36471, #2449 ),
 ( #102755, #84979, #53148 ),
 ( #76336, #77948, #76872 ),
 ( #28916, #102219, #28367 ),
 ( #27852, #35396, #101157 ),
 ( #45066, #93608, #12662 ),
 ( #60199, #101691, #44529 ),
 ( #52064, #11061, #43985 ),
 ( #2984, #61245, #94129 ),
 ( #45593, #4063, #78470 ),
 ( #35938, #60721, #52593 ),
 ( #20297, #69861, #4594 ),
 ( #85520, #11598, #37528 ),
 ( #70393, #81116, #103806 ),
 ( #63376, #54173, #47156 ),
 ( #38057, #47681, #70914 ),
 ( #105404, #38567, #21336 ),
 ( #96790, #55242, #13189 ),
 ( #62834, #80051, #64429 ),
 ( #46120, #7224, #31547 ),
 ( #48212, #63903, #40134 ),
 ( #46633, #88167, #14251 ),
 ( #31023, #73011, #79530 ),
 ( #104884, #80579, #6700 ),
 ( #71427, #105915, #97299 ),
 ( #104329, #62311, #39628 ),
 ( #23454, #87115, #96273 ),
 ( #95725, #72498, #79005 ),
 ( #56290, #22399, #95204 ),
 ( #5125, #29951, #14786 ),
 ( #89228, #15326, #6162 ),
 ( #21866, #54706, #87643 ),
 ( #13726, #5643, #30477 ),
 ( #39094, #71974, #22921 ),
 ( #55759, #88690, #16935 ),
 ( #99957, #81628, #106448 ),
 ( #40661, #8290, #7751 ),
 ( #25590, #24521, #89759 ),
 ( #16383, #33131, #83244 ),
 ( #91357, #32606, #75138 ),
 ( #42247, #9877, #32068 ),
 ( #15857, #33655, #49813 ),
 ( #50860, #82718, #57895 ),
 ( #90819, #18000, #73544 ),
 ( #74082, #42788, #66001 ),
 ( #65479, #58985, #98878 ),
 ( #8821, #49270, #98367 ),
 ( #57361, #90280, #41726 ),
 ( #48735, #91873, #82174 ),
 ( #99408, #1233, #74610 ),
 ( #167, #25038, #690 ),
 ( #66534, #41196, #58448 ),
 ( #9337, #34203, #83766 ),
 ( #17471, #50335, #67075 ),
 ( #26131, #75681, #64942 ),
 ( #97834, #23995, #56836 ),
 ( #26644, #102078, #101022 ),
 ( #84844, #60591, #69211 ),
 ( #51403, #76207, #59519 ),
 ( #52462, #93480, #86470 ),
 ( #61110, #44937, #69730 ),
 ( #43325, #19091, #44391 ),
 ( #19629, #77820, #67608 ),
 ( #27176, #43848, #12527 ),
 ( #20702, #2311, #28779 ),
 ( #100487, #85380, #92929 ),
 ( #93997, #84314, #35258 ),
 ( #3931, #92390, #61661 ),
 ( #28240, #20159, #12004 ),
 ( #101561, #76738, #2848 ),
 ( #60066, #68680, #68125 ),
 ( #3399, #53540, #51931 ),
 ( #27718, #53009, #77287 ),
 ( #11464, #85933, #36341 ),
 ( #36861, #102620, #10927 ),
 ( #94550, #35802, #45462 ),
 ( #1780, #34737, #18538 ),
 ( #10411, #88039, #4993 ),
 ( #70257, #88562, #80448 ),
 ( #4452, #21731, #78335 ),
 ( #30886, #96654, #37395 ),
 ( #64294, #79922, #63766 ),
 ( #56149, #22789, #14118 ),
 ( #14643, #70786, #38953 ),
 ( #62703, #47020, #104736 ),
 ( #55625, #103158, #71830 ),
 ( #6031, #29303, #89093 ),
 ( #63235, #37924, #78865 ),
 ( #103680, #15188, #5515 ),
 ( #54040, #86986, #62193 ),
 ( #47552, #39492, #6559 ),
 ( #96127, #95078, #72367 ),
 ( #105273, #22260, #31417 ),
 ( #21211, #97166, #23313 ),
 ( #38439, #13054, #45986 ),
 ( #54571, #29826, #95594 ),
 ( #87510, #55108, #13589 ),
 ( #46504, #79400, #71305 ),
 ( #104198, #30341, #49137 ),
 ( #57230, #56701, #24391 ),
 ( #8693, #23857, #97692 ),
 ( #105793, #89624, #98752 ),
 ( #26001, #58311, #558 ),
 ( #65873, #15724, #66949 ),
 ( #73953, #66399, #91236 ),
 ( #34077, #48608, #73411 ),
 ( #58864, #82038, #99829 ),
 ( #75008, #8162, #40010 ),
 ( #32473, #81494, #33527 ),
 ( #7613, #33006, #17343 ),
 ( #1103, #65344, #41601 ),
 ( #50218, #24906, #41069 ),
 ( #34, #31932, #91754 ),
 ( #49681, #9214, #99280 ),
 ( #48077, #80979, #7095 ),
 ( #72881, #74484, #57760 ),
 ( #83119, #25457, #42122 ),
 ( #64810, #40532, #98235 ),
 ( #90685, #16795, #106308 ),
 ( #90148, #16253, #82588 ),
 ( #2184, #52883, #68004 ),
 ( #44811, #60991, #93878 ),
 ( #67482, #26524, #76084 ),
 ( #2726, #20037, #1652 ),
 ( #35134, #85252, #11336 ),
 ( #18412, #35677, #85808 ),
 ( #34611, #36747, #11883 ),
 ( #3810, #19504, #69609 ),
 ( #100889, #43723, #69084 ),
 ( #28645, #27055, #27592 ),
 ( #59397, #101957, #9742 ),
 ( #68553, #60474, #17874 ),
 ( #101439, #93353, #51269 ),
 ( #83637, #51808, #52339 ),
 ( #3276, #42658, #28117 ),
 ( #18964, #50727, #59939 ),
 ( #102502, #77160, #36216 ),
 ( #92258, #61530, #44268 ),
 ( #75558, #100361, #77698 ),
 ( #84191, #10287, #43198 ),
 ( #92805, #84720, #10806 ),
 ( #76614, #4333, #30761 ),
 ( #5399, #4867, #29707 ),
 ( #70665, #37266, #12408 ),
 ( #86862, #45339, #39370 ),
 ( #95464, #38835, #63104 ),
 ( #94958, #63647, #78217 ),
 ( #29195, #37804, #30218 ),
 ( #38321, #96536, #53424 ),
 ( #86342, #87391, #71182 ),
 ( #22668, #103557, #55505 ),
 ( #88445, #14517, #62581 ),
 ( #103037, #45858, #47429 ),
 ( #21611, #70131, #21096 ),
 ( #13465, #62070, #96005 ),
 ( #79277, #80320, #46387 ),
 ( #6432, #72247, #104076 ),
 ( #22129, #105149, #12937 ),
 ( #54981, #71698, #87912 ),
 ( #78731, #13994, #46902 ),
 ( #104610, #53930, #79806 ),
 ( #5904, #94423, #31291 ),
 ( #20585, #54441, #64693 ),
 ( #98112, #73833, #97564 ),
 ( #56035, #74358, #66276 ),
 ( #97048, #7491, #64178 ),
 ( #968, #33407, #99164 ),
 ( #81913, #57633, #25321 ),
 ( #23189, #8029, #80859 ),
 ( #436, #56579, #24784 ),
 ( #88967, #49557, #48487 ),
 ( #6971, #58182, #40941 ),
 ( #81382, #106184, #39889 ),
 ( #72762, #15065, #90557 ),
 ( #47951, #9092, #40406 ) ),
 .UNSPECIFIED., .T., .F., .F.,
 ( 4, 1, 1, 1, 1, 1, 1, 1, 1, 1, 1, 1, 1, 1, 1, 1, 1, 1, 1, 1, 1, 1, 1, 1, 1, 1, 1, 1, 1, 1, 1, 1, 1, 1, 1, 1, 1, 1, 1, 1, 1, 1, 1, 1, 1, 1, 1, 1, 1, 1, 1, 1, 1, 1, 1, 1, 1, 1, 1, 1, 1, 1, 1, 1, 1, 1, 1, 1, 1, 1, 1, 1, 1, 1, 1, 1, 1, 1, 1, 1, 1, 1, 1, 1, 1, 1, 1, 1, 1, 1, 1, 1, 1, 1, 1, 1, 1, 1, 1, 1, 1, 1, 1, 1, 1, 1, 1, 1, 1, 1, 1, 1, 1, 1, 1, 1, 1, 1, 1, 1, 1, 1, 1, 1, 1, 1, 1, 1, 1, 1, 2, 1, 1, 1, 1, 1, 1, 1, 1, 1, 1, 1, 1, 1, 1, 1, 1, 1, 1, 1, 1, 1, 1, 1, 1, 1, 1, 1, 1, 1, 1, 1, 1, 1, 1, 1, 1, 1, 1, 1, 1, 1, 1, 1, 1, 1, 1, 1, 1, 1, 1, 1, 1, 1, 1, 1, 1, 1, 1, 1, 1, 1, 1, 1, 1, 1, 1, 1, 1, 1, 1, 1, 1, 1, 1, 1, 1, 1, 1, 1, 1, 1, 1, 1, 1, 1, 1, 1, 1, 1, 1, 1, 1, 1, 1, 1, 1, 1, 1, 1, 1, 1, 1, 1, 1, 1, 1, 1, 1, 1, 1, 1, 1, 1, 1, 1, 1, 1, 1, 1, 1, 1, 1, 1, 1, 1, 1, 1, 1, 4 ),
 ( 2, 1, 2 ),
 ( 0.000000000000000000, 0.003906146814772826562, 0.007812293629545653123, 0.01171844044431847968, 0.01562458725909130625, 0.01953073407386413107, 0.02343688088863695937, 0.02734302770340978420, 0.03124917451818261249, 0.03320224792556902144, 0.03515532133295543732, 0.03710839474034185320, 0.03906146814772826215, 0.04296761496250108697, 0.04687376177727391874, 0.05468605540681956839, 0.06249834903636522498, 0.07031064266591087464, 0.07812293629545652429, 0.08593522992500217395, 0.09374752355454783748, 0.1015598171840934594, 0.1093721108136391368, 0.1132782576284119685, 0.1171844044431848003, 0.1210905512579576043, 0.1249966980727304500, 0.1289028448875032540, 0.1328089917022760857, 0.1367151385170488620, 0.1406212853318217493, 0.1445274321465945810, 0.1484335789613673851, 0.1523397257761402168, 0.1562458725909130486, 0.1601520194056858248, 0.1640581662204587121, 0.1679643130352315439, 0.1718704598500043479, 0.1757766066647771797, 0.1796827534795499559, 0.1816358268869364412, 0.1835889002943228432, 0.1855419737017092452, 0.1874950471090956750, 0.1914011939238684790, 0.1933542673312549365, 0.1953073407386413107, 0.1992134875534140870, 0.2011665609608005445, 0.2031196343681869187, 0.2050727077755734040, 0.2060492444792665356, 0.2070257811829598060, 0.2089788545903461525, 0.2109319279977326378, 0.2128850014051190120, 0.2148380748125054418, 0.2167911482198918716, 0.2187442216272782736, 0.2206972950346647311, 0.2226503684420510498, 0.2246034418494375351, 0.2265565152568239371, 0.2285095886642103391, 0.2304626620715967689, 0.2324157354789831431, 0.2343688088863696006, 0.2363218822937560304, 0.2382749557011424046, 0.2402280291085288344, 0.2421811025159151809, 0.2441341759233016939, 0.2460872493306880127, 0.2499933961454608999, 0.2538995429602335929, 0.2578056897750065080, 0.2617118365897793675, 0.2656179834045521715, 0.2695241302193249755, 0.2734302770340977240, 0.2773364238488707501, 0.2812425706636434986, 0.2851487174784163581, 0.2890548642931891621, 0.2968671579227347701, 0.3046794515522804336, 0.3124917451818260972, 0.3203040388113716497, 0.3281163324409174242, 0.3359286260704630878, 0.3437409197000086958, 0.3476470665147816108, 0.3515532133295543593, 0.3554593601443271633, 0.3593655069590999118, 0.3632716537738728824, 0.3671778005886456864, 0.3710839474034184904, 0.3749900942181913499, 0.3788962410329640984, 0.3828023878477369579, 0.3867085346625097619, 0.3906146814772826215, 0.3945208282920554810, 0.3984269751068281740, 0.4023331219216010890, 0.4042861953289875743, 0.4062392687363738375, 0.4081923421437603228, 0.4101454155511468080, 0.4120984889585330713, 0.4140515623659196121, 0.4160046357733060973, 0.4179577091806923050, 0.4199107825880789013, 0.4218638559954652756, 0.4257700028102379686, 0.4296761496250108836, 0.4335822964397836876, 0.4374884432545565471, 0.4413945900693294067, 0.4453007368841020996, 0.4492068836988750702, 0.4531130305136478742, 0.4609253241431935377, 0.4687376177727392013, 0.4765499114022848093, 0.4843622050318303618, 0.4921744986613760253, 0.4999867922909217999, 0.5077994986613761919, 0.5156122050318305838, 0.5234249114022848648, 0.5312376177727392568, 0.5390503241431936488, 0.5468630305136479297, 0.5507693836988751812, 0.5546757368841022107, 0.5585820900693294622, 0.5624884432545566026, 0.5663947964397838541, 0.5703011496250109946, 0.5742075028102381351, 0.5781138559954652756, 0.5800670325880789013, 0.5820202091806925271, 0.5839733857733060418, 0.5859265623659195565, 0.5878797389585332933, 0.5898329155511468080, 0.5917860921437604338, 0.5937392687363740595, 0.5956924453289873522, 0.5976456219216012000, 0.6015519751068284515, 0.6054583282920554810, 0.6093646814772826215, 0.6132710346625098730, 0.6171773878477370134, 0.6210837410329641539, 0.6249900942181914054, 0.6288964474034186569, 0.6328028005886456864, 0.6367091537738729379, 0.6406155069591000784, 0.6445218601443273299, 0.6484282133295544703, 0.6523345665147814998, 0.6562409197000087513, 0.6640536260704632543, 0.6718663324409175353, 0.6796790388113718162, 0.6874917451818260972, 0.6953044515522806002, 0.7031171579227348811, 0.7109298642931891621, 0.7148362174784161915, 0.7187425706636435541, 0.7226489238488706945, 0.7265552770340979460, 0.7304616302193250865, 0.7343679834045522270, 0.7382743365897792565, 0.7421806897750065080, 0.7460870429602337595, 0.7499933961454610110, 0.7538997493306882625, 0.7558529259233015551, 0.7578061025159152919, 0.7597592791085288066, 0.7617124557011423214, 0.7636656322937560581, 0.7656188088863695729, 0.7675719854789833096, 0.7695251620715968244, 0.7714783386642103391, 0.7734315152568238538, 0.7753846918494375906, 0.7773378684420511053, 0.7792910450346646201, 0.7812442216272783568, 0.7831973982198916495, 0.7851505748125056083, 0.7871037514051189010, 0.7890569279977326378, 0.7910101045903461525, 0.7929632811829598893, 0.7949164577755734040, 0.7968696343681870298, 0.7988228109608006555, 0.8007759875534141703, 0.8046823407386413107, 0.8066355173312547144, 0.8085886939238684512, 0.8124950471090957027, 0.8144482237017094395, 0.8164014002943229542, 0.8183545768869363579, 0.8203077534795502057, 0.8242141066647772352, 0.8281204598500044867, 0.8320268130352314051, 0.8359331662204587676, 0.8398395194056857971, 0.8437458725909130486, 0.8476522257761403001, 0.8515585789613675516, 0.8554649321465945810, 0.8593712853318218325, 0.8632776385170490840, 0.8671839917022761135, 0.8710903448875033650, 0.8749966980727305055, 0.8789030512579574239, 0.8828094044431848975, 0.8867157576284119269, 0.8906221108136391784, 0.8984348171840934594, 0.9062475235545479624, 0.9140602299250022433, 0.9218729362954565243, 0.9296856426659108052, 0.9374983490363653083, 0.9453110554068195892, 0.9531237617772740922, 0.9570301149625010106, 0.9609364681477282621, 0.9628896447403418879, 0.9648428213329554026, 0.9667959979255691394, 0.9687491745181826541, 0.9726555277034099056, 0.9765618808886369351, 0.9804682340738641866, 0.9843745872590914381, 0.9882809404443185786, 0.9921872936295457190, 0.9960936468147727485, 1.000000000000000000 ),
 ( 0.000000000000000000, 1.000000000000000000, 1.526318052600188269 ),
 .UNSPECIFIED. ) ;
#38512 = CARTESIAN_POINT ( 'NONE',  ( 21.19348424345039206, 294.8901562694577478, 1.945151701991080673 ) ) ;
#38513 = ORIENTED_EDGE ( 'NONE', *, *, #10028, .T. ) ;
#38514 = B_SPLINE_CURVE_WITH_KNOTS ( 'NONE', 3,
 ( #3537, #61796, #67736, #53152 ),
 .UNSPECIFIED., .F., .F.,
 ( 4, 4 ),
 ( 0.000000000000000000, 1.000000000000000000 ),
 .UNSPECIFIED. ) ;
#38515 = CARTESIAN_POINT ( 'NONE',  ( 61.37206225042174879, 6.856755485862130937E-15, 0.000000000000000000 ) ) ;
#38516 = CARTESIAN_POINT ( 'NONE',  ( -5.650483388624515158, -13.45566596850383867, 2.031129859422142747 ) ) ;
#38517 = CARTESIAN_POINT ( 'NONE',  ( -9.699189539447123920, 81.82307771753286829, -2.444343703917209343 ) ) ;
#38518 = DIRECTION ( 'NONE',  ( 0.000000000000000000, 0.000000000000000000, -1.000000000000000000 ) ) ;
#38519 = CARTESIAN_POINT ( 'NONE',  ( -8.000000000000001776, -13.34375000409676915, 3.313708498984758943 ) ) ;
#38520 = CARTESIAN_POINT ( 'NONE',  ( -19.84524846389541963, -17.03792638373621671, 31.48019177038823102 ) ) ;
#38521 = PRESENTATION_STYLE_ASSIGNMENT (( #102707 ) ) ;
#38522 = VECTOR ( 'NONE', #66694, 1000.000000000000000 ) ;
#38523 = FACE_OUTER_BOUND ( 'NONE', #96393, .T. ) ;
#38524 = CARTESIAN_POINT ( 'NONE',  ( 7.500000000000003553, -0.03736385522455209357, -23.73594627047615901 ) ) ;
#38525 = CARTESIAN_POINT ( 'NONE',  ( 8.000000000000000000, -19.90624999999999289, -3.313708498984761164 ) ) ;
#38526 =( GEOMETRIC_REPRESENTATION_CONTEXT ( 3 ) GLOBAL_UNCERTAINTY_ASSIGNED_CONTEXT ( ( #51020 ) ) GLOBAL_UNIT_ASSIGNED_CONTEXT ( ( #22106, #56008, #54961 ) ) REPRESENTATION_CONTEXT ( 'NONE', 'WORKASPACE' ) );
#38528 = EDGE_CURVE ( 'NONE', #82654, #26677, #51449, .T. ) ;
#38527 = PRODUCT_CONTEXT ( 'NONE', #36304, 'mechanical' ) ;
#38529 = CARTESIAN_POINT ( 'NONE',  ( -12.06878958996594164, -6.474301304373300425, 19.90239611026824562 ) ) ;
#38530 = VERTEX_POINT ( 'NONE', #67652 ) ;
#38531 = CARTESIAN_POINT ( 'NONE',  ( 11.48415166351361627, 43.26076767676408963, 14.52437360466608141 ) ) ;
#38532 = LINE ( 'NONE', #22362, #9508 ) ;
#38533 = CYLINDRICAL_SURFACE ( 'NONE', #42820, 4.000000000000000000 ) ;
#38534 = CARTESIAN_POINT ( 'NONE',  ( 9.416339274345753907, -18.52858867495709561, -37.89033340655316806 ) ) ;
#38535 = CARTESIAN_POINT ( 'NONE',  ( -83.25245042638346149, -30.00000000000000000, 154.8156864715076892 ) ) ;
#38536 = VERTEX_POINT ( 'NONE', #100530 ) ;
#38537 = CARTESIAN_POINT ( 'NONE',  ( 33.58349330513379982, 4.000000000000002665, 0.000000000000000000 ) ) ;
#38538 = STYLED_ITEM ( 'NONE', ( #68741 ), #21784 ) ;
#38539 = CARTESIAN_POINT ( 'NONE',  ( 107.6567483471291524, -57.65797727960799079, 199.3974509801145416 ) ) ;
#38540 = CARTESIAN_POINT ( 'NONE',  ( 70.85504447565058683, -60.22828372538490527, -26.05905046828224769 ) ) ;
#38541 = DIRECTION ( 'NONE',  ( -1.000000000000000000, -0.000000000000000000, -0.000000000000000000 ) ) ;
#38542 = CARTESIAN_POINT ( 'NONE',  ( -15.79338834186285290, 22.74219270459669318, 1.000334277921258508 ) ) ;
#38543 = CARTESIAN_POINT ( 'NONE',  ( 58.90678327781098034, 40.83906611471667958, -28.11551192243881658 ) ) ;
#38544 = CARTESIAN_POINT ( 'NONE',  ( -74.81545634040968196, -60.00000000000000000, 179.8313476602450862 ) ) ;
#38545 = DIRECTION ( 'NONE',  ( -1.000000000000000000, -1.224606353822377258E-16, -0.000000000000000000 ) ) ;
#38546 = DIRECTION ( 'NONE',  ( -0.000000000000000000, -0.000000000000000000, -1.000000000000000000 ) ) ;
#38547 = CARTESIAN_POINT ( 'NONE',  ( -55.22048556080422799, 49.99999999999999289, 34.80214219305234025 ) ) ;
#38548 = CARTESIAN_POINT ( 'NONE',  ( -85.95813120774067784, -31.98553129542242601, 183.6009373032548524 ) ) ;
#38550 = VERTEX_POINT ( 'NONE', #59566 ) ;
#38549 = AXIS2_PLACEMENT_3D ( 'NONE', #68762, #93012, #72316 ) ;
#38551 = CARTESIAN_POINT ( 'NONE',  ( 32.65439066521594924, 316.1413580166883435, -7.048974138691598945 ) ) ;
#38552 =( BOUNDED_CURVE ( )  B_SPLINE_CURVE ( 2, ( #66700, #98523, #24670, #90443, #16554, #49437, #74248, #99041, #25209 ),
 .UNSPECIFIED., .F., .F. ) 
 B_SPLINE_CURVE_WITH_KNOTS ( ( 3, 2, 2, 2, 3 ),
 ( 0.1911764705882352811, 0.1985294117647058709, 0.2058823529411764608, 0.2132352941176470784, 0.2205882352941176683 ),
 .UNSPECIFIED. ) 
 CURVE ( )  GEOMETRIC_REPRESENTATION_ITEM ( )  RATIONAL_B_SPLINE_CURVE ( ( 1.000000000000000000, 0.9238795325112867385, 1.000000000000000000, 0.9238795325112867385, 1.000000000000000000, 0.9238795325112867385, 1.000000000000000000, 0.9238795325112864054, 1.000000000000000222 ) ) 
 REPRESENTATION_ITEM ( '' )  );
#38553 = VECTOR ( 'NONE', #42304, 1000.000000000000000 ) ;
#38554 = DIRECTION ( 'NONE',  ( 0.000000000000000000, -1.000000000000000000, 0.000000000000000000 ) ) ;
#38555 = EDGE_CURVE ( 'NONE', #82973, #88610, #35841, .T. ) ;
#38556 = CARTESIAN_POINT ( 'NONE',  ( -30.22241138358163326, 310.0030499099321446, -8.579635021166650333 ) ) ;
#38557 =( GEOMETRIC_REPRESENTATION_CONTEXT ( 3 ) GLOBAL_UNCERTAINTY_ASSIGNED_CONTEXT ( ( #3032 ) ) GLOBAL_UNIT_ASSIGNED_CONTEXT ( ( #5940, #86377, #28152 ) ) REPRESENTATION_CONTEXT ( 'NONE', 'WORKASPACE' ) );
#38558 = CARTESIAN_POINT ( 'NONE',  ( -84.22227036138077949, -52.73149474305196094, -14.85135597291962029 ) ) ;
#38559 = CYLINDRICAL_SURFACE ( 'NONE', #8058, 4.000000000000000000 ) ;
#38560 = FACE_OUTER_BOUND ( 'NONE', #20497, .T. ) ;
#38561 = CIRCLE ( 'NONE', #4055, 4.000000000000000888 ) ;
#38562 = ORIENTED_EDGE ( 'NONE', *, *, #24932, .T. ) ;
#38563 = CARTESIAN_POINT ( 'NONE',  ( 18.48458798779867607, 50.00000000000001421, 61.27751401116201890 ) ) ;
#38564 = ADVANCED_FACE ( 'NONE', ( #84891 ), #50617, .F. ) ;
#38565 = CARTESIAN_POINT ( 'NONE',  ( -3.093157300003891219, -6.874418838041296276, -7.169286865560398070E-15 ) ) ;
#38566 = CARTESIAN_POINT ( 'NONE',  ( 43.88846153846154152, 1.411358822780289120E-15, 0.000000000000000000 ) ) ;
#38567 = CARTESIAN_POINT ( 'NONE',  ( 89.36652584573501201, -30.00000000000001421, 5.436425775551051665 ) ) ;
#38568 = CARTESIAN_POINT ( 'NONE',  ( -78.92481610133761194, -46.43807971556969960, 146.4481032322226497 ) ) ;
#38569 = ORIENTED_EDGE ( 'NONE', *, *, #6251, .F. ) ;
#38570 = CARTESIAN_POINT ( 'NONE',  ( 51.40679407232553899, -29.99999999999998934, 68.09281640667435909 ) ) ;
#38571 = CARTESIAN_POINT ( 'NONE',  ( -5.600000207755311266, -12.35529564071044994, -12.99999999999999112 ) ) ;
#38572 = CARTESIAN_POINT ( 'NONE',  ( 101.8003409713441840, -57.63152670329829874, 203.3526965820661587 ) ) ;
#38573 = CARTESIAN_POINT ( 'NONE',  ( 31.81093863508777630, 310.9010134536062537, -8.120521125203326918 ) ) ;
#38574 = CARTESIAN_POINT ( 'NONE',  ( 4.165977904505308693, 16.00000000000000000, 9.090909090909091717 ) ) ;
#38575 = ORIENTED_EDGE ( 'NONE', *, *, #76359, .T. ) ;
#38576 = CARTESIAN_POINT ( 'NONE',  ( 7.500000000000000000, 1.489914625144004523, -0.1187923833806734525 ) ) ;
#38577 = CARTESIAN_POINT ( 'NONE',  ( 31.62259664290086647, 439.0130977130161227, 23.39453342550511294 ) ) ;
#38579 = CARTESIAN_POINT ( 'NONE',  ( -103.9369005074886729, -45.26540285949483433, 168.0494633293456559 ) ) ;
#38578 = CARTESIAN_POINT ( 'NONE',  ( -15.41108402501092201, 43.84921859367801034, -89.31326227421881470 ) ) ;
#38580 = CARTESIAN_POINT ( 'NONE',  ( 7.188101187500000044, -22.15625000204838457, 0.000000000000000000 ) ) ;
#38581 = DIRECTION ( 'NONE',  ( 1.000000000000000000, -0.000000000000000000, -0.000000000000000000 ) ) ;
#38582 = DIRECTION ( 'NONE',  ( -1.000000000000000000, -0.000000000000000000, -0.000000000000000000 ) ) ;
#38583 = CARTESIAN_POINT ( 'NONE',  ( 7.048357505843847903, 41.75164249415616524, -68.91429206277067010 ) ) ;
#38584 = CARTESIAN_POINT ( 'NONE',  ( 0.000000000000000000, 6.123233995736767268E-16, -5.000000000000000888 ) ) ;
#38585 = DIRECTION ( 'NONE',  ( 0.000000000000000000, 0.000000000000000000, 1.000000000000000000 ) ) ;
#38586 = PRESENTATION_LAYER_ASSIGNMENT (  '', '', ( #9289 ) ) ;
#38587 = CARTESIAN_POINT ( 'NONE',  ( 0.000000000000000000, -14.49999999999999822, 0.000000000000000000 ) ) ;
#38588 = VERTEX_POINT ( 'NONE', #93526 ) ;
#38589 = DIRECTION ( 'NONE',  ( -0.5735764363510461594, 0.8191520442889916875, 1.003171929053524870E-16 ) ) ;
#38591 = CARTESIAN_POINT ( 'NONE',  ( 25.97097906841934289, -36.00028574033248674, 31.37664239582928261 ) ) ;
#38590 = CARTESIAN_POINT ( 'NONE',  ( -13.38090213880806978, -54.00000000000000711, 31.11721482942554928 ) ) ;
#38592 = DIRECTION ( 'NONE',  ( -1.000000000000000000, -1.224606353822377258E-16, -0.000000000000000000 ) ) ;
#38593 = ORIENTED_EDGE ( 'NONE', *, *, #54812, .F. ) ;
#38594 = ADVANCED_FACE ( 'NONE', ( #69777 ), #32255, .F. ) ;
#38595 = UNCERTAINTY_MEASURE_WITH_UNIT (LENGTH_MEASURE( 1.000000000000000082E-05 ), #3642, 'distance_accuracy_value', 'NONE');
#38596 = ORIENTED_EDGE ( 'NONE', *, *, #77790, .T. ) ;
#38598 = SURFACE_STYLE_FILL_AREA ( #77450 ) ;
#38597 = CARTESIAN_POINT ( 'NONE',  ( 51.01037695545453232, 450.0000000000002274, 13.20242257375370976 ) ) ;
#38599 = DIRECTION ( 'NONE',  ( -1.000000000000000000, -1.224606353822377258E-16, -0.000000000000000000 ) ) ;
#38600 = DIRECTION ( 'NONE',  ( -1.000000000000000000, -1.224606353822377258E-16, -0.000000000000000000 ) ) ;
#38601 = CIRCLE ( 'NONE', #41955, 7.000000000000006217 ) ;
#38602 = DIRECTION ( 'NONE',  ( -0.1804394941703459376, -0.5071212677064720342, 0.8427749455123416666 ) ) ;
#38603 = CARTESIAN_POINT ( 'NONE',  ( 13.64462615244698540, 1.169661571067718731, 14.95672857179070725 ) ) ;
#38604 =( NAMED_UNIT ( * ) PLANE_ANGLE_UNIT ( ) SI_UNIT ( $, .RADIAN. ) );
#38605 = EDGE_LOOP ( 'NONE', ( #32885, #38596, #74757, #17044, #100150, #11406 ) ) ;
#38606 = EDGE_CURVE ( 'NONE', #73965, #77684, #99525, .T. ) ;
#38607 = CARTESIAN_POINT ( 'NONE',  ( -7.000000000000000000, -14.21727251091160404, 9.320362779991915758 ) ) ;
#38608 = CARTESIAN_POINT ( 'NONE',  ( 89.51307813876950092, -29.99999999999982947, 189.3934310507934242 ) ) ;
#38609 = CARTESIAN_POINT ( 'NONE',  ( -12.84988518786640199, 23.41409974762299484, 4.906243843517776426 ) ) ;
#38610 = AXIS2_PLACEMENT_3D ( 'NONE', #14277, #96813, #47176 ) ;
#38611 = CARTESIAN_POINT ( 'NONE',  ( -0.000000000000000000, 61.49999999999999289, -8.160374191332742555 ) ) ;
#38612 = CARTESIAN_POINT ( 'NONE',  ( 81.47646419641506554, -30.00000000000000355, -9.428529028395711720 ) ) ;
#38613 = AXIS2_PLACEMENT_3D ( 'NONE', #23458, #29442, #54178 ) ;
#38614 = DIRECTION ( 'NONE',  ( 0.000000000000000000, -1.000000000000000000, 0.000000000000000000 ) ) ;
#38615 = EDGE_CURVE ( 'NONE', #56862, #12958, #71737, .T. ) ;
#38616 = ORIENTED_EDGE ( 'NONE', *, *, #7117, .T. ) ;
#38617 = ORIENTED_EDGE ( 'NONE', *, *, #71269, .F. ) ;
#38618 = ORIENTED_EDGE ( 'NONE', *, *, #81851, .T. ) ;
#38619 = CARTESIAN_POINT ( 'NONE',  ( 102.6464385083043283, 5.000000000000021316, 0.000000000000000000 ) ) ;
#38620 = CARTESIAN_POINT ( 'NONE',  ( 64.29999999999999716, 6.915964383211875250E-15, 0.000000000000000000 ) ) ;
#38621 = DIRECTION ( 'NONE',  ( -1.000000000000000000, -0.000000000000000000, -0.000000000000000000 ) ) ;
#38622 = CARTESIAN_POINT ( 'NONE',  ( -43.58191388046994774, 439.3921676197703050, 13.97026443796441875 ) ) ;
#38623 = CARTESIAN_POINT ( 'NONE',  ( 6.999999999999993783, -4.000000000000005329, 102.2532056551910387 ) ) ;
#38624 = CARTESIAN_POINT ( 'NONE',  ( 88.20199406385988539, 1.030564683017419500E-14, 0.000000000000000000 ) ) ;
#38625 = CARTESIAN_POINT ( 'NONE',  ( 43.63899620156487202, 434.3182181978403946, 14.37213632273145336 ) ) ;
#38626 = EDGE_LOOP ( 'NONE', ( #8888, #56651, #30598, #2101 ) ) ;
#38627 = CARTESIAN_POINT ( 'NONE',  ( -2.617478844990583031, 48.00000000000000000, -75.26027323389584467 ) ) ;
#38628 = VERTEX_POINT ( 'NONE', #11510 ) ;
#38629 = FACE_OUTER_BOUND ( 'NONE', #8588, .T. ) ;
#38630 = SURFACE_STYLE_FILL_AREA ( #79069 ) ;
#38631 = CARTESIAN_POINT ( 'NONE',  ( -40.83852310120926887, 485.7816305618699175, -4.779469532615789440 ) ) ;
#38632 = CARTESIAN_POINT ( 'NONE',  ( 6.463344223170843783, -7.245769408789104027, -1.129975644293424786 ) ) ;
#38633 = CARTESIAN_POINT ( 'NONE',  ( 63.22564189622978148, -36.00690027551169692, 79.28506037756856983 ) ) ;
#38634 = AXIS2_PLACEMENT_3D ( 'NONE', #89966, #72710, #39311 ) ;
#38635 = ORIENTED_EDGE ( 'NONE', *, *, #36578, .F. ) ;
#38636 = CARTESIAN_POINT ( 'NONE',  ( 38.21362991493155192, 463.7316259062602626, 19.26248154875775143 ) ) ;
#38637 = DIRECTION ( 'NONE',  ( 1.000000000000000000, 0.000000000000000000, 0.000000000000000000 ) ) ;
#38638 = CARTESIAN_POINT ( 'NONE',  ( 43.00000000000000000, 461.9428920847649920, 12.03309428281479576 ) ) ;
#38639 = AXIS2_PLACEMENT_3D ( 'NONE', #78540, #94208, #62907 ) ;
#38640 =( NAMED_UNIT ( * ) SI_UNIT ( $, .STERADIAN. ) SOLID_ANGLE_UNIT ( ) );
#38641 = ADVANCED_FACE ( 'NONE', ( #80360 ), #35748, .T. ) ;
#38642 = VERTEX_POINT ( 'NONE', #76524 ) ;
#38643 = CARTESIAN_POINT ( 'NONE',  ( 47.77471032523678218, 17.34854710534463962, 14.37330285161466392 ) ) ;
#38644 = DIRECTION ( 'NONE',  ( -0.000000000000000000, 0.000000000000000000, 1.000000000000000000 ) ) ;
#38645 = ADVANCED_FACE ( 'NONE', ( #2635 ), #104695, .T. ) ;
#38646 = DIRECTION ( 'NONE',  ( 0.000000000000000000, -1.000000000000000000, 0.000000000000000000 ) ) ;
#38647 = CARTESIAN_POINT ( 'NONE',  ( 3.313708498984762496, -27.96875000409677980, 7.999999999999998224 ) ) ;
#38648 = SURFACE_STYLE_USAGE ( .BOTH. , #64508 ) ;
#38649 = CARTESIAN_POINT ( 'NONE',  ( 86.30952536086155646, -53.79458929396566447, 192.2603334925355512 ) ) ;
#38650 = CARTESIAN_POINT ( 'NONE',  ( -5.221097366536865181, 6.947291620979282101, -27.42108746706259836 ) ) ;
#38651 = CARTESIAN_POINT ( 'NONE',  ( -9.946294134353090399, 7.586021175265231342, 5.000000000000000888 ) ) ;
#38652 = CARTESIAN_POINT ( 'NONE',  ( 7.002619243997877163, -8.949926819861829586, -3.868708944012998696 ) ) ;
#38653 = EDGE_CURVE ( 'NONE', #17301, #11843, #77136, .T. ) ;
#38654 = ORIENTED_EDGE ( 'NONE', *, *, #29665, .F. ) ;
#38655 = CARTESIAN_POINT ( 'NONE',  ( 13.77150638301485941, -50.98655578268471089, 24.47399976921181519 ) ) ;
#38656 = DIRECTION ( 'NONE',  ( 0.000000000000000000, -0.000000000000000000, 1.000000000000000000 ) ) ;
#38657 = CARTESIAN_POINT ( 'NONE',  ( 21.29363090902129230, -60.00000000000000711, 40.40473236666584711 ) ) ;
#38658 = CARTESIAN_POINT ( 'NONE',  ( -99.43898474115941610, -30.00000000000000355, 187.6907289620029076 ) ) ;
#38659 = LINE ( 'NONE', #96879, #100265 ) ;
#38660 = CARTESIAN_POINT ( 'NONE',  ( 45.08640801759163708, -57.68306945118310125, 65.34958374638743805 ) ) ;
#38662 = DIRECTION ( 'NONE',  ( 0.000000000000000000, -1.000000000000000000, 0.000000000000000000 ) ) ;
#38661 = DIRECTION ( 'NONE',  ( 0.000000000000000000, -1.000000000000000000, 0.000000000000000000 ) ) ;
#38663 = CARTESIAN_POINT ( 'NONE',  ( -28.49160854680623700, 41.56004624539016845, -71.33051414923416189 ) ) ;
#38664 = CARTESIAN_POINT ( 'NONE',  ( -17.84986807784454044, 49.99999999999999289, 62.10144122030740022 ) ) ;
#38665 = SURFACE_STYLE_FILL_AREA ( #21961 ) ;
#38666 = CARTESIAN_POINT ( 'NONE',  ( 3.567823017641492012, -0.9316928131313192418, 103.5075034329448158 ) ) ;
#38667 = CARTESIAN_POINT ( 'NONE',  ( -17.49999999999995381, 51.54267222161957562, 62.45775632501238306 ) ) ;
#38668 = CIRCLE ( 'NONE', #90385, 3.309500000000001663 ) ;
#38669 = AXIS2_PLACEMENT_3D ( 'NONE', #15438, #48328, #47272 ) ;
#38670 = CARTESIAN_POINT ( 'NONE',  ( 0.000000000000000000, 0.000000000000000000, -3.432199999999999918 ) ) ;
#38671 = CARTESIAN_POINT ( 'NONE',  ( -10.00000000000000000, -15.00000000000000000, 10.00000000000000178 ) ) ;
#38672 = B_SPLINE_CURVE_WITH_KNOTS ( 'NONE', 3,
 ( #61053, #102565, #85873, #12998, #68622, #27119 ),
 .UNSPECIFIED., .F., .F.,
 ( 4, 2, 4 ),
 ( 0.003981881017442815036, 0.005970145066490141136, 0.007958409115537466369 ),
 .UNSPECIFIED. ) ;
#38673 = ORIENTED_EDGE ( 'NONE', *, *, #83718, .T. ) ;
#38674 = CARTESIAN_POINT ( 'NONE',  ( 17.50000000000392220, 50.01864923522649065, 61.58301093894417022 ) ) ;
#38675 = CARTESIAN_POINT ( 'NONE',  ( -13.27553105007237733, -25.54993549698307476, 28.22271134896314848 ) ) ;
#38677 = CARTESIAN_POINT ( 'NONE',  ( -35.53540878342338516, 439.9360873049408838, 24.32554890336280806 ) ) ;
#38676 = CARTESIAN_POINT ( 'NONE',  ( -106.4794109352461788, -59.99999999999998579, 170.5660833250976793 ) ) ;
#38678 = EDGE_CURVE ( 'NONE', #33126, #4002, #13376, .T. ) ;
#38679 = VERTEX_POINT ( 'NONE', #101870 ) ;
#38680 = CARTESIAN_POINT ( 'NONE',  ( 26.94507904750826555, 34.81440208126156932, 7.556984339685686614 ) ) ;
#38681 = DIRECTION ( 'NONE',  ( -1.000000000000000000, -0.000000000000000000, -0.000000000000000000 ) ) ;
#38682 = FACE_OUTER_BOUND ( 'NONE', #6115, .T. ) ;
#38683 = EDGE_CURVE ( 'NONE', #35975, #14419, #64644, .T. ) ;
#38684 = DIRECTION ( 'NONE',  ( 0.000000000000000000, 1.000000000000000000, 0.000000000000000000 ) ) ;
#38685 = CARTESIAN_POINT ( 'NONE',  ( 65.83830346953287460, -59.99999999999999289, 121.7195788828446297 ) ) ;
#38686 = CARTESIAN_POINT ( 'NONE',  ( -44.43774958859658142, 337.2802145563449017, 0.2445019049555710311 ) ) ;
#38687 = ORIENTED_EDGE ( 'NONE', *, *, #98491, .T. ) ;
#38688 = FACE_OUTER_BOUND ( 'NONE', #8556, .T. ) ;
#38689 = CYLINDRICAL_SURFACE ( 'NONE', #57572, 3.400000000000000355 ) ;
#38691 = DIRECTION ( 'NONE',  ( 1.000000000000000000, -0.000000000000000000, -0.000000000000000000 ) ) ;
#38690 = CARTESIAN_POINT ( 'NONE',  ( 34.60434289261801410, -60.00000000000002842, 49.20687062438629056 ) ) ;
#38692 = CARTESIAN_POINT ( 'NONE',  ( 3.021265037602215209, 104.3213281748178360, -4.999999999999999112 ) ) ;
#38693 = CARTESIAN_POINT ( 'NONE',  ( -43.49286403356592956, 484.8086342565612767, 4.190194857772802095 ) ) ;
#38694 = ORIENTED_EDGE ( 'NONE', *, *, #34779, .T. ) ;
#38695 = CONICAL_SURFACE ( 'NONE', #11103, 5.000000000000001776, 0.9599310885968803664 ) ;
#38696 = ORIENTED_EDGE ( 'NONE', *, *, #2460, .T. ) ;
#38697 = CARTESIAN_POINT ( 'NONE',  ( -26.01452734666768762, 309.4082761259522840, 11.00913782773181104 ) ) ;
#38698 = ORIENTED_EDGE ( 'NONE', *, *, #46079, .T. ) ;
#38699 = CARTESIAN_POINT ( 'NONE',  ( 20.19576726783346032, 303.8497611245961707, 9.936565449087714441 ) ) ;
#38700 =( GEOMETRIC_REPRESENTATION_CONTEXT ( 3 ) GLOBAL_UNCERTAINTY_ASSIGNED_CONTEXT ( ( #100917 ) ) GLOBAL_UNIT_ASSIGNED_CONTEXT ( ( #53990, #19574, #94492 ) ) REPRESENTATION_CONTEXT ( 'NONE', 'WORKASPACE' ) );
#38701 = DIRECTION ( 'NONE',  ( -0.000000000000000000, -1.000000000000000000, -0.000000000000000000 ) ) ;
#38702 = EDGE_LOOP ( 'NONE', ( #44361, #8129, #51771, #58147 ) ) ;
#38703 = EDGE_CURVE ( 'NONE', #105180, #18064, #70300, .T. ) ;
#38704 = CARTESIAN_POINT ( 'NONE',  ( -9.742555539022085043, 7.313362239096417916, -1.762132461011677309 ) ) ;
#38705 = AXIS2_PLACEMENT_3D ( 'NONE', #72699, #16057, #65678 ) ;
#38706 = CARTESIAN_POINT ( 'NONE',  ( -106.7905710028713457, -60.00000000000244427, 200.8526573591231283 ) ) ;
#38707 = CARTESIAN_POINT ( 'NONE',  ( 44.15550912980668841, 485.1924980653485591, 0.8858017399470232700 ) ) ;
#38708 = CARTESIAN_POINT ( 'NONE',  ( 93.74589095632293834, -59.99999999999995737, 202.5411262228464295 ) ) ;
#38709 = CARTESIAN_POINT ( 'NONE',  ( 43.75401118688382951, 486.3173572309547694, 5.908089951475070656 ) ) ;
#38710 = LINE ( 'NONE', #7369, #77896 ) ;
#38712 = CARTESIAN_POINT ( 'NONE',  ( 9.249740279238880092, -42.95370826011391330, 31.05136486455132072 ) ) ;
#38711 = CARTESIAN_POINT ( 'NONE',  ( -103.2977232915219048, -14.21045842199428577, 133.3115090881459253 ) ) ;
#38713 = DIRECTION ( 'NONE',  ( 0.000000000000000000, 0.000000000000000000, 1.000000000000000000 ) ) ;
#38714 = CARTESIAN_POINT ( 'NONE',  ( -46.32777947467088353, -46.44406913752303723, 47.27782089263724430 ) ) ;
#38715 = CARTESIAN_POINT ( 'NONE',  ( 3.347764182284693746, -69.92877180609107768, 13.40431717882780305 ) ) ;
#38716 = ORIENTED_EDGE ( 'NONE', *, *, #31386, .F. ) ;
#38717 = CARTESIAN_POINT ( 'NONE',  ( 42.00498316483407280, 460.5526920487831148, 2.538979661986996650 ) ) ;
#38718 = B_SPLINE_CURVE_WITH_KNOTS ( 'NONE', 3,
 ( #52757, #85677, #51148, #11754, #74886, #972, #99713, #25884, #58742, #86747, #46270, #22012, #38207, #103957 ),
 .UNSPECIFIED., .F., .F.,
 ( 4, 2, 2, 2, 2, 2, 4 ),
 ( 3.758192634394940486E-15, 0.0005542516808482931797, 0.001108503361692828298, 0.001385629202115091357, 0.001662755042537354417, 0.001939880882959617477, 0.002217006723381880536 ),
 .UNSPECIFIED. ) ;
#38719 = CYLINDRICAL_SURFACE ( 'NONE', #85738, 1.249999999999999334 ) ;
#38720 = DIRECTION ( 'NONE',  ( -0.000000000000000000, 1.000000000000000000, -0.000000000000000000 ) ) ;
#38721 = ORIENTED_EDGE ( 'NONE', *, *, #39569, .F. ) ;
#38722 = CARTESIAN_POINT ( 'NONE',  ( -4.150157478975854630, -8.979899373663997153, 13.48960253578191981 ) ) ;
#38723 = EDGE_CURVE ( 'NONE', #44784, #79740, #45657, .T. ) ;
#38724 = ORIENTED_EDGE ( 'NONE', *, *, #80375, .T. ) ;
#38725 = CARTESIAN_POINT ( 'NONE',  ( 106.2411241248946254, -29.99999999999826628, 193.3566646931754462 ) ) ;
#38726 = DIRECTION ( 'NONE',  ( 0.5735764363510554853, 0.8191520442889852482, 0.000000000000000000 ) ) ;
#38727 = CARTESIAN_POINT ( 'NONE',  ( 0.7145311798161605443, -4.618802153517258979, -8.000000000000001776 ) ) ;
#38728 = CARTESIAN_POINT ( 'NONE',  ( -29.87930712590254245, 10.71892156097790583, 14.93965356295128011 ) ) ;
#38729 = CARTESIAN_POINT ( 'NONE',  ( 98.72935129347025907, -30.00000000000000355, 189.4299880434703880 ) ) ;
#38730 = EDGE_CURVE ( 'NONE', #21786, #77143, #53215, .T. ) ;
#38731 = ORIENTED_EDGE ( 'NONE', *, *, #57664, .T. ) ;
#38732 = VECTOR ( 'NONE', #36114, 1000.000000000000000 ) ;
#38733 = VERTEX_POINT ( 'NONE', #85594 ) ;
#38734 = ORIENTED_EDGE ( 'NONE', *, *, #85769, .F. ) ;
#38735 = CARTESIAN_POINT ( 'NONE',  ( -28.20057399694874078, 36.30547655367008275, 9.431994021286264740 ) ) ;
#38736 = DIRECTION ( 'NONE',  ( 0.000000000000000000, 0.000000000000000000, 1.000000000000000000 ) ) ;
#38737 = CARTESIAN_POINT ( 'NONE',  ( 19.36103579130787367, 294.6347466944262692, -10.04613669444748503 ) ) ;
#38738 = ORIENTED_EDGE ( 'NONE', *, *, #81699, .F. ) ;
#38739 = CARTESIAN_POINT ( 'NONE',  ( -16.03926360544215157, 4.449054639247318477, -3.142406330834766948 ) ) ;
#38740 = ORIENTED_EDGE ( 'NONE', *, *, #23177, .F. ) ;
#38741 = CARTESIAN_POINT ( 'NONE',  ( 1.714505518806294638E-15, -80.00000000000000000, 13.00000000000000000 ) ) ;
#38742 = CARTESIAN_POINT ( 'NONE',  ( 94.05478402017182304, -38.49234810551472918, 201.1946758962800459 ) ) ;
#38743 = CARTESIAN_POINT ( 'NONE',  ( 12.55213272931464275, 5.188451237610401279, 8.093010545847016957 ) ) ;
#38744 = CIRCLE ( 'NONE', #52495, 8.000000000000000000 ) ;
#38745 = CARTESIAN_POINT ( 'NONE',  ( 86.93632132420292180, -60.21781714147697784, -9.632118793199575535 ) ) ;
#38746 = DIRECTION ( 'NONE',  ( -0.000000000000000000, 0.000000000000000000, -1.000000000000000000 ) ) ;
#38747 = CIRCLE ( 'NONE', #18110, 1.000000000000000888 ) ;
#38748 = CARTESIAN_POINT ( 'NONE',  ( 40.67681791045112760, 323.6015846532498585, 8.948094541999738638 ) ) ;
#38749 = DIRECTION ( 'NONE',  ( -1.000000000000000000, 0.000000000000000000, 0.000000000000000000 ) ) ;
#38750 = CIRCLE ( 'NONE', #30134, 3.309500000000001663 ) ;
#38751 = DIRECTION ( 'NONE',  ( -1.000000000000000000, -1.224606353822377258E-16, -0.000000000000000000 ) ) ;
#38752 = PRESENTATION_LAYER_ASSIGNMENT (  '', '', ( #85233 ) ) ;
#38753 = CARTESIAN_POINT ( 'NONE',  ( -40.21064024340174115, 459.8708642436288301, 1.907892319917269486 ) ) ;
#38754 = CARTESIAN_POINT ( 'NONE',  ( -4.051286199644060559, -48.60127012969240923, 103.8758286790404952 ) ) ;
#38755 = ORIENTED_EDGE ( 'NONE', *, *, #88383, .F. ) ;
#38756 = DIRECTION ( 'NONE',  ( 0.000000000000000000, 0.000000000000000000, 1.000000000000000000 ) ) ;
#38757 = EDGE_CURVE ( 'NONE', #84082, #78054, #51844, .T. ) ;
#38758 = LINE ( 'NONE', #12857, #16816 ) ;
#38759 = CARTESIAN_POINT ( 'NONE',  ( 6.249999999999998224, 0.000000000000000000, 8.000000000000000000 ) ) ;
#38760 = EDGE_LOOP ( 'NONE', ( #65423, #74385, #56361, #45515 ) ) ;
#38761 = CARTESIAN_POINT ( 'NONE',  ( -35.45036406932566564, 436.3203772529605544, 5.179456583033978490 ) ) ;
#38762 = CARTESIAN_POINT ( 'NONE',  ( -31.50862643367105775, 299.7654595037400327, 11.04213083294634146 ) ) ;
#38763 = LINE ( 'NONE', #72698, #14007 ) ;
#38764 = UNCERTAINTY_MEASURE_WITH_UNIT (LENGTH_MEASURE( 1.000000000000000082E-05 ), #93981, 'distance_accuracy_value', 'NONE');
#38765 = SURFACE_STYLE_USAGE ( .BOTH. , #61450 ) ;
#38766 = CARTESIAN_POINT ( 'NONE',  ( -8.000000000000000000, -17.84374999999999289, -3.313708498984762496 ) ) ;
#38767 = CARTESIAN_POINT ( 'NONE',  ( -8.532132811034937703, -15.83874480131545326, 34.63122062129517076 ) ) ;
#38768 = EDGE_CURVE ( 'NONE', #21366, #68926, #36539, .T. ) ;
#38769 = EDGE_LOOP ( 'NONE', ( #70007, #42502, #36455, #52622, #59771 ) ) ;
#38770 = CARTESIAN_POINT ( 'NONE',  ( 86.40302239653674121, -17.55444326215376094, 177.8619036970834486 ) ) ;
#38771 = CARTESIAN_POINT ( 'NONE',  ( -38.80477841475464373, 27.34308269247116741, 12.01489659479609351 ) ) ;
#38772 = CARTESIAN_POINT ( 'NONE',  ( 3.867083106918059787, -1.182498200942901256, 103.9715359882816159 ) ) ;
#38773 = ORIENTED_EDGE ( 'NONE', *, *, #12202, .T. ) ;
#38774 = CARTESIAN_POINT ( 'NONE',  ( 96.28659315884510761, -57.67146175308503331, 43.74667604778345265 ) ) ;
#38775 = EDGE_CURVE ( 'NONE', #46516, #22672, #4133, .T. ) ;
#38776 = CARTESIAN_POINT ( 'NONE',  ( 35.32911723019348926, 437.0667969981791430, 5.602639083904082717 ) ) ;
#38777 = CARTESIAN_POINT ( 'NONE',  ( 12.49955057316562090, -4.332870170068738425, -12.71907580248059233 ) ) ;
#38778 =( LENGTH_UNIT ( ) NAMED_UNIT ( * ) SI_UNIT ( .MILLI., .METRE. ) );
#38779 = CONICAL_SURFACE ( 'NONE', #16350, 4.172000000000001485, 0.9599310885968750373 ) ;
#38780 = CARTESIAN_POINT ( 'NONE',  ( -58.90678327781357382, 40.83906611473262416, -28.11551192243389607 ) ) ;
#38781 = CARTESIAN_POINT ( 'NONE',  ( 11.81719646716459948, -21.03406259286755642, 35.54759019141032894 ) ) ;
#38782 = CARTESIAN_POINT ( 'NONE',  ( 8.000000000000000000, -4.999999999999998224, 2.094395098902538166 ) ) ;
#38783 = CARTESIAN_POINT ( 'NONE',  ( -0.9763930676160361699, 8.096533237421388307, -7.213065638943060520 ) ) ;
#38785 = CARTESIAN_POINT ( 'NONE',  ( -14.78804146188508462, 5.762582778709502307, 6.905855753343613124 ) ) ;
#38784 = CARTESIAN_POINT ( 'NONE',  ( 42.58368960131090830, 480.4983903161937064, 9.551102386166812508 ) ) ;
#38786 = CARTESIAN_POINT ( 'NONE',  ( 0.000000000000000000, 0.000000000000000000, 0.000000000000000000 ) ) ;
#38787 = CARTESIAN_POINT ( 'NONE',  ( 9.341953373612906120, 15.21714514899110071, -3.572352985695328442 ) ) ;
#38788 = CARTESIAN_POINT ( 'NONE',  ( 0.000000000000000000, 0.000000000000000000, -0.01269999999999786924 ) ) ;
#38789 = CARTESIAN_POINT ( 'NONE',  ( -85.24003831912723683, -38.00000000000003553, 47.20936526245474596 ) ) ;
#38790 = AXIS2_PLACEMENT_3D ( 'NONE', #56384, #30570, #81718 ) ;
#38791 = VERTEX_POINT ( 'NONE', #61857 ) ;
#38792 = CARTESIAN_POINT ( 'NONE',  ( -15.44819439224355584, -0.7587808896114125456, 14.98257521071344911 ) ) ;
#38793 = SURFACE_STYLE_FILL_AREA ( #14478 ) ;
#38794 = CARTESIAN_POINT ( 'NONE',  ( 5.911778709945830101, -61.13338160583428760, 1.058844270818172451 ) ) ;
#38796 = CARTESIAN_POINT ( 'NONE',  ( -28.77979384944077523, -47.40897086083281664, -33.14033794634894292 ) ) ;
#38795 = CARTESIAN_POINT ( 'NONE',  ( 0.000000000000000000, 9.797174393178825657E-16, -8.000000000000000000 ) ) ;
#38797 = EDGE_CURVE ( 'NONE', #27771, #93549, #20387, .T. ) ;
#38798 = VECTOR ( 'NONE', #55672, 1000.000000000000000 ) ;
#38799 = VERTEX_POINT ( 'NONE', #4666 ) ;
#38800 = CARTESIAN_POINT ( 'NONE',  ( 0.000000000000000000, 152.0000000000000000, 0.000000000000000000 ) ) ;
#38801 = ORIENTED_EDGE ( 'NONE', *, *, #96255, .F. ) ;
#38802 = EDGE_CURVE ( 'NONE', #25666, #35056, #25520, .T. ) ;
#38803 = EDGE_CURVE ( 'NONE', #102690, #18921, #68528, .T. ) ;
#38804 = CARTESIAN_POINT ( 'NONE',  ( 23.15769230769230802, 1.411358822780289120E-15, 0.000000000000000000 ) ) ;
#38805 = CONICAL_SURFACE ( 'NONE', #28519, 5.000000000000010658, 0.9599310885968697082 ) ;
#38806 = CARTESIAN_POINT ( 'NONE',  ( -90.49378535418108527, -60.00000000000000711, -17.94840510955679136 ) ) ;
#38807 = EDGE_LOOP ( 'NONE', ( #6940, #77248, #54053, #67166, #15437 ) ) ;
#38808 = CARTESIAN_POINT ( 'NONE',  ( 5.656854249492378806, -27.87500000409677270, 5.656854249492381470 ) ) ;
#38809 = CARTESIAN_POINT ( 'NONE',  ( 0.000000000000000000, 1.502314598737160017E-15, -6.500000000000000000 ) ) ;
#38810 = MECHANICAL_DESIGN_GEOMETRIC_PRESENTATION_REPRESENTATION (  '', ( #21585 ), #87026 ) ;
#38811 = CARTESIAN_POINT ( 'NONE',  ( 98.54373379153146573, -45.26741342605672713, 193.5399338678095376 ) ) ;
#38812 = VECTOR ( 'NONE', #53261, 1000.000000000000114 ) ;
#38814 = DIRECTION ( 'NONE',  ( 0.000000000000000000, 0.000000000000000000, 1.000000000000000000 ) ) ;
#38813 = DIRECTION ( 'NONE',  ( 0.000000000000000000, 1.000000000000000000, 0.000000000000000000 ) ) ;
#38815 = CARTESIAN_POINT ( 'NONE',  ( -82.78929023607005888, -32.55497806570344466, 157.1457539419261309 ) ) ;
#38816 = ORIENTED_EDGE ( 'NONE', *, *, #64195, .T. ) ;
#38817 = AXIS2_PLACEMENT_3D ( 'NONE', #106741, #100248, #59280 ) ;
#38818 = CARTESIAN_POINT ( 'NONE',  ( -9.699121749566383954, 253.1766876027581930, 2.444499528233548435 ) ) ;
#38819 = ORIENTED_EDGE ( 'NONE', *, *, #87105, .T. ) ;
#38820 = TOROIDAL_SURFACE ( 'NONE', #47414, 13.00000000000000000, 2.000000000000000000 ) ;
#38821 = ORIENTED_EDGE ( 'NONE', *, *, #63984, .F. ) ;
#38822 = CARTESIAN_POINT ( 'NONE',  ( -6.113204517632431667, -61.77363733626824427, 14.40517576086940643 ) ) ;
#38823 = CARTESIAN_POINT ( 'NONE',  ( 0.000000000000000000, 0.000000000000000000, 4.000000000000000000 ) ) ;
#38824 = VERTEX_POINT ( 'NONE', #88760 ) ;
#38825 = EDGE_CURVE ( 'NONE', #81898, #19635, #46699, .T. ) ;
#38826 = FILL_AREA_STYLE_COLOUR ( '', #89219 ) ;
#38827 =( NAMED_UNIT ( * ) SI_UNIT ( $, .STERADIAN. ) SOLID_ANGLE_UNIT ( ) );
#38828 = CARTESIAN_POINT ( 'NONE',  ( -76.58308308725453628, -57.53248158402972479, 194.3307878365576187 ) ) ;
#38829 = CARTESIAN_POINT ( 'NONE',  ( 0.000000000000000000, 0.000000000000000000, 4.000000000000000888 ) ) ;
#38830 = CARTESIAN_POINT ( 'NONE',  ( -9.789044728060147804, 294.6486233851416614, -2.043184600577789833 ) ) ;
#38831 = DIRECTION ( 'NONE',  ( -1.000000000000000000, 0.000000000000000000, 0.000000000000000000 ) ) ;
#38832 = CARTESIAN_POINT ( 'NONE',  ( 1.219735312445022535, 27.62936970793004576, -39.81700975820285748 ) ) ;
#38833 = CARTESIAN_POINT ( 'NONE',  ( 89.53125762993630588, -30.00000000000007461, -13.19907884436577561 ) ) ;
#38834 = EDGE_CURVE ( 'NONE', #55889, #62536, #27219, .T. ) ;
#38835 = CARTESIAN_POINT ( 'NONE',  ( -72.40149263128425616, -29.99999999999999289, 139.7559031367707405 ) ) ;
#38836 = CARTESIAN_POINT ( 'NONE',  ( -55.20763222134070247, -18.68546736084697102, 52.51444300613069771 ) ) ;
#38837 = VERTEX_POINT ( 'NONE', #55311 ) ;
#38838 = CARTESIAN_POINT ( 'NONE',  ( 6.559876275494352704, 16.16983035391954360, -2.453497130494365575 ) ) ;
#38839 = VERTEX_POINT ( 'NONE', #62904 ) ;
#38840 = CARTESIAN_POINT ( 'NONE',  ( -102.7301835497670908, -60.18086027025601936, 193.2518684143816472 ) ) ;
#38841 = CARTESIAN_POINT ( 'NONE',  ( -30.29343180852501050, 12.93058661249364327, -41.94895705695265775 ) ) ;
#38842 = ORIENTED_EDGE ( 'NONE', *, *, #100402, .T. ) ;
#38843 = CARTESIAN_POINT ( 'NONE',  ( 19.23241393038752278, 49.80479087863259480, 61.49459632677954346 ) ) ;
#38844 = CARTESIAN_POINT ( 'NONE',  ( 90.14312592591035411, -38.39823370583771833, -15.62996679376882270 ) ) ;
#38845 = CARTESIAN_POINT ( 'NONE',  ( 6.123233995736771213E-16, 0.000000000000000000, 5.000000000000003553 ) ) ;
#38846 = CARTESIAN_POINT ( 'NONE',  ( -4.000000000000000000, 0.000000000000000000, -3.432199999999999918 ) ) ;
#38847 = DIRECTION ( 'NONE',  ( 0.000000000000000000, 0.000000000000000000, 1.000000000000000000 ) ) ;
#38848 =( BOUNDED_SURFACE ( )  B_SPLINE_SURFACE ( 3, 2, ( 
 ( #97501, #96478, #72192 ),
 ( #30701, #6913, #32283 ),
 ( #47893, #63589, #106127 ),
 ( #47372, #56517, #65153 ),
 ( #98053, #15003, #24201 ),
 ( #72709, #95948, #16071 ),
 ( #46846, #13935, #64633 ),
 ( #5851, #55975, #104015 ),
 ( #57048, #89446, #55452 ),
 ( #15536, #23134, #80263 ),
 ( #48953, #79746, #14460 ),
 ( #89965, #38776, #48430 ) ),
 .UNSPECIFIED., .F., .F., .F. ) 
 B_SPLINE_SURFACE_WITH_KNOTS ( ( 4, 2, 2, 2, 2, 4 ),
 ( 3, 3 ),
 ( 3.707971429900425164E-17, 0.0004396180695633393194, 0.0008792361391266415591, 0.001758472278253246038, 0.002637708417379850626, 0.003516944556506455214 ),
 ( 0.000000000000000000, 1.000000000000000000 ),
 .UNSPECIFIED. ) 
 GEOMETRIC_REPRESENTATION_ITEM ( )  RATIONAL_B_SPLINE_SURFACE ( (
 ( 1.000000000000000000, 0.9193453746270715543, 1.000000000000000000),
 ( 1.000000000000000000, 0.9231392589459156417, 1.000000000000000000),
 ( 1.000000000000000000, 0.9252300355209908123, 1.000000000000000000),
 ( 1.000000000000000000, 0.9257136340838321154, 1.000000000000000000),
 ( 1.000000000000000000, 0.9240662039545859407, 1.000000000000000000),
 ( 1.000000000000000000, 0.9140412217423881103, 1.000000000000000000),
 ( 1.000000000000000000, 0.9005671153087457803, 1.000000000000000000),
 ( 1.000000000000000000, 0.8672639112290936314, 1.000000000000000000),
 ( 1.000000000000000000, 0.8470036231256007353, 1.000000000000000000),
 ( 1.000000000000000000, 0.8036658034633893388, 1.000000000000000000),
 ( 1.000000000000000000, 0.7801896332604544293, 1.000000000000000000),
 ( 1.000000000000000000, 0.7557288854858671412, 1.000000000000000000) ) ) 
 REPRESENTATION_ITEM ( '' )  SURFACE ( )  );
#38849 = AXIS2_PLACEMENT_3D ( 'NONE', #57318, #39581, #41158 ) ;
#38850 = CARTESIAN_POINT ( 'NONE',  ( 43.55333112596303380, 465.2342844084865874, 9.238213423009675296 ) ) ;
#38851 = CARTESIAN_POINT ( 'NONE',  ( -37.04388863813380794, 311.3287000699716032, 13.89786840526617517 ) ) ;
#38852 = CARTESIAN_POINT ( 'NONE',  ( 95.70911704725124025, 1.016364837396684119E-14, 0.000000000000000000 ) ) ;
#38853 = CARTESIAN_POINT ( 'NONE',  ( -0.3344035310850524412, 34.18675715969972373, 29.70737310419187693 ) ) ;
#38854 = CARTESIAN_POINT ( 'NONE',  ( -33.88237199998293647, 485.0486819176492759, 1.241522336454330411 ) ) ;
#38855 = B_SPLINE_CURVE_WITH_KNOTS ( 'NONE', 3,
 ( #10942, #76755, #26141, #2863, #67623, #26658, #101576, #92405, #18554, #51417, #19644, #43340, #76223, #52477, #85395, #28254, #3415, #29840, #78880, #12543, #5527, #38453, #85948, #104213, #45478, #11478, #36357, #87000, #71319, #69226 ),
 .UNSPECIFIED., .F., .F.,
 ( 4, 2, 2, 2, 2, 2, 2, 2, 2, 2, 2, 2, 2, 2, 4 ),
 ( 0.002924093377768722125, 0.003854458377716627783, 0.004784823377664528671, 0.005715188377612428691, 0.006180370877586383906, 0.006645553377560339120, 0.007110735877534295202, 0.007343327127521271508, 0.007575918377508249549, 0.007808509627495227590, 0.008041100877482207365, 0.008506283377456165182, 0.008971465877430122998, 0.009436648377404082549, 0.01036701337735199818 ),
 .UNSPECIFIED. ) ;
#38856 = ORIENTED_EDGE ( 'NONE', *, *, #70473, .F. ) ;
#38857 = ORIENTED_EDGE ( 'NONE', *, *, #76488, .F. ) ;
#38858 = CARTESIAN_POINT ( 'NONE',  ( 50.87530857847808363, -36.04660271324092946, 51.03790572413701199 ) ) ;
#38859 = DIRECTION ( 'NONE',  ( -1.000000000000000000, -0.000000000000000000, -0.000000000000000000 ) ) ;
#38860 = CARTESIAN_POINT ( 'NONE',  ( -5.919343243681499445, 14.43244923957804460, -3.736960138817876143 ) ) ;
#38861 = CARTESIAN_POINT ( 'NONE',  ( -110.5687679044198291, -38.35612487468937104, 181.7317928493044974 ) ) ;
#38862 = ORIENTED_EDGE ( 'NONE', *, *, #87728, .F. ) ;
#38863 = CARTESIAN_POINT ( 'NONE',  ( 91.45439809862598679, -38.39047740764758032, -7.874681939750319160 ) ) ;
#38864 = CARTESIAN_POINT ( 'NONE',  ( 10.64742384531193942, 14.88071023319941411, -9.840650288117007705 ) ) ;
#38865 = CARTESIAN_POINT ( 'NONE',  ( 96.28888888888889142, 1.023464760207051730E-14, 0.000000000000000000 ) ) ;
#38866 = CARTESIAN_POINT ( 'NONE',  ( 13.50000000000000355, -5.228219631169429782, -0.5328967677612925780 ) ) ;
#38867 = CARTESIAN_POINT ( 'NONE',  ( 94.80615415396439971, -37.84849680385329407, 106.6770409997166382 ) ) ;
#38868 = CARTESIAN_POINT ( 'NONE',  ( -31.29447218978298650, 439.6461559793971219, 23.31027018619894875 ) ) ;
#38869 = CARTESIAN_POINT ( 'NONE',  ( -32.30941696154608422, 435.2301481353223949, 15.36959316898724737 ) ) ;
#38870 = CARTESIAN_POINT ( 'NONE',  ( -35.53899189460923225, 397.1537505765458604, 6.928033022457113610 ) ) ;
#38871 = CARTESIAN_POINT ( 'NONE',  ( -32.65592842490316627, 434.9896282828135554, 13.53682765909404040 ) ) ;
#38872 =( NAMED_UNIT ( * ) SI_UNIT ( $, .STERADIAN. ) SOLID_ANGLE_UNIT ( ) );
#38873 = CARTESIAN_POINT ( 'NONE',  ( 91.28860837299599496, -60.00000000000002132, 202.2318051499666467 ) ) ;
#38874 = CARTESIAN_POINT ( 'NONE',  ( -16.58664841766668019, 35.02554381010406814, 21.81514337942032355 ) ) ;
#38876 = ORIENTED_EDGE ( 'NONE', *, *, #22492, .F. ) ;
#38875 =( BOUNDED_SURFACE ( )  B_SPLINE_SURFACE ( 3, 2, ( 
 ( #48059, #39473, #105255 ),
 ( #43179, #19480, #77137 ),
 ( #18942, #35115, #26503 ),
 ( #2704, #10265, #51785 ),
 ( #91214, #92782, #36193 ),
 ( #59374, #10782, #17852 ),
 ( #60451, #99808, #99258 ),
 ( #59915, #84698, #92236 ),
 ( #50705, #43701, #67461 ),
 ( #83617, #25434, #1628 ),
 ( #9721, #66928, #68530 ),
 ( #18390, #42637, #84170 ),
 ( #42102, #51243, #9191 ),
 ( #75534, #74986, #27031 ) ),
 .UNSPECIFIED., .F., .F., .F. ) 
 B_SPLINE_SURFACE_WITH_KNOTS ( ( 4, 2, 2, 2, 2, 2, 4 ),
 ( 3, 3 ),
 ( -1.457818241124009262E-15, 0.001036839948807126086, 0.001555259923211418146, 0.002073679897615710206, 0.002592099872020002266, 0.003110519846424294327, 0.004147359795232878447 ),
 ( 0.000000000000000000, 1.000000000000000000 ),
 .UNSPECIFIED. ) 
 GEOMETRIC_REPRESENTATION_ITEM ( )  RATIONAL_B_SPLINE_SURFACE ( (
 ( 1.000000000000000000, 0.8806660624989138819, 1.000000000000000000),
 ( 1.000000000000000000, 0.8881715692662220940, 1.000000000000000000),
 ( 1.000000000000000000, 0.8928479710807014635, 1.000000000000000000),
 ( 1.000000000000000000, 0.8947313045151512600, 1.000000000000000000),
 ( 1.000000000000000000, 0.8944961860243509921, 1.000000000000000000),
 ( 1.000000000000000000, 0.8923679545988014716, 1.000000000000000000),
 ( 1.000000000000000000, 0.8904472546607837824, 1.000000000000000000),
 ( 1.000000000000000000, 0.8850746651129741682, 1.000000000000000000),
 ( 1.000000000000000000, 0.8816555630472442395, 1.000000000000000000),
 ( 1.000000000000000000, 0.8735136825623661672, 1.000000000000000000),
 ( 1.000000000000000000, 0.8687495631818540343, 1.000000000000000000),
 ( 1.000000000000000000, 0.8530568296116498583, 1.000000000000000000),
 ( 1.000000000000000000, 0.8406856949812601121, 1.000000000000000000),
 ( 1.000000000000000000, 0.8270258197359576791, 1.000000000000000000) ) ) 
 REPRESENTATION_ITEM ( '' )  SURFACE ( )  );
#38877 = CARTESIAN_POINT ( 'NONE',  ( 59.01113678252345807, -39.48982602246088192, 69.66931651419592697 ) ) ;
#38878 = CARTESIAN_POINT ( 'NONE',  ( -30.39554535350546161, 298.0292904638343998, -1.300630307310727707 ) ) ;
#38879 = CARTESIAN_POINT ( 'NONE',  ( 6.928203230275509661, 30.26479267253571592, 3.999999999999999112 ) ) ;
#38880 = EDGE_CURVE ( 'NONE', #6938, #62849, #95800, .T. ) ;
#38881 = FACE_OUTER_BOUND ( 'NONE', #84945, .T. ) ;
#38882 = ORIENTED_EDGE ( 'NONE', *, *, #48532, .F. ) ;
#38884 = DIRECTION ( 'NONE',  ( 1.000000000000000000, 0.000000000000000000, 0.000000000000000000 ) ) ;
#38883 = CARTESIAN_POINT ( 'NONE',  ( -109.9283950457840433, -38.35593267714713761, 186.3516114292234818 ) ) ;
#38885 = CARTESIAN_POINT ( 'NONE',  ( 8.099999999999999645, 0.000000000000000000, 0.000000000000000000 ) ) ;
#38886 = CARTESIAN_POINT ( 'NONE',  ( 26.53231809466943503, 310.2838222077303953, 10.22456148134894072 ) ) ;
#38887 = CARTESIAN_POINT ( 'NONE',  ( 63.07777777777777573, 3.309500000000014541, 4.052968581778174646E-16 ) ) ;
#38888 = CARTESIAN_POINT ( 'NONE',  ( -4.413588872808956509, -9.563952367648484554, 5.751921314263696239 ) ) ;
#38889 = PRESENTATION_LAYER_ASSIGNMENT (  '', '', ( #57792 ) ) ;
#38890 = CARTESIAN_POINT ( 'NONE',  ( 9.999999999999996447, -5.000000000000002665, -86.30899693748767731 ) ) ;
#38891 = EDGE_CURVE ( 'NONE', #90401, #52034, #14319, .T. ) ;
#38892 = ADVANCED_FACE ( 'NONE', ( #39163 ), #54713, .T. ) ;
#38893 = COLOUR_RGB ( '', 0.09019608, 0.27058824, 0.51372549) ;
#38894 = AXIS2_PLACEMENT_3D ( 'NONE', #62740, #45504, #3966 ) ;
#38895 = CIRCLE ( 'NONE', #45737, 5.000000000000000888 ) ;
#38896 = ORIENTED_EDGE ( 'NONE', *, *, #87921, .T. ) ;
#38897 = CARTESIAN_POINT ( 'NONE',  ( 85.33552361055200208, -25.38509375986750882, 170.5403938721447616 ) ) ;
#38898 = ADVANCED_FACE ( 'NONE', ( #54239 ), #68148, .F. ) ;
#38899 = CARTESIAN_POINT ( 'NONE',  ( 9.493245307752808060, 9.599219626221964674, -0.000000000000000000 ) ) ;
#38900 = CARTESIAN_POINT ( 'NONE',  ( -33.50393555050020922, 439.8572903566229684, 24.25426608324027455 ) ) ;
#38901 = ORIENTED_EDGE ( 'NONE', *, *, #93806, .F. ) ;
#38902 = CARTESIAN_POINT ( 'NONE',  ( -25.55259955101245950, 304.1867599840693970, -9.710062353868671892 ) ) ;
#38903 = EDGE_CURVE ( 'NONE', #36789, #37165, #28187, .T. ) ;
#38904 =( LENGTH_UNIT ( ) NAMED_UNIT ( * ) SI_UNIT ( .MILLI., .METRE. ) );
#38905 = CARTESIAN_POINT ( 'NONE',  ( 40.34377649348542860, 485.2488587072590462, -4.812891347181404100 ) ) ;
#38906 = CARTESIAN_POINT ( 'NONE',  ( -3.122695041978579056, 50.00000000000000711, -96.69538631875555268 ) ) ;
#38907 = CARTESIAN_POINT ( 'NONE',  ( -24.28924816910272710, 43.70283635897345675, -77.10780450745573944 ) ) ;
#38908 = SURFACE_STYLE_USAGE ( .BOTH. , #16737 ) ;
#38909 = EDGE_LOOP ( 'NONE', ( #101966, #34232, #94801, #627, #83231 ) ) ;
#38910 = CARTESIAN_POINT ( 'NONE',  ( -81.58738582554423147, -30.00000000000000000, 29.51690375706957425 ) ) ;
#38911 = CARTESIAN_POINT ( 'NONE',  ( 6.499999999999998224, 0.6659426636834143709, -5.719325464431598505 ) ) ;
#38912 = CARTESIAN_POINT ( 'NONE',  ( 0.3167204509598363082, 5.377136764700156668, 6.686525924292793022 ) ) ;
#38914 = CARTESIAN_POINT ( 'NONE',  ( -12.35636350804288774, 17.94545210593157236, -8.708632758017785136 ) ) ;
#38913 = CARTESIAN_POINT ( 'NONE',  ( 43.03880698781976832, 435.3545807224048190, 16.83573131045122651 ) ) ;
#38915 = CARTESIAN_POINT ( 'NONE',  ( -5.082755093536325042, -20.09375000204838457, -5.082755093536325930 ) ) ;
#38916 = CARTESIAN_POINT ( 'NONE',  ( -28.45500467043791204, 17.07616014098841362, -41.11859397474302114 ) ) ;
#38917 = CARTESIAN_POINT ( 'NONE',  ( 27.10511071441197117, -1.200000000000000030E-05, 7.556984339685704377 ) ) ;
#38918 = EDGE_LOOP ( 'NONE', ( #62297, #4396, #51162, #71362, #62054 ) ) ;
#38919 = CARTESIAN_POINT ( 'NONE',  ( -18.91769957617901809, 48.49892424865640805, 62.17828500952143145 ) ) ;
#38920 = CARTESIAN_POINT ( 'NONE',  ( 7.894705354778059458, 0.7527931906213466418, -7.590204373988306941 ) ) ;
#38921 = AXIS2_PLACEMENT_3D ( 'NONE', #23464, #103818, #40143 ) ;
#38922 = CARTESIAN_POINT ( 'NONE',  ( -2.856083322019343118, 67.83493845259130239, -5.000000000000000000 ) ) ;
#38923 = CARTESIAN_POINT ( 'NONE',  ( -7.421727621021489973, -3.000000000000118128, -70.37058875307404548 ) ) ;
#38924 = CARTESIAN_POINT ( 'NONE',  ( 6.394343112843832166, 3.776352960569632877, 6.540835195019754522 ) ) ;
#38925 = EDGE_LOOP ( 'NONE', ( #55794, #52106, #100747, #31392, #103399, #17092 ) ) ;
#38926 = DIRECTION ( 'NONE',  ( 0.000000000000000000, 0.000000000000000000, 1.000000000000000000 ) ) ;
#38927 = DIRECTION ( 'NONE',  ( 0.000000000000000000, 0.000000000000000000, 1.000000000000000000 ) ) ;
#38928 = ORIENTED_EDGE ( 'NONE', *, *, #90174, .F. ) ;
#38929 = EDGE_CURVE ( 'NONE', #21000, #102866, #8362, .T. ) ;
#38930 = DIRECTION ( 'NONE',  ( 0.000000000000000000, 0.000000000000000000, -1.000000000000000000 ) ) ;
#38931 = DIRECTION ( 'NONE',  ( 0.000000000000000000, 0.000000000000000000, 1.000000000000000000 ) ) ;
#38932 = CARTESIAN_POINT ( 'NONE',  ( 16.14595037822608603, 7.274337365584590209, -6.616591826375515240 ) ) ;
#38933 = FACE_OUTER_BOUND ( 'NONE', #83372, .T. ) ;
#38934 = CARTESIAN_POINT ( 'NONE',  ( -112.0891722639055814, -59.99999999999999289, 178.1611067759957336 ) ) ;
#38935 = FACE_OUTER_BOUND ( 'NONE', #88724, .T. ) ;
#38936 = DIRECTION ( 'NONE',  ( -0.9090909090909091717, 0.000000000000000000, -0.4165977904505311913 ) ) ;
#38937 = CARTESIAN_POINT ( 'NONE',  ( 6.542049517734651154, 53.55479212070640926, -7.321410255469364081 ) ) ;
#38938 = CARTESIAN_POINT ( 'NONE',  ( 43.33498512661115143, 464.9732568094945577, 13.98542553804674426 ) ) ;
#38939 = CARTESIAN_POINT ( 'NONE',  ( -82.07449229012887315, -53.53251292769294167, 181.8262338053436906 ) ) ;
#38940 = VERTEX_POINT ( 'NONE', #8889 ) ;
#38941 = CARTESIAN_POINT ( 'NONE',  ( 43.73099574044837823, 41.41642832801956331, -50.37982054108119456 ) ) ;
#38942 = ORIENTED_EDGE ( 'NONE', *, *, #14486, .T. ) ;
#38944 = EDGE_CURVE ( 'NONE', #27308, #46431, #28785, .T. ) ;
#38943 = DIRECTION ( 'NONE',  ( 0.5564727496918440153, 0.8308658609248538163, 0.000000000000000000 ) ) ;
#38946 = CARTESIAN_POINT ( 'NONE',  ( 4.660674839411963255, -66.31782485304402996, -3.778981567323764779 ) ) ;
#38945 = AXIS2_PLACEMENT_3D ( 'NONE', #12352, #29648, #12879 ) ;
#38947 = CARTESIAN_POINT ( 'NONE',  ( -82.41975597616887228, -37.82984823159566190, 11.94393511651135142 ) ) ;
#38948 = CARTESIAN_POINT ( 'NONE',  ( -13.26814552884363962, 304.5542534004749768, 8.873748344450744341 ) ) ;
#38949 = CARTESIAN_POINT ( 'NONE',  ( 8.642300018659421212, 22.39467290678169320, -4.999999999999385381 ) ) ;
#38950 = FILL_AREA_STYLE ('',( #14640 ) ) ;
#38951 = CARTESIAN_POINT ( 'NONE',  ( 7.754160006592983656, 42.00000000000000711, 59.23741894013591036 ) ) ;
#38952 = CARTESIAN_POINT ( 'NONE',  ( 84.52829458723479661, -59.99999999999986500, 202.7046071135156069 ) ) ;
#38953 = CARTESIAN_POINT ( 'NONE',  ( -90.94649322911389788, -14.21045842199428222, 57.96573475225447680 ) ) ;
#38954 = CARTESIAN_POINT ( 'NONE',  ( -63.81269489221281788, -42.96200065895143894, 84.51879323443225189 ) ) ;
#38955 = AXIS2_PLACEMENT_3D ( 'NONE', #97066, #36890, #84874 ) ;
#38956 = ORIENTED_EDGE ( 'NONE', *, *, #26674, .F. ) ;
#38957 = CARTESIAN_POINT ( 'NONE',  ( 39.08459411749380052, 39.42618201486132534, 52.27850612433365995 ) ) ;
#38958 = CARTESIAN_POINT ( 'NONE',  ( 70.43415898748341419, -60.00000000002942357, 160.5900936467152746 ) ) ;
#38959 = AXIS2_PLACEMENT_3D ( 'NONE', #22301, #23896, #97206 ) ;
#38961 = ORIENTED_EDGE ( 'NONE', *, *, #47647, .F. ) ;
#38960 = AXIS2_PLACEMENT_3D ( 'NONE', #4468, #79932, #104747 ) ;
#38962 = CARTESIAN_POINT ( 'NONE',  ( 1.974351198080348091, -18.58616468225248397, 26.98526860823282547 ) ) ;
#38964 = PRESENTATION_LAYER_ASSIGNMENT (  '', '', ( #50945 ) ) ;
#38963 = CARTESIAN_POINT ( 'NONE',  ( 4.401442555609581635E-16, -17.65625000204838813, -7.188101187500000044 ) ) ;
#38965 = EDGE_CURVE ( 'NONE', #94321, #22777, #9542, .T. ) ;
#38966 = CARTESIAN_POINT ( 'NONE',  ( 0.000000000000000000, 0.000000000000000000, -10.42450674750459072 ) ) ;
#38967 = EDGE_LOOP ( 'NONE', ( #80669, #69092, #20763, #57346 ) ) ;
#38968 = CARTESIAN_POINT ( 'NONE',  ( -1.469576158976823947E-15, -26.56250000409677270, 8.000000000000000000 ) ) ;
#38969 = ORIENTED_EDGE ( 'NONE', *, *, #64517, .F. ) ;
#38970 = CARTESIAN_POINT ( 'NONE',  ( 11.27392099353245669, 45.76150927139935476, -13.37519430359090755 ) ) ;
#38971 = CARTESIAN_POINT ( 'NONE',  ( -7.188101187500000044, -29.28125000204838813, -8.802885111219163269E-16 ) ) ;
#38972 = CARTESIAN_POINT ( 'NONE',  ( -89.85221766084636386, -60.00000000000002132, 201.9352697163374160 ) ) ;
#38973 = CARTESIAN_POINT ( 'NONE',  ( 35.70257255451698342, 337.7971262439807560, -1.754882810684410321 ) ) ;
#38974 = CARTESIAN_POINT ( 'NONE',  ( 5.082755093536324154, -27.21875000204838813, 5.082755093536326818 ) ) ;
#38975 = DIRECTION ( 'NONE',  ( -0.8191520442889975717, 0.000000000000000000, -0.5735764363510378328 ) ) ;
#38976 =( GEOMETRIC_REPRESENTATION_CONTEXT ( 3 ) GLOBAL_UNCERTAINTY_ASSIGNED_CONTEXT ( ( #30783 ) ) GLOBAL_UNIT_ASSIGNED_CONTEXT ( ( #47651, #2817, #93445 ) ) REPRESENTATION_CONTEXT ( 'NONE', 'WORKASPACE' ) );
#38977 = CARTESIAN_POINT ( 'NONE',  ( -5.910549702781506376, 54.01482550163699869, -6.184394181519167866 ) ) ;
#38978 = CARTESIAN_POINT ( 'NONE',  ( 5.000000000000000888, -68.69132998577062210, 12.24443901500599807 ) ) ;
#38979 = FACE_OUTER_BOUND ( 'NONE', #41379, .T. ) ;
#38980 = CARTESIAN_POINT ( 'NONE',  ( 9.283862214035533356, -2.881445901645539820, 14.75262417026159412 ) ) ;
#38981 = CARTESIAN_POINT ( 'NONE',  ( 28.09999999999999787, 3.309500000000003439, 4.052968581778167743E-16 ) ) ;
#38982 = CARTESIAN_POINT ( 'NONE',  ( 33.43292762174942112, 315.2036803431912517, -7.045335761960068055 ) ) ;
#38983 = CARTESIAN_POINT ( 'NONE',  ( -39.12603572575172706, -60.26799234672426309, 42.39855392131921974 ) ) ;
#38984 = EDGE_LOOP ( 'NONE', ( #71611, #11384, #42410, #35504, #17617, #65438 ) ) ;
#38985 = CARTESIAN_POINT ( 'NONE',  ( -38.85446894546474539, 460.8903912184078422, 2.218456751110488678 ) ) ;
#38986 = AXIS2_PLACEMENT_3D ( 'NONE', #32396, #71753, #57161 ) ;
#38987 = CARTESIAN_POINT ( 'NONE',  ( 36.22549068229315594, -46.43024825669357369, 37.39601728665412850 ) ) ;
#38988 = CARTESIAN_POINT ( 'NONE',  ( 13.66642973270348627, -9.677049996499534265E-13, 17.78317311657527000 ) ) ;
#38989 = EDGE_LOOP ( 'NONE', ( #48088, #46494, #33508, #92215, #56560, #103620 ) ) ;
#38990 = ADVANCED_FACE ( 'NONE', ( #25661 ), #65311, .F. ) ;
#38991 = CARTESIAN_POINT ( 'NONE',  ( -57.78802091145840336, -38.34425951725483372, 89.61089764502102639 ) ) ;
#38992 = VERTEX_POINT ( 'NONE', #96729 ) ;
#38994 = CARTESIAN_POINT ( 'NONE',  ( 45.33180403702434091, 464.4945808635454227, 2.178908857919817699 ) ) ;
#38993 = CARTESIAN_POINT ( 'NONE',  ( 8.074093511841809345, -5.000000000000000000, -15.92331255328525330 ) ) ;
#38995 = FACE_BOUND ( 'NONE', #33868, .T. ) ;
#38996 = CARTESIAN_POINT ( 'NONE',  ( -34.84618260875176787, 489.9833681528637044, 11.97975507378787619 ) ) ;
#38997 = FACE_OUTER_BOUND ( 'NONE', #34936, .T. ) ;
#38998 = CYLINDRICAL_SURFACE ( 'NONE', #18837, 15.00000000000000000 ) ;
#38999 = DIRECTION ( 'NONE',  ( -1.000000000000000000, 0.000000000000000000, 0.000000000000000000 ) ) ;
#39000 = CARTESIAN_POINT ( 'NONE',  ( -4.153385784896416411, -48.47379020312671827, 43.45327407259872388 ) ) ;
#39001 = CIRCLE ( 'NONE', #18371, 12.00000000000000711 ) ;
#39002 = CARTESIAN_POINT ( 'NONE',  ( 100.7505531824810987, -60.00000000000000711, 85.43635729793463440 ) ) ;
#39003 = DIRECTION ( 'NONE',  ( 0.000000000000000000, 0.000000000000000000, -1.000000000000000000 ) ) ;
#39004 = LINE ( 'NONE', #71884, #38798 ) ;
#39005 = LINE ( 'NONE', #66861, #68477 ) ;
#39006 = VERTEX_POINT ( 'NONE', #29891 ) ;
#39007 = EDGE_CURVE ( 'NONE', #86317, #82792, #67334, .T. ) ;
#39008 = CARTESIAN_POINT ( 'NONE',  ( -89.26149008746590141, -29.99999999999675993, -13.97880863715630184 ) ) ;
#39009 = ORIENTED_EDGE ( 'NONE', *, *, #41419, .F. ) ;
#39010 = CARTESIAN_POINT ( 'NONE',  ( 0.000000000000000000, 0.000000000000000000, 5.000000000000002665 ) ) ;
#39011 = CARTESIAN_POINT ( 'NONE',  ( -15.90328822607555281, 3.524689239577517341, 2.889827284417966435 ) ) ;
#39012 = CARTESIAN_POINT ( 'NONE',  ( 9.439237903447189382, 10.07757316350726207, 9.227579807199164141E-13 ) ) ;
#39013 = CARTESIAN_POINT ( 'NONE',  ( 15.66340762197770786, 21.48519827103249469, 5.204287273250217893 ) ) ;
#39014 = CARTESIAN_POINT ( 'NONE',  ( 83.87732489606810304, -52.73295681655777400, -15.45569567703784131 ) ) ;
#39015 = CARTESIAN_POINT ( 'NONE',  ( -2.977408999572654480, -27.50000000204838813, 7.188101187499999156 ) ) ;
#39016 = DIRECTION ( 'NONE',  ( -8.566042448110249984E-17, -0.7561819230143457249, 0.6543614439331877364 ) ) ;
#39017 = DIRECTION ( 'NONE',  ( -1.000000000000000000, -0.000000000000000000, -0.000000000000000000 ) ) ;
#39018 = CARTESIAN_POINT ( 'NONE',  ( 4.472135954999579610, -85.00000000000000000, 4.000000000000001776 ) ) ;
#39019 = EDGE_CURVE ( 'NONE', #25504, #24752, #22107, .T. ) ;
#39020 = ORIENTED_EDGE ( 'NONE', *, *, #99714, .T. ) ;
#39021 = EDGE_CURVE ( 'NONE', #58994, #52182, #23898, .T. ) ;
#39023 = EDGE_LOOP ( 'NONE', ( #70647, #8352, #22359, #23215, #44693 ) ) ;
#39022 = DIRECTION ( 'NONE',  ( -1.000000000000000000, -1.224606353822377258E-16, -0.000000000000000000 ) ) ;
#39024 = CARTESIAN_POINT ( 'NONE',  ( 81.44529849088311835, -39.49779538557150005, 155.9713579814424520 ) ) ;
#39025 = CIRCLE ( 'NONE', #63113, 4.000000000000007105 ) ;
#39026 = CARTESIAN_POINT ( 'NONE',  ( 14.24976063295490825, 2.188309765130968199, -4.656908667353339304 ) ) ;
#39027 = ORIENTED_EDGE ( 'NONE', *, *, #92084, .T. ) ;
#39028 = CARTESIAN_POINT ( 'NONE',  ( -12.50000000000000711, 18.64303733123573537, -36.27143273323382999 ) ) ;
#39029 = EDGE_CURVE ( 'NONE', #27490, #103169, #105343, .T. ) ;
#39030 = CARTESIAN_POINT ( 'NONE',  ( 7.744329845603314944, -88.46288230153457732, -2.018701143083234673 ) ) ;
#39031 = CARTESIAN_POINT ( 'NONE',  ( 7.188101187499999156, -14.75000000204838457, 2.977408999572654924 ) ) ;
#39032 = CARTESIAN_POINT ( 'NONE',  ( 11.38830949524109215, 45.34487012134832185, 14.75357462089488259 ) ) ;
#39033 = CARTESIAN_POINT ( 'NONE',  ( 13.70960934686813637, 294.5458232874115083, 9.871961475911533057 ) ) ;
#39034 = CIRCLE ( 'NONE', #28496, 6.500000000000000888 ) ;
#39035 = ORIENTED_EDGE ( 'NONE', *, *, #33997, .F. ) ;
#39036 = VECTOR ( 'NONE', #84165, 1000.000000000000227 ) ;
#39037 = DIRECTION ( 'NONE',  ( 0.000000000000000000, 0.000000000000000000, -1.000000000000000000 ) ) ;
#39038 = CARTESIAN_POINT ( 'NONE',  ( 6.828042838857774299, 41.63841260098274688, -58.95291818684747653 ) ) ;
#39039 = DIRECTION ( 'NONE',  ( -1.000000000000000000, -0.000000000000000000, -0.000000000000000000 ) ) ;
#39040 = EDGE_LOOP ( 'NONE', ( #20775, #102531, #6091, #89768, #37894, #42030 ) ) ;
#39041 = CARTESIAN_POINT ( 'NONE',  ( 8.000000000000000000, -11.09375000409677092, -3.313708498984761608 ) ) ;
#39042 = CIRCLE ( 'NONE', #71733, 5.000000000000002665 ) ;
#39043 = CARTESIAN_POINT ( 'NONE',  ( -25.64088414607024546, -19.60199216900910102, 31.60029921600921554 ) ) ;
#39044 = CIRCLE ( 'NONE', #59682, 0.9999999999999911182 ) ;
#39045 = CARTESIAN_POINT ( 'NONE',  ( 104.0908829527487711, 1.030564683017419500E-14, 0.000000000000000000 ) ) ;
#39046 = CIRCLE ( 'NONE', #21900, 5.000000000000011546 ) ;
#39047 = MECHANICAL_DESIGN_GEOMETRIC_PRESENTATION_REPRESENTATION (  '', ( #104463 ), #59685 ) ;
#39048 =( BOUNDED_SURFACE ( )  B_SPLINE_SURFACE ( 2, 3, ( 
 ( #6014, #63750, #105256, #8674, #58290, #72866, #7077, #105775, #23297, #89077, #65326, #40514, #56685, #24887, #57211, #98214, #89608, #6542, #49660, #41576, #90130, #31914, #16773, #23840, #56132, #57739, #97148, #90663, #64792, #74462, #80961, #542, #16232, #49117 ),
 ( #48590, #82569, #97675, #73932, #15702, #33505, #7596, #15173, #48062, #39993, #81479, #72353, #32982, #73391, #106292, #82017, #66379, #24367, #99259, #64280, #8142, #31403, #25436, #32454, #14625, #41049, #47537, #80432, #14, #65853, #39474, #98731, #1630, #99809 ),
 ( #25980, #43702, #76061, #51244, #18943, #27571, #85228, #59916, #51786, #74987, #93326, #58841, #76594, #26504, #92237, #11315, #10783, #35654, #92783, #35116, #18391, #34055, #2705, #42103, #66929, #84699, #91734, #10266, #69063, #28096, #101936, #50706, #68532, #101420 ) ),
 .UNSPECIFIED., .F., .T., .F. ) 
 B_SPLINE_SURFACE_WITH_KNOTS ( ( 3, 3 ),
 ( 4, 2, 2, 2, 2, 2, 2, 2, 2, 2, 2, 2, 2, 2, 2, 2, 4 ),
 ( 0.000000000000000000, 1.000000000000000000 ),
 ( 0.000000000000000000, 0.3926990816987241395, 0.7853981633974482790, 1.178097245096172418, 1.570796326794896558, 1.963495408493620697, 2.356194490192344837, 2.748893571891068976, 3.141592653589793116, 3.534291735288517255, 3.926990816987241395, 4.319689898685965090, 4.712388980384689674, 5.105088062083414258, 5.497787143782137953, 5.890486225480861648, 6.283185307179586232 ),
 .UNSPECIFIED. ) 
 GEOMETRIC_REPRESENTATION_ITEM ( )  RATIONAL_B_SPLINE_SURFACE ( (
 ( 1.000000000000000000, 1.000000000000000000, 1.000000000000000000, 1.000000000000000000, 1.000000000000000000, 1.000000000000000000, 1.000000000000000000, 1.000000000000000000, 1.000000000000000000, 1.000000000000000000, 1.000000000000000000, 1.000000000000000000, 1.000000000000000000, 1.000000000000000000, 1.000000000000000000, 1.000000000000000000, 1.000000000000000000, 1.000000000000000000, 1.000000000000000000, 1.000000000000000000, 1.000000000000000000, 1.000000000000000000, 1.000000000000000000, 1.000000000000000000, 1.000000000000000000, 1.000000000000000000, 1.000000000000000000, 1.000000000000000000, 1.000000000000000000, 1.000000000000000000, 1.000000000000000000, 1.000000000000000000, 1.000000000000000000, 1.000000000000000000),
 ( 1.857142857142858317, 1.857142857142858317, 1.857142857142858317, 1.857142857142858317, 1.857142857142858317, 1.857142857142858317, 1.857142857142858317, 1.857142857142858317, 1.857142857142858317, 1.857142857142858317, 1.857142857142858317, 1.857142857142858317, 1.857142857142858317, 1.857142857142858317, 1.857142857142858317, 1.857142857142858317, 1.857142857142858317, 1.857142857142858317, 1.857142857142858317, 1.857142857142858317, 1.857142857142858317, 1.857142857142858317, 1.857142857142858317, 1.857142857142858317, 1.857142857142858317, 1.857142857142858317, 1.857142857142858317, 1.857142857142858317, 1.857142857142858317, 1.857142857142858317, 1.857142857142858317, 1.857142857142858317, 1.857142857142858317, 1.857142857142858317),
 ( 1.000000000000000000, 1.000000000000000000, 1.000000000000000000, 1.000000000000000000, 1.000000000000000000, 1.000000000000000000, 1.000000000000000000, 1.000000000000000000, 1.000000000000000000, 1.000000000000000000, 1.000000000000000000, 1.000000000000000000, 1.000000000000000000, 1.000000000000000000, 1.000000000000000000, 1.000000000000000000, 1.000000000000000000, 1.000000000000000000, 1.000000000000000000, 1.000000000000000000, 1.000000000000000000, 1.000000000000000000, 1.000000000000000000, 1.000000000000000000, 1.000000000000000000, 1.000000000000000000, 1.000000000000000000, 1.000000000000000000, 1.000000000000000000, 1.000000000000000000, 1.000000000000000000, 1.000000000000000000, 1.000000000000000000, 1.000000000000000000) ) ) 
 REPRESENTATION_ITEM ( '' )  SURFACE ( )  );
#39049 = CARTESIAN_POINT ( 'NONE',  ( 1.220787089173188678, 51.58155239968396444, -9.312747329387569550 ) ) ;
#39050 = CARTESIAN_POINT ( 'NONE',  ( -37.29743259733409388, 437.4067882691437603, 4.451017177258851376 ) ) ;
#39051 = DIRECTION ( 'NONE',  ( 0.000000000000000000, 0.000000000000000000, 1.000000000000000000 ) ) ;
#39052 = PRODUCT_CONTEXT ( 'NONE', #23198, 'mechanical' ) ;
#39053 = CARTESIAN_POINT ( 'NONE',  ( -10.99438716495651214, -10.50257049600883263, 18.32467394275776584 ) ) ;
#39054 = ORIENTED_EDGE ( 'NONE', *, *, #95943, .F. ) ;
#39056 = AXIS2_PLACEMENT_3D ( 'NONE', #87239, #72100, #105007 ) ;
#39055 = CARTESIAN_POINT ( 'NONE',  ( 35.90484354297773706, 1.340359594676612611E-15, 0.000000000000000000 ) ) ;
#39057 = CARTESIAN_POINT ( 'NONE',  ( -2.563280883359616791, 15.30085158940939571, 9.673800154114420735 ) ) ;
#39058 = AXIS2_PLACEMENT_3D ( 'NONE', #73792, #71664, #23155 ) ;
#39059 = CARTESIAN_POINT ( 'NONE',  ( -1.056558204502631382, 13.98563387401484981, -6.924760179648891345 ) ) ;
#39060 = CARTESIAN_POINT ( 'NONE',  ( -46.00000000004250467, 463.8885932306518498, 10.44912889367152786 ) ) ;
#39061 = CARTESIAN_POINT ( 'NONE',  ( -64.74643051176546749, -30.00000000000000711, 79.49596584610381456 ) ) ;
#39062 = FACE_OUTER_BOUND ( 'NONE', #48657, .T. ) ;
#39063 = ORIENTED_EDGE ( 'NONE', *, *, #69650, .T. ) ;
#39064 = CARTESIAN_POINT ( 'NONE',  ( -26.12445749286578334, 36.99838226188546741, -9.598433884020590057 ) ) ;
#39065 = CARTESIAN_POINT ( 'NONE',  ( 95.70874240590093507, -57.62122494225103253, 204.5320780021935150 ) ) ;
#39066 = CARTESIAN_POINT ( 'NONE',  ( 62.88617926675873804, -47.40891080665988255, -26.65499022469952806 ) ) ;
#39067 = EDGE_CURVE ( 'NONE', #73863, #94099, #62776, .T. ) ;
#39068 = CARTESIAN_POINT ( 'NONE',  ( 10.00000000000000000, 15.00000000000000000, 10.00000000000000000 ) ) ;
#39069 = CARTESIAN_POINT ( 'NONE',  ( -15.72449985194402977, 22.05660461081803803, 3.876398783261274961 ) ) ;
#39070 = CARTESIAN_POINT ( 'NONE',  ( 0.1306530452038068557, -5.952467836904147269, 5.690023276062396107 ) ) ;
#39071 = CARTESIAN_POINT ( 'NONE',  ( -73.43589654061896965, -59.99999999999999289, 166.5613341509786096 ) ) ;
#39072 = DIRECTION ( 'NONE',  ( -0.000000000000000000, 1.000000000000000000, -0.000000000000000000 ) ) ;
#39073 = DIRECTION ( 'NONE',  ( 0.000000000000000000, 1.000000000000000000, 0.000000000000000000 ) ) ;
#39074 = CARTESIAN_POINT ( 'NONE',  ( -56.06936961864204250, 48.00000000000000000, -33.41736086623469504 ) ) ;
#39075 = COLOUR_RGB ( '', 0.31764706, 0.68627451, 0.89019608) ;
#39076 = B_SPLINE_CURVE_WITH_KNOTS ( 'NONE', 3,
 ( #55124, #80464, #31435, #47038, #79937, #30903 ),
 .UNSPECIFIED., .F., .F.,
 ( 4, 2, 4 ),
 ( 0.000000000000000000, 0.001916782365109770663, 0.003833564730219541326 ),
 .UNSPECIFIED. ) ;
#39077 = CARTESIAN_POINT ( 'NONE',  ( -85.31064313351537010, -46.56325337622924820, 188.2330627234076417 ) ) ;
#39078 = ORIENTED_EDGE ( 'NONE', *, *, #25478, .F. ) ;
#39079 = CARTESIAN_POINT ( 'NONE',  ( 36.72895593185456420, 408.8932456075058894, 6.289864422344447092 ) ) ;
#39080 = PRESENTATION_LAYER_ASSIGNMENT (  '', '', ( #95896 ) ) ;
#39081 = ORIENTED_EDGE ( 'NONE', *, *, #60320, .F. ) ;
#39083 = EDGE_CURVE ( 'NONE', #35138, #54417, #97916, .T. ) ;
#39082 = DIRECTION ( 'NONE',  ( 1.000000000000000000, 1.224606353822377258E-16, 0.000000000000000000 ) ) ;
#39084 = EDGE_CURVE ( 'NONE', #57394, #1686, #89162, .T. ) ;
#39085 = CARTESIAN_POINT ( 'NONE',  ( -31.21280335960756958, 312.0095200496609777, -8.085286564489109651 ) ) ;
#39086 = CARTESIAN_POINT ( 'NONE',  ( -83.39454600545269614, -45.25859893168446035, -13.67588221705811158 ) ) ;
#39087 = DIRECTION ( 'NONE',  ( 0.000000000000000000, -1.000000000000000000, 0.000000000000000000 ) ) ;
#39088 = CARTESIAN_POINT ( 'NONE',  ( 23.58349330513380337, 4.000000000000003553, 0.000000000000000000 ) ) ;
#39089 = ORIENTED_EDGE ( 'NONE', *, *, #81919, .F. ) ;
#39090 = CARTESIAN_POINT ( 'NONE',  ( 92.82022815836235452, -2.002967142162725287E-29, 5.000000000000011546 ) ) ;
#39091 = CARTESIAN_POINT ( 'NONE',  ( 11.90699106250066741, 6.512150199977177145, 8.940599429151134814 ) ) ;
#39092 = CARTESIAN_POINT ( 'NONE',  ( 13.66642973271503081, -8.673617379884035472E-16, -17.78317311657917088 ) ) ;
#39093 = CARTESIAN_POINT ( 'NONE',  ( -36.67995261982857613, 463.9785544991901247, 19.62073859179952606 ) ) ;
#39094 = CARTESIAN_POINT ( 'NONE',  ( 67.59883368830136874, -59.99999999999988631, -35.88524404060949990 ) ) ;
#39095 = CARTESIAN_POINT ( 'NONE',  ( -77.17139058806502305, -60.31594504996868977, 150.0157547586008775 ) ) ;
#39096 = ORIENTED_EDGE ( 'NONE', *, *, #46430, .F. ) ;
#39097 = CARTESIAN_POINT ( 'NONE',  ( 25.54731711030018815, -59.99999999999990763, 43.65505808401614019 ) ) ;
#39098 = CARTESIAN_POINT ( 'NONE',  ( 108.5906273926863861, -57.66325265620239549, 198.2982773438044148 ) ) ;
#39099 = CARTESIAN_POINT ( 'NONE',  ( 9.491091496279695579E-16, 54.30758622938872549, 7.749999999999999112 ) ) ;
#39100 = CONICAL_SURFACE ( 'NONE', #68354, 4.172000000000001485, 0.9599310885968750373 ) ;
#39101 = CARTESIAN_POINT ( 'NONE',  ( 38.87981064652338148, 307.2829811854333002, -7.103582886926979256 ) ) ;
#39102 = EDGE_CURVE ( 'NONE', #104331, #91175, #70860, .T. ) ;
#39103 = CARTESIAN_POINT ( 'NONE',  ( -13.24448459474634809, 8.079006937257503296, 8.710096806171129913 ) ) ;
#39104 = ORIENTED_EDGE ( 'NONE', *, *, #51335, .T. ) ;
#39105 = FACE_OUTER_BOUND ( 'NONE', #34829, .T. ) ;
#39106 = DIRECTION ( 'NONE',  ( -1.000000000000000000, -1.224606353822377258E-16, -0.000000000000000000 ) ) ;
#39108 = CARTESIAN_POINT ( 'NONE',  ( -102.3071268033655059, -37.82052401323348079, 161.0073083074867952 ) ) ;
#39107 = DIRECTION ( 'NONE',  ( 0.000000000000000000, -1.000000000000000000, 0.000000000000000000 ) ) ;
#39109 = CARTESIAN_POINT ( 'NONE',  ( -2.977408999572650039, -18.68750000204838102, -7.188101187500001821 ) ) ;
#39111 = EDGE_CURVE ( 'NONE', #33159, #30622, #30741, .T. ) ;
#39110 = DIRECTION ( 'NONE',  ( 0.000000000000000000, -1.000000000000000000, 0.000000000000000000 ) ) ;
#39112 = CARTESIAN_POINT ( 'NONE',  ( 6.503370466877179012, 41.93912984867880311, -59.84719185825785104 ) ) ;
#39113 = CARTESIAN_POINT ( 'NONE',  ( -13.00000000000003730, 249.9999999999999432, -4.000000000000002665 ) ) ;
#39114 = SURFACE_STYLE_FILL_AREA ( #80075 ) ;
#39115 = B_SPLINE_CURVE_WITH_KNOTS ( 'NONE', 3,
 ( #59306, #35050, #43112, #3184, #85163, #75999, #28554, #11250, #93255, #93792, #85715, #19419, #61437, #67915, #10722, #2636, #92176, #27505, #51180, #59845, #84101, #3725 ),
 .UNSPECIFIED., .F., .F.,
 ( 4, 2, 2, 2, 2, 2, 2, 2, 2, 2, 4 ),
 ( 0.007089767286567579853, 0.007341907183935019073, 0.007594047081302459160, 0.008098326876037337599, 0.008350466773404773349, 0.008602606670772209099, 0.009106886465507085804, 0.009611166260241964243, 0.01011544605497684095, 0.01061972584971171939, 0.01112400564444659609 ),
 .UNSPECIFIED. ) ;
#39116 = ORIENTED_EDGE ( 'NONE', *, *, #19424, .F. ) ;
#39117 = CARTESIAN_POINT ( 'NONE',  ( -6.924711584187146052, 40.92328497002484511, -70.90711766174086961 ) ) ;
#39118 = CONICAL_SURFACE ( 'NONE', #94233, 5.000000000000010658, 0.9599310885968697082 ) ;
#39119 =( GEOMETRIC_REPRESENTATION_CONTEXT ( 3 ) GLOBAL_UNCERTAINTY_ASSIGNED_CONTEXT ( ( #93459 ) ) GLOBAL_UNIT_ASSIGNED_CONTEXT ( ( #86710, #21977, #78581 ) ) REPRESENTATION_CONTEXT ( 'NONE', 'WORKASPACE' ) );
#39121 = CARTESIAN_POINT ( 'NONE',  ( 26.57462979862440022, -36.00149129685673444, 31.51357150688723863 ) ) ;
#39120 = CARTESIAN_POINT ( 'NONE',  ( 31.83945028356544071, 465.6738295161419501, 10.98138951113134709 ) ) ;
#39122 = DIRECTION ( 'NONE',  ( 0.000000000000000000, 0.000000000000000000, -1.000000000000000000 ) ) ;
#39123 = ORIENTED_EDGE ( 'NONE', *, *, #20913, .T. ) ;
#39124 = VERTEX_POINT ( 'NONE', #58382 ) ;
#39125 = PRODUCT_DEFINITION_SHAPE ( 'NONE', 'NONE',  #106820 ) ;
#39126 = VECTOR ( 'NONE', #103211, 1000.000000000000227 ) ;
#39128 = CARTESIAN_POINT ( 'NONE',  ( -0.4146333384834792746, 43.19860944066726205, -18.68223018281585368 ) ) ;
#39127 = CARTESIAN_POINT ( 'NONE',  ( 8.099999999999999645, 3.752776749732565253, 6.499999999999997335 ) ) ;
#39129 = VECTOR ( 'NONE', #92099, 1000.000000000000000 ) ;
#39130 = PRESENTATION_STYLE_ASSIGNMENT (( #97867 ) ) ;
#39131 = CARTESIAN_POINT ( 'NONE',  ( -44.22225178597525286, 464.2590902508154613, 9.202154635652870951 ) ) ;
#39132 = CARTESIAN_POINT ( 'NONE',  ( -3.313708498984760276, -19.71875000409677270, -8.000000000000000000 ) ) ;
#39133 = CARTESIAN_POINT ( 'NONE',  ( -30.00000000000000355, 490.2058330551859626, 6.957713811045728391 ) ) ;
#39134 = CARTESIAN_POINT ( 'NONE',  ( 0.000000000000000000, 60.00000000000000000, 0.000000000000000000 ) ) ;
#39135 = EDGE_LOOP ( 'NONE', ( #101594, #61827, #61116, #80224, #17606, #74106 ) ) ;
#39136 = CARTESIAN_POINT ( 'NONE',  ( 33.23733598311309123, -59.99999999999999289, -40.52796009714472802 ) ) ;
#39137 = CARTESIAN_POINT ( 'NONE',  ( 22.19904875965656643, 26.05953402208906411, -31.21225605184647378 ) ) ;
#39138 = AXIS2_PLACEMENT_3D ( 'NONE', #105410, #175, #89236 ) ;
#39139 = CARTESIAN_POINT ( 'NONE',  ( -0.000000000000000000, 46.03420836107012093, -33.38430095398285147 ) ) ;
#39140 = AXIS2_PLACEMENT_3D ( 'NONE', #75659, #91853, #77268 ) ;
#39141 = CARTESIAN_POINT ( 'NONE',  ( -3.122376895879317882, -5.000000000000000000, -73.30448186995486992 ) ) ;
#39142 = DIRECTION ( 'NONE',  ( 0.000000000000000000, 0.000000000000000000, -1.000000000000000000 ) ) ;
#39143 = ORIENTED_EDGE ( 'NONE', *, *, #53045, .F. ) ;
#39144 = ORIENTED_EDGE ( 'NONE', *, *, #85532, .F. ) ;
#39145 = EDGE_LOOP ( 'NONE', ( #22868, #35040, #50629, #99917 ) ) ;
#39146 = FILL_AREA_STYLE ('',( #22969 ) ) ;
#39147 = PRESENTATION_STYLE_ASSIGNMENT (( #48261 ) ) ;
#39148 = CARTESIAN_POINT ( 'NONE',  ( -36.37624454313544220, 28.20756701710648784, 11.81579238979949587 ) ) ;
#39149 = CARTESIAN_POINT ( 'NONE',  ( 32.64148745189749690, 347.3146175066438559, 20.23427429214728690 ) ) ;
#39150 = CARTESIAN_POINT ( 'NONE',  ( 8.559508646656349029, 51.83514083332403999, -1.531152949374623873 ) ) ;
#39151 = DIRECTION ( 'NONE',  ( -1.000000000000000000, -0.000000000000000000, -0.000000000000000000 ) ) ;
#39152 = DIRECTION ( 'NONE',  ( 0.000000000000000000, -1.000000000000000000, 0.000000000000000000 ) ) ;
#39153 = ORIENTED_EDGE ( 'NONE', *, *, #25289, .T. ) ;
#39154 = CARTESIAN_POINT ( 'NONE',  ( 2.617478844990903664, 48.00000000000000000, -75.26027323389595836 ) ) ;
#39155 = ORIENTED_EDGE ( 'NONE', *, *, #89521, .T. ) ;
#39156 = FACE_OUTER_BOUND ( 'NONE', #17478, .T. ) ;
#39157 = CARTESIAN_POINT ( 'NONE',  ( 19.70764564238367100, 304.7954121406193053, 9.925013215726757210 ) ) ;
#39158 = CARTESIAN_POINT ( 'NONE',  ( -40.49428179616828061, 485.6422782434504484, -4.370491944118827909 ) ) ;
#39159 = CIRCLE ( 'NONE', #99388, 5.000000000000010658 ) ;
#39160 = CARTESIAN_POINT ( 'NONE',  ( 6.326592304916282217, -6.579439845142166732, -2.267162479624768689 ) ) ;
#39161 = CARTESIAN_POINT ( 'NONE',  ( 64.47128789977597307, -32.52970818110316031, 81.05340315809206686 ) ) ;
#39162 = ORIENTED_EDGE ( 'NONE', *, *, #90958, .T. ) ;
#39163 = FACE_OUTER_BOUND ( 'NONE', #44578, .T. ) ;
#39164 = AXIS2_PLACEMENT_3D ( 'NONE', #21509, #13898, #88874 ) ;
#39165 = ADVANCED_FACE ( 'NONE', ( #50282 ), #41666, .F. ) ;
#39166 = CARTESIAN_POINT ( 'NONE',  ( -6.013035130119651406, 11.20840185166977498, 3.585725784831610419 ) ) ;
#39167 = EDGE_CURVE ( 'NONE', #23893, #53830, #80662, .T. ) ;
#39168 = DIRECTION ( 'NONE',  ( 0.000000000000000000, -1.000000000000000000, 0.000000000000000000 ) ) ;
#39169 = ORIENTED_EDGE ( 'NONE', *, *, #54674, .T. ) ;
#39170 =( NAMED_UNIT ( * ) PLANE_ANGLE_UNIT ( ) SI_UNIT ( $, .RADIAN. ) );
#39171 = CONICAL_SURFACE ( 'NONE', #16831, 13.50000000000000178, 1.047197551196596077 ) ;
#39172 = CARTESIAN_POINT ( 'NONE',  ( 17.61650669486618881, -3.999999999999998224, 0.000000000000000000 ) ) ;
#39173 = CARTESIAN_POINT ( 'NONE',  ( 8.000000000000000000, -29.18750000409677270, 0.000000000000000000 ) ) ;
#39174 = CARTESIAN_POINT ( 'NONE',  ( 8.000000000000000000, -3.000000000000000000, -2.094395098902536834 ) ) ;
#39175 = CARTESIAN_POINT ( 'NONE',  ( 86.66893764443852888, -46.47199666242754290, 190.4867299908505061 ) ) ;
#39176 = AXIS2_PLACEMENT_3D ( 'NONE', #649, #8779, #41685 ) ;
#39177 = SURFACE_STYLE_USAGE ( .BOTH. , #47238 ) ;
#39178 = STYLED_ITEM ( 'NONE', ( #75617 ), #66937 ) ;
#39179 = CARTESIAN_POINT ( 'NONE',  ( -9.971054623845207132, 7.543597283302578838, 4.999999999999846345 ) ) ;
#39180 = CARTESIAN_POINT ( 'NONE',  ( -2.837346585668845567, 6.232092946297383307, -6.171287963165197787 ) ) ;
#39181 = ORIENTED_EDGE ( 'NONE', *, *, #17009, .T. ) ;
#39182 = CARTESIAN_POINT ( 'NONE',  ( 0.000000000000000000, -4.000000000000003553, 112.0000000000000000 ) ) ;
#39183 = FACE_OUTER_BOUND ( 'NONE', #43169, .T. ) ;
#39185 =( BOUNDED_SURFACE ( )  B_SPLINE_SURFACE ( 3, 2, ( 
 ( #100460, #75103, #31641 ),
 ( #23022, #26619, #72597 ),
 ( #59492, #67046, #6801 ),
 ( #17970, #50827, #92358 ),
 ( #105501, #18509, #51370 ),
 ( #39195, #72072, #104982 ),
 ( #31126, #66499, #64010 ),
 ( #64523, #96887, #55853 ) ),
 .UNSPECIFIED., .F., .F., .F. ) 
 B_SPLINE_SURFACE_WITH_KNOTS ( ( 4, 2, 2, 4 ),
 ( 3, 3 ),
 ( 0.006715319241923278261, 0.008391857906694557070, 0.009230127239080197776, 0.01006839657146583675 ),
 ( 0.000000000000000000, 0.8433639608880305616 ),
 .UNSPECIFIED. ) 
 GEOMETRIC_REPRESENTATION_ITEM ( )  RATIONAL_B_SPLINE_SURFACE ( (
 ( 1.000000000000000000, 0.7529844148637855339, 0.9226169142906758269),
 ( 1.000000000000000000, 0.7706979643850044859, 0.9281660747619107088),
 ( 1.000000000000000000, 0.7822228831078168465, 0.9317765100015680257),
 ( 1.000000000000000000, 0.7860222813518789042, 0.9329667553854859019),
 ( 1.000000000000000000, 0.7850393348246805791, 0.9326588256841275015),
 ( 1.000000000000000000, 0.7784080814446623364, 0.9305814391565394583),
 ( 1.000000000000000000, 0.7727688943794591703, 0.9288148393051297580),
 ( 1.000000000000000000, 0.7650504347444155862, 0.9263968614145721148) ) ) 
 REPRESENTATION_ITEM ( '' )  SURFACE ( )  );
#39184 = CARTESIAN_POINT ( 'NONE',  ( 19.62218219363544236, -60.00000000000000000, 40.16747987769195305 ) ) ;
#39186 = CARTESIAN_POINT ( 'NONE',  ( -99.66052428874382940, -30.00000000000000355, 186.9484570685918357 ) ) ;
#39187 = CIRCLE ( 'NONE', #20289, 3.309500000000001663 ) ;
#39188 = DIRECTION ( 'NONE',  ( 0.000000000000000000, -1.000000000000000000, 0.000000000000000000 ) ) ;
#39189 = AXIS2_PLACEMENT_3D ( 'NONE', #48728, #81619, #72490 ) ;
#39190 = CARTESIAN_POINT ( 'NONE',  ( 52.17905232536506333, -57.67658488488999069, 83.19886591059480452 ) ) ;
#39192 = DIRECTION ( 'NONE',  ( 0.5735764363510442720, -0.8191520442889930198, 1.003171929053526349E-16 ) ) ;
#39191 = CARTESIAN_POINT ( 'NONE',  ( 13.09294039136050181, 8.329457025090279743, -8.860870387164958117 ) ) ;
#39193 = EDGE_CURVE ( 'NONE', #8349, #59362, #68615, .T. ) ;
#39194 =( NAMED_UNIT ( * ) PLANE_ANGLE_UNIT ( ) SI_UNIT ( $, .RADIAN. ) );
#39195 = CARTESIAN_POINT ( 'NONE',  ( -30.00000000000000355, 461.9652624853977159, 12.11314247086471596 ) ) ;
#39196 = DIRECTION ( 'NONE',  ( -1.000000000000000000, 0.000000000000000000, 0.000000000000000000 ) ) ;
#39197 = CARTESIAN_POINT ( 'NONE',  ( -20.56724024172385512, -59.99999999999999289, 40.29721615606709406 ) ) ;
#39198 = CIRCLE ( 'NONE', #99447, 3.309500000000007880 ) ;
#39199 = CIRCLE ( 'NONE', #97756, 3.309500000000001663 ) ;
#39200 =( GEOMETRIC_REPRESENTATION_CONTEXT ( 3 ) GLOBAL_UNCERTAINTY_ASSIGNED_CONTEXT ( ( #6190 ) ) GLOBAL_UNIT_ASSIGNED_CONTEXT ( ( #101582, #51423, #26663 ) ) REPRESENTATION_CONTEXT ( 'NONE', 'WORKASPACE' ) );
#39201 = CARTESIAN_POINT ( 'NONE',  ( 0.000000000000000000, 115.0000000000000000, 0.000000000000000000 ) ) ;
#39202 = CARTESIAN_POINT ( 'NONE',  ( -86.62987691488393693, -16.99726452457568726, 185.2254060544966023 ) ) ;
#39203 = ORIENTED_EDGE ( 'NONE', *, *, #50497, .T. ) ;
#39204 = CARTESIAN_POINT ( 'NONE',  ( 17.50000000000006040, 50.79875088430608798, 63.37001662959071524 ) ) ;
#39205 = CARTESIAN_POINT ( 'NONE',  ( -3.352941176470589646, -48.79941684889505638, 104.5794940929807524 ) ) ;
#39206 = CARTESIAN_POINT ( 'NONE',  ( -13.32466295366451448, -29.03150478239603416, 28.80490044896601276 ) ) ;
#39207 =( GEOMETRIC_REPRESENTATION_CONTEXT ( 3 ) GLOBAL_UNCERTAINTY_ASSIGNED_CONTEXT ( ( #2748 ) ) GLOBAL_UNIT_ASSIGNED_CONTEXT ( ( #97020, #47923, #72222 ) ) REPRESENTATION_CONTEXT ( 'NONE', 'WORKASPACE' ) );
#39209 = EDGE_CURVE ( 'NONE', #81288, #59054, #18239, .T. ) ;
#39208 = CARTESIAN_POINT ( 'NONE',  ( -104.2214876769391054, -60.00000000000002132, 190.2337882128940407 ) ) ;
#39210 = EDGE_CURVE ( 'NONE', #49781, #23997, #90233, .T. ) ;
#39211 = VERTEX_POINT ( 'NONE', #67550 ) ;
#39212 = CARTESIAN_POINT ( 'NONE',  ( 26.01891250190696425, 35.07265168611927209, 8.182742802489435974 ) ) ;
#39213 = PRESENTATION_LAYER_ASSIGNMENT (  '', '', ( #11621 ) ) ;
#39214 = CARTESIAN_POINT ( 'NONE',  ( -7.464071982070691114, -3.053493056027888120, -19.53076229012244269 ) ) ;
#39215 = CARTESIAN_POINT ( 'NONE',  ( 0.000000000000000000, 0.000000000000000000, 0.000000000000000000 ) ) ;
#39216 = DIRECTION ( 'NONE',  ( 0.000000000000000000, 1.000000000000000000, 0.000000000000000000 ) ) ;
#39217 = CARTESIAN_POINT ( 'NONE',  ( 0.000000000000000000, 4.898587196589412829E-16, -4.000000000000000000 ) ) ;
#39218 = CARTESIAN_POINT ( 'NONE',  ( 73.07493821064443296, -59.99999999999999289, 163.1432788538008367 ) ) ;
#39219 = AXIS2_PLACEMENT_3D ( 'NONE', #105448, #31586, #64473 ) ;
#39220 = CARTESIAN_POINT ( 'NONE',  ( -22.91651842568165165, 295.0901107613288445, -9.949346074078587066 ) ) ;
#39221 = VERTEX_POINT ( 'NONE', #92332 ) ;
#39222 = CYLINDRICAL_SURFACE ( 'NONE', #55031, 8.000000000000000000 ) ;
#39223 = CARTESIAN_POINT ( 'NONE',  ( -5.656854249492379694, -21.12500000409676915, -5.656854249492380582 ) ) ;
#39225 =( NAMED_UNIT ( * ) PLANE_ANGLE_UNIT ( ) SI_UNIT ( $, .RADIAN. ) );
#39224 = CARTESIAN_POINT ( 'NONE',  ( 32.49824730387988581, -59.99999999999999289, 47.28149596916139075 ) ) ;
#39226 = CARTESIAN_POINT ( 'NONE',  ( 3.668358303306901380, -1.103610535301068563, 104.6014313550541175 ) ) ;
#39227 = ADVANCED_FACE ( 'NONE', ( #10870 ), #93418, .T. ) ;
#39228 = CARTESIAN_POINT ( 'NONE',  ( -4.551587301587301404, -1.200583151104944513, 104.4018401814738013 ) ) ;
#39229 = ORIENTED_EDGE ( 'NONE', *, *, #96902, .T. ) ;
#39230 = CARTESIAN_POINT ( 'NONE',  ( -23.65589420198908499, 306.0724382492799123, 10.20579241568104578 ) ) ;
#39231 = ORIENTED_EDGE ( 'NONE', *, *, #40212, .T. ) ;
#39232 = CYLINDRICAL_SURFACE ( 'NONE', #75880, 5.000000000000000888 ) ;
#39233 = ADVANCED_FACE ( 'NONE', ( #36804 ), #13639, .F. ) ;
#39234 = FACE_OUTER_BOUND ( 'NONE', #15679, .T. ) ;
#39235 = DIRECTION ( 'NONE',  ( 0.000000000000000000, 1.000000000000000000, 0.000000000000000000 ) ) ;
#39236 = VERTEX_POINT ( 'NONE', #84788 ) ;
#39237 = CARTESIAN_POINT ( 'NONE',  ( 1.724765290377481275, -5.000000000000002665, -69.73714729961211845 ) ) ;
#39238 = CARTESIAN_POINT ( 'NONE',  ( 6.611670918688536958, -11.93296314122835078, 9.735702799543512143 ) ) ;
#39239 = CARTESIAN_POINT ( 'NONE',  ( -113.9444010383659105, -60.00000000002935252, 184.0739081374410659 ) ) ;
#39240 = CARTESIAN_POINT ( 'NONE',  ( 6.222583235320747974, 4.088462131826499757, -6.500000000000000888 ) ) ;
#39241 = CARTESIAN_POINT ( 'NONE',  ( 82.53305096376368510, -59.99999999999992895, 198.4978234872852738 ) ) ;
#39242 = CARTESIAN_POINT ( 'NONE',  ( -18.99999999999999645, -4.000000000000000000, -2.500000000000000000 ) ) ;
#39243 = CARTESIAN_POINT ( 'NONE',  ( 3.616665348617805752E-21, 26.07813853931757464, -38.25000000000000000 ) ) ;
#39245 = CARTESIAN_POINT ( 'NONE',  ( 11.20590345621723039, -29.02957503740841361, 28.75286772522219536 ) ) ;
#39244 = CARTESIAN_POINT ( 'NONE',  ( -106.6793529335496515, -14.21045842199435860, 163.7930604915816559 ) ) ;
#39246 = EDGE_CURVE ( 'NONE', #76952, #8366, #84255, .T. ) ;
#39247 = CARTESIAN_POINT ( 'NONE',  ( 82.46348125551625685, -37.99999999999998579, 10.05151166824885500 ) ) ;
#39248 = AXIS2_PLACEMENT_3D ( 'NONE', #30648, #24158, #57004 ) ;
#39249 = CARTESIAN_POINT ( 'NONE',  ( -47.77545754411675460, -22.22741228947390013, 42.11508245023937747 ) ) ;
#39250 = CARTESIAN_POINT ( 'NONE',  ( -0.08425897456643699490, 34.17188553058037570, -29.74999999999992184 ) ) ;
#39251 = ORIENTED_EDGE ( 'NONE', *, *, #82549, .T. ) ;
#39252 = EDGE_CURVE ( 'NONE', #21098, #51812, #86446, .T. ) ;
#39253 = LINE ( 'NONE', #72128, #37075 ) ;
#39254 = CARTESIAN_POINT ( 'NONE',  ( -1.106403059298377123, 17.29028464265184795, 49.90220135503628285 ) ) ;
#39255 =( NAMED_UNIT ( * ) SI_UNIT ( $, .STERADIAN. ) SOLID_ANGLE_UNIT ( ) );
#39256 = CARTESIAN_POINT ( 'NONE',  ( 36.08349330513379982, 1.593028355512270962E-15, 0.000000000000000000 ) ) ;
#39257 = EDGE_LOOP ( 'NONE', ( #84359, #90275, #3842, #72501 ) ) ;
#39258 = CARTESIAN_POINT ( 'NONE',  ( -8.830818839454250835, -4.082547224762430815, 14.50827515792006217 ) ) ;
#39259 = VECTOR ( 'NONE', #48160, 1000.000000000000114 ) ;
#39260 = VERTEX_POINT ( 'NONE', #2795 ) ;
#39261 = CARTESIAN_POINT ( 'NONE',  ( 101.2363978237404751, -29.99999999999453948, 198.5817383530316818 ) ) ;
#39262 = DIRECTION ( 'NONE',  ( 0.000000000000000000, 0.000000000000000000, 1.000000000000000000 ) ) ;
#39263 = EDGE_CURVE ( 'NONE', #105278, #85106, #66904, .T. ) ;
#39264 = CARTESIAN_POINT ( 'NONE',  ( 5.500000000000325073, 41.99999999999999289, -59.88032989331690459 ) ) ;
#39265 = CARTESIAN_POINT ( 'NONE',  ( 93.01436231026998769, -30.00000000000000000, 106.1217855030838280 ) ) ;
#39266 = CARTESIAN_POINT ( 'NONE',  ( 0.000000000000000000, 0.000000000000000000, 8.000000000000000000 ) ) ;
#39267 = EDGE_LOOP ( 'NONE', ( #55869, #15411, #49359, #30849 ) ) ;
#39268 = EDGE_LOOP ( 'NONE', ( #19409, #2231, #33594, #40717 ) ) ;
#39269 = VERTEX_POINT ( 'NONE', #51872 ) ;
#39270 = CIRCLE ( 'NONE', #84056, 5.000000000000010658 ) ;
#39271 = FACE_OUTER_BOUND ( 'NONE', #82578, .T. ) ;
#39272 = CARTESIAN_POINT ( 'NONE',  ( -43.64277943678018801, 435.6477504884530276, 9.088095002171668213 ) ) ;
#39273 = COLOUR_RGB ( '', 0.40784314, 0.44705882, 0.49803922) ;
#39274 = CARTESIAN_POINT ( 'NONE',  ( 0.000000000000000000, 294.8518027762758038, -10.00000000000000178 ) ) ;
#39275 = EDGE_LOOP ( 'NONE', ( #58644, #98220, #43426, #62949 ) ) ;
#39276 = DIRECTION ( 'NONE',  ( -1.000000000000000000, -0.000000000000000000, -0.000000000000000000 ) ) ;
#39277 = VERTEX_POINT ( 'NONE', #69153 ) ;
#39278 = DIRECTION ( 'NONE',  ( -0.000000000000000000, -0.000000000000000000, 1.000000000000000000 ) ) ;
#39279 = CARTESIAN_POINT ( 'NONE',  ( 79.84666553715925374, -38.77034851676472726, 192.7062979745145981 ) ) ;
#39280 = CARTESIAN_POINT ( 'NONE',  ( 13.95195489779432307, 6.945883722228267665, 7.976544621831442861 ) ) ;
#39281 = CARTESIAN_POINT ( 'NONE',  ( 85.46358041537231998, -52.72117977435281944, -0.4810073681625586794 ) ) ;
#39282 = CARTESIAN_POINT ( 'NONE',  ( 76.42237582680409957, -38.00000000000002132, 125.4842420748356346 ) ) ;
#39283 = CARTESIAN_POINT ( 'NONE',  ( 36.84238428740148663, 310.7453882974721751, 13.75124073885965892 ) ) ;
#39284 = DIRECTION ( 'NONE',  ( 0.000000000000000000, 0.000000000000000000, 1.000000000000000000 ) ) ;
#39285 = FACE_OUTER_BOUND ( 'NONE', #19483, .T. ) ;
#39286 = DIRECTION ( 'NONE',  ( 0.000000000000000000, 1.000000000000000000, 0.000000000000000000 ) ) ;
#39287 = DIRECTION ( 'NONE',  ( 0.000000000000000000, 0.000000000000000000, 1.000000000000000000 ) ) ;
#39288 = ORIENTED_EDGE ( 'NONE', *, *, #92468, .T. ) ;
#39289 = ADVANCED_FACE ( 'NONE', ( #50799 ), #61055, .T. ) ;
#39290 = DIRECTION ( 'NONE',  ( -1.000000000000000000, -1.224606353822377258E-16, -0.000000000000000000 ) ) ;
#39291 = CARTESIAN_POINT ( 'NONE',  ( -36.05619378504946582, 461.6897174690496968, 3.777659454257536353 ) ) ;
#39292 = CARTESIAN_POINT ( 'NONE',  ( -3.949145016516434126, 15.90303839293037669, 5.000000000000000888 ) ) ;
#39293 = ORIENTED_EDGE ( 'NONE', *, *, #105111, .F. ) ;
#39294 = CIRCLE ( 'NONE', #66840, 8.000000000000000000 ) ;
#39295 = CARTESIAN_POINT ( 'NONE',  ( 32.17646412119353272, 464.6980787822281513, 10.84896803613063021 ) ) ;
#39296 = CARTESIAN_POINT ( 'NONE',  ( -26.71365596510858964, 306.5311303962027978, 10.78021858148648349 ) ) ;
#39297 = CARTESIAN_POINT ( 'NONE',  ( -3.991147588110737665, -48.94961024798170257, 104.5610969444638698 ) ) ;
#39298 = DIRECTION ( 'NONE',  ( -1.000000000000000000, -0.000000000000000000, -0.000000000000000000 ) ) ;
#39299 = CARTESIAN_POINT ( 'NONE',  ( -8.000000000000001776, -17.65624999999999289, 3.313708498984758943 ) ) ;
#39300 = CARTESIAN_POINT ( 'NONE',  ( -3.883979799181499715, -15.02869017758564141, 34.49744884119316879 ) ) ;
#39301 = ADVANCED_FACE ( 'NONE', ( #3340 ), #83705, .T. ) ;
#39302 = MECHANICAL_DESIGN_GEOMETRIC_PRESENTATION_REPRESENTATION (  '', ( #54739 ), #75376 ) ;
#39303 = CARTESIAN_POINT ( 'NONE',  ( 19.83463548332445825, 303.8035096162420245, 9.926734387303332241 ) ) ;
#39304 = ORIENTED_EDGE ( 'NONE', *, *, #36452, .F. ) ;
#39305 = CARTESIAN_POINT ( 'NONE',  ( 84.57259215197804281, -46.56816764461522951, 186.4401838890023555 ) ) ;
#39306 = CIRCLE ( 'NONE', #84100, 4.000000000000007105 ) ;
#39307 =( NAMED_UNIT ( * ) SI_UNIT ( $, .STERADIAN. ) SOLID_ANGLE_UNIT ( ) );
#39308 = VERTEX_POINT ( 'NONE', #27660 ) ;
#39309 = CARTESIAN_POINT ( 'NONE',  ( 96.55249329909841549, -57.67139621948945205, 45.80016927409987204 ) ) ;
#39310 = CARTESIAN_POINT ( 'NONE',  ( -18.99999999999999289, 4.000000000000000888, -1.500000000000001332 ) ) ;
#39311 = DIRECTION ( 'NONE',  ( 0.000000000000000000, 0.000000000000000000, 1.000000000000000000 ) ) ;
#39312 = CARTESIAN_POINT ( 'NONE',  ( 29.07948315939635719, 13.68628896012809903, 39.75806671536113157 ) ) ;
#39313 = ADVANCED_FACE ( 'NONE', ( #76149 ), #15233, .T. ) ;
#39315 = B_SPLINE_CURVE_WITH_KNOTS ( 'NONE', 3,
 ( #84213, #59419, #85828, #28139 ),
 .UNSPECIFIED., .F., .F.,
 ( 4, 4 ),
 ( 0.000000000000000000, 0.001019617110105362117 ),
 .UNSPECIFIED. ) ;
#39314 = AXIS2_PLACEMENT_3D ( 'NONE', #88008, #70756, #96096 ) ;
#39316 = CARTESIAN_POINT ( 'NONE',  ( 28.46814188645437582, 18.16755603797503937, 40.55128649371861371 ) ) ;
#39317 = CARTESIAN_POINT ( 'NONE',  ( 7.137815226410046066, -3.000000000000000000, 4.175893272574714210 ) ) ;
#39318 = DIRECTION ( 'NONE',  ( 0.000000000000000000, -1.000000000000000000, 0.000000000000000000 ) ) ;
#39319 = AXIS2_PLACEMENT_3D ( 'NONE', #101730, #27897, #79049 ) ;
#39321 = LINE ( 'NONE', #63053, #18995 ) ;
#39320 = DIRECTION ( 'NONE',  ( -1.000000000000000000, -0.000000000000000000, -0.000000000000000000 ) ) ;
#39322 = EDGE_CURVE ( 'NONE', #71278, #94858, #13443, .T. ) ;
#39323 = CARTESIAN_POINT ( 'NONE',  ( 16.05785784214673129, 4.775831776474256607, -3.710403933782447261 ) ) ;
#39324 = DIRECTION ( 'NONE',  ( -0.000000000000000000, 1.000000000000000000, -0.000000000000000000 ) ) ;
#39325 = CARTESIAN_POINT ( 'NONE',  ( 9.999999999999998224, 15.00000000000000000, -1.734723475976806306E-15 ) ) ;
#39326 = DIRECTION ( 'NONE',  ( -0.5735764363510497121, 0.8191520442889892450, 1.003171929053521665E-16 ) ) ;
#39327 = AXIS2_PLACEMENT_3D ( 'NONE', #58305, #41593, #92798 ) ;
#39328 = FACE_OUTER_BOUND ( 'NONE', #20166, .T. ) ;
#39329 = PRESENTATION_LAYER_ASSIGNMENT (  '', '', ( #49619 ) ) ;
#39330 = VERTEX_POINT ( 'NONE', #34678 ) ;
#39331 = CARTESIAN_POINT ( 'NONE',  ( -5.919014529058259200, -3.357354825248717523E-15, 18.71571423408288126 ) ) ;
#39332 = SURFACE_STYLE_FILL_AREA ( #6396 ) ;
#39333 = CARTESIAN_POINT ( 'NONE',  ( -14.50943445205030002, -17.10998225175372411, -34.39758505370421204 ) ) ;
#39336 = EDGE_CURVE ( 'NONE', #51812, #11400, #37558, .T. ) ;
#39335 = CARTESIAN_POINT ( 'NONE',  ( -57.70311871300574325, -34.58944410828412686, -25.91705731457850703 ) ) ;
#39334 = CARTESIAN_POINT ( 'NONE',  ( 20.05074616892822448, 67.05096163904791240, -10.02537308446411402 ) ) ;
#39337 = ORIENTED_EDGE ( 'NONE', *, *, #105061, .F. ) ;
#39338 = CARTESIAN_POINT ( 'NONE',  ( 3.295171437449430307, 7.213553046161576887, -7.590212325761433121 ) ) ;
#39339 = VECTOR ( 'NONE', #70414, 1000.000000000000000 ) ;
#39340 = ORIENTED_EDGE ( 'NONE', *, *, #31946, .F. ) ;
#39341 = AXIS2_PLACEMENT_3D ( 'NONE', #83901, #1909, #49397 ) ;
#39342 = CIRCLE ( 'NONE', #77216, 5.000000000000002665 ) ;
#39343 = PRESENTATION_STYLE_ASSIGNMENT (( #6405 ) ) ;
#39344 = CARTESIAN_POINT ( 'NONE',  ( -13.00000000000003730, 249.9999999999999432, 0.000000000000000000 ) ) ;
#39345 = CARTESIAN_POINT ( 'NONE',  ( -92.73296030468360129, -59.99999999999999289, -5.965765328958698710 ) ) ;
#39346 = ORIENTED_EDGE ( 'NONE', *, *, #40161, .T. ) ;
#39347 = DIRECTION ( 'NONE',  ( 0.000000000000000000, -1.000000000000000000, 0.000000000000000000 ) ) ;
#39348 = CARTESIAN_POINT ( 'NONE',  ( -7.435027261853919711, 54.30343294327740722, -2.228677732260373912 ) ) ;
#39349 = CARTESIAN_POINT ( 'NONE',  ( 100.2677560643444394, -52.76192752009863085, 194.0135600122352741 ) ) ;
#39351 = LINE ( 'NONE', #29685, #75357 ) ;
#39350 = DIRECTION ( 'NONE',  ( -1.000000000000000000, -0.000000000000000000, -0.000000000000000000 ) ) ;
#39352 = EDGE_CURVE ( 'NONE', #97780, #7894, #75510, .T. ) ;
#39353 = CARTESIAN_POINT ( 'NONE',  ( -82.94221917796012633, -36.01794431359551396, 163.7362876441995923 ) ) ;
#39354 = ORIENTED_EDGE ( 'NONE', *, *, #96453, .F. ) ;
#39355 = ORIENTED_EDGE ( 'NONE', *, *, #42069, .T. ) ;
#39356 = ORIENTED_EDGE ( 'NONE', *, *, #82631, .T. ) ;
#39357 = CARTESIAN_POINT ( 'NONE',  ( 31.38691588366916818, 427.9687656044268920, 23.57225804472849617 ) ) ;
#39358 = EDGE_CURVE ( 'NONE', #20770, #55118, #65195, .T. ) ;
#39359 = CARTESIAN_POINT ( 'NONE',  ( -5.000000000000038192, -13.46492586503062050, 12.82257630554777883 ) ) ;
#39360 =( NAMED_UNIT ( * ) SI_UNIT ( $, .STERADIAN. ) SOLID_ANGLE_UNIT ( ) );
#39361 = ORIENTED_EDGE ( 'NONE', *, *, #9184, .T. ) ;
#39362 = AXIS2_PLACEMENT_3D ( 'NONE', #9718, #51782, #84695 ) ;
#39363 = CARTESIAN_POINT ( 'NONE',  ( -114.1029252960232725, -57.67113437255621022, 166.8310794691209367 ) ) ;
#39364 = CARTESIAN_POINT ( 'NONE',  ( 0.4973051450610294633, -3.866309095671266238, 8.000000000000000000 ) ) ;
#39365 = CARTESIAN_POINT ( 'NONE',  ( 2.262848203703084149, 6.566616684922156999, -6.208169345099793901 ) ) ;
#39366 = CARTESIAN_POINT ( 'NONE',  ( -0.6457708876286766264, 25.22709477130971933, 40.58338319097169489 ) ) ;
#39367 = CARTESIAN_POINT ( 'NONE',  ( 14.34999999999999787, 1.533819458162526451E-15, 0.000000000000000000 ) ) ;
#39368 = CARTESIAN_POINT ( 'NONE',  ( 48.21450566731007825, -29.99999999999995381, -35.59756164575514958 ) ) ;
#39369 = EDGE_CURVE ( 'NONE', #59362, #62868, #96173, .T. ) ;
#39370 = CARTESIAN_POINT ( 'NONE',  ( -74.83603090277703984, -14.21045842199441012, 137.5224045200043577 ) ) ;
#39371 = CARTESIAN_POINT ( 'NONE',  ( -53.53337026754450534, -36.03630593442233021, 55.90610740931312961 ) ) ;
#39372 = ORIENTED_EDGE ( 'NONE', *, *, #92013, .F. ) ;
#39373 = CARTESIAN_POINT ( 'NONE',  ( 0.000000000000000000, 0.000000000000000000, 4.000000000000000000 ) ) ;
#39374 = ORIENTED_EDGE ( 'NONE', *, *, #404, .F. ) ;
#39375 = CARTESIAN_POINT ( 'NONE',  ( -100.3932303477031809, -45.25917866372384424, 192.1829530928476117 ) ) ;
#39376 = CARTESIAN_POINT ( 'NONE',  ( 32.84237740334622657, 485.2251842821286800, 5.746442123025142124 ) ) ;
#39377 = CONICAL_SURFACE ( 'NONE', #13553, 5.000000000000001776, 0.9599310885968803664 ) ;
#39378 = VERTEX_POINT ( 'NONE', #96602 ) ;
#39379 = CARTESIAN_POINT ( 'NONE',  ( 18.93524409176044898, 49.17398178157321098, 62.07515712285433551 ) ) ;
#39380 = CARTESIAN_POINT ( 'NONE',  ( 95.15023610446269231, -38.35584284022535684, 58.97509959524118273 ) ) ;
#39381 = LINE ( 'NONE', #15078, #57081 ) ;
#39382 = CARTESIAN_POINT ( 'NONE',  ( -38.51502786940007184, 460.0233756673457606, 2.043034587342192676 ) ) ;
#39383 = ADVANCED_FACE ( 'NONE', ( #47495 ), #53124, .T. ) ;
#39384 = SURFACE_STYLE_USAGE ( .BOTH. , #96019 ) ;
#39385 = DIRECTION ( 'NONE',  ( 0.000000000000000000, -1.000000000000000000, 0.000000000000000000 ) ) ;
#39386 = CARTESIAN_POINT ( 'NONE',  ( 80.76653117601198062, -30.00000000000000000, 138.6873283208337568 ) ) ;
#39387 = B_SPLINE_SURFACE_WITH_KNOTS ( 'NONE', 3, 3, ( 
 ( #3006, #3550, #12153, #77964, #101177, #36489, #35956, #84995 ),
 ( #27338, #93625, #102236, #45613, #29455, #37545, #45085, #61261 ),
 ( #60737, #28936, #94147, #4079, #20320, #61809, #94702, #11078 ),
 ( #37010, #44004, #76889, #102771, #52608, #62327, #53164, #86081 ),
 ( #93082, #69877, #20849, #68829, #2464, #85537, #86617, #12680 ),
 ( #84464, #101707, #70411, #78485, #27872, #4613, #11617, #44546 ),
 ( #77435, #68280, #51551, #35412, #10557, #43473, #60216, #76350 ),
 ( #46649, #38583, #6721, #80599, #13208, #47170, #71448, #97319 ) ),
 .UNSPECIFIED., .F., .F., .F.,
 ( 4, 2, 2, 4 ),
 ( 4, 2, 2, 4 ),
 ( 0.000000000000000000, 0.2500000000000000000, 0.5000000000000000000, 1.000000000000000000 ),
 ( 0.000000000000000000, 0.2500000000000000000, 0.5000000000000000000, 1.000000000000000000 ),
 .UNSPECIFIED. ) ;
#39388 = CARTESIAN_POINT ( 'NONE',  ( 70.89460441624491693, 6.975173280561618775E-15, 0.000000000000000000 ) ) ;
#39389 = CARTESIAN_POINT ( 'NONE',  ( 4.726289671093704570, 52.17352334379410905, -6.162350474469696415 ) ) ;
#39390 = DIRECTION ( 'NONE',  ( -1.000000000000000000, -1.224606353822377258E-16, -0.000000000000000000 ) ) ;
#39391 = DIRECTION ( 'NONE',  ( 0.000000000000000000, -1.000000000000000000, 0.000000000000000000 ) ) ;
#39392 = ORIENTED_EDGE ( 'NONE', *, *, #30324, .T. ) ;
#39393 = ORIENTED_EDGE ( 'NONE', *, *, #82149, .T. ) ;
#39394 = CARTESIAN_POINT ( 'NONE',  ( 49.82584992942429380, -56.82805176776372491, 56.28939656403482417 ) ) ;
#39395 = CARTESIAN_POINT ( 'NONE',  ( -0.5285826653655552043, 13.43369763208850287, 49.36091062968711896 ) ) ;
#39396 = CARTESIAN_POINT ( 'NONE',  ( 0.000000000000000000, 0.000000000000000000, -8.000000000000000000 ) ) ;
#39397 = CARTESIAN_POINT ( 'NONE',  ( -108.9893057958549605, -38.35643123286386924, 190.1635235720441131 ) ) ;
#39398 = ORIENTED_EDGE ( 'NONE', *, *, #77719, .T. ) ;
#39399 = CARTESIAN_POINT ( 'NONE',  ( 90.74781813830772137, -38.34261101312728215, 6.475050893663723883 ) ) ;
#39400 = CARTESIAN_POINT ( 'NONE',  ( 12.35050418871243139, 20.41302141647243573, -6.749052883688374749 ) ) ;
#39401 = FACE_OUTER_BOUND ( 'NONE', #30312, .T. ) ;
#39402 = CARTESIAN_POINT ( 'NONE',  ( 13.50000000000000178, 0.000000000000000000, 0.000000000000000000 ) ) ;
#39403 = CARTESIAN_POINT ( 'NONE',  ( 98.00862599427638600, -52.71700389358836247, 110.7962579094794933 ) ) ;
#39404 = DIRECTION ( 'NONE',  ( 0.000000000000000000, 0.000000000000000000, 1.000000000000000000 ) ) ;
#39405 = CARTESIAN_POINT ( 'NONE',  ( 22.66566284726422964, 27.53292244466711480, 33.08065323819726444 ) ) ;
#39406 = CARTESIAN_POINT ( 'NONE',  ( -35.52712812490531746, 408.9705615248064419, 7.034401458122156114 ) ) ;
#39407 = SURFACE_STYLE_USAGE ( .BOTH. , #5945 ) ;
#39408 = CIRCLE ( 'NONE', #3204, 4.000000000000003553 ) ;
#39409 = CARTESIAN_POINT ( 'NONE',  ( 91.11537606070176309, -60.00000000000000711, 202.2000497971606592 ) ) ;
#39410 = VECTOR ( 'NONE', #97271, 1000.000000000000000 ) ;
#39411 = CARTESIAN_POINT ( 'NONE',  ( -16.10958011051322814, 35.08395293542164950, 21.97156943567877718 ) ) ;
#39412 = ORIENTED_EDGE ( 'NONE', *, *, #83053, .T. ) ;
#39413 = CARTESIAN_POINT ( 'NONE',  ( 57.46915197135655262, -53.38142663087884188, 72.11230974744191258 ) ) ;
#39414 = CARTESIAN_POINT ( 'NONE',  ( -34.29742002188510241, 300.7002447392828799, -8.688633338721277966 ) ) ;
#39415 = EDGE_CURVE ( 'NONE', #26344, #49975, #4936, .T. ) ;
#39416 = CARTESIAN_POINT ( 'NONE',  ( 9.981919929974880645, -50.02752553709775896, 27.65434374221348435 ) ) ;
#39417 = CARTESIAN_POINT ( 'NONE',  ( -6.928203230275512325, 29.73116675491001715, -4.000000000000001776 ) ) ;
#39418 = ORIENTED_EDGE ( 'NONE', *, *, #98205, .F. ) ;
#39420 = CARTESIAN_POINT ( 'NONE',  ( -10.00250692948970865, -49.99952737940893144, 26.86088010484640165 ) ) ;
#39419 = CARTESIAN_POINT ( 'NONE',  ( -110.7961550858539255, -38.35618406817627601, 179.4776150961166081 ) ) ;
#39421 = CARTESIAN_POINT ( 'NONE',  ( -42.10086803841218739, 435.6552064019005002, 19.95582312411058368 ) ) ;
#39422 = CARTESIAN_POINT ( 'NONE',  ( 29.91076667616410489, 328.9704351996689979, 14.85080938783550231 ) ) ;
#39423 = CARTESIAN_POINT ( 'NONE',  ( 0.000000000000000000, 1.502314598737160412E-15, 6.500000000000000888 ) ) ;
#39424 = CARTESIAN_POINT ( 'NONE',  ( 8.000000000000000000, -30.40625000000000000, -3.313708498984761608 ) ) ;
#39425 = AXIS2_PLACEMENT_3D ( 'NONE', #41991, #25313, #82988 ) ;
#39426 = CARTESIAN_POINT ( 'NONE',  ( 2.617478844989858722, -3.000000000000002665, -75.26027323389553203 ) ) ;
#39427 = VECTOR ( 'NONE', #58654, 1000.000000000000000 ) ;
#39428 = EDGE_CURVE ( 'NONE', #70645, #28989, #54794, .T. ) ;
#39429 = B_SPLINE_CURVE_WITH_KNOTS ( 'NONE', 3,
 ( #20496, #55433, #22045, #104524, #71622, #37181, #46825, #30678, #54356, #61981 ),
 .UNSPECIFIED., .F., .F.,
 ( 4, 2, 2, 2, 4 ),
 ( -4.786264512459483439E-05, 0.0004191110641584722693, 0.0008860847734415393121, 0.001820032192007644016, 0.003687927029139882913 ),
 .UNSPECIFIED. ) ;
#39430 = CARTESIAN_POINT ( 'NONE',  ( 7.914984360234579519, -3.818534719232097085, -7.907701344400645205 ) ) ;
#39431 = ORIENTED_EDGE ( 'NONE', *, *, #66582, .F. ) ;
#39432 = CARTESIAN_POINT ( 'NONE',  ( 81.43749204890434612, -57.00584086149340379, 181.8846221577169047 ) ) ;
#39433 = DIRECTION ( 'NONE',  ( -1.000000000000000000, 0.000000000000000000, 0.000000000000000000 ) ) ;
#39434 = B_SPLINE_CURVE_WITH_KNOTS ( 'NONE', 3,
 ( #44947, #52471, #34747, #67619, #3410, #100496, #76750, #61119, #68692, #2857, #84325, #85392, #43335, #77830, #20169, #59532, #76217, #10936, #53549, #44400 ),
 .UNSPECIFIED., .F., .F.,
 ( 4, 2, 2, 2, 2, 2, 2, 2, 2, 4 ),
 ( 0.007283033696500349971, 0.007786984348840834957, 0.008290935001181318209, 0.008794885653521803195, 0.009298836305862288182, 0.009802786958202773168, 0.01030673761054325815, 0.01081068826288374141, 0.01106266358905398303, 0.01131463891522422639 ),
 .UNSPECIFIED. ) ;
#39435 = CARTESIAN_POINT ( 'NONE',  ( -36.48988454258796565, 439.4722615773889629, 23.89747316622354845 ) ) ;
#39436 = ORIENTED_EDGE ( 'NONE', *, *, #74483, .T. ) ;
#39437 = CARTESIAN_POINT ( 'NONE',  ( 69.67238219402268840, 6.975173280561618775E-15, 0.000000000000000000 ) ) ;
#39438 = CARTESIAN_POINT ( 'NONE',  ( 6.731961105520387179, -4.334285474477063360, -16.87634736349912501 ) ) ;
#39439 = FACE_OUTER_BOUND ( 'NONE', #69152, .T. ) ;
#39440 = CARTESIAN_POINT ( 'NONE',  ( -12.00013170160693576, 50.00000000000001421, -86.59063654372916119 ) ) ;
#39441 =( NAMED_UNIT ( * ) SI_UNIT ( $, .STERADIAN. ) SOLID_ANGLE_UNIT ( ) );
#39442 = DIRECTION ( 'NONE',  ( 0.000000000000000000, 0.000000000000000000, 1.000000000000000000 ) ) ;
#39443 = EDGE_CURVE ( 'NONE', #8540, #87039, #34209, .T. ) ;
#39444 = ORIENTED_EDGE ( 'NONE', *, *, #66023, .F. ) ;
#39445 = CIRCLE ( 'NONE', #84238, 10.00000000000000000 ) ;
#39446 = CARTESIAN_POINT ( 'NONE',  ( 6.499999999999998224, 3.350125858420228919, -6.343571411522940018 ) ) ;
#39447 = CARTESIAN_POINT ( 'NONE',  ( 1.092184909756600097, 25.84081523104171652, 38.88672836633164565 ) ) ;
#39450 = CIRCLE ( 'NONE', #37771, 4.000000000000002665 ) ;
#39449 = CARTESIAN_POINT ( 'NONE',  ( -11.50180495297654204, 15.06797554620490232, -9.787940426045702580 ) ) ;
#39448 = CARTESIAN_POINT ( 'NONE',  ( 7.500000000000007105, 39.99999999999998579, -68.91429205785453860 ) ) ;
#39451 = CARTESIAN_POINT ( 'NONE',  ( 5.082755093536324154, -20.84375000204838813, 5.082755093536326818 ) ) ;
#39452 = CARTESIAN_POINT ( 'NONE',  ( -29.68315524077005207, 13.47185074185902209, -42.10535821593474282 ) ) ;
#39453 = CARTESIAN_POINT ( 'NONE',  ( -27.99999999999999645, 0.000000000000000000, -13.00000000000000000 ) ) ;
#39454 =( GEOMETRIC_REPRESENTATION_CONTEXT ( 3 ) GLOBAL_UNCERTAINTY_ASSIGNED_CONTEXT ( ( #46150 ) ) GLOBAL_UNIT_ASSIGNED_CONTEXT ( ( #17074, #16526, #66680 ) ) REPRESENTATION_CONTEXT ( 'NONE', 'WORKASPACE' ) );
#39455 = ORIENTED_EDGE ( 'NONE', *, *, #78040, .T. ) ;
#39456 =( LENGTH_UNIT ( ) NAMED_UNIT ( * ) SI_UNIT ( .MILLI., .METRE. ) );
#39457 = CARTESIAN_POINT ( 'NONE',  ( 23.62759301673245815, 25.18629740126316818, 33.13999265739832367 ) ) ;
#39458 = CARTESIAN_POINT ( 'NONE',  ( -9.061861678845534840, 137.7616487646043311, 0.000000000000000000 ) ) ;
#39459 = CARTESIAN_POINT ( 'NONE',  ( -34.92499999999994742, 0.000000000000000000, 0.000000000000000000 ) ) ;
#39460 = CARTESIAN_POINT ( 'NONE',  ( -14.59561887822985327, 1.699647480229564245, 3.448601310208504689 ) ) ;
#39461 = VERTEX_POINT ( 'NONE', #15660 ) ;
#39462 = AXIS2_PLACEMENT_3D ( 'NONE', #42368, #59100, #83888 ) ;
#39463 = CARTESIAN_POINT ( 'NONE',  ( 44.18670859114681804, 435.3672560506858531, 10.83164355295159709 ) ) ;
#39464 = DIRECTION ( 'NONE',  ( 1.000000000000000000, 0.000000000000000000, 0.000000000000000000 ) ) ;
#39465 = ORIENTED_EDGE ( 'NONE', *, *, #33933, .F. ) ;
#39466 = CARTESIAN_POINT ( 'NONE',  ( -3.037443755948696200, -0.5477000578292443578, 103.2087721268169389 ) ) ;
#39467 = CARTESIAN_POINT ( 'NONE',  ( -49.99542551630922560, 38.95362649332037108, -39.50291754361181518 ) ) ;
#39468 = DIRECTION ( 'NONE',  ( 0.000000000000000000, 0.000000000000000000, 1.000000000000000000 ) ) ;
#39469 = UNCERTAINTY_MEASURE_WITH_UNIT (LENGTH_MEASURE( 1.000000000000000082E-05 ), #96381, 'distance_accuracy_value', 'NONE');
#39470 = CARTESIAN_POINT ( 'NONE',  ( -111.3399326272597989, -60.00000000000000711, 155.6059937888795730 ) ) ;
#39471 = AXIS2_PLACEMENT_3D ( 'NONE', #26684, #18581, #34238 ) ;
#39472 = CARTESIAN_POINT ( 'NONE',  ( 102.6464385083043283, -2.002967142162725287E-29, 5.000000000000011546 ) ) ;
#39473 = CARTESIAN_POINT ( 'NONE',  ( 38.73386039798916869, 460.3889633641978776, 2.371405894923816149 ) ) ;
#39474 = CARTESIAN_POINT ( 'NONE',  ( -5.036189802309444907, -5.000000000000002665, -76.26213611588271135 ) ) ;
#39475 = CONICAL_SURFACE ( 'NONE', #46396, 3.309500000000001663, 0.9599310885968770357 ) ;
#39476 = CARTESIAN_POINT ( 'NONE',  ( -81.82008106255986490, -57.07570580673551319, 184.1260291814842844 ) ) ;
#39477 = ORIENTED_EDGE ( 'NONE', *, *, #59656, .F. ) ;
#39478 = SURFACE_SIDE_STYLE ('',( #73937 ) ) ;
#39479 =( BOUNDED_CURVE ( )  B_SPLINE_CURVE ( 2, ( #25268, #26353, #59748, #75372, #1471, #912, #57580 ),
 .UNSPECIFIED., .F., .F. ) 
 B_SPLINE_CURVE_WITH_KNOTS ( ( 3, 2, 2, 3 ),
 ( 0.1445660357747511060, 0.1470588235294117696, 0.1544117647058823317, 0.1617647058823529216 ),
 .UNSPECIFIED. ) 
 CURVE ( )  GEOMETRIC_REPRESENTATION_ITEM ( )  RATIONAL_B_SPLINE_CURVE ( ( 0.9658850655769295468, 0.9741937049840523333, 1.000000000000000000, 0.9238795325112867385, 1.000000000000000000, 0.9238795325112870716, 0.9999999999999996669 ) ) 
 REPRESENTATION_ITEM ( '' )  );
#39480 = VERTEX_POINT ( 'NONE', #56645 ) ;
#39481 = DIRECTION ( 'NONE',  ( 0.000000000000000000, -0.9584033143583832182, 0.2854173908977277185 ) ) ;
#39482 = ADVANCED_FACE ( 'NONE', ( #97112, #73353 ), #58246, .T. ) ;
#39483 = CARTESIAN_POINT ( 'NONE',  ( 0.000000000000000000, 0.000000000000000000, -10.00000000000000000 ) ) ;
#39484 = CARTESIAN_POINT ( 'NONE',  ( -85.58732770572241577, -52.70779370753110982, 27.65126831969156029 ) ) ;
#39485 = FACE_OUTER_BOUND ( 'NONE', #48377, .T. ) ;
#39486 = PRESENTATION_STYLE_ASSIGNMENT (( #71300 ) ) ;
#39487 = CARTESIAN_POINT ( 'NONE',  ( 8.830661707197100085, 18.20374273969819257, -9.201869806248672558E-30 ) ) ;
#39488 = CARTESIAN_POINT ( 'NONE',  ( 11.76480859346303554, -5.000000000000000000, -79.34597263090529395 ) ) ;
#39489 = DIRECTION ( 'NONE',  ( 0.000000000000000000, -1.000000000000000000, 0.000000000000000000 ) ) ;
#39490 = CARTESIAN_POINT ( 'NONE',  ( 80.26999927900735088, -59.99999999999982947, 200.1019127161866606 ) ) ;
#39491 = EDGE_CURVE ( 'NONE', #21200, #81655, #73611, .T. ) ;
#39492 = CARTESIAN_POINT ( 'NONE',  ( -102.4477130004285499, -30.00000000000004974, 111.1018478433771151 ) ) ;
#39493 = CARTESIAN_POINT ( 'NONE',  ( -61.58610401018594160, -56.86967154772055721, 85.14694393301525110 ) ) ;
#39494 = ORIENTED_EDGE ( 'NONE', *, *, #24625, .F. ) ;
#39495 = CARTESIAN_POINT ( 'NONE',  ( 14.81477527478923228, 39.42585065352723461, 63.35881087812447277 ) ) ;
#39496 = CARTESIAN_POINT ( 'NONE',  ( 97.19628318239716691, -59.99999999999878497, 204.8875827899316846 ) ) ;
#39497 = CIRCLE ( 'NONE', #92905, 4.000000000000001776 ) ;
#39498 = VERTEX_POINT ( 'NONE', #33466 ) ;
#39499 = CARTESIAN_POINT ( 'NONE',  ( 2.014047737277413042, -39.47254121402686877, 30.46601114062715610 ) ) ;
#39500 = CARTESIAN_POINT ( 'NONE',  ( -5.082755093536326818, -20.09375000204838457, 5.082755093536325042 ) ) ;
#39501 = CARTESIAN_POINT ( 'NONE',  ( -4.696906829037968301, -8.560018525121078525, -3.734050370377311800 ) ) ;
#39502 = ORIENTED_EDGE ( 'NONE', *, *, #5543, .F. ) ;
#39503 = CARTESIAN_POINT ( 'NONE',  ( -3.313708498984783812, -26.65625000409676915, 7.999999999999979572 ) ) ;
#39504 = ORIENTED_EDGE ( 'NONE', *, *, #98458, .F. ) ;
#39505 = CARTESIAN_POINT ( 'NONE',  ( 0.000000000000000000, 29.08768991669519721, 35.82893434829263413 ) ) ;
#39506 = CARTESIAN_POINT ( 'NONE',  ( -7.908030677224553884, 3.059924800338339246, -7.792662696733363425 ) ) ;
#39507 = CARTESIAN_POINT ( 'NONE',  ( -89.17390004647626256, -59.99999999999994316, 201.7553460497344417 ) ) ;
#39508 = CARTESIAN_POINT ( 'NONE',  ( 4.463429423125061746, -13.01149508916979336, -0.1387913946425961276 ) ) ;
#39509 = CARTESIAN_POINT ( 'NONE',  ( 2.977408999572650927, -23.75000000204839168, -7.188101187500001821 ) ) ;
#39510 = ADVANCED_FACE ( 'NONE', ( #25390 ), #88660, .T. ) ;
#39511 = CARTESIAN_POINT ( 'NONE',  ( 46.00000000000000000, 461.5066419892501131, 9.508543545646363171 ) ) ;
#39512 = CARTESIAN_POINT ( 'NONE',  ( -5.372766443841437756, 53.45888839938537274, -8.531152949374524397 ) ) ;
#39513 = CARTESIAN_POINT ( 'NONE',  ( 4.999999999996198596, -56.64186896439935026, 6.232146447249109933 ) ) ;
#39514 = CARTESIAN_POINT ( 'NONE',  ( -9.739726766104087829, 48.00000000000000000, -87.61747884499078509 ) ) ;
#39515 = CARTESIAN_POINT ( 'NONE',  ( 7.317451043433990776, -6.276491506186944846, 13.99669291930579007 ) ) ;
#39516 = FACE_OUTER_BOUND ( 'NONE', #13232, .T. ) ;
#39517 = CARTESIAN_POINT ( 'NONE',  ( 36.89131349651913894, 342.5581385403770582, -0.5070065298284284205 ) ) ;
#39518 = CARTESIAN_POINT ( 'NONE',  ( -31.88243720866665143, -32.55223407456951179, 32.57539379951157343 ) ) ;
#39519 = AXIS2_PLACEMENT_3D ( 'NONE', #1501, #52188, #67336 ) ;
#39520 = EDGE_LOOP ( 'NONE', ( #765, #76543 ) ) ;
#39521 = CARTESIAN_POINT ( 'NONE',  ( -14.81732167757165008, 41.99559907176403328, -87.50313943119428473 ) ) ;
#39522 = CARTESIAN_POINT ( 'NONE',  ( 42.47999858120645200, -49.88713018564629920, 43.43313861898666772 ) ) ;
#39523 = CARTESIAN_POINT ( 'NONE',  ( 14.86825985028009001, 0.000000000000000000, 8.569529079650957115 ) ) ;
#39524 = EDGE_LOOP ( 'NONE', ( #56669, #55377 ) ) ;
#39525 = PLANE ( 'NONE',  #106402 ) ;
#39526 = MECHANICAL_DESIGN_GEOMETRIC_PRESENTATION_REPRESENTATION (  '', ( #25784 ), #3396 ) ;
#39527 = CARTESIAN_POINT ( 'NONE',  ( -73.92819207610308752, -38.32663662495320978, 159.7473140453433302 ) ) ;
#39528 = ORIENTED_EDGE ( 'NONE', *, *, #27784, .T. ) ;
#39530 = CARTESIAN_POINT ( 'NONE',  ( -31.00389226249483698, 502.9289871839745842, 8.047326149841639520 ) ) ;
#39529 = CARTESIAN_POINT ( 'NONE',  ( 6.542296142763995626, -4.999999999999999112, -15.34579906099600599 ) ) ;
#39531 = CARTESIAN_POINT ( 'NONE',  ( -32.99999999999999289, 439.7597899781498541, 24.16317522621304903 ) ) ;
#39532 = DIRECTION ( 'NONE',  ( 0.000000000000000000, 0.000000000000000000, -1.000000000000000000 ) ) ;
#39533 = DIRECTION ( 'NONE',  ( -1.000000000000000000, -0.000000000000000000, -0.000000000000000000 ) ) ;
#39534 = DIRECTION ( 'NONE',  ( 0.000000000000000000, 1.000000000000000000, 0.000000000000000000 ) ) ;
#39535 = CARTESIAN_POINT ( 'NONE',  ( -48.48434714564471193, 13.98045800628875313, -16.77138779655891909 ) ) ;
#39536 = FACE_OUTER_BOUND ( 'NONE', #82964, .T. ) ;
#39537 = CONICAL_SURFACE ( 'NONE', #22380, 5.000000000000000000, 0.9599310885968913576 ) ;
#39538 = CARTESIAN_POINT ( 'NONE',  ( 98.00938096300853886, -59.99999999999998579, 68.98427090110736515 ) ) ;
#39539 = DIRECTION ( 'NONE',  ( -1.000000000000000000, -1.224606353822377258E-16, -0.000000000000000000 ) ) ;
#39540 = DIRECTION ( 'NONE',  ( 1.000000000000000000, 0.000000000000000000, 0.000000000000000000 ) ) ;
#39541 = DIRECTION ( 'NONE',  ( 1.000000000000000000, 1.224606353822377258E-16, 0.000000000000000000 ) ) ;
#39542 = ORIENTED_EDGE ( 'NONE', *, *, #39683, .T. ) ;
#39543 = EDGE_CURVE ( 'NONE', #17581, #84503, #87765, .T. ) ;
#39544 = CARTESIAN_POINT ( 'NONE',  ( -53.08935917470196131, -30.00000000000000711, 52.21147893555082220 ) ) ;
#39545 = EDGE_LOOP ( 'NONE', ( #80903, #50774, #33191, #12901, #82574, #16443 ) ) ;
#39546 = CIRCLE ( 'NONE', #1615, 4.172000000000009479 ) ;
#39547 = CARTESIAN_POINT ( 'NONE',  ( -9.934750400155193617, -57.86805517166717294, 28.16945530398552222 ) ) ;
#39548 = CARTESIAN_POINT ( 'NONE',  ( -15.46466052604883323, 2.715844537113373924, 1.564829471106392145 ) ) ;
#39549 = CARTESIAN_POINT ( 'NONE',  ( 9.239881047873428344, 12.03209342863740972, 3.069484470019327247E-13 ) ) ;
#39550 = CYLINDRICAL_SURFACE ( 'NONE', #31152, 8.000000000000000000 ) ;
#39551 = DIRECTION ( 'NONE',  ( -1.000000000000000000, -0.000000000000000000, -0.000000000000000000 ) ) ;
#39552 = CARTESIAN_POINT ( 'NONE',  ( -7.188101187500000044, -26.28125000204838813, -8.802885111219163269E-16 ) ) ;
#39553 = CARTESIAN_POINT ( 'NONE',  ( 5.700000000000000178, 4.898587196589412829E-16, -4.000000000000000000 ) ) ;
#39554 =( NAMED_UNIT ( * ) PLANE_ANGLE_UNIT ( ) SI_UNIT ( $, .RADIAN. ) );
#39556 = ADVANCED_FACE ( 'NONE', ( #41533 ), #92759, .T. ) ;
#39555 = CARTESIAN_POINT ( 'NONE',  ( 6.809786364711801099, 41.36669071793862429, -70.61902766783229879 ) ) ;
#39557 = EDGE_CURVE ( 'NONE', #4842, #12476, #66340, .T. ) ;
#39558 = ORIENTED_EDGE ( 'NONE', *, *, #8740, .F. ) ;
#39560 = ORIENTED_EDGE ( 'NONE', *, *, #12261, .F. ) ;
#39559 = CARTESIAN_POINT ( 'NONE',  ( 19.00000000000001066, -4.000000000000000000, -2.500000000000000000 ) ) ;
#39561 = CARTESIAN_POINT ( 'NONE',  ( 82.92136997883486060, -18.68766406158728088, 141.1224335365927232 ) ) ;
#39562 = AXIS2_PLACEMENT_3D ( 'NONE', #59239, #84032, #76458 ) ;
#39563 = CARTESIAN_POINT ( 'NONE',  ( -37.72547481417448978, 27.55009981184272760, -13.45617127781033417 ) ) ;
#39564 = ORIENTED_EDGE ( 'NONE', *, *, #92680, .T. ) ;
#39565 = CARTESIAN_POINT ( 'NONE',  ( -12.50000000000000711, 34.76080778227605350, -54.01526194481859733 ) ) ;
#39566 = CARTESIAN_POINT ( 'NONE',  ( -0.6254118074930600235, 13.29657844059611449, -51.58631799359783798 ) ) ;
#39567 = CARTESIAN_POINT ( 'NONE',  ( 7.188101187500000933, -10.06250000204838457, -2.977408999572650483 ) ) ;
#39568 = CARTESIAN_POINT ( 'NONE',  ( 0.3167204509598346984, -8.479269695850854660, 1.313474075707213196 ) ) ;
#39569 = EDGE_CURVE ( 'NONE', #48676, #40649, #498, .T. ) ;
#39570 = CARTESIAN_POINT ( 'NONE',  ( 11.54075930460769506, 45.44590361214169150, 14.27956357151531286 ) ) ;
#39571 = CARTESIAN_POINT ( 'NONE',  ( 43.43869229197127169, 464.9661605157749591, 13.42065392471465834 ) ) ;
#39572 = EDGE_CURVE ( 'NONE', #2944, #32770, #42794, .T. ) ;
#39573 = ORIENTED_EDGE ( 'NONE', *, *, #65954, .F. ) ;
#39574 = SHAPE_REPRESENTATION_RELATIONSHIP ( 'NONE' , 'NONE' ,  #25516, #92356 ) ;
#39575 = CARTESIAN_POINT ( 'NONE',  ( 0.000000000000000000, 5.629165124598842773, -3.250000000000011990 ) ) ;
#39576 = CARTESIAN_POINT ( 'NONE',  ( 25.95755237148832961, 18.64284798592537129, -28.33950252048799001 ) ) ;
#39577 = LINE ( 'NONE', #95674, #92958 ) ;
#39578 = ORIENTED_EDGE ( 'NONE', *, *, #48024, .T. ) ;
#39579 = CARTESIAN_POINT ( 'NONE',  ( -8.000000000000000000, -11.93750000409677092, -9.797174393178825657E-16 ) ) ;
#39580 = CARTESIAN_POINT ( 'NONE',  ( -11.78651013471115050, -14.22498507149665414, 31.80223059555903475 ) ) ;
#39581 = DIRECTION ( 'NONE',  ( 0.000000000000000000, 1.000000000000000000, 0.000000000000000000 ) ) ;
#39582 = VECTOR ( 'NONE', #26966, 1000.000000000000000 ) ;
#39583 = CARTESIAN_POINT ( 'NONE',  ( 0.7783529810093747781, 51.35606173618085535, -9.981590251641023315 ) ) ;
#39584 = ADVANCED_FACE ( 'NONE', ( #57697 ), #83062, .T. ) ;
#39585 = DIRECTION ( 'NONE',  ( -1.000000000000000000, 0.000000000000000000, 0.000000000000000000 ) ) ;
#39586 = CARTESIAN_POINT ( 'NONE',  ( 4.278555824747665604, 52.15500882501390123, 6.542026809210045535 ) ) ;
#39587 = APPLICATION_PROTOCOL_DEFINITION ( 'draft international standard', 'automotive_design', 1998, #45249 ) ;
#39588 = DIRECTION ( 'NONE',  ( -0.000000000000000000, -0.000000000000000000, -1.000000000000000000 ) ) ;
#39589 = VERTEX_POINT ( 'NONE', #80927 ) ;
#39590 = CARTESIAN_POINT ( 'NONE',  ( 11.38597746671299582, 43.57657614512142175, 13.48406053558915119 ) ) ;
#39591 =( LENGTH_UNIT ( ) NAMED_UNIT ( * ) SI_UNIT ( .MILLI., .METRE. ) );
#39592 = LINE ( 'NONE', #30445, #89328 ) ;
#39593 = CARTESIAN_POINT ( 'NONE',  ( -1.313803945217351110, -21.30231999290575118, -38.55323443611015932 ) ) ;
#39594 = FACE_OUTER_BOUND ( 'NONE', #34796, .T. ) ;
#39595 = CYLINDRICAL_SURFACE ( 'NONE', #10124, 5.000000000000000888 ) ;
#39596 = AXIS2_PLACEMENT_3D ( 'NONE', #89502, #8567, #23727 ) ;
#39597 = EDGE_LOOP ( 'NONE', ( #29132, #68688, #56219, #71480 ) ) ;
#39598 = AXIS2_PLACEMENT_3D ( 'NONE', #31109, #38144, #80667 ) ;
#39599 = CARTESIAN_POINT ( 'NONE',  ( -43.71217423904474231, 435.6632154632216043, 9.092528312227496912 ) ) ;
#39600 = CARTESIAN_POINT ( 'NONE',  ( 87.75520861027411001, -57.59389832414498755, 203.3620971134121760 ) ) ;
#39601 = AXIS2_PLACEMENT_3D ( 'NONE', #32826, #26356, #17692 ) ;
#39602 = CARTESIAN_POINT ( 'NONE',  ( 37.72498816021352752, 463.3860965757704093, 19.97126500438806218 ) ) ;
#39603 = CARTESIAN_POINT ( 'NONE',  ( -15.77996175643155929, 22.60291536984139071, 1.987376761536549408 ) ) ;
#39604 = CARTESIAN_POINT ( 'NONE',  ( 0.000000000000000000, 0.000000000000000000, 0.000000000000000000 ) ) ;
#39605 = CARTESIAN_POINT ( 'NONE',  ( -74.34427579237575401, -59.99999999999999289, 175.6371688333348970 ) ) ;
#39606 = CARTESIAN_POINT ( 'NONE',  ( -40.93292669599463096, 378.0706848361106722, 26.55786848468904537 ) ) ;
#39607 = CARTESIAN_POINT ( 'NONE',  ( 64.32759900501075379, 49.99999999999999289, -11.06576400629166912 ) ) ;
#39608 = CARTESIAN_POINT ( 'NONE',  ( -83.77086022884309102, -57.39681495382750853, 190.2519600005473421 ) ) ;
#39609 = ORIENTED_EDGE ( 'NONE', *, *, #17136, .T. ) ;
#39610 = CARTESIAN_POINT ( 'NONE',  ( 23.00643915961089903, 305.3757170294761067, -8.887520214983368305 ) ) ;
#39611 = VERTEX_POINT ( 'NONE', #105731 ) ;
#39612 = CARTESIAN_POINT ( 'NONE',  ( 9.833493305133805151, 4.000000000000002665, 0.000000000000000000 ) ) ;
#39613 = ADVANCED_FACE ( 'NONE', ( #16732 ), #51488, .T. ) ;
#39614 = CARTESIAN_POINT ( 'NONE',  ( 0.000000000000000000, 0.000000000000000000, 0.000000000000000000 ) ) ;
#39615 = CARTESIAN_POINT ( 'NONE',  ( -82.12931037298532999, -37.78909381349949115, -13.51468982751548964 ) ) ;
#39616 = AXIS2_PLACEMENT_3D ( 'NONE', #83720, #9828, #75636 ) ;
#39617 = CARTESIAN_POINT ( 'NONE',  ( -42.64966854229462001, 465.0854819100622422, 13.23715615004960178 ) ) ;
#39618 = EDGE_CURVE ( 'NONE', #43619, #42218, #32413, .T. ) ;
#39619 = CARTESIAN_POINT ( 'NONE',  ( 6.289692432696780244, 0.6618655008720331079, -6.828989928337167115 ) ) ;
#39620 = ORIENTED_EDGE ( 'NONE', *, *, #5781, .T. ) ;
#39621 = FILL_AREA_STYLE_COLOUR ( '', #28685 ) ;
#39622 = FACE_OUTER_BOUND ( 'NONE', #78389, .T. ) ;
#39623 = EDGE_CURVE ( 'NONE', #24268, #86867, #99224, .T. ) ;
#39624 = CARTESIAN_POINT ( 'NONE',  ( -23.05251019904581611, 27.41544800856653552, 33.20617127781058286 ) ) ;
#39625 = CARTESIAN_POINT ( 'NONE',  ( 0.000000000000000000, 0.000000000000000000, 0.000000000000000000 ) ) ;
#39626 = EDGE_CURVE ( 'NONE', #52941, #68169, #22192, .T. ) ;
#39627 = AXIS2_PLACEMENT_3D ( 'NONE', #51822, #11350, #100903 ) ;
#39628 = CARTESIAN_POINT ( 'NONE',  ( 85.44123078815633221, -14.21045842199435505, -16.45204874176463150 ) ) ;
#39629 = CARTESIAN_POINT ( 'NONE',  ( -77.86666928232057217, -18.66659128473655471, 117.1585483000689010 ) ) ;
#39630 = EDGE_LOOP ( 'NONE', ( #93928, #26655 ) ) ;
#39631 = CARTESIAN_POINT ( 'NONE',  ( 39.49823726628140719, -30.00000000000007461, 47.07845324830893929 ) ) ;
#39632 = DIRECTION ( 'NONE',  ( -1.000000000000000000, -1.224606353822377258E-16, -0.000000000000000000 ) ) ;
#39633 = CARTESIAN_POINT ( 'NONE',  ( 74.89313546090642149, -57.57953941245633445, 190.3487796247399615 ) ) ;
#39634 = DIRECTION ( 'NONE',  ( 4.738110706560371839E-17, -0.9221233147934838614, 0.3868961001538753219 ) ) ;
#39635 = CARTESIAN_POINT ( 'NONE',  ( 37.77771400876960683, 305.2406471639163215, -7.604042599900936672 ) ) ;
#39636 = CIRCLE ( 'NONE', #26725, 1.000000000000019540 ) ;
#39637 = CARTESIAN_POINT ( 'NONE',  ( -13.68990076057127148, 7.343638245770522488, 8.266402366871409058 ) ) ;
#39638 = ORIENTED_EDGE ( 'NONE', *, *, #47652, .F. ) ;
#39639 = CARTESIAN_POINT ( 'NONE',  ( -71.17284327374473207, -38.00000000000000711, -21.88481141223168436 ) ) ;
#39640 =( NAMED_UNIT ( * ) SI_UNIT ( $, .STERADIAN. ) SOLID_ANGLE_UNIT ( ) );
#39642 = CARTESIAN_POINT ( 'NONE',  ( -102.1546786399030680, -45.26555502571823553, 146.8815317979925226 ) ) ;
#39641 = DIRECTION ( 'NONE',  ( 0.000000000000000000, 0.000000000000000000, 1.000000000000000000 ) ) ;
#39643 = CARTESIAN_POINT ( 'NONE',  ( 2.977408999572651815, -19.43750000204838457, 7.188101187500000933 ) ) ;
#39644 = EDGE_CURVE ( 'NONE', #13347, #40083, #63526, .T. ) ;
#39645 = ADVANCED_FACE ( 'NONE', ( #51203 ), #75491, .F. ) ;
#39646 = DIRECTION ( 'NONE',  ( 0.000000000000000000, -1.000000000000000000, 0.000000000000000000 ) ) ;
#39647 = SURFACE_SIDE_STYLE ('',( #81644 ) ) ;
#39648 = CARTESIAN_POINT ( 'NONE',  ( 1.127244920694520092, 34.38903298460757441, 29.13254641235529263 ) ) ;
#39649 = CARTESIAN_POINT ( 'NONE',  ( -7.500000000000000000, -1.572902445675619099, -7.069816568113129307 ) ) ;
#39650 = VERTEX_POINT ( 'NONE', #26461 ) ;
#39651 = CARTESIAN_POINT ( 'NONE',  ( 0.000000000000000000, 79.50000000000000000, 0.000000000000000000 ) ) ;
#39653 = CARTESIAN_POINT ( 'NONE',  ( 32.69658716609513505, -60.31220508583461992, 38.00824357461662828 ) ) ;
#39652 = CARTESIAN_POINT ( 'NONE',  ( -4.155049527179308200, -30.00000000000002842, 36.99135516471767460 ) ) ;
#39654 = CIRCLE ( 'NONE', #8592, 3.000000000000017764 ) ;
#39655 = CARTESIAN_POINT ( 'NONE',  ( -23.86015722654359195, 25.16617832201437110, 33.04145880079988729 ) ) ;
#39656 = ORIENTED_EDGE ( 'NONE', *, *, #15458, .F. ) ;
#39657 = ORIENTED_EDGE ( 'NONE', *, *, #27246, .F. ) ;
#39658 = CARTESIAN_POINT ( 'NONE',  ( -1.249340999377952510, 43.67393701204134260, -17.33575850031895271 ) ) ;
#39659 = DIRECTION ( 'NONE',  ( 0.000000000000000000, 0.000000000000000000, 1.000000000000000000 ) ) ;
#39660 = LINE ( 'NONE', #47717, #1830 ) ;
#39661 = PRESENTATION_STYLE_ASSIGNMENT (( #79568 ) ) ;
#39662 = EDGE_LOOP ( 'NONE', ( #36112, #3583, #72482, #106251 ) ) ;
#39663 = DIRECTION ( 'NONE',  ( -0.000000000000000000, 0.5482566341169983204, 0.8363101477004208917 ) ) ;
#39664 = CARTESIAN_POINT ( 'NONE',  ( 22.22683576871073186, 25.59856940243015799, -32.73475386601680270 ) ) ;
#39665 = CARTESIAN_POINT ( 'NONE',  ( -0.000000000000000000, 4.501353321498349658, -60.59507871780017751 ) ) ;
#39666 = FACE_OUTER_BOUND ( 'NONE', #33843, .T. ) ;
#39667 = CARTESIAN_POINT ( 'NONE',  ( 47.57472544752255317, 12.59044387134409071, -14.43844179794168880 ) ) ;
#39668 = VERTEX_POINT ( 'NONE', #4146 ) ;
#39669 = ADVANCED_BREP_SHAPE_REPRESENTATION ( '', ( #51906, #10728 ), #38490 ) ;
#39670 =( GEOMETRIC_REPRESENTATION_CONTEXT ( 3 ) GLOBAL_UNCERTAINTY_ASSIGNED_CONTEXT ( ( #98039 ) ) GLOBAL_UNIT_ASSIGNED_CONTEXT ( ( #4210, #37682, #30632 ) ) REPRESENTATION_CONTEXT ( 'NONE', 'WORKASPACE' ) );
#39671 = VERTEX_POINT ( 'NONE', #69942 ) ;
#39672 = ORIENTED_EDGE ( 'NONE', *, *, #8120, .T. ) ;
#39673 = CARTESIAN_POINT ( 'NONE',  ( -33.00000000000000000, 464.3970849722209664, 17.41240408234212111 ) ) ;
#39674 = CARTESIAN_POINT ( 'NONE',  ( -36.56688176566701287, 28.18335144162340811, 11.43747163042122494 ) ) ;
#39675 = CARTESIAN_POINT ( 'NONE',  ( 27.50975502829663100, 307.9109348731828959, 11.11733839782984745 ) ) ;
#39676 = CARTESIAN_POINT ( 'NONE',  ( -37.60552182430246404, 371.2989764267708210, 4.344118227128259235 ) ) ;
#39677 = CARTESIAN_POINT ( 'NONE',  ( -2.261820640632148827, -69.44553280094153536, 12.91242553541718152 ) ) ;
#39678 = DIRECTION ( 'NONE',  ( -0.000000000000000000, -1.000000000000000000, -0.000000000000000000 ) ) ;
#39679 = DIRECTION ( 'NONE',  ( -0.5735764363510497121, 0.8191520442889892450, 1.003171929053521665E-16 ) ) ;
#39681 = ORIENTED_EDGE ( 'NONE', *, *, #98301, .F. ) ;
#39680 = AXIS2_PLACEMENT_3D ( 'NONE', #92496, #18649, #51506 ) ;
#39683 = EDGE_CURVE ( 'NONE', #717, #27489, #84125, .T. ) ;
#39682 = DIRECTION ( 'NONE',  ( -1.000000000000000000, -0.000000000000000000, -0.000000000000000000 ) ) ;
#39684 = VERTEX_POINT ( 'NONE', #83575 ) ;
#39685 = DIRECTION ( 'NONE',  ( -1.000000000000000000, -0.000000000000000000, -0.000000000000000000 ) ) ;
#39686 = CARTESIAN_POINT ( 'NONE',  ( 3.587928128302542596, 304.8518027750386636, 9.936999415048941131 ) ) ;
#39687 = CARTESIAN_POINT ( 'NONE',  ( -39.78276460673632187, 485.2153259665885798, -4.379159006359595097 ) ) ;
#39688 = CARTESIAN_POINT ( 'NONE',  ( -79.51359773737226533, -59.99999999999994316, 169.4842920155362265 ) ) ;
#39689 = CARTESIAN_POINT ( 'NONE',  ( 66.38356152105049546, -53.38427602353998225, 97.96190166083606243 ) ) ;
#39690 = ORIENTED_EDGE ( 'NONE', *, *, #11672, .T. ) ;
#39691 = STYLED_ITEM ( 'NONE', ( #78058 ), #80013 ) ;
#39692 = CARTESIAN_POINT ( 'NONE',  ( 40.44044047303815859, 465.0924562876297159, 17.36401474854813287 ) ) ;
#39693 = CARTESIAN_POINT ( 'NONE',  ( 0.000000000000000000, -5.629165124598848990, -3.250000000000003553 ) ) ;
#39694 = AXIS2_PLACEMENT_3D ( 'NONE', #7787, #40169, #66569 ) ;
#39695 = CARTESIAN_POINT ( 'NONE',  ( 6.643884894376898664, -3.901062859469766497, -6.756839076127126198 ) ) ;
#39696 = ORIENTED_EDGE ( 'NONE', *, *, #41690, .F. ) ;
#39697 = VECTOR ( 'NONE', #99655, 1000.000000000000000 ) ;
#39698 = CARTESIAN_POINT ( 'NONE',  ( 46.92723468898980599, 18.82863087225951304, 15.00902207511731667 ) ) ;
#39699 = CARTESIAN_POINT ( 'NONE',  ( 6.536669471946908949, 51.40519842345576507, -7.404314278401480820 ) ) ;
#39700 = CONICAL_SURFACE ( 'NONE', #99956, 3.309500000000001663, 0.9599310885968770357 ) ;
#39701 = CARTESIAN_POINT ( 'NONE',  ( 5.656854249492378806, -29.37500000409677270, 5.656854249492381470 ) ) ;
#39702 = CARTESIAN_POINT ( 'NONE',  ( -2.094395098902536390, -4.999999999999998224, -8.000000000000000000 ) ) ;
#39703 = CARTESIAN_POINT ( 'NONE',  ( 86.82806741021897778, -24.34697663169452397, 185.7438550995267406 ) ) ;
#39704 = EDGE_CURVE ( 'NONE', #103615, #84434, #58799, .T. ) ;
#39705 = CIRCLE ( 'NONE', #10421, 66.00000000000000000 ) ;
#39706 = CARTESIAN_POINT ( 'NONE',  ( 9.842984802582137149, 33.59069590475652234, 1.781981959250508618 ) ) ;
#39707 = CARTESIAN_POINT ( 'NONE',  ( 7.344505440741524893, -7.553810727012976400, -3.175463080953007999 ) ) ;
#39708 = CARTESIAN_POINT ( 'NONE',  ( 3.318391428298041124, 303.8518027738843443, 9.936999414637822881 ) ) ;
#39709 = ORIENTED_EDGE ( 'NONE', *, *, #17076, .T. ) ;
#39710 = DIRECTION ( 'NONE',  ( -0.2244612941943540108, 0.4655631424236075233, 0.8560771506267712549 ) ) ;
#39711 = CARTESIAN_POINT ( 'NONE',  ( 0.000000000000000000, 0.000000000000000000, 0.000000000000000000 ) ) ;
#39712 = CARTESIAN_POINT ( 'NONE',  ( 28.81571653886122419, -59.99999999999999289, 42.47396466590021191 ) ) ;
#39713 = CARTESIAN_POINT ( 'NONE',  ( -98.73540789171605070, -29.99999999999999645, 189.4149580153970760 ) ) ;
#39714 = DIRECTION ( 'NONE',  ( -0.8191520442889974607, 0.000000000000000000, -0.5735764363510379438 ) ) ;
#39715 = CARTESIAN_POINT ( 'NONE',  ( 49.43476175332632039, -57.67888354579591947, 75.71380488283527654 ) ) ;
#39716 = VECTOR ( 'NONE', #65301, 1000.000000000000000 ) ;
#39718 = CARTESIAN_POINT ( 'NONE',  ( 43.87189908087982104, 464.7380721632374048, 11.09531536897046422 ) ) ;
#39717 = CARTESIAN_POINT ( 'NONE',  ( 6.232496355896457452, 41.83455062734740437, -59.02481358918409171 ) ) ;
#39719 =( GEOMETRIC_REPRESENTATION_CONTEXT ( 3 ) GLOBAL_UNCERTAINTY_ASSIGNED_CONTEXT ( ( #79012 ) ) GLOBAL_UNIT_ASSIGNED_CONTEXT ( ( #24814, #70307, #62239 ) ) REPRESENTATION_CONTEXT ( 'NONE', 'WORKASPACE' ) );
#39720 = CYLINDRICAL_SURFACE ( 'NONE', #72206, 1.250000000000001110 ) ;
#39721 = DIRECTION ( 'NONE',  ( -0.000000000000000000, 1.000000000000000000, -0.000000000000000000 ) ) ;
#39722 = PRODUCT_DEFINITION ( 'UNKNOWN', '', #6022, #68291 ) ;
#39723 = CARTESIAN_POINT ( 'NONE',  ( -7.930648640465597587, -60.00000000000000711, 39.63302098071156365 ) ) ;
#39724 = APPLICATION_CONTEXT ( 'automotive_design' ) ;
#39725 = CARTESIAN_POINT ( 'NONE',  ( -86.66245912624070513, -20.68510438609584767, 184.7494804068583392 ) ) ;
#39726 = ORIENTED_EDGE ( 'NONE', *, *, #106755, .F. ) ;
#39727 = CARTESIAN_POINT ( 'NONE',  ( 17.50000000000004619, 51.99978697404952044, 59.99316026186414064 ) ) ;
#39728 = CARTESIAN_POINT ( 'NONE',  ( 37.75487775365388643, 438.6157932507177293, 23.62942516414488026 ) ) ;
#39729 = CARTESIAN_POINT ( 'NONE',  ( -12.66716468281169483, -60.36572609861780592, 34.01381952931010488 ) ) ;
#39730 = DIRECTION ( 'NONE',  ( -0.8086898285216187476, 0.000000000000000000, -0.5882352941176471894 ) ) ;
#39732 = DIRECTION ( 'NONE',  ( 0.000000000000000000, -1.000000000000000000, 0.000000000000000000 ) ) ;
#39731 = FACE_OUTER_BOUND ( 'NONE', #29895, .T. ) ;
#39733 = ORIENTED_EDGE ( 'NONE', *, *, #13177, .F. ) ;
#39734 = DIRECTION ( 'NONE',  ( 0.000000000000000000, -1.000000000000000000, 0.000000000000000000 ) ) ;
#39735 = MECHANICAL_DESIGN_GEOMETRIC_PRESENTATION_REPRESENTATION (  '', ( #88007 ), #58677 ) ;
#39736 = CARTESIAN_POINT ( 'NONE',  ( -7.145220222863677861, -5.000000000000017764, -15.42794826860982305 ) ) ;
#39737 = CARTESIAN_POINT ( 'NONE',  ( 0.4042117618284704061, -3.141900367810047889, -6.500000000000002665 ) ) ;
#39738 = CARTESIAN_POINT ( 'NONE',  ( 7.493944697689368439, 40.57567825174881904, -59.86116849737391021 ) ) ;
#39739 = ADVANCED_FACE ( 'NONE', ( #54252 ), #83260, .T. ) ;
#39740 = CARTESIAN_POINT ( 'NONE',  ( 62.15290319597050939, -60.00000000000000711, 107.8068670736100785 ) ) ;
#39741 = CARTESIAN_POINT ( 'NONE',  ( -0.7873503183212902101, 53.48327185720855681, -9.984552898249470232 ) ) ;
#39742 = ORIENTED_EDGE ( 'NONE', *, *, #97591, .T. ) ;
#39743 = CARTESIAN_POINT ( 'NONE',  ( 0.000000000000000000, 300.0000000000000568, -10.00000000000000178 ) ) ;
#39744 = SURFACE_STYLE_FILL_AREA ( #73135 ) ;
#39746 = CARTESIAN_POINT ( 'NONE',  ( -35.62292360717025019, 485.2979424254038463, -2.983350328822282904 ) ) ;
#39745 = CARTESIAN_POINT ( 'NONE',  ( 41.69321614992608716, -29.99999999999995737, 49.76314934024226488 ) ) ;
#39747 =( NAMED_UNIT ( * ) SI_UNIT ( $, .STERADIAN. ) SOLID_ANGLE_UNIT ( ) );
#39748 = FILL_AREA_STYLE_COLOUR ( '', #15260 ) ;
#39749 = ORIENTED_EDGE ( 'NONE', *, *, #78052, .T. ) ;
#39750 = VECTOR ( 'NONE', #17523, 1000.000000000000227 ) ;
#39751 = CARTESIAN_POINT ( 'NONE',  ( -29.34822610931458087, 317.9602820924653201, 13.40329343600991407 ) ) ;
#39752 = EDGE_CURVE ( 'NONE', #59443, #34982, #84228, .T. ) ;
#39753 = ORIENTED_EDGE ( 'NONE', *, *, #50265, .F. ) ;
#39754 = DIRECTION ( 'NONE',  ( -0.000000000000000000, -1.000000000000000000, -0.000000000000000000 ) ) ;
#39755 = AXIS2_PLACEMENT_3D ( 'NONE', #58083, #75328, #49997 ) ;
#39756 = EDGE_CURVE ( 'NONE', #88153, #76051, #29519, .T. ) ;
#39757 = PRESENTATION_STYLE_ASSIGNMENT (( #25183 ) ) ;
#39758 = FILL_AREA_STYLE_COLOUR ( '', #37148 ) ;
#39759 = FACE_OUTER_BOUND ( 'NONE', #67572, .T. ) ;
#39760 = VERTEX_POINT ( 'NONE', #53748 ) ;
#39761 = FILL_AREA_STYLE ('',( #66142 ) ) ;
#39762 = B_SPLINE_CURVE_WITH_KNOTS ( 'NONE', 3,
 ( #75878, #57547, #82373, #90467, #8480, #41385, #52127, #18747, #53731, #29502, #61308, #3597, #78528, #86659 ),
 .UNSPECIFIED., .F., .F.,
 ( 4, 2, 2, 2, 2, 2, 4 ),
 ( 5.204170427930421283E-18, 0.002831373411936749778, 0.004247060117905107970, 0.005662746823873466596, 0.007078433529841825222, 0.008494120235810182981, 0.01132549364774689329 ),
 .UNSPECIFIED. ) ;
#39763 = CARTESIAN_POINT ( 'NONE',  ( 5.000000000000000000, -13.80294717177706154, 10.52286356751840479 ) ) ;
#39764 = CARTESIAN_POINT ( 'NONE',  ( -113.1713605750742602, -60.00000000000491696, 188.4473907172926204 ) ) ;
#39765 = AXIS2_PLACEMENT_3D ( 'NONE', #79365, #80413, #38407 ) ;
#39766 = CARTESIAN_POINT ( 'NONE',  ( 45.99999999999995026, 485.6428795626757164, -1.077934839663798439 ) ) ;
#39767 = CARTESIAN_POINT ( 'NONE',  ( 58.19072685764542996, -60.00000000000000000, 94.67969609638358008 ) ) ;
#39768 = CARTESIAN_POINT ( 'NONE',  ( 25.59999999999999787, 3.309500000000003439, 0.000000000000000000 ) ) ;
#39769 = CARTESIAN_POINT ( 'NONE',  ( 1.100317426399643139, 25.84114585796975305, -38.88560695975913006 ) ) ;
#39770 =( GEOMETRIC_REPRESENTATION_CONTEXT ( 3 ) GLOBAL_UNCERTAINTY_ASSIGNED_CONTEXT ( ( #1954 ) ) GLOBAL_UNIT_ASSIGNED_CONTEXT ( ( #85242, #52868, #86328 ) ) REPRESENTATION_CONTEXT ( 'NONE', 'WORKASPACE' ) );
#39772 = CARTESIAN_POINT ( 'NONE',  ( 10.23004908500708687, -35.99163919401772205, 29.89939049008435390 ) ) ;
#39771 = CARTESIAN_POINT ( 'NONE',  ( -110.6385074381434066, -60.00000000000007816, 195.8055798097608147 ) ) ;
#39773 = CARTESIAN_POINT ( 'NONE',  ( 83.10241079684797683, -38.00000000000000711, -1.999425119195920919 ) ) ;
#39774 =( NAMED_UNIT ( * ) SI_UNIT ( $, .STERADIAN. ) SOLID_ANGLE_UNIT ( ) );
#39775 = CARTESIAN_POINT ( 'NONE',  ( -46.18499865988201947, -22.24145118935602383, 40.24121074957823652 ) ) ;
#39776 = CIRCLE ( 'NONE', #87973, 5.000000000000002665 ) ;
#39777 = CARTESIAN_POINT ( 'NONE',  ( 42.19179521601841287, 485.4956273777429487, -3.824025998174274577 ) ) ;
#39778 = ORIENTED_EDGE ( 'NONE', *, *, #31759, .F. ) ;
#39779 = CARTESIAN_POINT ( 'NONE',  ( 16.11737681246577480, 21.56249621366840330, -2.179529459261059898 ) ) ;
#39780 = ADVANCED_FACE ( 'NONE', ( #21413 ), #15304, .T. ) ;
#39781 = DIRECTION ( 'NONE',  ( 0.000000000000000000, 0.000000000000000000, 1.000000000000000000 ) ) ;
#39782 = PLANE ( 'NONE',  #68207 ) ;
#39783 = CARTESIAN_POINT ( 'NONE',  ( 5.384233811324309116, -6.997829086552269651, 2.655407383564615920 ) ) ;
#39784 = CARTESIAN_POINT ( 'NONE',  ( 35.56416567029047116, 496.2909070316903239, -10.19064917708978335 ) ) ;
#39785 = ORIENTED_EDGE ( 'NONE', *, *, #49602, .T. ) ;
#39786 = DIRECTION ( 'NONE',  ( 0.000000000000000000, -1.000000000000000000, 0.000000000000000000 ) ) ;
#39787 = EDGE_LOOP ( 'NONE', ( #54785, #92263, #28825, #50830, #6156 ) ) ;
#39788 = CARTESIAN_POINT ( 'NONE',  ( 106.0132497538753142, -30.00000000000378719, 193.7988435085632091 ) ) ;
#39789 = CARTESIAN_POINT ( 'NONE',  ( 5.935763094077899815, 41.97455539652511192, -59.37421805147159404 ) ) ;
#39790 = CARTESIAN_POINT ( 'NONE',  ( 2.470381878726035567E-14, 18.87382441218300144, 49.24999999999992184 ) ) ;
#39791 = CARTESIAN_POINT ( 'NONE',  ( 94.31600719128907429, -30.00000000000000000, 113.8625557724812722 ) ) ;
#39792 = CARTESIAN_POINT ( 'NONE',  ( -22.35502908346653328, 304.3280978137025272, 10.03953411925336248 ) ) ;
#39793 = ORIENTED_EDGE ( 'NONE', *, *, #106607, .T. ) ;
#39794 = ORIENTED_EDGE ( 'NONE', *, *, #104553, .F. ) ;
#39795 = ORIENTED_EDGE ( 'NONE', *, *, #66882, .F. ) ;
#39796 = DIRECTION ( 'NONE',  ( -1.000000000000000000, -1.224606353822377258E-16, -0.000000000000000000 ) ) ;
#39797 = CARTESIAN_POINT ( 'NONE',  ( 23.05330517246050448, 26.02474360266739595, 30.70617127781016364 ) ) ;
#39798 = AXIS2_PLACEMENT_3D ( 'NONE', #105417, #70406, #46131 ) ;
#39799 = CARTESIAN_POINT ( 'NONE',  ( -38.21273700183271416, 463.7314486282535881, 19.26286508106272422 ) ) ;
#39800 = VERTEX_POINT ( 'NONE', #67940 ) ;
#39801 = ADVANCED_FACE ( 'NONE', ( #28450 ), #64678, .T. ) ;
#39802 = MECHANICAL_DESIGN_GEOMETRIC_PRESENTATION_REPRESENTATION (  '', ( #89760 ), #19206 ) ;
#39803 = ORIENTED_EDGE ( 'NONE', *, *, #65566, .T. ) ;
#39804 = DIRECTION ( 'NONE',  ( -1.000000000000000000, -1.224606353822377258E-16, -0.000000000000000000 ) ) ;
#39805 = CARTESIAN_POINT ( 'NONE',  ( 85.15204736842385103, -38.69186732370133086, 198.5736475422584704 ) ) ;
#39806 = DIRECTION ( 'NONE',  ( -1.000000000000000000, -0.000000000000000000, -0.000000000000000000 ) ) ;
#39807 = CARTESIAN_POINT ( 'NONE',  ( 85.37734265273529388, -52.71760933736054966, 0.7316266844141512404 ) ) ;
#39808 = CARTESIAN_POINT ( 'NONE',  ( 79.77431866835297569, -37.99999999999995026, 142.7581769456982954 ) ) ;
#39809 = CARTESIAN_POINT ( 'NONE',  ( 39.14633636556600038, 314.2407992262670291, 6.611805377155580032 ) ) ;
#39810 = CARTESIAN_POINT ( 'NONE',  ( 10.12102021413156905, 45.41888843717377000, -15.40779740156171762 ) ) ;
#39811 = DIRECTION ( 'NONE',  ( 0.000000000000000000, 0.000000000000000000, -1.000000000000000000 ) ) ;
#39812 = CARTESIAN_POINT ( 'NONE',  ( -28.18119922952890377, 34.32264690212790015, -8.150096433134891072 ) ) ;
#39813 = CARTESIAN_POINT ( 'NONE',  ( -4.844458925425546347, -47.14101111564401947, 103.3760426044494807 ) ) ;
#39814 =( BOUNDED_CURVE ( )  B_SPLINE_CURVE ( 2, ( #69359, #44006, #102238, #20852, #60739, #19780, #69879, #61263, #53686 ),
 .UNSPECIFIED., .F., .F. ) 
 B_SPLINE_CURVE_WITH_KNOTS ( ( 3, 2, 2, 2, 3 ),
 ( 0.6617647058823529216, 0.6691176470588234837, 0.6764705882352941568, 0.6838235294117648300, 0.6911764705882353921 ),
 .UNSPECIFIED. ) 
 CURVE ( )  GEOMETRIC_REPRESENTATION_ITEM ( )  RATIONAL_B_SPLINE_CURVE ( ( 1.000000000000000000, 0.9238795325112867385, 1.000000000000000000, 0.9238795325112867385, 1.000000000000000000, 0.9238795325112867385, 1.000000000000000000, 0.9238795325112856283, 1.000000000000001110 ) ) 
 REPRESENTATION_ITEM ( '' )  );
#39815 = EDGE_CURVE ( 'NONE', #101661, #9600, #3764, .T. ) ;
#39816 = FILL_AREA_STYLE ('',( #88887 ) ) ;
#39817 = CARTESIAN_POINT ( 'NONE',  ( -4.250000000000000000, 5.204748896376250699E-16, -9.078441367943003826 ) ) ;
#39818 = ORIENTED_EDGE ( 'NONE', *, *, #97287, .T. ) ;
#39819 = LINE ( 'NONE', #22054, #1048 ) ;
#39820 = CARTESIAN_POINT ( 'NONE',  ( -29.83138824175510706, 298.2147009232574533, 10.68178215045177026 ) ) ;
#39821 = DIRECTION ( 'NONE',  ( 0.000000000000000000, 1.000000000000000000, 0.000000000000000000 ) ) ;
#39822 = UNCERTAINTY_MEASURE_WITH_UNIT (LENGTH_MEASURE( 1.000000000000000082E-05 ), #36309, 'distance_accuracy_value', 'NONE');
#39823 = DIRECTION ( 'NONE',  ( 0.5735764363510490460, 0.8191520442889896891, 0.000000000000000000 ) ) ;
#39824 = CARTESIAN_POINT ( 'NONE',  ( 8.000000000000000000, -13.99999999999999112, 0.000000000000000000 ) ) ;
#39825 = CARTESIAN_POINT ( 'NONE',  ( 28.03182135562585486, -31.11828738288172502, 39.52190999426944273 ) ) ;
#39826 = PRESENTATION_STYLE_ASSIGNMENT (( #90490 ) ) ;
#39827 = VERTEX_POINT ( 'NONE', #77111 ) ;
#39828 = CARTESIAN_POINT ( 'NONE',  ( 83.92266184464492085, -57.40603453690408031, 190.5289941760056251 ) ) ;
#39829 = CARTESIAN_POINT ( 'NONE',  ( 4.165977904505311358, 16.00000000000000000, -9.090909090909089940 ) ) ;
#39830 = ADVANCED_FACE ( 'NONE', ( #1602 ), #34319, .F. ) ;
#39831 = ORIENTED_EDGE ( 'NONE', *, *, #6161, .T. ) ;
#39832 = CARTESIAN_POINT ( 'NONE',  ( 93.83812592755332105, -57.67477530323803592, 11.02985781185799397 ) ) ;
#39833 = CIRCLE ( 'NONE', #17430, 4.000000000000000888 ) ;
#39834 = AXIS2_PLACEMENT_3D ( 'NONE', #93932, #27644, #93407 ) ;
#39835 = CARTESIAN_POINT ( 'NONE',  ( -16.64348903516521005, 45.88445698070336221, -4.157797401561533768 ) ) ;
#39836 = DIRECTION ( 'NONE',  ( -0.8191520442889884679, 1.003171929053520679E-16, 0.5735764363510509334 ) ) ;
#39837 = CYLINDRICAL_SURFACE ( 'NONE', #4529, 1.250000000000000000 ) ;
#39838 = CIRCLE ( 'NONE', #82858, 4.000000000000001776 ) ;
#39839 = EDGE_CURVE ( 'NONE', #63106, #67261, #75597, .T. ) ;
#39840 = CARTESIAN_POINT ( 'NONE',  ( -64.25898179071923266, -38.00000000000000711, 83.23079767160567144 ) ) ;
#39841 = CARTESIAN_POINT ( 'NONE',  ( 2.617993873628327250, -5.000000000000000000, 10.00000000000000000 ) ) ;
#39842 = CARTESIAN_POINT ( 'NONE',  ( 37.96538461538461462, 1.411358822780289120E-15, 0.000000000000000000 ) ) ;
#39843 = EDGE_CURVE ( 'NONE', #59167, #16558, #18816, .T. ) ;
#39845 = CARTESIAN_POINT ( 'NONE',  ( -11.57142077548166093, 7.251212190646564082, 9.335706481127813205 ) ) ;
#39844 = CARTESIAN_POINT ( 'NONE',  ( 3.910135399454936600, -48.93965050918993143, 104.5757312272370712 ) ) ;
#39846 = VECTOR ( 'NONE', #83992, 1000.000000000000000 ) ;
#39847 = ORIENTED_EDGE ( 'NONE', *, *, #82682, .T. ) ;
#39848 = CARTESIAN_POINT ( 'NONE',  ( -10.50000000000000711, -5.000000000000000000, -79.51734232575269345 ) ) ;
#39849 = CARTESIAN_POINT ( 'NONE',  ( 1.590954573998430099, -4.999999999999999112, -73.00000000000001421 ) ) ;
#39850 = CARTESIAN_POINT ( 'NONE',  ( 9.673800154114786665, 15.30085158940974921, -2.563280883359599027 ) ) ;
#39851 = CARTESIAN_POINT ( 'NONE',  ( 32.04230769230768772, -4.171999999999999709, 0.000000000000000000 ) ) ;
#39852 = CARTESIAN_POINT ( 'NONE',  ( 68.05201484286467917, -29.92325765820791261, -21.69912042315977985 ) ) ;
#39853 = ADVANCED_FACE ( 'NONE', ( #14470 ), #89389, .T. ) ;
#39854 = EDGE_CURVE ( 'NONE', #54950, #82447, #30822, .T. ) ;
#39855 = ORIENTED_EDGE ( 'NONE', *, *, #37648, .F. ) ;
#39856 = CARTESIAN_POINT ( 'NONE',  ( 0.1306530452038086043, 5.952467836904148157, -5.690023276062398772 ) ) ;
#39857 = DIRECTION ( 'NONE',  ( 0.000000000000000000, 1.000000000000000000, 0.000000000000000000 ) ) ;
#39858 = CARTESIAN_POINT ( 'NONE',  ( -59.86887900601052337, -21.77002156294910051, -23.08918318703028660 ) ) ;
#39859 = VERTEX_POINT ( 'NONE', #79755 ) ;
#39860 = AXIS2_PLACEMENT_3D ( 'NONE', #94399, #61504, #96906 ) ;
#39861 = ORIENTED_EDGE ( 'NONE', *, *, #19814, .T. ) ;
#39862 = CARTESIAN_POINT ( 'NONE',  ( 10.45316333433563649, 43.22580471055811557, -15.39941299950120523 ) ) ;
#39863 = AXIS2_PLACEMENT_3D ( 'NONE', #12367, #43159, #45292 ) ;
#39864 = CARTESIAN_POINT ( 'NONE',  ( -92.38893592253350562, -60.00000000000000711, 0.3012529127975949739 ) ) ;
#39865 = ORIENTED_EDGE ( 'NONE', *, *, #38428, .F. ) ;
#39866 = CARTESIAN_POINT ( 'NONE',  ( 64.13695837427279400, -37.76356166761983246, -24.56640574812671574 ) ) ;
#39867 = CARTESIAN_POINT ( 'NONE',  ( -9.607634652977999679, 15.83450757143046950, 2.797224791467300076 ) ) ;
#39868 = CARTESIAN_POINT ( 'NONE',  ( -3.415268428525006339, -0.8295777316436665494, 103.8819066263154411 ) ) ;
#39870 = CARTESIAN_POINT ( 'NONE',  ( -17.27438113373179362, 45.65101552804006246, 4.281429632575695976 ) ) ;
#39869 = CARTESIAN_POINT ( 'NONE',  ( 63.07777777777777573, -3.309500000000000774, 0.000000000000000000 ) ) ;
#39871 = CARTESIAN_POINT ( 'NONE',  ( -82.07322838537869814, -42.97417978104021330, 166.6889830305388784 ) ) ;
#39872 = ORIENTED_EDGE ( 'NONE', *, *, #66370, .F. ) ;
#39873 = ORIENTED_EDGE ( 'NONE', *, *, #4373, .F. ) ;
#39874 = VERTEX_POINT ( 'NONE', #39323 ) ;
#39875 = EDGE_CURVE ( 'NONE', #63425, #87056, #41319, .T. ) ;
#39876 = CARTESIAN_POINT ( 'NONE',  ( -5.977446511990853750, -14.23238268868709611, 14.05797248976396574 ) ) ;
#39877 = SURFACE_SIDE_STYLE ('',( #31280 ) ) ;
#39878 = ORIENTED_EDGE ( 'NONE', *, *, #47917, .F. ) ;
#39879 = CARTESIAN_POINT ( 'NONE',  ( -32.84724476090489986, 479.6963199345864268, 7.498190490636539529 ) ) ;
#39880 = CARTESIAN_POINT ( 'NONE',  ( -113.4944653854903862, 14.17434517210798006, -56.74723269274520732 ) ) ;
#39881 = CARTESIAN_POINT ( 'NONE',  ( -10.00000000000000000, 15.00000000000000000, -4.582575694955836276 ) ) ;
#39882 = CARTESIAN_POINT ( 'NONE',  ( -112.2456557016906942, -57.67113047748567567, 190.5314477545807392 ) ) ;
#39883 = CARTESIAN_POINT ( 'NONE',  ( -9.994350908930156763, 294.6428469334700253, -0.7388987851124564354 ) ) ;
#39884 = CARTESIAN_POINT ( 'NONE',  ( -20.34819189090134017, 294.7750624004232805, -2.016311483866853660 ) ) ;
#39885 = CARTESIAN_POINT ( 'NONE',  ( -0.08410583490319520350, 26.07813853931757464, 38.25000000000002132 ) ) ;
#39886 = FACE_OUTER_BOUND ( 'NONE', #8172, .T. ) ;
#39887 = EDGE_CURVE ( 'NONE', #73382, #86709, #54868, .T. ) ;
#39888 = CARTESIAN_POINT ( 'NONE',  ( -55.21321105934377726, -60.00000000000002842, -39.23988760269474341 ) ) ;
#39889 = CARTESIAN_POINT ( 'NONE',  ( -4.090533018665307274, -14.21045842199441722, 34.36071901318091903 ) ) ;
#39890 = CARTESIAN_POINT ( 'NONE',  ( -53.74619955778950242, -42.97187427616553634, 59.00820073232069518 ) ) ;
#39891 = CARTESIAN_POINT ( 'NONE',  ( 0.000000000000000000, 0.000000000000000000, -0.7702282920306786629 ) ) ;
#39892 = EDGE_LOOP ( 'NONE', ( #72432, #74673 ) ) ;
#39893 = CARTESIAN_POINT ( 'NONE',  ( -98.97495582109610268, -52.78644234849187455, 194.7710799945916165 ) ) ;
#39894 = CARTESIAN_POINT ( 'NONE',  ( -3.001409217703660648, 294.8245242021811237, -9.555569693199137404 ) ) ;
#39895 = ORIENTED_EDGE ( 'NONE', *, *, #32994, .F. ) ;
#39896 = CARTESIAN_POINT ( 'NONE',  ( -17.46661644397501689, 43.23536754299439622, 6.352185647016465708 ) ) ;
#39897 = B_SPLINE_CURVE_WITH_KNOTS ( 'NONE', 3,
 ( #17159, #908, #50548, #83463, #9563, #42470 ),
 .UNSPECIFIED., .F., .F.,
 ( 4, 2, 4 ),
 ( 2.380733003137416059E-07, 0.001898835937927372897, 0.003797433802554431997 ),
 .UNSPECIFIED. ) ;
#39898 = CARTESIAN_POINT ( 'NONE',  ( 91.38085702308197256, -38.39709809381331240, -9.519024297102184562 ) ) ;
#39899 = CARTESIAN_POINT ( 'NONE',  ( 48.91605700228181064, 13.22299455561256387, 16.49079035033173568 ) ) ;
#39900 = CARTESIAN_POINT ( 'NONE',  ( 2.977408999572650927, -10.25000000204838813, -7.188101187500001821 ) ) ;
#39901 = CIRCLE ( 'NONE', #70859, 4.000000000000007105 ) ;
#39902 = CARTESIAN_POINT ( 'NONE',  ( -13.81794228156022974, 302.5467222371539719, 9.872154306231394116 ) ) ;
#39903 = DIRECTION ( 'NONE',  ( -0.02876443886042204245, 0.9995862179207181120, 0.000000000000000000 ) ) ;
#39904 = CARTESIAN_POINT ( 'NONE',  ( 80.21334409234347618, -30.00000000000000000, 135.6879503079539688 ) ) ;
#39905 = CARTESIAN_POINT ( 'NONE',  ( 3.398996499095806811, 303.8518027749813655, -10.00000000027310421 ) ) ;
#39906 = DIRECTION ( 'NONE',  ( 0.5735764363510490460, 0.8191520442889896891, 0.000000000000000000 ) ) ;
#39907 = DIRECTION ( 'NONE',  ( -1.000000000000000000, 0.000000000000000000, 0.000000000000000000 ) ) ;
#39908 = ADVANCED_FACE ( 'NONE', ( #90508 ), #49511, .T. ) ;
#39909 = FACE_OUTER_BOUND ( 'NONE', #63540, .T. ) ;
#39910 = ORIENTED_EDGE ( 'NONE', *, *, #57838, .F. ) ;
#39911 = ORIENTED_EDGE ( 'NONE', *, *, #13163, .T. ) ;
#39912 = CARTESIAN_POINT ( 'NONE',  ( 48.85299720893686981, -25.67496275475526346, 44.56502496020352311 ) ) ;
#39913 = CARTESIAN_POINT ( 'NONE',  ( 6.738100180926640093, 41.71798714554645215, -59.05424661244425266 ) ) ;
#39914 = AXIS2_PLACEMENT_3D ( 'NONE', #51289, #102521, #26545 ) ;
#39915 = CARTESIAN_POINT ( 'NONE',  ( 8.559508646656405872, 51.55638410492942825, 4.031152949374444461 ) ) ;
#39916 = STYLED_ITEM ( 'NONE', ( #18782 ), #74678 ) ;
#39917 = ORIENTED_EDGE ( 'NONE', *, *, #98874, .F. ) ;
#39919 = ADVANCED_FACE ( 'NONE', ( #23680 ), #20650, .T. ) ;
#39918 = CARTESIAN_POINT ( 'NONE',  ( -110.1014534723386191, -38.35607734749763864, 185.3304993136136432 ) ) ;
#39920 = ORIENTED_EDGE ( 'NONE', *, *, #3338, .T. ) ;
#39921 = CARTESIAN_POINT ( 'NONE',  ( 110.1708031426684187, -38.35604441332869641, 156.5327596993846839 ) ) ;
#39922 = CARTESIAN_POINT ( 'NONE',  ( 10.18861149534500932, 16.01981654604731986, -10.17146396841989109 ) ) ;
#39923 = CARTESIAN_POINT ( 'NONE',  ( -19.45165646949288885, 49.97831066704853953, 60.61089002369819667 ) ) ;
#39924 = DIRECTION ( 'NONE',  ( 0.000000000000000000, -1.000000000000000000, 0.000000000000000000 ) ) ;
#39925 = CARTESIAN_POINT ( 'NONE',  ( 104.9571888707694427, -60.15142560926327064, 149.1774971079043723 ) ) ;
#39926 = CARTESIAN_POINT ( 'NONE',  ( -32.05181932688683588, 439.7174019519748072, 23.91393675278271758 ) ) ;
#39927 = CARTESIAN_POINT ( 'NONE',  ( -27.23735134814286951, 307.8362383646490343, -8.331602159243709949 ) ) ;
#39928 = CARTESIAN_POINT ( 'NONE',  ( -16.75187969033532553, 34.25544727262118982, 24.30698433968612449 ) ) ;
#39929 = CARTESIAN_POINT ( 'NONE',  ( 80.08440833438228879, -60.00000000000001421, 196.0901278236156600 ) ) ;
#39930 = FACE_OUTER_BOUND ( 'NONE', #97237, .T. ) ;
#39931 = ORIENTED_EDGE ( 'NONE', *, *, #24443, .F. ) ;
#39932 = CARTESIAN_POINT ( 'NONE',  ( 57.65574661060767880, -49.90878574621957142, 71.01292799359110575 ) ) ;
#39933 = CARTESIAN_POINT ( 'NONE',  ( -33.36333480850094446, 300.5116995142376481, -0.7277600820885061772 ) ) ;
#39934 = EDGE_CURVE ( 'NONE', #68006, #33682, #60659, .T. ) ;
#39935 = CARTESIAN_POINT ( 'NONE',  ( 9.286995370816610418, -52.22232280126255688, 30.70990524772856034 ) ) ;
#39936 = PRESENTATION_LAYER_ASSIGNMENT (  '', '', ( #64047 ) ) ;
#39937 = SURFACE_SIDE_STYLE ('',( #48001 ) ) ;
#39938 = EDGE_LOOP ( 'NONE', ( #70672, #53772, #61122, #62863, #32695, #62941 ) ) ;
#39940 = CARTESIAN_POINT ( 'NONE',  ( -9.499205784528923502, -51.35693084752516313, 30.13083833152229829 ) ) ;
#39939 = CARTESIAN_POINT ( 'NONE',  ( -90.72701990683636097, -38.34112183637917326, 6.693821972579170776 ) ) ;
#39941 = CARTESIAN_POINT ( 'NONE',  ( 17.33349330513380337, -4.000000000000000000, 4.898587196589415787E-16 ) ) ;
#39942 = CARTESIAN_POINT ( 'NONE',  ( 24.10451817204156910, 306.3800824377233880, 9.276234954072691608 ) ) ;
#39943 = DIRECTION ( 'NONE',  ( -1.000000000000000000, -0.000000000000000000, -0.000000000000000000 ) ) ;
#39944 = CARTESIAN_POINT ( 'NONE',  ( -1.469576158976823947E-15, -33.87499999999999289, 8.000000000000000000 ) ) ;
#39945 = AXIS2_PLACEMENT_3D ( 'NONE', #56044, #80871, #66290 ) ;
#39946 = CARTESIAN_POINT ( 'NONE',  ( -17.49999999999996803, 46.94999999999998153, 64.09953197957064219 ) ) ;
#39947 = CARTESIAN_POINT ( 'NONE',  ( 80.97977184163765685, 1.030564683017419500E-14, 0.000000000000000000 ) ) ;
#39948 = ORIENTED_EDGE ( 'NONE', *, *, #45516, .T. ) ;
#39949 = CARTESIAN_POINT ( 'NONE',  ( 81.25017303853442741, -60.55690295631904263, 184.6554220054742075 ) ) ;
#39950 = ADVANCED_FACE ( 'NONE', ( #25831 ), #68373, .T. ) ;
#39951 = DIRECTION ( 'NONE',  ( -0.9086146812040659659, 0.000000000000000000, 0.4176354404267356157 ) ) ;
#39952 = CARTESIAN_POINT ( 'NONE',  ( 37.40771152851837655, 27.94111240654205730, 10.95617127780990607 ) ) ;
#39953 = VERTEX_POINT ( 'NONE', #35497 ) ;
#39954 = DIRECTION ( 'NONE',  ( -1.000000000000000000, -1.224606353822377258E-16, -0.000000000000000000 ) ) ;
#39955 = CARTESIAN_POINT ( 'NONE',  ( 6.617039711668479818, -4.368567403894799916, -16.80329192430645335 ) ) ;
#39956 = CARTESIAN_POINT ( 'NONE',  ( 27.10511071441176156, 34.47735702144343861, -10.05698433968637673 ) ) ;
#39957 = CARTESIAN_POINT ( 'NONE',  ( 14.89763918506130835, 1.348991191049166538, 1.758109506431186686 ) ) ;
#39958 = CARTESIAN_POINT ( 'NONE',  ( -43.29298354046672159, 41.46939958648897573, -50.98198775960019447 ) ) ;
#39959 = CARTESIAN_POINT ( 'NONE',  ( -28.43259016867738609, 12.18852863928159991, -40.99039043055300624 ) ) ;
#39960 = EDGE_CURVE ( 'NONE', #15279, #67879, #26358, .T. ) ;
#39961 = ORIENTED_EDGE ( 'NONE', *, *, #54374, .F. ) ;
#39962 =( NAMED_UNIT ( * ) PLANE_ANGLE_UNIT ( ) SI_UNIT ( $, .RADIAN. ) );
#39963 = CARTESIAN_POINT ( 'NONE',  ( 6.499999999999999112, 4.077976443323001909, -6.122137821720841977 ) ) ;
#39964 = DIRECTION ( 'NONE',  ( 0.000000000000000000, 1.000000000000000000, 0.000000000000000000 ) ) ;
#39965 = EDGE_CURVE ( 'NONE', #91921, #82451, #67137, .T. ) ;
#39967 = CARTESIAN_POINT ( 'NONE',  ( -11.09180518623727529, 10.57614021777674118, -9.722244198893070788 ) ) ;
#39966 = DIRECTION ( 'NONE',  ( -1.000000000000000000, -1.224606353822377258E-16, -0.000000000000000000 ) ) ;
#39968 = CARTESIAN_POINT ( 'NONE',  ( 7.188101187499999156, -16.25000000204838813, 2.977408999572654924 ) ) ;
#39969 = FACE_OUTER_BOUND ( 'NONE', #13240, .T. ) ;
#39970 = DIRECTION ( 'NONE',  ( 0.000000000000000000, 1.000000000000000000, 0.000000000000000000 ) ) ;
#39971 = ORIENTED_EDGE ( 'NONE', *, *, #97831, .F. ) ;
#39972 = COLOUR_RGB ( '', 0.31764706, 0.68627451, 0.89019608) ;
#39973 = CARTESIAN_POINT ( 'NONE',  ( 0.000000000000000000, 0.000000000000000000, 4.000000000000000000 ) ) ;
#39974 = DIRECTION ( 'NONE',  ( -0.8191520442889974607, 0.000000000000000000, -0.5735764363510379438 ) ) ;
#39975 = PRESENTATION_LAYER_ASSIGNMENT (  '', '', ( #86516 ) ) ;
#39976 = CARTESIAN_POINT ( 'NONE',  ( -3.148155568693087769, 111.7595494157684612, -5.000000000000000000 ) ) ;
#39977 = CARTESIAN_POINT ( 'NONE',  ( 0.000000000000000000, 0.000000000000000000, -0.01269999999999830292 ) ) ;
#39978 = CARTESIAN_POINT ( 'NONE',  ( -15.22818746202677787, 3.929489829936595235, 4.609438620834709788 ) ) ;
#39979 = B_SPLINE_CURVE_WITH_KNOTS ( 'NONE', 3,
 ( #23906, #56202, #104786, #105321, #31464, #96702 ),
 .UNSPECIFIED., .F., .F.,
 ( 4, 2, 4 ),
 ( 0.006874058789394420221, 0.008773169699889928064, 0.01067228061038543591 ),
 .UNSPECIFIED. ) ;
#39980 = ORIENTED_EDGE ( 'NONE', *, *, #12978, .T. ) ;
#39981 = CARTESIAN_POINT ( 'NONE',  ( 44.21332904831284338, 435.2494715644500616, 14.45449769377396976 ) ) ;
#39982 = DIRECTION ( 'NONE',  ( -0.5000109054779156015, 0.000000000000000000, 0.8660191074122758348 ) ) ;
#39984 = EDGE_LOOP ( 'NONE', ( #7211, #19934 ) ) ;
#39983 = AXIS2_PLACEMENT_3D ( 'NONE', #10823, #93898, #100907 ) ;
#39985 = AXIS2_PLACEMENT_3D ( 'NONE', #45682, #40753, #97386 ) ;
#39986 = CARTESIAN_POINT ( 'NONE',  ( 84.15356149169568312, -2.002967142162725287E-29, 5.000000000000011546 ) ) ;
#39987 = CARTESIAN_POINT ( 'NONE',  ( 16.14595037822607182, 6.785770140112303395, -6.193810554583006223 ) ) ;
#39988 = CARTESIAN_POINT ( 'NONE',  ( -109.0276826879899943, -60.00000000000000711, 136.1730525503504907 ) ) ;
#39989 = CARTESIAN_POINT ( 'NONE',  ( 29.68315524076926692, 13.47185074185900255, -42.10535821593530414 ) ) ;
#39990 = CARTESIAN_POINT ( 'NONE',  ( 43.66694997075330775, 484.4025358507092278, 1.806736142167242321 ) ) ;
#39991 = CARTESIAN_POINT ( 'NONE',  ( 0.000000000000000000, 4.898587196589412829E-16, -4.000000000000000000 ) ) ;
#39992 = DIRECTION ( 'NONE',  ( -1.000000000000000000, 0.000000000000000000, 0.000000000000000000 ) ) ;
#39994 = DIRECTION ( 'NONE',  ( -0.000000000000000000, -1.000000000000000000, -0.000000000000000000 ) ) ;
#39993 = CARTESIAN_POINT ( 'NONE',  ( 9.999999999999996447, -5.000000000000002665, -86.30899693748767731 ) ) ;
#39995 = CARTESIAN_POINT ( 'NONE',  ( -84.93114117115241868, -28.90604097065245881, 171.9502745002261292 ) ) ;
#39996 = ORIENTED_EDGE ( 'NONE', *, *, #21752, .T. ) ;
#39997 = ORIENTED_EDGE ( 'NONE', *, *, #93001, .F. ) ;
#39998 = VERTEX_POINT ( 'NONE', #93710 ) ;
#39999 = DIRECTION ( 'NONE',  ( -1.000000000000000000, -1.224606353822377258E-16, -0.000000000000000000 ) ) ;
#40000 = EDGE_CURVE ( 'NONE', #105135, #27903, #79899, .T. ) ;
#40001 = CARTESIAN_POINT ( 'NONE',  ( 33.77559172535808329, 464.7834715296607442, 7.192701217093171451 ) ) ;
#40002 = AXIS2_PLACEMENT_3D ( 'NONE', #106057, #47823, #22546 ) ;
#40003 = CARTESIAN_POINT ( 'NONE',  ( 0.000000000000000000, 273.9999999999999432, 0.000000000000000000 ) ) ;
#40004 = AXIS2_PLACEMENT_3D ( 'NONE', #8728, #90186, #66985 ) ;
#40005 = CARTESIAN_POINT ( 'NONE',  ( 8.986804597294771213, 15.43199845812625703, -5.000000000000000888 ) ) ;
#40006 = CARTESIAN_POINT ( 'NONE',  ( 0.000000000000000000, -50.00000000000000000, 27.00000000000000000 ) ) ;
#40007 = DIRECTION ( 'NONE',  ( 1.000000000000000000, 1.224606353822377258E-16, 0.000000000000000000 ) ) ;
#40008 = EDGE_CURVE ( 'NONE', #18717, #44354, #85082, .T. ) ;
#40009 = CARTESIAN_POINT ( 'NONE',  ( 114.2222497212829495, -60.00000000000000000, 162.1251737369585726 ) ) ;
#40010 = CARTESIAN_POINT ( 'NONE',  ( -106.9310521912263710, -14.21045842199434794, 169.9232300575910131 ) ) ;
#40011 = CARTESIAN_POINT ( 'NONE',  ( -61.75299678764660882, -42.96448552206198457, 78.62763974756443019 ) ) ;
#40012 = ORIENTED_EDGE ( 'NONE', *, *, #51316, .T. ) ;
#40013 = CARTESIAN_POINT ( 'NONE',  ( -28.16608175993714269, 38.95286782169205253, 57.17295417723011042 ) ) ;
#40014 = CARTESIAN_POINT ( 'NONE',  ( 104.9308453125034646, -60.00000000000243006, 202.2520219887860549 ) ) ;
#40015 = ORIENTED_EDGE ( 'NONE', *, *, #49242, .T. ) ;
#40016 = CARTESIAN_POINT ( 'NONE',  ( 13.45079846400083312, -54.00000000000000711, 23.11721482942554928 ) ) ;
#40017 = CARTESIAN_POINT ( 'NONE',  ( 2.977408999572650927, -11.75000000204838813, -7.188101187500000933 ) ) ;
#40018 = AXIS2_PLACEMENT_3D ( 'NONE', #16436, #56880, #73596 ) ;
#40019 = DIRECTION ( 'NONE',  ( 1.000000000000000000, 1.224606353822377258E-16, 0.000000000000000000 ) ) ;
#40020 = ORIENTED_EDGE ( 'NONE', *, *, #55828, .T. ) ;
#40021 = CARTESIAN_POINT ( 'NONE',  ( -10.61653353389834464, 45.33051817006433737, 15.36625836153905489 ) ) ;
#40022 = ORIENTED_EDGE ( 'NONE', *, *, #51003, .F. ) ;
#40023 = CARTESIAN_POINT ( 'NONE',  ( 11.53815258514788411, 45.46891437459016316, -14.20004885619772139 ) ) ;
#40024 = CARTESIAN_POINT ( 'NONE',  ( 0.000000000000000000, 0.000000000000000000, 0.000000000000000000 ) ) ;
#40025 = CARTESIAN_POINT ( 'NONE',  ( -84.00882247759808763, -60.00000000000006395, 199.5195877717709152 ) ) ;
#40026 = CARTESIAN_POINT ( 'NONE',  ( 9.574118164638793615, -56.64626512664418811, 24.10642939627973291 ) ) ;
#40027 = CARTESIAN_POINT ( 'NONE',  ( 5.082755093536325930, -26.84375000204838813, -5.082755093536325042 ) ) ;
#40028 = CARTESIAN_POINT ( 'NONE',  ( 43.89455633144091706, 462.7155212543453331, 5.467842138882834213 ) ) ;
#40029 = CARTESIAN_POINT ( 'NONE',  ( -13.46456120603693662, 20.01150154851706020, 7.140757873385461529 ) ) ;
#40030 = CARTESIAN_POINT ( 'NONE',  ( -10.68563486923847705, -4.999065512597902661, -12.55094748029354790 ) ) ;
#40031 = CARTESIAN_POINT ( 'NONE',  ( 8.018229784881205191, -5.437562848952134154, 14.17839565075627739 ) ) ;
#40032 = ADVANCED_FACE ( 'NONE', ( #34967 ), #67830, .T. ) ;
#40033 = CARTESIAN_POINT ( 'NONE',  ( 102.6429790572119458, -59.99999999999993605, 193.3319502104955916 ) ) ;
#40034 = CARTESIAN_POINT ( 'NONE',  ( -32.74448902475613465, -42.96476387111531636, 34.86933629716781269 ) ) ;
#40035 = B_SPLINE_CURVE_WITH_KNOTS ( 'NONE', 3,
 ( #36051, #60826, #51105, #61900, #93718, #85635, #10646, #43563, #92641, #76449, #94795, #44102, #84023, #26890, #59764, #10129, #43038, #28479, #12248, #44646, #77530, #3647, #69448, #2027, #18799, #29034, #86176, #45178, #34975, #100728, #2558, #35506, #68384, #76992 ),
 .UNSPECIFIED., .F., .F.,
 ( 4, 2, 2, 2, 2, 2, 2, 2, 2, 2, 2, 2, 2, 2, 2, 2, 4 ),
 ( 1.422579022190208801E-17, 0.0007899309203816186776, 0.001579861840763223261, 0.002369792761144827627, 0.003159723681526432210, 0.003949654601908035925, 0.004739585522289640508, 0.005529516442671245091, 0.006319447363052849674, 0.007109378283434454257, 0.007899309203816057973, 0.008689240124197663423, 0.009479171044579267139, 0.01026910196496087259, 0.01105903288534247630, 0.01184896380572408175, 0.01263889472610568547 ),
 .UNSPECIFIED. ) ;
#40036 = CARTESIAN_POINT ( 'NONE',  ( -14.91339176601158734, 41.98696008795855050, -86.62219925848569346 ) ) ;
#40037 = CARTESIAN_POINT ( 'NONE',  ( 37.36725091415993205, -25.66895752586749069, 33.86584213023738243 ) ) ;
#40038 = CARTESIAN_POINT ( 'NONE',  ( -4.453875240773214728, -1.734723475976807094E-15, -16.57301948837565675 ) ) ;
#40039 = VERTEX_POINT ( 'NONE', #50556 ) ;
#40040 = CARTESIAN_POINT ( 'NONE',  ( 32.99999999999998579, 464.3970849722209095, 17.41240408234205717 ) ) ;
#40041 = CARTESIAN_POINT ( 'NONE',  ( -66.95983133501314910, -38.33558760111643693, 121.1209903420379703 ) ) ;
#40042 = ORIENTED_EDGE ( 'NONE', *, *, #90756, .T. ) ;
#40044 = CARTESIAN_POINT ( 'NONE',  ( 35.96492786661492858, 302.4488314805894902, -8.278427239160079054 ) ) ;
#40043 = FACE_OUTER_BOUND ( 'NONE', #10270, .T. ) ;
#40045 = FACE_OUTER_BOUND ( 'NONE', #64033, .T. ) ;
#40046 = DIRECTION ( 'NONE',  ( 1.000000000000000000, 0.000000000000000000, 0.000000000000000000 ) ) ;
#40047 = DIRECTION ( 'NONE',  ( 0.000000000000000000, 1.000000000000000000, 0.000000000000000000 ) ) ;
#40048 = DIRECTION ( 'NONE',  ( 0.000000000000000000, -0.000000000000000000, 1.000000000000000000 ) ) ;
#40049 = CARTESIAN_POINT ( 'NONE',  ( -31.39112176491482842, 426.5443834901637956, 23.68269498481550173 ) ) ;
#40050 = CARTESIAN_POINT ( 'NONE',  ( 0.06809871960542614178, -7.710219529346607814, 2.645508037661882472 ) ) ;
#40051 = CARTESIAN_POINT ( 'NONE',  ( 93.30919872547751481, -59.99999999999999289, 35.28464305277864810 ) ) ;
#40053 = CARTESIAN_POINT ( 'NONE',  ( -7.000000000000000000, -46.00000000000000000, 39.12435565298213902 ) ) ;
#40052 = VECTOR ( 'NONE', #99099, 1000.000000000000114 ) ;
#40054 = CARTESIAN_POINT ( 'NONE',  ( -16.64348903516517098, 43.47556584774767430, 6.657797401561654560 ) ) ;
#40055 = CARTESIAN_POINT ( 'NONE',  ( 8.990409435383423187, -4.999999999999999112, -71.93151781320761984 ) ) ;
#40056 = ORIENTED_EDGE ( 'NONE', *, *, #42504, .F. ) ;
#40057 = CARTESIAN_POINT ( 'NONE',  ( -61.17075129193928973, -30.00000000000000711, 69.80672871272592772 ) ) ;
#40058 = ORIENTED_EDGE ( 'NONE', *, *, #51719, .F. ) ;
#40059 = FACE_OUTER_BOUND ( 'NONE', #49819, .T. ) ;
#40060 =( NAMED_UNIT ( * ) PLANE_ANGLE_UNIT ( ) SI_UNIT ( $, .RADIAN. ) );
#40061 = CARTESIAN_POINT ( 'NONE',  ( 8.588409832221012508, 23.79849351030796711, -1.228354175402838067E-12 ) ) ;
#40062 = CARTESIAN_POINT ( 'NONE',  ( 25.11650669486618881, 0.000000000000000000, 4.000000000000000888 ) ) ;
#40063 = CARTESIAN_POINT ( 'NONE',  ( -22.57912246414728585, 28.20550200792851214, -30.87816999938245033 ) ) ;
#40064 = AXIS2_PLACEMENT_3D ( 'NONE', #19543, #61032, #43242 ) ;
#40065 = CARTESIAN_POINT ( 'NONE',  ( 7.188101187499999156, -27.12500000204838457, 2.977408999572654924 ) ) ;
#40066 = CARTESIAN_POINT ( 'NONE',  ( 46.85000000000000142, 0.000000000000000000, 0.000000000000000000 ) ) ;
#40067 = CARTESIAN_POINT ( 'NONE',  ( 7.078150634444296152, 41.46400361730934492, -70.18186710228739855 ) ) ;
#40068 = ORIENTED_EDGE ( 'NONE', *, *, #3329, .F. ) ;
#40070 = ORIENTED_EDGE ( 'NONE', *, *, #31191, .T. ) ;
#40069 = CARTESIAN_POINT ( 'NONE',  ( 28.86650669486618881, 1.474610560812782335E-15, 0.000000000000000000 ) ) ;
#40071 = CARTESIAN_POINT ( 'NONE',  ( 83.25407933603389665, -18.68591088087092089, 143.1428255547100150 ) ) ;
#40072 = CARTESIAN_POINT ( 'NONE',  ( 6.400000000000000355, 9.797174393178825657E-16, -8.000000000000000000 ) ) ;
#40073 = DIRECTION ( 'NONE',  ( -1.000000000000000000, -0.000000000000000000, -0.000000000000000000 ) ) ;
#40074 = VERTEX_POINT ( 'NONE', #100720 ) ;
#40075 =( LENGTH_UNIT ( ) NAMED_UNIT ( * ) SI_UNIT ( .MILLI., .METRE. ) );
#40076 = CARTESIAN_POINT ( 'NONE',  ( -14.29190075645216851, 12.99999999999999289, 0.000000000000000000 ) ) ;
#40077 = CARTESIAN_POINT ( 'NONE',  ( 4.401442555609581635E-16, -11.28125000204838457, -7.188101187500000044 ) ) ;
#40078 = CARTESIAN_POINT ( 'NONE',  ( 25.59999999999999787, -3.309499999999999886, 4.475777889183790779E-16 ) ) ;
#40080 = CARTESIAN_POINT ( 'NONE',  ( -50.71028374685950268, -57.67771315371629726, 79.11066721451838646 ) ) ;
#40079 = CIRCLE ( 'NONE', #3898, 4.000000000000007105 ) ;
#40081 = DIRECTION ( 'NONE',  ( -1.000000000000000000, -1.224606353822377258E-16, -0.000000000000000000 ) ) ;
#40082 = EDGE_CURVE ( 'NONE', #32960, #54991, #15729, .T. ) ;
#40083 = VERTEX_POINT ( 'NONE', #59755 ) ;
#40084 = EDGE_CURVE ( 'NONE', #59054, #74620, #98065, .T. ) ;
#40085 = PRESENTATION_STYLE_ASSIGNMENT (( #23395 ) ) ;
#40086 = STYLED_ITEM ( 'NONE', ( #3859 ), #94617 ) ;
#40087 = CARTESIAN_POINT ( 'NONE',  ( 3.021254343616690097, 104.3205651224084249, 4.999999999999999112 ) ) ;
#40088 = CARTESIAN_POINT ( 'NONE',  ( 7.484956712770276965, 40.70737338351729306, -59.65999187730301401 ) ) ;
#40089 = EDGE_CURVE ( 'NONE', #25901, #63111, #45687, .T. ) ;
#40090 = CARTESIAN_POINT ( 'NONE',  ( -6.499999999999999112, -1.604619215278546562E-14, -5.592027715088706330 ) ) ;
#40091 = ORIENTED_EDGE ( 'NONE', *, *, #51112, .F. ) ;
#40092 = CARTESIAN_POINT ( 'NONE',  ( -5.656854249492379694, -10.62500000409677092, -5.656854249492380582 ) ) ;
#40093 = CARTESIAN_POINT ( 'NONE',  ( -20.83805790964204263, -17.45317829300839207, 31.47035416265072527 ) ) ;
#40094 = CARTESIAN_POINT ( 'NONE',  ( -39.18961397227251098, 489.8685109512363738, 11.78848534766373746 ) ) ;
#40095 = VECTOR ( 'NONE', #65399, 1000.000000000000000 ) ;
#40096 = CARTESIAN_POINT ( 'NONE',  ( 0.1698589296850801789, 52.17552313485973770, -7.758756120565298176 ) ) ;
#40097 = CARTESIAN_POINT ( 'NONE',  ( -3.220999722221654600E-16, 7.895640089090876224, -6.564402953523721607 ) ) ;
#40098 = CARTESIAN_POINT ( 'NONE',  ( 33.21102376836596903, 438.9613914113129454, 23.92328486949907784 ) ) ;
#40099 = PRODUCT_CONTEXT ( 'NONE', #56217, 'mechanical' ) ;
#40100 = CARTESIAN_POINT ( 'NONE',  ( 3.400000000000000355, 0.000000000000000000, -8.000000000000000000 ) ) ;
#40101 = ORIENTED_EDGE ( 'NONE', *, *, #33268, .F. ) ;
#40102 = CARTESIAN_POINT ( 'NONE',  ( -4.783461066586094823, -47.30494748504202107, 42.83084740999873219 ) ) ;
#40103 = EDGE_CURVE ( 'NONE', #104525, #61960, #24737, .T. ) ;
#40104 = DIRECTION ( 'NONE',  ( -1.000000000000000000, -1.224606353822377258E-16, -0.000000000000000000 ) ) ;
#40105 = CARTESIAN_POINT ( 'NONE',  ( 13.49450391516581504, 42.88037855346097871, -91.94812430286241067 ) ) ;
#40106 = CARTESIAN_POINT ( 'NONE',  ( -52.71312636462211287, -36.17903179718669548, -35.74065954623077346 ) ) ;
#40107 = CARTESIAN_POINT ( 'NONE',  ( -8.400342417351219037E-11, 303.8518027762758038, 8.936999415352287812 ) ) ;
#40108 = VERTEX_POINT ( 'NONE', #20405 ) ;
#40109 = CARTESIAN_POINT ( 'NONE',  ( -26.78668668169135358, 36.71437112124606017, -10.05698433968604810 ) ) ;
#40110 = CARTESIAN_POINT ( 'NONE',  ( 86.90535743190535811, -57.58543819784419782, 203.0634495632118899 ) ) ;
#40111 = CARTESIAN_POINT ( 'NONE',  ( 35.02700494597931424, 463.8298975055690221, 19.03023931480278463 ) ) ;
#40112 = CARTESIAN_POINT ( 'NONE',  ( -9.807649484915852867, 51.30023088812457388, -2.672895936288036012 ) ) ;
#40113 = CARTESIAN_POINT ( 'NONE',  ( 64.32759900502375672, 40.83906611471775250, -11.06576400654987147 ) ) ;
#40114 = CARTESIAN_POINT ( 'NONE',  ( -74.33902240994966348, -59.99999999999999289, 175.5866348027616937 ) ) ;
#40115 = AXIS2_PLACEMENT_3D ( 'NONE', #82469, #106187, #65222 ) ;
#40116 = CARTESIAN_POINT ( 'NONE',  ( -36.91281931599076671, 303.7809130842520631, -7.959270006439831846 ) ) ;
#40117 =( NAMED_UNIT ( * ) PLANE_ANGLE_UNIT ( ) SI_UNIT ( $, .RADIAN. ) );
#40118 = CARTESIAN_POINT ( 'NONE',  ( -40.95595929481465447, 405.2208686710653183, 27.85131585683114963 ) ) ;
#40119 = CARTESIAN_POINT ( 'NONE',  ( -85.57874514396658583, -35.68260388560343443, 183.8368203787026118 ) ) ;
#40120 = ORIENTED_EDGE ( 'NONE', *, *, #10972, .T. ) ;
#40121 = CARTESIAN_POINT ( 'NONE',  ( 30.73677158032236889, 310.9900250146528151, -8.337346309561983304 ) ) ;
#40122 =( GEOMETRIC_REPRESENTATION_CONTEXT ( 3 ) GLOBAL_UNCERTAINTY_ASSIGNED_CONTEXT ( ( #3909 ) ) GLOBAL_UNIT_ASSIGNED_CONTEXT ( ( #80965, #105781, #90135 ) ) REPRESENTATION_CONTEXT ( 'NONE', 'WORKASPACE' ) );
#40123 = EDGE_LOOP ( 'NONE', ( #71090, #35827, #25344, #95711, #98803 ) ) ;
#40124 = CARTESIAN_POINT ( 'NONE',  ( 12.26069947439007457, -4.513567243280836472, -76.78238181720162459 ) ) ;
#40125 = ADVANCED_FACE ( 'NONE', ( #54270 ), #13290, .F. ) ;
#40126 = CARTESIAN_POINT ( 'NONE',  ( -83.48784346132804046, -52.72151958306880459, -16.05522805912662676 ) ) ;
#40127 = CARTESIAN_POINT ( 'NONE',  ( 0.000000000000000000, 47.00000000000000000, 56.99999999999999289 ) ) ;
#40128 = CARTESIAN_POINT ( 'NONE',  ( 47.33349330513379982, 1.593028355512270567E-15, 0.000000000000000000 ) ) ;
#40129 = ORIENTED_EDGE ( 'NONE', *, *, #59618, .F. ) ;
#40130 = CARTESIAN_POINT ( 'NONE',  ( 6.817720316173498496, 41.26212635516822758, -58.42655815993595780 ) ) ;
#40131 = ADVANCED_FACE ( 'NONE', ( #33625 ), #39720, .F. ) ;
#40132 = CARTESIAN_POINT ( 'NONE',  ( -17.01589776168603407, -1.734723475976807094E-15, -2.227375807157456755 ) ) ;
#40133 = DIRECTION ( 'NONE',  ( -1.000000000000000000, -1.224606353822377258E-16, -0.000000000000000000 ) ) ;
#40134 = CARTESIAN_POINT ( 'NONE',  ( 87.76937946118395928, -14.21045842199442433, -6.551255600857777139 ) ) ;
#40135 = CARTESIAN_POINT ( 'NONE',  ( -74.57516802433143255, -56.85267850989483662, 131.8985892516079446 ) ) ;
#40136 = VERTEX_POINT ( 'NONE', #83215 ) ;
#40137 = CARTESIAN_POINT ( 'NONE',  ( 1.384974311275041225, -30.00000000000000000, 37.00000000000000711 ) ) ;
#40138 = LINE ( 'NONE', #32072, #62459 ) ;
#40139 = CARTESIAN_POINT ( 'NONE',  ( 113.5159275335152671, -57.67115463665075481, 157.6643028401185518 ) ) ;
#40140 = CARTESIAN_POINT ( 'NONE',  ( 0.4037800551813744976, 7.199367570657607018, 0.5303295852573157720 ) ) ;
#40141 = LINE ( 'NONE', #13199, #9789 ) ;
#40142 = EDGE_LOOP ( 'NONE', ( #77496, #9343, #77012, #56240, #42963 ) ) ;
#40143 = DIRECTION ( 'NONE',  ( 0.000000000000000000, -0.000000000000000000, 1.000000000000000000 ) ) ;
#40144 = CARTESIAN_POINT ( 'NONE',  ( -12.49999999999999822, 9.372078614953675668, -27.37193630958070401 ) ) ;
#40145 = FACE_BOUND ( 'NONE', #83732, .T. ) ;
#40146 = CARTESIAN_POINT ( 'NONE',  ( -7.188101187500001821, -17.00000000204838457, -2.977408999572651371 ) ) ;
#40147 = CARTESIAN_POINT ( 'NONE',  ( 4.599534470798633201, -6.460478697736662390, -7.590212325761506840 ) ) ;
#40148 = VECTOR ( 'NONE', #56346, 1000.000000000000000 ) ;
#40149 = CARTESIAN_POINT ( 'NONE',  ( 6.289692432696784685, -1.240516797660047330E-13, -6.828989928337167115 ) ) ;
#40150 = CARTESIAN_POINT ( 'NONE',  ( 0.7831191144357741996, 34.98236821775393679, 27.51229094925169605 ) ) ;
#40151 = DIRECTION ( 'NONE',  ( -1.000000000000000000, 0.000000000000000000, 0.000000000000000000 ) ) ;
#40152 = CARTESIAN_POINT ( 'NONE',  ( -3.313708498984760276, -13.71875000409676737, -8.000000000000000000 ) ) ;
#40153 = ADVANCED_FACE ( 'NONE', ( #58954 ), #30891, .F. ) ;
#40154 = ORIENTED_EDGE ( 'NONE', *, *, #61572, .F. ) ;
#40155 = CARTESIAN_POINT ( 'NONE',  ( 43.32920196732025886, 484.9664025106548593, 4.870547201839677598 ) ) ;
#40156 =( GEOMETRIC_REPRESENTATION_CONTEXT ( 3 ) GLOBAL_UNCERTAINTY_ASSIGNED_CONTEXT ( ( #11397 ) ) GLOBAL_UNIT_ASSIGNED_CONTEXT ( ( #40329, #72693, #14980 ) ) REPRESENTATION_CONTEXT ( 'NONE', 'WORKASPACE' ) );
#40158 = CARTESIAN_POINT ( 'NONE',  ( 28.84991513505058691, -32.53357776115905864, 31.52034378082766608 ) ) ;
#40157 = CARTESIAN_POINT ( 'NONE',  ( 0.000000000000000000, 6.928203230275506108, 4.000000000000007105 ) ) ;
#40159 = CARTESIAN_POINT ( 'NONE',  ( 23.29992259251640263, 27.36384728240175690, -33.20617127781078892 ) ) ;
#40160 = ORIENTED_EDGE ( 'NONE', *, *, #68224, .F. ) ;
#40161 = EDGE_CURVE ( 'NONE', #67261, #71609, #17441, .T. ) ;
#40162 = ORIENTED_EDGE ( 'NONE', *, *, #31044, .F. ) ;
#40164 = CARTESIAN_POINT ( 'NONE',  ( 38.26671806398906739, 461.1046247403738789, 2.389135870405684869 ) ) ;
#40163 = FILL_AREA_STYLE_COLOUR ( '', #12354 ) ;
#40165 =( NAMED_UNIT ( * ) SI_UNIT ( $, .STERADIAN. ) SOLID_ANGLE_UNIT ( ) );
#40166 = CARTESIAN_POINT ( 'NONE',  ( -16.15504899495356028, 294.5642704844590298, -10.06111734223398635 ) ) ;
#40167 = CARTESIAN_POINT ( 'NONE',  ( 4.286263797015736595E-16, 3.500000000000000000, -3.500000000000000000 ) ) ;
#40168 = ADVANCED_FACE ( 'NONE', ( #658 ), #39185, .T. ) ;
#40169 = DIRECTION ( 'NONE',  ( -0.3108677890940723665, -0.06041750367988984322, -0.9485309393756504726 ) ) ;
#40170 = DIRECTION ( 'NONE',  ( 0.000000000000000000, 0.000000000000000000, -1.000000000000000000 ) ) ;
#40171 = ORIENTED_EDGE ( 'NONE', *, *, #75007, .T. ) ;
#40172 = CARTESIAN_POINT ( 'NONE',  ( 64.85336408992664303, -60.00000000000001421, -34.25061881763944172 ) ) ;
#40173 = CARTESIAN_POINT ( 'NONE',  ( 74.34313532025329607, -30.00000000000000000, 109.1728309539285817 ) ) ;
#40174 = CARTESIAN_POINT ( 'NONE',  ( 7.500000000000002665, -1.486698507076798625, -0.09861472150523793723 ) ) ;
#40175 = FACE_OUTER_BOUND ( 'NONE', #95262, .T. ) ;
#40176 = CARTESIAN_POINT ( 'NONE',  ( 46.83547786243074285, 13.71028427728499466, -15.22387951582032528 ) ) ;
#40177 = ORIENTED_EDGE ( 'NONE', *, *, #100725, .T. ) ;
#40178 = ORIENTED_EDGE ( 'NONE', *, *, #90377, .T. ) ;
#40179 = EDGE_LOOP ( 'NONE', ( #36355, #31111, #100206, #101943 ) ) ;
#40180 = CARTESIAN_POINT ( 'NONE',  ( -12.50000000000000000, -4.999999999999997335, -14.04024970282782547 ) ) ;
#40181 = SURFACE_STYLE_USAGE ( .BOTH. , #81162 ) ;
#40182 = CARTESIAN_POINT ( 'NONE',  ( 22.51458678521758827, 303.3309683193314186, 10.03994171628768406 ) ) ;
#40183 = CARTESIAN_POINT ( 'NONE',  ( -37.67361056029813682, 380.0437454810148097, 5.298401756046660083 ) ) ;
#40184 = CARTESIAN_POINT ( 'NONE',  ( -5.104025146928732326, -62.81240710122727222, 13.92109052487369603 ) ) ;
#40185 = CARTESIAN_POINT ( 'NONE',  ( -44.14731978900761789, 485.1890916993070277, 0.8858938469252318759 ) ) ;
#40186 = LINE ( 'NONE', #31082, #10555 ) ;
#40187 = ORIENTED_EDGE ( 'NONE', *, *, #104273, .T. ) ;
#40188 = CARTESIAN_POINT ( 'NONE',  ( 30.90685644053189662, 9.526079354490885720, 40.57200395206826471 ) ) ;
#40189 = ORIENTED_EDGE ( 'NONE', *, *, #44856, .T. ) ;
#40190 = CYLINDRICAL_SURFACE ( 'NONE', #74272, 4.000000000000000888 ) ;
#40191 = CARTESIAN_POINT ( 'NONE',  ( -27.10511071441183262, 36.88665068479722464, 7.556984339686156460 ) ) ;
#40192 = CARTESIAN_POINT ( 'NONE',  ( -40.02990647470183205, 485.1981161833896863, -4.348266463184057962 ) ) ;
#40193 = VECTOR ( 'NONE', #20728, 1000.000000000000000 ) ;
#40194 = CARTESIAN_POINT ( 'NONE',  ( -4.174453427199569688, -59.99999999999997868, 33.87834425268652438 ) ) ;
#40195 = CARTESIAN_POINT ( 'NONE',  ( 64.58841386258137618, -36.00601803332205719, 83.18175225845169507 ) ) ;
#40196 = B_SPLINE_CURVE_WITH_KNOTS ( 'NONE', 3,
 ( #96016, #38332, #29717, #22143 ),
 .UNSPECIFIED., .F., .F.,
 ( 4, 4 ),
 ( 4.336808689942017736E-18, 0.001327912649053314235 ),
 .UNSPECIFIED. ) ;
#40197 = AXIS2_PLACEMENT_3D ( 'NONE', #53908, #28093, #68527 ) ;
#40198 = ORIENTED_EDGE ( 'NONE', *, *, #97486, .F. ) ;
#40199 = DIRECTION ( 'NONE',  ( 1.000000000000000000, 0.000000000000000000, 0.000000000000000000 ) ) ;
#40200 = CARTESIAN_POINT ( 'NONE',  ( -5.763828452502798072, 12.46312952775077676, 3.972702736835262982 ) ) ;
#40201 = CARTESIAN_POINT ( 'NONE',  ( -36.37294538904226471, -57.67119865010090507, -42.13310955380372747 ) ) ;
#40202 = EDGE_CURVE ( 'NONE', #87625, #68880, #99377, .T. ) ;
#40203 = VERTEX_POINT ( 'NONE', #90790 ) ;
#40204 = SURFACE_STYLE_USAGE ( .BOTH. , #74156 ) ;
#40205 = SURFACE_STYLE_USAGE ( .BOTH. , #97908 ) ;
#40206 = CIRCLE ( 'NONE', #52211, 4.000000000000000888 ) ;
#40207 = EDGE_CURVE ( 'NONE', #95054, #56223, #77448, .T. ) ;
#40208 = CARTESIAN_POINT ( 'NONE',  ( -35.62683129835190954, 491.6879615318166543, 12.48649695628544976 ) ) ;
#40209 = ADVANCED_FACE ( 'NONE', ( #102595 ), #61231, .T. ) ;
#40210 = CARTESIAN_POINT ( 'NONE',  ( 7.999999999999998224, -29.28125000409677270, 3.313708498984766493 ) ) ;
#40211 = CARTESIAN_POINT ( 'NONE',  ( 9.948181520647876752, 246.1310719723961995, 1.049088206181493677 ) ) ;
#40212 = EDGE_CURVE ( 'NONE', #62903, #102355, #6767, .T. ) ;
#40213 = DIRECTION ( 'NONE',  ( -0.000000000000000000, -0.000000000000000000, -1.000000000000000000 ) ) ;
#40214 = CARTESIAN_POINT ( 'NONE',  ( 9.843481099141458301, 33.59204556153386534, -1.779148000612201352 ) ) ;
#40215 = B_SPLINE_CURVE_WITH_KNOTS ( 'NONE', 3,
 ( #98520, #24666, #23607, #39779, #24148, #65634, #90440, #105036, #56992, #16549, #49434, #56458, #48373, #81266, #8451, #74245 ),
 .UNSPECIFIED., .F., .F.,
 ( 4, 2, 2, 2, 2, 2, 2, 4 ),
 ( 0.000000000000000000, 0.002612557234031565555, 0.003918835851047347031, 0.005225114468063129375, 0.005878253776571019246, 0.006531393085078909984, 0.007837671702094688858, 0.01045022893612624661 ),
 .UNSPECIFIED. ) ;
#40216 = LINE ( 'NONE', #98448, #22370 ) ;
#40217 = ADVANCED_FACE ( 'NONE', ( #77792, #76710, #28214, #101532, #35776 ), #48082, .T. ) ;
#40218 = CIRCLE ( 'NONE', #100500, 4.172000000000001485 ) ;
#40219 = CARTESIAN_POINT ( 'NONE',  ( 13.26813409727140680, 304.5542536273018186, 8.873748392553073572 ) ) ;
#40220 = EDGE_LOOP ( 'NONE', ( #100654, #12715, #41242, #19772, #10590 ) ) ;
#40221 = EDGE_CURVE ( 'NONE', #45098, #54191, #94310, .T. ) ;
#40222 = CARTESIAN_POINT ( 'NONE',  ( -8.000000000000001776, -10.15624999999999112, 3.313708498984759387 ) ) ;
#40223 = CARTESIAN_POINT ( 'NONE',  ( 2.841782347625613436, -59.99999999999999289, 39.63376178591555998 ) ) ;
#40224 = MECHANICAL_DESIGN_GEOMETRIC_PRESENTATION_REPRESENTATION (  '', ( #7476 ), #85053 ) ;
#40225 = CARTESIAN_POINT ( 'NONE',  ( -92.63040736140382592, -29.99999999999999645, 191.0343855628001393 ) ) ;
#40226 = AXIS2_PLACEMENT_3D ( 'NONE', #17562, #66089, #42345 ) ;
#40227 = AXIS2_PLACEMENT_3D ( 'NONE', #98689, #37197, #52271 ) ;
#40228 = DIRECTION ( 'NONE',  ( 0.000000000000000000, 1.000000000000000000, 0.000000000000000000 ) ) ;
#40229 = CARTESIAN_POINT ( 'NONE',  ( 51.98618296257861715, -57.67674160844479303, 82.65666769069098052 ) ) ;
#40231 = CARTESIAN_POINT ( 'NONE',  ( -9.999999999999994671, 7.499999999999983125, 0.3301729510373770382 ) ) ;
#40230 = LINE ( 'NONE', #98974, #77638 ) ;
#40232 = CARTESIAN_POINT ( 'NONE',  ( 3.308827153974509994, -21.42733763530625168, -38.54996605793198938 ) ) ;
#40233 = CARTESIAN_POINT ( 'NONE',  ( 4.898587196589412829E-16, -15.12499999999999289, -8.000000000000000000 ) ) ;
#40234 = CARTESIAN_POINT ( 'NONE',  ( -12.68889540457527154, -60.00000000000001421, 39.70531046957451338 ) ) ;
#40235 = B_SPLINE_CURVE_WITH_KNOTS ( 'NONE', 3,
 ( #26087, #92348, #50818, #60550, #43809, #28205 ),
 .UNSPECIFIED., .F., .F.,
 ( 4, 2, 4 ),
 ( -5.145455527292617106E-06, 0.0004153350442917344717, 0.0008358155441107594386 ),
 .UNSPECIFIED. ) ;
#40236 = CARTESIAN_POINT ( 'NONE',  ( 12.02599986777602048, 10.59850526615580257, 9.713964925274206408 ) ) ;
#40237 = CARTESIAN_POINT ( 'NONE',  ( 6.308797461351612235, 53.41353044709899933, 8.024790098550512951 ) ) ;
#40238 = CARTESIAN_POINT ( 'NONE',  ( -86.31431195955053681, -57.42698322520472232, 193.3924140938322864 ) ) ;
#40239 = EDGE_LOOP ( 'NONE', ( #39337, #1283, #103721, #46133 ) ) ;
#40240 = CARTESIAN_POINT ( 'NONE',  ( 17.50000000000003908, 51.99999999999945288, 59.71562975592906497 ) ) ;
#40241 = CARTESIAN_POINT ( 'NONE',  ( 9.795930887471511639, -12.69766919046054277, 16.99563166591020646 ) ) ;
#40242 = CARTESIAN_POINT ( 'NONE',  ( -6.015098659326455710, -25.54938308050677520, 28.13832966994452534 ) ) ;
#40243 = CYLINDRICAL_SURFACE ( 'NONE', #77340, 4.000000000000000000 ) ;
#40245 = CARTESIAN_POINT ( 'NONE',  ( 40.09057539293721106, 460.7411201710881414, 2.126307971703979671 ) ) ;
#40244 = FACE_OUTER_BOUND ( 'NONE', #1508, .T. ) ;
#40246 = ORIENTED_EDGE ( 'NONE', *, *, #51061, .T. ) ;
#40248 = FACE_OUTER_BOUND ( 'NONE', #82886, .T. ) ;
#40247 = CIRCLE ( 'NONE', #17863, 4.000000000000001776 ) ;
#40249 = B_SPLINE_CURVE_WITH_KNOTS ( 'NONE', 3,
 ( #64486, #81686, #24049, #33717, #40716, #57417, #106509, #65537, #23509, #56353, #41784, #48269, #66594, #98424, #82776, #81170, #74140, #89289, #25098, #88750, #15383, #24575, #225, #47739, #16444, #49328 ),
 .UNSPECIFIED., .F., .F.,
 ( 4, 2, 2, 2, 2, 2, 2, 2, 2, 2, 2, 2, 4 ),
 ( 0.002887119676744016351, 0.003139154421792429879, 0.003391189166840843407, 0.003895258656937666125, 0.004399328147034487976, 0.004903397637131310695, 0.005155432382179719018, 0.005407467127228127342, 0.005659501872276535665, 0.005911536617324943121, 0.006415606107421763238, 0.006667640852470176765, 0.006919675597518590293 ),
 .UNSPECIFIED. ) ;
#40250 = CARTESIAN_POINT ( 'NONE',  ( -6.689814467817122967, -4.999999999994103383, -16.20004731218735827 ) ) ;
#40251 = CARTESIAN_POINT ( 'NONE',  ( 15.54299285489016391, 34.77154309520251019, 23.41290371719734509 ) ) ;
#40252 = CARTESIAN_POINT ( 'NONE',  ( 33.10504549936585050, 299.5985994039988327, -8.944502871241384767 ) ) ;
#40253 = DIRECTION ( 'NONE',  ( 0.000000000000000000, -1.000000000000000000, 0.000000000000000000 ) ) ;
#40254 = EDGE_CURVE ( 'NONE', #34982, #74683, #63605, .T. ) ;
#40255 = DIRECTION ( 'NONE',  ( 0.000000000000000000, 0.000000000000000000, 1.000000000000000000 ) ) ;
#40256 = CARTESIAN_POINT ( 'NONE',  ( 69.49330227205123833, -59.99999999999997868, 138.6641764573228102 ) ) ;
#40257 = CARTESIAN_POINT ( 'NONE',  ( -35.59667163540026280, 463.9592197885497171, -0.04846191499040426731 ) ) ;
#40258 = ORIENTED_EDGE ( 'NONE', *, *, #78693, .F. ) ;
#40259 = CARTESIAN_POINT ( 'NONE',  ( -6.274085929497640102, -30.00000000000001066, 4.398938879594368245 ) ) ;
#40260 = DIRECTION ( 'NONE',  ( 0.000000000000000000, 0.000000000000000000, -1.000000000000000000 ) ) ;
#40261 = VECTOR ( 'NONE', #63208, 1000.000000000000000 ) ;
#40263 = CARTESIAN_POINT ( 'NONE',  ( -36.14207491790881477, 485.3942915881596605, -3.424055767583114029 ) ) ;
#40262 = CARTESIAN_POINT ( 'NONE',  ( 20.43634719630433594, -14.21045842199429998, 34.90381869870211062 ) ) ;
#40264 = CARTESIAN_POINT ( 'NONE',  ( 35.11650669486618170, 1.474610560812782335E-15, 0.000000000000000000 ) ) ;
#40265 = CARTESIAN_POINT ( 'NONE',  ( -4.973317752991481377, -3.468598768254719911, 102.2736751349651456 ) ) ;
#40266 = ORIENTED_EDGE ( 'NONE', *, *, #20083, .F. ) ;
#40267 = CONICAL_SURFACE ( 'NONE', #71222, 45.10524579772351217, 0.3972631705159501148 ) ;
#40268 = CARTESIAN_POINT ( 'NONE',  ( -25.70012971588764117, 306.8024630045113099, 10.60968151228726519 ) ) ;
#40269 = AXIS2_PLACEMENT_3D ( 'NONE', #15329, #90284, #66005 ) ;
#40270 = ORIENTED_EDGE ( 'NONE', *, *, #26321, .F. ) ;
#40271 = CYLINDRICAL_SURFACE ( 'NONE', #89671, 1.250000000000001110 ) ;
#40272 = ADVANCED_FACE ( 'NONE', ( #11975 ), #68094, .F. ) ;
#40273 = CARTESIAN_POINT ( 'NONE',  ( 31.02195986096099745, 439.2860129589981284, 22.60718686867361527 ) ) ;
#40274 = ORIENTED_EDGE ( 'NONE', *, *, #50800, .T. ) ;
#40275 = CARTESIAN_POINT ( 'NONE',  ( 58.90678327788049273, 50.00000000002003731, -28.11551192221532247 ) ) ;
#40276 = CARTESIAN_POINT ( 'NONE',  ( 5.000000000000000000, -12.33523449218792223, 10.71643274013084657 ) ) ;
#40277 = CARTESIAN_POINT ( 'NONE',  ( -23.40723339434643435, -60.00000000000986233, 43.19923654131418544 ) ) ;
#40278 = CARTESIAN_POINT ( 'NONE',  ( 44.06229749045533595, 485.7005620094865321, 3.983350637705970865 ) ) ;
#40279 = CARTESIAN_POINT ( 'NONE',  ( 42.28582005287888279, -60.00000000000002132, 55.60554140212523322 ) ) ;
#40280 = CARTESIAN_POINT ( 'NONE',  ( 3.400000000000000355, 0.000000000000000000, -3.012075477074183105 ) ) ;
#40282 = CARTESIAN_POINT ( 'NONE',  ( 17.15269105894165236, -60.35792664080034342, 34.22063819385883221 ) ) ;
#40281 = CARTESIAN_POINT ( 'NONE',  ( -114.3490076612200568, -60.00000000000000000, 164.2604626692111367 ) ) ;
#40284 = DIRECTION ( 'NONE',  ( 0.000000000000000000, 1.000000000000000000, 0.000000000000000000 ) ) ;
#40283 = UNCERTAINTY_MEASURE_WITH_UNIT (LENGTH_MEASURE( 1.000000000000000082E-05 ), #53360, 'distance_accuracy_value', 'NONE');
#40285 = DIRECTION ( 'NONE',  ( 0.000000000000000000, -0.000000000000000000, 1.000000000000000000 ) ) ;
#40286 = EDGE_CURVE ( 'NONE', #30532, #59127, #4424, .T. ) ;
#40287 = CARTESIAN_POINT ( 'NONE',  ( -44.33452073850874342, -60.25607191441693544, 48.29083679502918613 ) ) ;
#40288 = CARTESIAN_POINT ( 'NONE',  ( -4.491425985185824032, 18.64284798592936809, 38.16738163467832123 ) ) ;
#40289 = VERTEX_POINT ( 'NONE', #62159 ) ;
#40290 =( NAMED_UNIT ( * ) PLANE_ANGLE_UNIT ( ) SI_UNIT ( $, .RADIAN. ) );
#40291 = CARTESIAN_POINT ( 'NONE',  ( 0.000000000000000000, -1.500000000000000000, 15.43455230191221261 ) ) ;
#40292 = CARTESIAN_POINT ( 'NONE',  ( 6.575925811255157072, -3.850887307289496686, 6.669932470447527351 ) ) ;
#40293 = DIRECTION ( 'NONE',  ( 0.000000000000000000, 0.000000000000000000, -1.000000000000000000 ) ) ;
#40294 = ADVANCED_FACE ( 'NONE', ( #15161 ), #1578, .T. ) ;
#40295 = DIRECTION ( 'NONE',  ( -1.000000000000000000, -1.224606353822377258E-16, -0.000000000000000000 ) ) ;
#40296 = CARTESIAN_POINT ( 'NONE',  ( 35.74363442581862671, 380.1068966271811860, 4.951945592532029927 ) ) ;
#40297 = ORIENTED_EDGE ( 'NONE', *, *, #46484, .T. ) ;
#40298 = DIRECTION ( 'NONE',  ( -1.000000000000000000, -1.224606353822377258E-16, -0.000000000000000000 ) ) ;
#40299 = ORIENTED_EDGE ( 'NONE', *, *, #77663, .T. ) ;
#40300 = CARTESIAN_POINT ( 'NONE',  ( 97.56484421644714189, -30.00000000002681944, 199.7415702076955597 ) ) ;
#40301 = CARTESIAN_POINT ( 'NONE',  ( 54.52222222222221859, 6.915964383211875250E-15, 0.000000000000000000 ) ) ;
#40302 = CARTESIAN_POINT ( 'NONE',  ( 5.675015017080928814, 41.92512468593253772, -59.11382255160837929 ) ) ;
#40303 = FACE_OUTER_BOUND ( 'NONE', #8013, .T. ) ;
#40304 = CARTESIAN_POINT ( 'NONE',  ( 97.90508973058878439, -30.00000000000000711, 136.8651816328178086 ) ) ;
#40305 = MECHANICAL_DESIGN_GEOMETRIC_PRESENTATION_REPRESENTATION (  '', ( #105738 ), #69572 ) ;
#40306 = DIRECTION ( 'NONE',  ( 0.000000000000000000, 0.000000000000000000, 1.000000000000000000 ) ) ;
#40307 = EDGE_LOOP ( 'NONE', ( #20435, #101760, #106414, #49531 ) ) ;
#40308 = PRESENTATION_LAYER_ASSIGNMENT (  '', '', ( #50592 ) ) ;
#40309 = CONICAL_SURFACE ( 'NONE', #5810, 4.172000000000009479, 0.9599310885968813656 ) ;
#40310 = ORIENTED_EDGE ( 'NONE', *, *, #10494, .T. ) ;
#40311 = VERTEX_POINT ( 'NONE', #22231 ) ;
#40312 = CARTESIAN_POINT ( 'NONE',  ( -4.000000000000000000, 17.85270131633358304, 5.744562646538042827 ) ) ;
#40313 = CARTESIAN_POINT ( 'NONE',  ( -6.999999999999999112, -14.05766640829038394, -5.232782735144285269 ) ) ;
#40314 = DIRECTION ( 'NONE',  ( 0.000000000000000000, 1.000000000000000000, 0.000000000000000000 ) ) ;
#40315 = VERTEX_POINT ( 'NONE', #31389 ) ;
#40316 = CARTESIAN_POINT ( 'NONE',  ( 9.843481099141454749, 108.5920455615338653, -1.779148000612198022 ) ) ;
#40317 = ORIENTED_EDGE ( 'NONE', *, *, #5278, .T. ) ;
#40318 = CARTESIAN_POINT ( 'NONE',  ( 48.02835407290544367, 14.94086294439726892, 16.85535821593427386 ) ) ;
#40319 = CARTESIAN_POINT ( 'NONE',  ( 85.17744768472425676, -38.69024637654926835, 198.5893117286057361 ) ) ;
#40320 = CARTESIAN_POINT ( 'NONE',  ( 12.30282354285915680, 5.677685097715426288, 8.440510770982715627 ) ) ;
#40321 = CARTESIAN_POINT ( 'NONE',  ( 82.21598800793653083, -38.00000000000003553, 160.2028133164328381 ) ) ;
#40322 = CARTESIAN_POINT ( 'NONE',  ( 38.65571709296854408, 312.2086733158335505, 6.098135005489119465 ) ) ;
#40323 = SURFACE_STYLE_FILL_AREA ( #352 ) ;
#40324 = DIRECTION ( 'NONE',  ( 0.000000000000000000, 0.000000000000000000, 1.000000000000000000 ) ) ;
#40325 = CARTESIAN_POINT ( 'NONE',  ( -27.85246203510405394, 34.47333191833108401, -7.792023951491530376 ) ) ;
#40326 = CARTESIAN_POINT ( 'NONE',  ( -5.374793246923619705, -47.77528324145959715, 104.0614974883207395 ) ) ;
#40327 = DIRECTION ( 'NONE',  ( 0.000000000000000000, 0.000000000000000000, 1.000000000000000000 ) ) ;
#40328 = AXIS2_PLACEMENT_3D ( 'NONE', #65629, #99572, #74762 ) ;
#40329 =( LENGTH_UNIT ( ) NAMED_UNIT ( * ) SI_UNIT ( .MILLI., .METRE. ) );
#40330 = VERTEX_POINT ( 'NONE', #31903 ) ;
#40331 = CARTESIAN_POINT ( 'NONE',  ( -42.73089261237369385, 435.7309723475636360, 18.11242468272465089 ) ) ;
#40333 = CARTESIAN_POINT ( 'NONE',  ( -30.76131805048738954, 299.0178075277323160, 10.86737662268762605 ) ) ;
#40332 = CARTESIAN_POINT ( 'NONE',  ( 0.000000000000000000, 0.000000000000000000, 4.000000000000000000 ) ) ;
#40334 = DIRECTION ( 'NONE',  ( 1.000000000000000000, 1.224606353822377258E-16, 0.000000000000000000 ) ) ;
#40335 = EDGE_CURVE ( 'NONE', #26696, #61668, #44661, .T. ) ;
#40336 = FILL_AREA_STYLE ('',( #57559 ) ) ;
#40337 = CARTESIAN_POINT ( 'NONE',  ( 5.656854249492378806, -17.18749999999999289, 5.656854249492381470 ) ) ;
#40338 = CARTESIAN_POINT ( 'NONE',  ( -20.04862318086297890, -25.72039272919216657, 36.80507196085346067 ) ) ;
#40339 = EDGE_CURVE ( 'NONE', #36732, #88469, #104706, .T. ) ;
#40340 = DIRECTION ( 'NONE',  ( 8.355988613032100413E-17, 0.7310552682428690385, -0.6823182503600110360 ) ) ;
#40341 = VECTOR ( 'NONE', #34925, 1000.000000000000000 ) ;
#40342 = ORIENTED_EDGE ( 'NONE', *, *, #82546, .F. ) ;
#40343 = CARTESIAN_POINT ( 'NONE',  ( 86.39964040925956112, -17.50171996465882174, 178.3850458645602828 ) ) ;
#40344 = CARTESIAN_POINT ( 'NONE',  ( 0.000000000000000000, -20.00000000000001776, -9.000000000000007105 ) ) ;
#40345 = FACE_OUTER_BOUND ( 'NONE', #52076, .T. ) ;
#40346 = ORIENTED_EDGE ( 'NONE', *, *, #8152, .T. ) ;
#40347 = CARTESIAN_POINT ( 'NONE',  ( 88.75764767935135069, -57.66845035223018101, -23.73888392983841555 ) ) ;
#40348 = CARTESIAN_POINT ( 'NONE',  ( 9.833493305133805151, 1.593028355512270962E-15, 0.000000000000000000 ) ) ;
#40349 = CARTESIAN_POINT ( 'NONE',  ( 36.84999999999999432, 1.533819458162526451E-15, 0.000000000000000000 ) ) ;
#40350 = EDGE_CURVE ( 'NONE', #64595, #15159, #18029, .T. ) ;
#40351 = CARTESIAN_POINT ( 'NONE',  ( 28.58355031030010096, 11.06033896639477732, 41.46143022647122933 ) ) ;
#40352 = EDGE_CURVE ( 'NONE', #77823, #51686, #78835, .T. ) ;
#40353 = CARTESIAN_POINT ( 'NONE',  ( 28.62002530331290018, 18.65065574497674206, 40.19565755993141210 ) ) ;
#40354 = CARTESIAN_POINT ( 'NONE',  ( -7.137815226409941260, -3.000000000000000000, 4.175893272574811910 ) ) ;
#40355 = CARTESIAN_POINT ( 'NONE',  ( 0.000000000000000000, 47.00000000000000000, 0.000000000000000000 ) ) ;
#40356 = CARTESIAN_POINT ( 'NONE',  ( -11.51709745524291684, 12.46548236075430260, 10.00164875338921178 ) ) ;
#40357 = CARTESIAN_POINT ( 'NONE',  ( -4.999999999999993783, -4.000000000000003553, 102.2532056551910387 ) ) ;
#40358 = CARTESIAN_POINT ( 'NONE',  ( -28.56372199056537298, 18.54333498561203442, 40.29094744152372698 ) ) ;
#40359 = CARTESIAN_POINT ( 'NONE',  ( -7.898269865231991815, -11.02838903529593928, -0.02849990174191728218 ) ) ;
#40360 = CARTESIAN_POINT ( 'NONE',  ( -28.35805447588125361, 36.30513988744195331, -8.950293267375700523 ) ) ;
#40361 = CARTESIAN_POINT ( 'NONE',  ( 61.11682663846713837, 4.000000000000013323, 0.000000000000000000 ) ) ;
#40362 = FACE_OUTER_BOUND ( 'NONE', #68541, .T. ) ;
#40363 = CARTESIAN_POINT ( 'NONE',  ( -100.6662216249829243, -38.00000000000002132, 189.2678359082001123 ) ) ;
#40364 = TOROIDAL_SURFACE ( 'NONE', #38634, 7.999999999999998224, 2.000000000000000000 ) ;
#40365 = EDGE_LOOP ( 'NONE', ( #91453, #93362, #105003, #82548 ) ) ;
#40366 = CARTESIAN_POINT ( 'NONE',  ( -5.385673916453011856, 3.157894736842102645, 14.66382285868951030 ) ) ;
#40367 =( NAMED_UNIT ( * ) PLANE_ANGLE_UNIT ( ) SI_UNIT ( $, .RADIAN. ) );
#40368 = CARTESIAN_POINT ( 'NONE',  ( 0.000000000000000000, -99.99999999999997158, 0.000000000000000000 ) ) ;
#40369 = VECTOR ( 'NONE', #11409, 1000.000000000000000 ) ;
#40371 = CARTESIAN_POINT ( 'NONE',  ( -44.60760376941820482, -47.40887594010209938, -30.95105337255921185 ) ) ;
#40370 = FACE_OUTER_BOUND ( 'NONE', #10459, .T. ) ;
#40372 = AXIS2_PLACEMENT_3D ( 'NONE', #20789, #46593, #54132 ) ;
#40373 = ORIENTED_EDGE ( 'NONE', *, *, #50660, .F. ) ;
#40374 = B_SPLINE_CURVE_WITH_KNOTS ( 'NONE', 3,
 ( #83741, #49247, #76185, #82152, #35233, #17975, #74057, #66509, #57870, #27157, #92903, #68099, #60045, #75112, #8265, #145, #33112, #99932 ),
 .UNSPECIFIED., .F., .F.,
 ( 4, 2, 2, 2, 2, 2, 2, 2, 4 ),
 ( 0.004289890562715018008, 0.005298017633127179507, 0.005550049400730218581, 0.005802081168333258522, 0.006306144703539339272, 0.006810208238745420889, 0.007314271773951502506, 0.007818335309157584123, 0.008322398844363665740 ),
 .UNSPECIFIED. ) ;
#40375 = ORIENTED_EDGE ( 'NONE', *, *, #64591, .T. ) ;
#40376 = CARTESIAN_POINT ( 'NONE',  ( -42.08762648273019380, 487.0030674539066808, 9.106351919860241395 ) ) ;
#40377 = ADVANCED_FACE ( 'NONE', ( #22761 ), #27442, .T. ) ;
#40378 = CARTESIAN_POINT ( 'NONE',  ( 10.36885343410368243, 43.24044830979637766, -15.40779740156171940 ) ) ;
#40379 = DIRECTION ( 'NONE',  ( 0.000000000000000000, -1.000000000000000000, 0.000000000000000000 ) ) ;
#40380 = CARTESIAN_POINT ( 'NONE',  ( -79.45792651602657486, -60.00000000000000711, -28.32091169615220494 ) ) ;
#40381 = ORIENTED_EDGE ( 'NONE', *, *, #65093, .F. ) ;
#40382 = FACE_OUTER_BOUND ( 'NONE', #89691, .T. ) ;
#40383 = FACE_OUTER_BOUND ( 'NONE', #106508, .T. ) ;
#40384 = CARTESIAN_POINT ( 'NONE',  ( 95.67817354102299987, -37.71398327266919637, 193.0022183632935082 ) ) ;
#40386 = CARTESIAN_POINT ( 'NONE',  ( -47.14735620107897773, 13.37129584416856964, 14.71343070694194921 ) ) ;
#40385 = FILL_AREA_STYLE_COLOUR ( '', #45732 ) ;
#40387 = CARTESIAN_POINT ( 'NONE',  ( -82.60449197779891506, -36.02481693259124995, 160.6711189363873302 ) ) ;
#40388 = ORIENTED_EDGE ( 'NONE', *, *, #75417, .T. ) ;
#40389 = ORIENTED_EDGE ( 'NONE', *, *, #93604, .F. ) ;
#40390 = ORIENTED_EDGE ( 'NONE', *, *, #42885, .F. ) ;
#40391 = CARTESIAN_POINT ( 'NONE',  ( 9.479859806995825977, -5.000000000000000000, -13.37835090744263944 ) ) ;
#40392 = ADVANCED_FACE ( 'NONE', ( #14614 ), #105761, .T. ) ;
#40393 = CARTESIAN_POINT ( 'NONE',  ( -5.000000000000000000, -14.73708290047480496, 12.39211607762596401 ) ) ;
#40394 = DIRECTION ( 'NONE',  ( 0.000000000000000000, 0.000000000000000000, 1.000000000000000000 ) ) ;
#40395 = EDGE_LOOP ( 'NONE', ( #74549, #39356, #103452, #18272, #85413, #52237 ) ) ;
#40396 = CIRCLE ( 'NONE', #7665, 8.000000000000000000 ) ;
#40397 = DIRECTION ( 'NONE',  ( 0.000000000000000000, 1.000000000000000000, 0.000000000000000000 ) ) ;
#40398 = CARTESIAN_POINT ( 'NONE',  ( 6.499999999999999112, -1.431146867680865853E-14, -5.592027715088708106 ) ) ;
#40399 = CARTESIAN_POINT ( 'NONE',  ( 37.38561277374697056, 5.000000000000004441, 6.123233995736770227E-16 ) ) ;
#40400 = CARTESIAN_POINT ( 'NONE',  ( -97.80441453946778552, -57.62343821539597855, 204.4198989768915453 ) ) ;
#40401 = CARTESIAN_POINT ( 'NONE',  ( 4.401442555609581635E-16, -33.78125000204838813, -7.188101187500000044 ) ) ;
#40402 = LINE ( 'NONE', #72757, #13419 ) ;
#40403 = CARTESIAN_POINT ( 'NONE',  ( 43.58349330513380693, -4.000000000000000000, 4.898587196589415787E-16 ) ) ;
#40404 = CARTESIAN_POINT ( 'NONE',  ( 1.544939622598899831, 15.00000000000000000, -9.999999999999998224 ) ) ;
#40405 = CARTESIAN_POINT ( 'NONE',  ( 55.21462903151665813, -59.99999999999998579, -39.23961370773703550 ) ) ;
#40406 = CARTESIAN_POINT ( 'NONE',  ( -1.309564884278361513E-05, -14.21045842199434972, 34.36840973699906243 ) ) ;
#40407 = CARTESIAN_POINT ( 'NONE',  ( -54.43306722364180672, -25.62724657511986237, 53.68909144041590054 ) ) ;
#40408 = CARTESIAN_POINT ( 'NONE',  ( 43.00000000000000000, 487.9285348210859752, 8.903916466042430145 ) ) ;
#40409 = CIRCLE ( 'NONE', #92075, 4.172000000000001485 ) ;
#40410 = EDGE_LOOP ( 'NONE', ( #94294, #94204 ) ) ;
#40411 = CARTESIAN_POINT ( 'NONE',  ( -99.66131679920104602, -45.25319430717961211, 192.8901977128174963 ) ) ;
#40412 =( GEOMETRIC_REPRESENTATION_CONTEXT ( 3 ) GLOBAL_UNCERTAINTY_ASSIGNED_CONTEXT ( ( #103136 ) ) GLOBAL_UNIT_ASSIGNED_CONTEXT ( ( #25715, #49929, #74728 ) ) REPRESENTATION_CONTEXT ( 'NONE', 'WORKASPACE' ) );
#40413 = AXIS2_PLACEMENT_3D ( 'NONE', #90428, #17614, #50477 ) ;
#40414 = DIRECTION ( 'NONE',  ( -1.000000000000000000, -1.224606353822377258E-16, -0.000000000000000000 ) ) ;
#40415 = EDGE_CURVE ( 'NONE', #79740, #49120, #104948, .T. ) ;
#40416 = ORIENTED_EDGE ( 'NONE', *, *, #69682, .T. ) ;
#40417 = CARTESIAN_POINT ( 'NONE',  ( -17.89483185117538255, 43.18956583916507697, 5.468282401795739212 ) ) ;
#40418 = CARTESIAN_POINT ( 'NONE',  ( 90.50996382122711736, -38.40237687013089385, -14.56173365871752168 ) ) ;
#40419 = CARTESIAN_POINT ( 'NONE',  ( -23.21751746555280249, 28.11705169068991239, -30.70617127781034839 ) ) ;
#40420 = DIRECTION ( 'NONE',  ( -1.000000000000000000, -1.224606353822377258E-16, -0.000000000000000000 ) ) ;
#40421 = CARTESIAN_POINT ( 'NONE',  ( -4.061792834527171436, 294.8078979827683384, 9.927667182094811693 ) ) ;
#40422 = AXIS2_PLACEMENT_3D ( 'NONE', #59197, #25809, #106656 ) ;
#40423 = CARTESIAN_POINT ( 'NONE',  ( -8.559508646656370345, 51.55638410492942114, 4.031152949374564365 ) ) ;
#40424 = CARTESIAN_POINT ( 'NONE',  ( 78.31067388355049275, -30.00000000000000000, 126.2693683704580394 ) ) ;
#40425 =( BOUNDED_CURVE ( )  B_SPLINE_CURVE ( 2, ( #32623, #99976, #65496 ),
 .UNSPECIFIED., .F., .F. ) 
 B_SPLINE_CURVE_WITH_KNOTS ( ( 3, 3 ),
 ( 0.000000000000000000, 1.000000000000000000 ),
 .UNSPECIFIED. ) 
 CURVE ( )  GEOMETRIC_REPRESENTATION_ITEM ( )  RATIONAL_B_SPLINE_CURVE ( ( 1.000000000000000000, 1.857142857142858317, 1.000000000000000000 ) ) 
 REPRESENTATION_ITEM ( '' )  );
#40426 = EDGE_CURVE ( 'NONE', #27178, #14501, #30313, .T. ) ;
#40427 = CARTESIAN_POINT ( 'NONE',  ( 37.17693862423350737, 491.8028371848114944, 12.56217450279973846 ) ) ;
#40428 = CARTESIAN_POINT ( 'NONE',  ( -28.43271360265415382, 12.18326821505116619, 40.99299228862962252 ) ) ;
#40429 = CARTESIAN_POINT ( 'NONE',  ( -34.04714008975742701, 484.1152113529151961, 1.016147467615854172 ) ) ;
#40430 = VERTEX_POINT ( 'NONE', #80416 ) ;
#40431 = ORIENTED_EDGE ( 'NONE', *, *, #74666, .F. ) ;
#40432 = CARTESIAN_POINT ( 'NONE',  ( 49.14122930290414359, -49.90062465560988159, 52.73429724734012325 ) ) ;
#40433 = CARTESIAN_POINT ( 'NONE',  ( 6.943035990376877464, 41.50417910381163011, -58.81491866537869129 ) ) ;
#40434 = CARTESIAN_POINT ( 'NONE',  ( 9.181445049447248152, 51.37268433381575505, 3.877508282323112621 ) ) ;
#40435 = EDGE_LOOP ( 'NONE', ( #5, #90053, #77535, #18591, #25908, #79245 ) ) ;
#40436 = CARTESIAN_POINT ( 'NONE',  ( -90.91152594127831321, -38.34737926575705558, 3.482876280662382307 ) ) ;
#40437 = ORIENTED_EDGE ( 'NONE', *, *, #91657, .F. ) ;
#40438 = CARTESIAN_POINT ( 'NONE',  ( 28.23197554257926711, 34.17505064455689023, -9.354563056550400546 ) ) ;
#40439 = CARTESIAN_POINT ( 'NONE',  ( 102.8148430110912699, -38.35590780206664618, 104.8312485263550116 ) ) ;
#40440 = CARTESIAN_POINT ( 'NONE',  ( 11.42547868101649655, 20.37551526749874142, -8.168836983366716709 ) ) ;
#40441 = CARTESIAN_POINT ( 'NONE',  ( 30.00000000000000355, 461.8163627757391509, 11.11111419091022512 ) ) ;
#40442 = CARTESIAN_POINT ( 'NONE',  ( 102.4777983945700299, -52.71700600495957190, 139.6461353976963835 ) ) ;
#40443 =( LENGTH_UNIT ( ) NAMED_UNIT ( * ) SI_UNIT ( .MILLI., .METRE. ) );
#40444 = CARTESIAN_POINT ( 'NONE',  ( 22.37441460685049677, 28.20471216883544230, 31.02949312230836298 ) ) ;
#40445 = CARTESIAN_POINT ( 'NONE',  ( -30.50452656062791590, 313.2483899364063973, -7.014562113412794453 ) ) ;
#40446 = CARTESIAN_POINT ( 'NONE',  ( 2.539812460490211254, -69.30643486802681252, 12.95064966738993206 ) ) ;
#40447 = CARTESIAN_POINT ( 'NONE',  ( 77.79618479429522893, -60.00000000000002132, 192.4023258609882703 ) ) ;
#40448 = ADVANCED_FACE ( 'NONE', ( #86959 ), #70519, .T. ) ;
#40449 = AXIS2_PLACEMENT_3D ( 'NONE', #44746, #61466, #93815 ) ;
#40450 = CARTESIAN_POINT ( 'NONE',  ( 17.53610142485861445, 45.00000000000000000, 63.40563617903067950 ) ) ;
#40451 = ORIENTED_EDGE ( 'NONE', *, *, #65720, .T. ) ;
#40452 = CARTESIAN_POINT ( 'NONE',  ( 55.88705846244756259, -25.61800759129437566, 56.56929643049215173 ) ) ;
#40453 = CARTESIAN_POINT ( 'NONE',  ( -29.90770810728629669, 297.4343786746629235, -9.436196628746156279 ) ) ;
#40454 = CARTESIAN_POINT ( 'NONE',  ( 9.125013381092353271, -53.47235446719983543, 31.09113645985706142 ) ) ;
#40455 = CARTESIAN_POINT ( 'NONE',  ( 5.082755093536325930, -14.46875000204838457, -5.082755093536325042 ) ) ;
#40456 = CARTESIAN_POINT ( 'NONE',  ( -4.651132217449170270, -5.000000000000000000, -15.66661053588738106 ) ) ;
#40457 = ORIENTED_EDGE ( 'NONE', *, *, #53996, .T. ) ;
#40459 = CARTESIAN_POINT ( 'NONE',  ( -9.378402013738298848, -52.21550925151184686, 23.52762072402763849 ) ) ;
#40458 = CARTESIAN_POINT ( 'NONE',  ( -73.94868650964912149, -29.99999999967765874, 149.0933909881836996 ) ) ;
#40460 = CARTESIAN_POINT ( 'NONE',  ( 20.28383506696346572, 302.8321527159674815, -2.004176749255714540 ) ) ;
#40461 = CARTESIAN_POINT ( 'NONE',  ( 26.77982661073470183, 310.9515876031056223, 10.39176322513353945 ) ) ;
#40462 = DIRECTION ( 'NONE',  ( 0.000000000000000000, 1.000000000000000000, 0.000000000000000000 ) ) ;
#40463 = CARTESIAN_POINT ( 'NONE',  ( 5.656854249492378806, -30.68749999999999645, 5.656854249492381470 ) ) ;
#40464 = CARTESIAN_POINT ( 'NONE',  ( -6.145467200824362486, -3.000000000000002665, -77.00333157709341947 ) ) ;
#40465 = CARTESIAN_POINT ( 'NONE',  ( 64.32470902915412125, 48.00000000000002842, 10.67393577672274496 ) ) ;
#40466 = ORIENTED_EDGE ( 'NONE', *, *, #74666, .T. ) ;
#40467 = CARTESIAN_POINT ( 'NONE',  ( 85.58024585952806262, -21.93954400496754076, 167.0656778985148208 ) ) ;
#40468 = DIRECTION ( 'NONE',  ( -0.000000000000000000, 1.000000000000000000, 0.000000000000000000 ) ) ;
#40469 = CARTESIAN_POINT ( 'NONE',  ( 8.559508646656398767, 51.83514083332404709, 1.531152949374243510 ) ) ;
#40470 = ORIENTED_EDGE ( 'NONE', *, *, #12855, .T. ) ;
#40471 = DIRECTION ( 'NONE',  ( -1.000000000000000000, -0.000000000000000000, -0.000000000000000000 ) ) ;
#40472 = CARTESIAN_POINT ( 'NONE',  ( 7.007554382048097885, -4.192628124804436140, -17.12907408884460381 ) ) ;
#40473 = CARTESIAN_POINT ( 'NONE',  ( 44.35000000000000142, 1.533819458162526451E-15, 0.000000000000000000 ) ) ;
#40474 = CARTESIAN_POINT ( 'NONE',  ( 67.22793774957824553, -1.232595164407830946E-29, 4.000000000000007105 ) ) ;
#40475 = CARTESIAN_POINT ( 'NONE',  ( -38.05267008021335329, 42.17823295822772423, -58.18622768867230377 ) ) ;
#40476 = EDGE_CURVE ( 'NONE', #47808, #87076, #99193, .T. ) ;
#40477 = CARTESIAN_POINT ( 'NONE',  ( -28.88581594204406144, 13.70410095367683567, -39.88976374582071571 ) ) ;
#40478 = EDGE_CURVE ( 'NONE', #26898, #9600, #39497, .T. ) ;
#40479 = AXIS2_PLACEMENT_3D ( 'NONE', #27633, #93398, #85295 ) ;
#40480 =( LENGTH_UNIT ( ) NAMED_UNIT ( * ) SI_UNIT ( .MILLI., .METRE. ) );
#40481 = CIRCLE ( 'NONE', #87016, 4.000000000000001776 ) ;
#40482 = EDGE_CURVE ( 'NONE', #41809, #79477, #25969, .T. ) ;
#40483 = CARTESIAN_POINT ( 'NONE',  ( 38.17897261654190544, 25.52811330230706233, 11.10485842511383581 ) ) ;
#40484 = DIRECTION ( 'NONE',  ( 0.000000000000000000, -1.000000000000000000, 0.000000000000000000 ) ) ;
#40486 = CARTESIAN_POINT ( 'NONE',  ( -10.93260317179502472, 11.17563650224738403, -9.852957799267798578 ) ) ;
#40485 = CARTESIAN_POINT ( 'NONE',  ( -25.75788261965884018, -29.55814103031516638, 38.55856135386892447 ) ) ;
#40487 = AXIS2_PLACEMENT_3D ( 'NONE', #59501, #26629, #44372 ) ;
#40488 = CARTESIAN_POINT ( 'NONE',  ( 7.188101187499999156, -13.25000000204838280, 2.977408999572654924 ) ) ;
#40489 = CARTESIAN_POINT ( 'NONE',  ( 19.59433841236636553, 302.7299593794648445, -10.02589861385249215 ) ) ;
#40490 = AXIS2_PLACEMENT_3D ( 'NONE', #57519, #82343, #6855 ) ;
#40491 = VECTOR ( 'NONE', #72360, 1000.000000000000000 ) ;
#40492 = CARTESIAN_POINT ( 'NONE',  ( -7.090506018371190322, 41.24767894959148151, -58.61600934880981839 ) ) ;
#40493 = AXIS2_PLACEMENT_3D ( 'NONE', #58435, #7739, #58975 ) ;
#40494 = AXIS2_PLACEMENT_3D ( 'NONE', #9104, #98645, #2073 ) ;
#40495 = EDGE_LOOP ( 'NONE', ( #62996, #60030, #103941, #86870 ) ) ;
#40496 = CARTESIAN_POINT ( 'NONE',  ( -17.49999999999999289, 49.17341269449792662, 64.03715209376036910 ) ) ;
#40497 = CARTESIAN_POINT ( 'NONE',  ( 43.95063711303827603, 484.1591904870578560, -1.189330446659109697 ) ) ;
#40498 = COLOUR_RGB ( '', 0.31764706, 0.68627451, 0.89019608) ;
#40499 = CARTESIAN_POINT ( 'NONE',  ( -8.147310229341139021, 111.6670789908538381, -1.269956413672949300E-12 ) ) ;
#40500 = LINE ( 'NONE', #16215, #51543 ) ;
#40501 = DIRECTION ( 'NONE',  ( -1.000000000000000000, -1.224606353822377258E-16, -0.000000000000000000 ) ) ;
#40502 = ORIENTED_EDGE ( 'NONE', *, *, #63592, .T. ) ;
#40503 = CARTESIAN_POINT ( 'NONE',  ( 12.95110512856954443, 19.14606607232447999, -7.926761694102399503 ) ) ;
#40504 = CARTESIAN_POINT ( 'NONE',  ( -4.071242075002222904, 52.05516629550404417, 6.992118958553540153 ) ) ;
#40505 = EDGE_LOOP ( 'NONE', ( #99461, #78337, #10472, #77205, #83021, #755 ) ) ;
#40506 = ADVANCED_FACE ( 'NONE', ( #3 ), #74977, .T. ) ;
#40507 = DIRECTION ( 'NONE',  ( -1.000000000000000000, 0.000000000000000000, 0.000000000000000000 ) ) ;
#40508 = DIRECTION ( 'NONE',  ( 1.000000000000000000, -0.000000000000000000, -0.000000000000000000 ) ) ;
#40509 = CARTESIAN_POINT ( 'NONE',  ( -110.1309406653868734, -59.99999999999999289, 144.5015686475491066 ) ) ;
#40510 = FACE_BOUND ( 'NONE', #32132, .T. ) ;
#40511 = CARTESIAN_POINT ( 'NONE',  ( -14.73061733093910419, 41.88685485518190177, -82.04000854990557912 ) ) ;
#40512 = LINE ( 'NONE', #55607, #1877 ) ;
#40513 = CARTESIAN_POINT ( 'NONE',  ( -11.33763709711443823, 2.316981289466677918, 14.82083525685649228 ) ) ;
#40515 = CARTESIAN_POINT ( 'NONE',  ( 30.00000000000000355, 489.8675765671201248, 6.488452894205156696 ) ) ;
#40514 = CARTESIAN_POINT ( 'NONE',  ( 10.48543666094595217, -5.000000000000002665, -91.04342776276725147 ) ) ;
#40516 = EDGE_CURVE ( 'NONE', #50935, #4789, #8, .T. ) ;
#40517 = CARTESIAN_POINT ( 'NONE',  ( -84.23375024055349058, -35.93203514404092402, 175.7405516498321560 ) ) ;
#40518 = ORIENTED_EDGE ( 'NONE', *, *, #62201, .T. ) ;
#40519 = CARTESIAN_POINT ( 'NONE',  ( 4.852941176470593199, 41.41666666666666430, -70.80672828634229177 ) ) ;
#40520 = ORIENTED_EDGE ( 'NONE', *, *, #56251, .F. ) ;
#40521 = COLOUR_RGB ( '', 0.72549020, 0.75294118, 0.79215686) ;
#40522 = ORIENTED_EDGE ( 'NONE', *, *, #37183, .T. ) ;
#40523 = DIRECTION ( 'NONE',  ( 0.5735764363510466035, -0.8191520442889914655, 1.003171929053524500E-16 ) ) ;
#40524 = EDGE_CURVE ( 'NONE', #33126, #33037, #98720, .T. ) ;
#40525 = CARTESIAN_POINT ( 'NONE',  ( 32.64206520363632791, 464.2415374745278882, 8.403253426445765228 ) ) ;
#40526 = DIRECTION ( 'NONE',  ( 0.000000000000000000, 0.000000000000000000, -1.000000000000000000 ) ) ;
#40527 = CARTESIAN_POINT ( 'NONE',  ( -14.44581512915354615, 5.963299184995717539, -7.135127315210193721 ) ) ;
#40528 = CARTESIAN_POINT ( 'NONE',  ( 9.075140001326078121, 14.05259049549145978, 0.000000000000000000 ) ) ;
#40529 = CARTESIAN_POINT ( 'NONE',  ( 12.51690618612821204, -5.000000000000000000, -88.70140625282380142 ) ) ;
#40530 = CARTESIAN_POINT ( 'NONE',  ( 0.000000000000000000, 0.000000000000000000, 0.000000000000000000 ) ) ;
#40531 = CARTESIAN_POINT ( 'NONE',  ( 106.4003153237399459, -14.21045842199437281, 159.7124754531589019 ) ) ;
#40532 = CARTESIAN_POINT ( 'NONE',  ( -107.3650189024811681, -30.00000000000002842, 190.7478110277085648 ) ) ;
#40533 = CARTESIAN_POINT ( 'NONE',  ( -63.44189309749444305, -32.53320303695706173, 78.14391273869415500 ) ) ;
#40534 = ORIENTED_EDGE ( 'NONE', *, *, #16740, .F. ) ;
#40535 = CARTESIAN_POINT ( 'NONE',  ( -43.19279117978085480, 484.2727584554530154, -0.4218381927343575200 ) ) ;
#40536 = CARTESIAN_POINT ( 'NONE',  ( 96.28976944069333399, -59.99999999998052402, 40.92003399396909202 ) ) ;
#40537 = ORIENTED_EDGE ( 'NONE', *, *, #57076, .F. ) ;
#40538 = DIRECTION ( 'NONE',  ( -0.000000000000000000, -1.000000000000000000, -0.000000000000000000 ) ) ;
#40539 = CARTESIAN_POINT ( 'NONE',  ( -5.082755093536325042, -11.46875000204838635, -5.082755093536325930 ) ) ;
#40540 = DIRECTION ( 'NONE',  ( -0.000000000000000000, 1.000000000000000000, -0.000000000000000000 ) ) ;
#40541 = ORIENTED_EDGE ( 'NONE', *, *, #52675, .T. ) ;
#40542 = LINE ( 'NONE', #15735, #7912 ) ;
#40543 = ORIENTED_EDGE ( 'NONE', *, *, #21881, .F. ) ;
#40544 = DIRECTION ( 'NONE',  ( 0.000000000000000000, 1.000000000000000000, 0.000000000000000000 ) ) ;
#40545 = MECHANICAL_DESIGN_GEOMETRIC_PRESENTATION_REPRESENTATION (  '', ( #18171 ), #28574 ) ;
#40546 = CARTESIAN_POINT ( 'NONE',  ( 6.797283463257937974, -29.92009708584722461, -3.368226723814712109 ) ) ;
#40547 = CARTESIAN_POINT ( 'NONE',  ( -109.2164123534708580, -60.00000000000000000, 193.3227612444920851 ) ) ;
#40548 = CARTESIAN_POINT ( 'NONE',  ( -3.454253436624959317, -0.8414180287960622007, 103.7259032015042379 ) ) ;
#40549 = CARTESIAN_POINT ( 'NONE',  ( -1.320432766682874540E-15, -25.90625000204838813, 7.188101187500000044 ) ) ;
#40550 = CARTESIAN_POINT ( 'NONE',  ( 45.99999999999999289, 461.9217514388778341, 5.107711371735583761 ) ) ;
#40551 = CARTESIAN_POINT ( 'NONE',  ( -24.42523734047231798, 27.59258781593598542, -31.59665717925402006 ) ) ;
#40552 = CARTESIAN_POINT ( 'NONE',  ( 0.000000000000000000, 0.000000000000000000, 5.000000000000002665 ) ) ;
#40553 = CARTESIAN_POINT ( 'NONE',  ( 13.50000000000000355, 2.646256834279079317, -12.86070865178833600 ) ) ;
#40554 =( NAMED_UNIT ( * ) SI_UNIT ( $, .STERADIAN. ) SOLID_ANGLE_UNIT ( ) );
#40555 = EDGE_CURVE ( 'NONE', #89315, #67219, #76578, .T. ) ;
#40556 = CARTESIAN_POINT ( 'NONE',  ( 8.826976704351871206, -4.090868165775439103, 14.50637990094349306 ) ) ;
#40557 = FILL_AREA_STYLE_COLOUR ( '', #20402 ) ;
#40558 = CARTESIAN_POINT ( 'NONE',  ( 105.7220129672738693, -60.00000000000001421, 184.2428138410215581 ) ) ;
#40559 = CARTESIAN_POINT ( 'NONE',  ( -32.48662781215343642, -49.90568005501813786, 36.01986044320511837 ) ) ;
#40560 = CARTESIAN_POINT ( 'NONE',  ( -3.037443755949079005, -49.45229994217047675, 103.2087721268168252 ) ) ;
#40561 = CARTESIAN_POINT ( 'NONE',  ( 41.95256787860516567, -60.24835236458953602, 45.28280848969064465 ) ) ;
#40562 = CARTESIAN_POINT ( 'NONE',  ( 0.000000000000000000, 61.50000000000000000, 6.999999999999992895 ) ) ;
#40563 = ORIENTED_EDGE ( 'NONE', *, *, #47774, .F. ) ;
#40564 = EDGE_CURVE ( 'NONE', #44923, #24536, #86248, .T. ) ;
#40565 = CARTESIAN_POINT ( 'NONE',  ( -7.934914944860279817, 88.86845647200112808, -1.051261972695690439 ) ) ;
#40566 = CARTESIAN_POINT ( 'NONE',  ( -82.29585130749137534, -38.83734455563418919, 196.2398665998169918 ) ) ;
#40567 = ORIENTED_EDGE ( 'NONE', *, *, #34703, .T. ) ;
#40569 = CARTESIAN_POINT ( 'NONE',  ( 39.24156521425334176, 307.7088117867400001, -7.003459073692002157 ) ) ;
#40568 = LINE ( 'NONE', #24431, #28047 ) ;
#40570 = CARTESIAN_POINT ( 'NONE',  ( -13.55583764533404612, 24.70617620989347074, -1.273591148780106153 ) ) ;
#40572 = ADVANCED_FACE ( 'NONE', ( #51772 ), #61496, .T. ) ;
#40571 = CARTESIAN_POINT ( 'NONE',  ( -33.11888822396105780, 438.9412710830819151, 23.90522241289612992 ) ) ;
#40573 = CARTESIAN_POINT ( 'NONE',  ( -6.738100187484505454, 41.71798639774085160, -59.05424569925489209 ) ) ;
#40574 = AXIS2_PLACEMENT_3D ( 'NONE', #84354, #83804, #92968 ) ;
#40575 = CARTESIAN_POINT ( 'NONE',  ( 6.683837171061803417, 3.955946848495959234, -6.851900933636991375 ) ) ;
#40576 = CARTESIAN_POINT ( 'NONE',  ( -39.41219261697557386, 436.7611714244557675, 5.258763975273992308 ) ) ;
#40577 = CARTESIAN_POINT ( 'NONE',  ( 5.191472769733078252, -87.64091576718952581, -3.014900733016756540 ) ) ;
#40578 = CARTESIAN_POINT ( 'NONE',  ( -8.000000000000000000, -25.43750000409677270, -9.797174393178825657E-16 ) ) ;
#40579 = CARTESIAN_POINT ( 'NONE',  ( 92.01709497311385633, -60.00000000000000711, 18.79751796720415769 ) ) ;
#40580 = AXIS2_PLACEMENT_3D ( 'NONE', #87805, #13884, #31701 ) ;
#40581 = CARTESIAN_POINT ( 'NONE',  ( -5.681858674226697659, -50.93014719887724340, 39.79579700850658952 ) ) ;
#40582 = VECTOR ( 'NONE', #68080, 1000.000000000000000 ) ;
#40583 = EDGE_LOOP ( 'NONE', ( #37702, #15619, #93026, #21542 ) ) ;
#40584 = CARTESIAN_POINT ( 'NONE',  ( -89.76477315035992888, -29.99999999999963407, 189.6654235243697144 ) ) ;
#40585 = ORIENTED_EDGE ( 'NONE', *, *, #36716, .T. ) ;
#40586 = CARTESIAN_POINT ( 'NONE',  ( -10.00248409573528896, -58.00033248952951936, 26.85804522429446095 ) ) ;
#40587 = CARTESIAN_POINT ( 'NONE',  ( -16.01236629286567492, 3.722328191965275312, 0.3359674916118658983 ) ) ;
#40588 = CARTESIAN_POINT ( 'NONE',  ( 3.836943873307946173, 17.95160350248317371, 4.999999999999999112 ) ) ;
#40589 = DIRECTION ( 'NONE',  ( 0.000000000000000000, -0.000000000000000000, 1.000000000000000000 ) ) ;
#40590 = CARTESIAN_POINT ( 'NONE',  ( -22.39889803669559143, 27.64071832785175786, -32.90416900124266419 ) ) ;
#40591 = CARTESIAN_POINT ( 'NONE',  ( 5.082755093536325930, -25.34375000204838813, -5.082755093536325042 ) ) ;
#40592 = FACE_OUTER_BOUND ( 'NONE', #38909, .T. ) ;
#40593 = DIRECTION ( 'NONE',  ( -1.000000000000000000, 0.000000000000000000, 0.000000000000000000 ) ) ;
#40594 = ORIENTED_EDGE ( 'NONE', *, *, #41815, .F. ) ;
#40596 = VERTEX_POINT ( 'NONE', #20005 ) ;
#40595 = CARTESIAN_POINT ( 'NONE',  ( -7.343808464831893090, 40.90987269173472640, -58.79603257166633057 ) ) ;
#40597 = CARTESIAN_POINT ( 'NONE',  ( 82.78508296686045753, -25.62180102098898260, 148.0795101033245942 ) ) ;
#40598 = CARTESIAN_POINT ( 'NONE',  ( 19.50000000000000000, 12.99999999999999289, 6.999999999999999112 ) ) ;
#40599 = DIRECTION ( 'NONE',  ( -1.000000000000000000, -0.000000000000000000, -0.000000000000000000 ) ) ;
#40600 = ORIENTED_EDGE ( 'NONE', *, *, #100251, .F. ) ;
#40601 = CARTESIAN_POINT ( 'NONE',  ( -59.10637965291887497, 50.00000000000001421, -21.83934624968677340 ) ) ;
#40602 = CARTESIAN_POINT ( 'NONE',  ( -14.24907788157500121, 2.189443139868889165, -4.658781708030211632 ) ) ;
#40603 = CARTESIAN_POINT ( 'NONE',  ( 4.401442555609581635E-16, -15.78125000204838635, -7.188101187500000044 ) ) ;
#40604 = DIRECTION ( 'NONE',  ( 0.000000000000000000, 0.000000000000000000, 1.000000000000000000 ) ) ;
#40605 = DIRECTION ( 'NONE',  ( -0.5735764363510494901, -0.8191520442889894671, 0.000000000000000000 ) ) ;
#40606 = CARTESIAN_POINT ( 'NONE',  ( -19.49904798085934843, -57.67182591607114261, 42.12704350231687300 ) ) ;
#40607 = CARTESIAN_POINT ( 'NONE',  ( -33.16948502134867027, 434.2034787425552622, 15.24753222728177882 ) ) ;
#40608 = EDGE_CURVE ( 'NONE', #48231, #72001, #29001, .T. ) ;
#40609 = ORIENTED_EDGE ( 'NONE', *, *, #73796, .T. ) ;
#40610 = DIRECTION ( 'NONE',  ( 0.000000000000000000, 0.000000000000000000, 1.000000000000000000 ) ) ;
#40611 = ADVANCED_FACE ( 'NONE', ( #102467 ), #101406, .F. ) ;
#40612 = CARTESIAN_POINT ( 'NONE',  ( 7.413001015142842931, 41.14546113202533206, -59.83891282166461423 ) ) ;
#40613 = CARTESIAN_POINT ( 'NONE',  ( 34.83349330513379982, 4.000000000000003553, 0.000000000000000000 ) ) ;
#40614 = ORIENTED_EDGE ( 'NONE', *, *, #50323, .T. ) ;
#40615 = CARTESIAN_POINT ( 'NONE',  ( -5.082755093536325042, -29.09375000204838813, -5.082755093536325930 ) ) ;
#40616 = CARTESIAN_POINT ( 'NONE',  ( 24.60495542872522989, -28.77046205659021183, 38.13801889905689535 ) ) ;
#40617 = CARTESIAN_POINT ( 'NONE',  ( 0.6461105361034419348, 52.10944840786394394, -7.916821239980341929 ) ) ;
#40618 = DIRECTION ( 'NONE',  ( 0.000000000000000000, -0.8568390274594218647, -0.5155840193628893342 ) ) ;
#40619 = VECTOR ( 'NONE', #31895, 1000.000000000000227 ) ;
#40620 = APPLICATION_PROTOCOL_DEFINITION ( 'draft international standard', 'automotive_design', 1998, #84455 ) ;
#40621 = CARTESIAN_POINT ( 'NONE',  ( 48.90253429252455675, 9.379793601652295365, 14.70143532337736403 ) ) ;
#40622 = VERTEX_POINT ( 'NONE', #85771 ) ;
#40623 = CARTESIAN_POINT ( 'NONE',  ( -2.918503601030651318, 15.30040232763897023, 9.571198553004045095 ) ) ;
#40624 = CARTESIAN_POINT ( 'NONE',  ( 13.54749644447708512, 42.91257261702131842, -91.87527161981162749 ) ) ;
#40625 = CARTESIAN_POINT ( 'NONE',  ( 3.718545543012941490, -21.49349533113791821, -38.54945152629040450 ) ) ;
#40626 = DIRECTION ( 'NONE',  ( -1.000000000000000000, -1.224606353822377258E-16, -0.000000000000000000 ) ) ;
#40627 = CARTESIAN_POINT ( 'NONE',  ( 0.000000000000000000, 4.898587196589412829E-16, -4.000000000000000000 ) ) ;
#40628 = EDGE_CURVE ( 'NONE', #104803, #39277, #101475, .T. ) ;
#40629 = ORIENTED_EDGE ( 'NONE', *, *, #85737, .F. ) ;
#40630 = DIRECTION ( 'NONE',  ( -0.8191520442889884679, 1.003171929053520679E-16, 0.5735764363510509334 ) ) ;
#40631 =( GEOMETRIC_REPRESENTATION_CONTEXT ( 3 ) GLOBAL_UNCERTAINTY_ASSIGNED_CONTEXT ( ( #79296 ) ) GLOBAL_UNIT_ASSIGNED_CONTEXT ( ( #58061, #90985, #105038 ) ) REPRESENTATION_CONTEXT ( 'NONE', 'WORKASPACE' ) );
#40632 = CARTESIAN_POINT ( 'NONE',  ( 114.2143086744109866, -57.67130378733651241, 175.1586867808284467 ) ) ;
#40633 = EDGE_CURVE ( 'NONE', #33590, #42859, #68769, .T. ) ;
#40634 = CARTESIAN_POINT ( 'NONE',  ( -9.183473878344010188, 51.37213498224890884, -3.876623111190086846 ) ) ;
#40635 = DIRECTION ( 'NONE',  ( 0.000000000000000000, -1.000000000000000000, 0.000000000000000000 ) ) ;
#40636 = CIRCLE ( 'NONE', #33738, 4.172000000000009479 ) ;
#40637 = CARTESIAN_POINT ( 'NONE',  ( -9.797174393178825657E-16, -3.000000000000000000, 8.000000000000000000 ) ) ;
#40638 = CARTESIAN_POINT ( 'NONE',  ( -74.81582692897852382, -59.99999999999998579, 179.8343382549642229 ) ) ;
#40639 = CONICAL_SURFACE ( 'NONE', #26903, 3.309500000000001663, 0.9599310885968770357 ) ;
#40640 = CIRCLE ( 'NONE', #71658, 61.23540616453487218 ) ;
#40641 = VECTOR ( 'NONE', #1639, 1000.000000000000000 ) ;
#40642 = LINE ( 'NONE', #91338, #18355 ) ;
#40643 = CARTESIAN_POINT ( 'NONE',  ( -50.18984356160270011, 50.00000000000000000, 38.51389699557558544 ) ) ;
#40644 = EDGE_CURVE ( 'NONE', #13955, #98501, #36066, .T. ) ;
#40645 = CARTESIAN_POINT ( 'NONE',  ( -85.12695384070762827, -39.34156027617945739, 184.1518049699909625 ) ) ;
#40646 = ORIENTED_EDGE ( 'NONE', *, *, #20515, .T. ) ;
#40647 = CARTESIAN_POINT ( 'NONE',  ( 26.73461998295247000, 307.3006012187427132, -9.456373384271907767 ) ) ;
#40648 = CIRCLE ( 'NONE', #59617, 6.999999999999992895 ) ;
#40649 = VERTEX_POINT ( 'NONE', #51229 ) ;
#40650 = CARTESIAN_POINT ( 'NONE',  ( 14.75116209840774495, 43.55504285524111907, -90.22050492864485705 ) ) ;
#40651 = EDGE_CURVE ( 'NONE', #5701, #41862, #49791, .T. ) ;
#40652 = CARTESIAN_POINT ( 'NONE',  ( 31.36650669486618881, 4.000000000000003553, 4.898587196589414801E-16 ) ) ;
#40653 = CARTESIAN_POINT ( 'NONE',  ( -85.67493770007969545, -52.74798379930503245, -9.150851446102391762 ) ) ;
#40654 = CARTESIAN_POINT ( 'NONE',  ( -32.64200203778431586, 464.2416672416182450, 8.403568186820926655 ) ) ;
#40656 = CIRCLE ( 'NONE', #11392, 5.000000000000010658 ) ;
#40655 = CARTESIAN_POINT ( 'NONE',  ( 27.33349330513380337, 1.593028355512270567E-15, 0.000000000000000000 ) ) ;
#40657 = EDGE_LOOP ( 'NONE', ( #60850, #38102, #100325, #25181, #80044, #24265, #103956, #69783 ) ) ;
#40658 = CARTESIAN_POINT ( 'NONE',  ( 13.70756188771709283, 3.094783711518300784, -6.047234902213228125 ) ) ;
#40659 = CARTESIAN_POINT ( 'NONE',  ( -16.57301948837645256, -1.734723475976807094E-15, 4.453875240771298039 ) ) ;
#40660 = CARTESIAN_POINT ( 'NONE',  ( -35.72538317320573498, 438.1659592258367297, 3.984952432983437376 ) ) ;
#40661 = CARTESIAN_POINT ( 'NONE',  ( 55.21462903151665813, -59.99999999999998579, -39.23961370773703550 ) ) ;
#40662 = CARTESIAN_POINT ( 'NONE',  ( -76.65370120091482420, -42.96681426229719136, 130.6272736503597969 ) ) ;
#40663 = ORIENTED_EDGE ( 'NONE', *, *, #95493, .F. ) ;
#40664 = CARTESIAN_POINT ( 'NONE',  ( 7.344361273354515163, 87.44560530588523761, -3.175733139645585457 ) ) ;
#40665 = CARTESIAN_POINT ( 'NONE',  ( 114.1124408062617448, -57.67112371907345647, 167.6041526721556636 ) ) ;
#40666 = ORIENTED_EDGE ( 'NONE', *, *, #54618, .F. ) ;
#40667 = CARTESIAN_POINT ( 'NONE',  ( 27.42222224296737565, 34.64411886747944180, 7.587464081913322111 ) ) ;
#40668 = DIRECTION ( 'NONE',  ( 0.000000000000000000, 0.000000000000000000, -1.000000000000000000 ) ) ;
#40669 = ORIENTED_EDGE ( 'NONE', *, *, #78625, .F. ) ;
#40670 = CARTESIAN_POINT ( 'NONE',  ( 53.29999999999999716, 6.915964383211875250E-15, 0.000000000000000000 ) ) ;
#40671 = DIRECTION ( 'NONE',  ( 0.000000000000000000, -1.000000000000000000, 0.000000000000000000 ) ) ;
#40672 = DIRECTION ( 'NONE',  ( 0.000000000000000000, 0.000000000000000000, 1.000000000000000000 ) ) ;
#40673 = CARTESIAN_POINT ( 'NONE',  ( 7.188101187499999156, -19.25000000204838813, 2.977408999572654924 ) ) ;
#40674 = CARTESIAN_POINT ( 'NONE',  ( 43.68959978692338098, 484.5138553196885596, 2.648407630515406286 ) ) ;
#40675 = VECTOR ( 'NONE', #69743, 1000.000000000000000 ) ;
#40676 = FILL_AREA_STYLE_COLOUR ( '', #79556 ) ;
#40677 = EDGE_CURVE ( 'NONE', #32988, #44416, #31056, .T. ) ;
#40678 = CARTESIAN_POINT ( 'NONE',  ( -17.85737165039477148, 45.30383319674704978, -5.717692534355175660 ) ) ;
#40679 = CARTESIAN_POINT ( 'NONE',  ( 13.58349330513380515, 1.593028355512270962E-15, 0.000000000000000000 ) ) ;
#40680 = ORIENTED_EDGE ( 'NONE', *, *, #57348, .T. ) ;
#40681 = CARTESIAN_POINT ( 'NONE',  ( -7.418912472240797307, 41.12212780509316445, -69.28711574108936588 ) ) ;
#40683 = CARTESIAN_POINT ( 'NONE',  ( 29.01152024031640408, -36.00842521231714954, 32.18407090136901871 ) ) ;
#40682 = CARTESIAN_POINT ( 'NONE',  ( -12.27152016684560820, -14.21045842199446874, 34.40193250091021326 ) ) ;
#40684 = CARTESIAN_POINT ( 'NONE',  ( 28.32487310513930012, 309.0837454060449545, -8.036865677558150622 ) ) ;
#40685 = EDGE_LOOP ( 'NONE', ( #4965, #72789, #40171, #37664, #95233 ) ) ;
#40686 = EDGE_CURVE ( 'NONE', #35905, #103542, #48944, .T. ) ;
#40687 = ORIENTED_EDGE ( 'NONE', *, *, #50278, .F. ) ;
#40689 = CARTESIAN_POINT ( 'NONE',  ( 35.57182711849233669, 461.3662169729752804, 3.401134023656063654 ) ) ;
#40688 = DIRECTION ( 'NONE',  ( -1.000000000000000000, -1.224606353822377258E-16, -0.000000000000000000 ) ) ;
#40690 = FACE_OUTER_BOUND ( 'NONE', #92035, .T. ) ;
#40691 = DIRECTION ( 'NONE',  ( -1.000000000000000000, -0.000000000000000000, -0.000000000000000000 ) ) ;
#40692 = CARTESIAN_POINT ( 'NONE',  ( -3.313708498984765161, -19.15625000409677270, 7.999999999999998224 ) ) ;
#40693 = CARTESIAN_POINT ( 'NONE',  ( 0.6451975519659806091, 45.36065750478253733, 18.58354771593489474 ) ) ;
#40694 = CARTESIAN_POINT ( 'NONE',  ( -36.32791536946549371, 464.0041716472547364, 19.58704090454801872 ) ) ;
#40695 = VERTEX_POINT ( 'NONE', #4831 ) ;
#40696 = DIRECTION ( 'NONE',  ( 0.000000000000000000, 1.000000000000000000, 0.000000000000000000 ) ) ;
#40697 = AXIS2_PLACEMENT_3D ( 'NONE', #72963, #46064, #30424 ) ;
#40698 = CARTESIAN_POINT ( 'NONE',  ( -10.61948831387139336, 45.32774727476011378, -15.37414989828182676 ) ) ;
#40700 = EDGE_CURVE ( 'NONE', #58207, #6171, #63617, .T. ) ;
#40699 = FACE_OUTER_BOUND ( 'NONE', #97171, .T. ) ;
#40701 = CARTESIAN_POINT ( 'NONE',  ( 6.326622418652845248, -1.327077765693001954, 6.831545684615176306 ) ) ;
#40702 = FACE_OUTER_BOUND ( 'NONE', #79016, .T. ) ;
#40703 = VERTEX_POINT ( 'NONE', #22640 ) ;
#40704 = CONICAL_SURFACE ( 'NONE', #14897, 4.000000000000001776, 0.9599310885968774798 ) ;
#40705 = LINE ( 'NONE', #73593, #5733 ) ;
#40706 = ORIENTED_EDGE ( 'NONE', *, *, #83989, .T. ) ;
#40707 = ORIENTED_EDGE ( 'NONE', *, *, #99508, .F. ) ;
#40708 = DIRECTION ( 'NONE',  ( 0.9915366780650375356, 0.1269898409407626272, 0.02699252395738695881 ) ) ;
#40709 = CARTESIAN_POINT ( 'NONE',  ( 17.92907372343373851, 41.95109139595307823, -82.51358908730536257 ) ) ;
#40710 = CARTESIAN_POINT ( 'NONE',  ( -36.44570453002955901, 439.0052206251579037, 23.96112351096716253 ) ) ;
#40711 = CARTESIAN_POINT ( 'NONE',  ( 30.15981381208334611, 316.9131350538594916, 13.38073451593941243 ) ) ;
#40712 = CARTESIAN_POINT ( 'NONE',  ( -37.40172753335533429, 356.7446856187958701, 2.250060923472283481 ) ) ;
#40713 = CARTESIAN_POINT ( 'NONE',  ( -5.100994920550437683, -63.33738541091079810, 13.92370273215852627 ) ) ;
#40714 =( LENGTH_UNIT ( ) NAMED_UNIT ( * ) SI_UNIT ( .MILLI., .METRE. ) );
#40715 = ORIENTED_EDGE ( 'NONE', *, *, #30086, .F. ) ;
#40716 = CARTESIAN_POINT ( 'NONE',  ( -9.882256759026930126, 43.35737001761634701, 15.34350100720170218 ) ) ;
#40717 = ORIENTED_EDGE ( 'NONE', *, *, #720, .F. ) ;
#40718 = DIRECTION ( 'NONE',  ( 0.000000000000000000, 1.000000000000000000, 0.000000000000000000 ) ) ;
#40719 = CARTESIAN_POINT ( 'NONE',  ( 0.000000000000000000, 304.8518027762758038, 9.936999415352289589 ) ) ;
#40720 =( LENGTH_UNIT ( ) NAMED_UNIT ( * ) SI_UNIT ( .MILLI., .METRE. ) );
#40721 = AXIS2_PLACEMENT_3D ( 'NONE', #44588, #60776, #52651 ) ;
#40722 = CIRCLE ( 'NONE', #23516, 13.00000000000003730 ) ;
#40723 = COLOUR_RGB ( '', 0.08235294, 0.09019608, 0.10196078) ;
#40724 = CIRCLE ( 'NONE', #70059, 5.000000000000001776 ) ;
#40725 = CARTESIAN_POINT ( 'NONE',  ( -66.69712465749149999, -59.99999999999995026, 102.5519887578948044 ) ) ;
#40726 = CARTESIAN_POINT ( 'NONE',  ( 65.80416729607647142, -42.95812090186399246, 90.41729902910192607 ) ) ;
#40727 = VECTOR ( 'NONE', #61117, 1000.000000000000000 ) ;
#40728 = ORIENTED_EDGE ( 'NONE', *, *, #14037, .T. ) ;
#40729 = SURFACE_SIDE_STYLE ('',( #74151 ) ) ;
#40730 = COLOUR_RGB ( '', 0.31764706, 0.68627451, 0.89019608) ;
#40731 = CARTESIAN_POINT ( 'NONE',  ( 3.368226723814772505, -29.92009708584722461, 6.797283463257880243 ) ) ;
#40732 =( BOUNDED_SURFACE ( )  B_SPLINE_SURFACE ( 2, 3, ( 
 ( #102052, #93976, #93452, #69703, #95052, #100993, #3903, #19601, #62161, #52432 ),
 ( #86437, #28215, #27151, #92898, #28745, #54017, #19063, #36835, #51904, #78836 ),
 ( #2822, #84817, #12501, #101533, #61630, #85349, #60039, #4425, #86960, #20672 ) ),
 .UNSPECIFIED., .F., .F., .F. ) 
 B_SPLINE_SURFACE_WITH_KNOTS ( ( 3, 3 ),
 ( 4, 2, 2, 2, 4 ),
 ( 0.000000000000000000, 1.000000000000000000 ),
 ( -0.9419214012998446961, -0.4709607006499223480, 5.551115123125782702E-17, 0.4709607006499224591, 0.9419214012998448071 ),
 .UNSPECIFIED. ) 
 GEOMETRIC_REPRESENTATION_ITEM ( )  RATIONAL_B_SPLINE_SURFACE ( (
 ( 1.000000000000000000, 1.000000000000000000, 1.000000000000000000, 1.000000000000000000, 1.000000000000000000, 1.000000000000000000, 1.000000000000000000, 1.000000000000000000, 1.000000000000000000, 1.000000000000000000),
 ( 1.857142857142858317, 1.857142857142858317, 1.857142857142858317, 1.857142857142858317, 1.857142857142858317, 1.857142857142858317, 1.857142857142858317, 1.857142857142858317, 1.857142857142858317, 1.857142857142858317),
 ( 1.000000000000000000, 1.000000000000000000, 1.000000000000000000, 1.000000000000000000, 1.000000000000000000, 1.000000000000000000, 1.000000000000000000, 1.000000000000000000, 1.000000000000000000, 1.000000000000000000) ) ) 
 REPRESENTATION_ITEM ( '' )  SURFACE ( )  );
#40733 = CARTESIAN_POINT ( 'NONE',  ( -76.10153353667877241, -57.67120126903460431, -32.17100317442078961 ) ) ;
#40734 = ADVANCED_FACE ( 'NONE', ( #55476 ), #37767, .F. ) ;
#40735 = ORIENTED_EDGE ( 'NONE', *, *, #77992, .F. ) ;
#40736 =( NAMED_UNIT ( * ) SI_UNIT ( $, .STERADIAN. ) SOLID_ANGLE_UNIT ( ) );
#40737 = CARTESIAN_POINT ( 'NONE',  ( 46.79057916015454310, 18.53868985150169024, 15.81409158839495355 ) ) ;
#40738 = EDGE_CURVE ( 'NONE', #61174, #53832, #68610, .T. ) ;
#40739 = CARTESIAN_POINT ( 'NONE',  ( -37.17693862423640638, 491.8028371848064353, 12.56217450279643089 ) ) ;
#40740 = CARTESIAN_POINT ( 'NONE',  ( -48.26938392169753200, 11.04962899253378694, 14.37319483549275390 ) ) ;
#40741 = CARTESIAN_POINT ( 'NONE',  ( 3.313708498984762052, -24.40625000409677270, -8.000000000000000000 ) ) ;
#40742 = CARTESIAN_POINT ( 'NONE',  ( -2.617993873628169599, -5.000000000000000000, -10.00000000000000000 ) ) ;
#40743 = DIRECTION ( 'NONE',  ( 0.000000000000000000, 0.000000000000000000, 1.000000000000000000 ) ) ;
#40744 = CARTESIAN_POINT ( 'NONE',  ( -5.906143312800266720, 4.629399289606634937, 4.999999999999999112 ) ) ;
#40745 = CARTESIAN_POINT ( 'NONE',  ( 84.73333333333332007, -4.171999999999998820, 0.000000000000000000 ) ) ;
#40746 = CARTESIAN_POINT ( 'NONE',  ( -3.884543032214529124, 15.13241195026090047, -9.216463528758191970 ) ) ;
#40747 = ORIENTED_EDGE ( 'NONE', *, *, #78643, .F. ) ;
#40748 = CARTESIAN_POINT ( 'NONE',  ( 86.75754961941542831, 6.123233995736568081E-16, -5.000000000000011546 ) ) ;
#40749 = DIRECTION ( 'NONE',  ( 0.000000000000000000, 1.000000000000000000, 0.000000000000000000 ) ) ;
#40750 = AXIS2_PLACEMENT_3D ( 'NONE', #17754, #32886, #106193 ) ;
#40751 = CARTESIAN_POINT ( 'NONE',  ( -4.999999999999999112, -34.80414770699324833, 1.298653836421715946 ) ) ;
#40752 = CARTESIAN_POINT ( 'NONE',  ( -92.98499943475361817, -29.99999999999999645, 191.1145340721902244 ) ) ;
#40753 = DIRECTION ( 'NONE',  ( 0.000000000000000000, 1.000000000000000000, -5.401608413889052066E-13 ) ) ;
#40754 = CARTESIAN_POINT ( 'NONE',  ( 58.88557130045238353, -57.67677570217782801, 103.6297432740264099 ) ) ;
#40756 = CARTESIAN_POINT ( 'NONE',  ( -7.008653203440415425, 5.325399036039260459, 4.838637849014732595 ) ) ;
#40755 = CARTESIAN_POINT ( 'NONE',  ( 15.10022144576333503, -0.2188905726113574979, 15.00000000000000178 ) ) ;
#40757 = EDGE_CURVE ( 'NONE', #75037, #27550, #29158, .T. ) ;
#40758 = CARTESIAN_POINT ( 'NONE',  ( 18.16042551299854324, -25.16802437573015894, -38.50727583685194588 ) ) ;
#40759 = CARTESIAN_POINT ( 'NONE',  ( -0.7852320185050503110, 43.98274617669912345, 16.51395379932535690 ) ) ;
#40760 = UNCERTAINTY_MEASURE_WITH_UNIT (LENGTH_MEASURE( 1.000000000000000082E-05 ), #47275, 'distance_accuracy_value', 'NONE');
#40761 = FILL_AREA_STYLE_COLOUR ( '', #35763 ) ;
#40762 = CARTESIAN_POINT ( 'NONE',  ( -2.999195618040080280, -60.00000000000000711, 39.63393146347493712 ) ) ;
#40763 = CARTESIAN_POINT ( 'NONE',  ( -0.8750000000009725554, -70.58759490697451611, 13.02737050516266848 ) ) ;
#40764 = CARTESIAN_POINT ( 'NONE',  ( 6.534168656350041182, 53.62238902978714350, 7.078273912249937183 ) ) ;
#40765 = CIRCLE ( 'NONE', #64876, 4.000000000000007105 ) ;
#40766 = CARTESIAN_POINT ( 'NONE',  ( -86.09502989984670762, -57.44075046393530215, 193.2120879883706266 ) ) ;
#40767 = ORIENTED_EDGE ( 'NONE', *, *, #72982, .F. ) ;
#40768 = CARTESIAN_POINT ( 'NONE',  ( 17.50000000000462208, 50.03760136707476391, 61.20291971386502894 ) ) ;
#40769 = CARTESIAN_POINT ( 'NONE',  ( 6.655774809717873275, -15.37882222362587470, 14.67993930426211513 ) ) ;
#40770 = CARTESIAN_POINT ( 'NONE',  ( -9.088156012238943759, -25.54958950038574272, 28.14908607299276255 ) ) ;
#40771 = CYLINDRICAL_SURFACE ( 'NONE', #66943, 4.000000000000000888 ) ;
#40773 = CARTESIAN_POINT ( 'NONE',  ( 3.594139794580319069, -68.26681892886726644, 13.09870760474886531 ) ) ;
#40772 = CARTESIAN_POINT ( 'NONE',  ( -100.1817682225040755, -59.99999999999998579, 195.6478515624593513 ) ) ;
#40774 = VERTEX_POINT ( 'NONE', #5875 ) ;
#40775 = CARTESIAN_POINT ( 'NONE',  ( -6.106525010887766669, -4.373161893764723196, -16.80699797897936421 ) ) ;
#40776 = CARTESIAN_POINT ( 'NONE',  ( -7.002619243997878939, 31.05007318013818463, -3.868708944012996920 ) ) ;
#40777 = AXIS2_PLACEMENT_3D ( 'NONE', #3248, #77672, #18385 ) ;
#40778 = AXIS2_PLACEMENT_3D ( 'NONE', #4585, #103281, #13182 ) ;
#40779 = CARTESIAN_POINT ( 'NONE',  ( 28.02604061233149579, 305.7734989515280404, -9.350961192283897105 ) ) ;
#40780 = CARTESIAN_POINT ( 'NONE',  ( 42.33349330513380693, -7.703719777548943412E-31, 4.000000000000001776 ) ) ;
#40781 = CARTESIAN_POINT ( 'NONE',  ( -7.213352437320217803, -82.98163526992318850, -3.463014597543483841 ) ) ;
#40782 = DIRECTION ( 'NONE',  ( 0.000000000000000000, -1.000000000000000000, 0.000000000000000000 ) ) ;
#40783 = CARTESIAN_POINT ( 'NONE',  ( 106.9596233951320698, -14.21045842199439591, 171.9689152078629775 ) ) ;
#40784 = DIRECTION ( 'NONE',  ( 1.000000000000000000, 1.224606353822377258E-16, 0.000000000000000000 ) ) ;
#40785 = ORIENTED_EDGE ( 'NONE', *, *, #46780, .F. ) ;
#40786 = CARTESIAN_POINT ( 'NONE',  ( -7.782059566932863603, -29.99999999999999289, 1.004593303788806846 ) ) ;
#40787 = DIRECTION ( 'NONE',  ( 0.000000000000000000, -1.000000000000000000, 0.000000000000000000 ) ) ;
#40788 = PRESENTATION_LAYER_ASSIGNMENT (  '', '', ( #104541 ) ) ;
#40789 =( NAMED_UNIT ( * ) PLANE_ANGLE_UNIT ( ) SI_UNIT ( $, .RADIAN. ) );
#40790 = STYLED_ITEM ( 'NONE', ( #44638 ), #58421 ) ;
#40791 = AXIS2_PLACEMENT_3D ( 'NONE', #70660, #45335, #30215 ) ;
#40792 = CARTESIAN_POINT ( 'NONE',  ( 5.232798140227935768, -1.976627073750571117, 104.1190344879414056 ) ) ;
#40793 = ORIENTED_EDGE ( 'NONE', *, *, #3808, .F. ) ;
#40794 = UNCERTAINTY_MEASURE_WITH_UNIT (LENGTH_MEASURE( 1.000000000000000082E-05 ), #29367, 'distance_accuracy_value', 'NONE');
#40795 = VECTOR ( 'NONE', #43466, 1000.000000000000227 ) ;
#40796 = LINE ( 'NONE', #58592, #89754 ) ;
#40797 = ORIENTED_EDGE ( 'NONE', *, *, #99863, .F. ) ;
#40798 = CARTESIAN_POINT ( 'NONE',  ( 32.90756164719129373, 485.1133553471450455, 5.490574211028886431 ) ) ;
#40799 = CARTESIAN_POINT ( 'NONE',  ( 34.35000000000000142, 1.533819458162526451E-15, 0.000000000000000000 ) ) ;
#40800 = CARTESIAN_POINT ( 'NONE',  ( 9.954785814282153922, 46.18621183893551319, 12.94079623093649190 ) ) ;
#40801 = ORIENTED_EDGE ( 'NONE', *, *, #53219, .T. ) ;
#40802 = ADVANCED_FACE ( 'NONE', ( #79770 ), #31629, .F. ) ;
#40803 = FILL_AREA_STYLE ('',( #7364 ) ) ;
#40804 = CARTESIAN_POINT ( 'NONE',  ( -75.53587094680203506, -59.99999999999879208, 193.5314785434904934 ) ) ;
#40805 = DIRECTION ( 'NONE',  ( -1.000000000000000000, -0.000000000000000000, -0.000000000000000000 ) ) ;
#40806 = CARTESIAN_POINT ( 'NONE',  ( 39.99284958193202755, -59.99999999999998579, 52.04651499647973623 ) ) ;
#40808 = CARTESIAN_POINT ( 'NONE',  ( 14.45045434211625413, -32.51087426405054970, 29.42422261037161846 ) ) ;
#40807 = CARTESIAN_POINT ( 'NONE',  ( -106.5495191435086468, -14.21045842199437992, 161.7519935124221604 ) ) ;
#40809 = CARTESIAN_POINT ( 'NONE',  ( 102.0588018568102342, -38.00000000000000711, 183.9494848540979319 ) ) ;
#40810 = DIRECTION ( 'NONE',  ( -1.000000000000000000, -1.224606353822377258E-16, -0.000000000000000000 ) ) ;
#40811 = EDGE_CURVE ( 'NONE', #17716, #82575, #96162, .T. ) ;
#40812 = CARTESIAN_POINT ( 'NONE',  ( -46.23481718400766027, -29.15784190260456654, 42.24713126758013004 ) ) ;
#40813 = DIRECTION ( 'NONE',  ( 0.000000000000000000, 0.000000000000000000, 1.000000000000000000 ) ) ;
#40814 = VERTEX_POINT ( 'NONE', #46353 ) ;
#40815 = FILL_AREA_STYLE_COLOUR ( '', #42646 ) ;
#40816 = FACE_OUTER_BOUND ( 'NONE', #39662, .T. ) ;
#40817 = CARTESIAN_POINT ( 'NONE',  ( 6.437509419382464237, -11.87447412552789139, 10.48822171390117930 ) ) ;
#40818 = ADVANCED_FACE ( 'NONE', ( #21061 ), #87541, .T. ) ;
#40819 = DIRECTION ( 'NONE',  ( 1.000000000000000000, 0.000000000000000000, 0.000000000000000000 ) ) ;
#40820 = CARTESIAN_POINT ( 'NONE',  ( 6.326445470157509909, 5.253846677262519194, 4.563138989068573181 ) ) ;
#40821 = CARTESIAN_POINT ( 'NONE',  ( 35.76482652855951017, 405.2378813769876729, 6.148826621638260548 ) ) ;
#40823 = ORIENTED_EDGE ( 'NONE', *, *, #81408, .F. ) ;
#40822 = AXIS2_PLACEMENT_3D ( 'NONE', #90828, #97843, #57370 ) ;
#40824 = CARTESIAN_POINT ( 'NONE',  ( 4.844458925424167894, -47.14101111564401236, 103.3760426044467096 ) ) ;
#40825 = ORIENTED_EDGE ( 'NONE', *, *, #38510, .F. ) ;
#40826 = B_SPLINE_CURVE_WITH_KNOTS ( 'NONE', 3,
 ( #101248, #44074, #11680, #44615 ),
 .UNSPECIFIED., .F., .F.,
 ( 4, 4 ),
 ( 4.718958039861916012E-17, 0.001833966606955493919 ),
 .UNSPECIFIED. ) ;
#40827 = CARTESIAN_POINT ( 'NONE',  ( 82.30761750810208355, -30.00000000000000711, 37.47418852386814336 ) ) ;
#40828 = CARTESIAN_POINT ( 'NONE',  ( 48.02835407290544367, 11.61227450977237829, 14.35535821593427386 ) ) ;
#40829 = UNCERTAINTY_MEASURE_WITH_UNIT (LENGTH_MEASURE( 1.000000000000000082E-05 ), #61928, 'distance_accuracy_value', 'NONE');
#40831 = ADVANCED_FACE ( 'NONE', ( #24636 ), #35909, .T. ) ;
#40830 = CARTESIAN_POINT ( 'NONE',  ( 24.00240153465340498, 25.16456132408722723, -32.94378638812468552 ) ) ;
#40832 = CIRCLE ( 'NONE', #94272, 5.000000000000001776 ) ;
#40833 = CARTESIAN_POINT ( 'NONE',  ( 0.000000000000000000, -5.000000000000000000, 0.000000000000000000 ) ) ;
#40834 = CARTESIAN_POINT ( 'NONE',  ( 100.5628734160808193, -30.00000000000000000, 160.0131903483690792 ) ) ;
#40835 = FACE_OUTER_BOUND ( 'NONE', #76517, .T. ) ;
#40836 = VERTEX_POINT ( 'NONE', #98483 ) ;
#40837 = VERTEX_POINT ( 'NONE', #99546 ) ;
#40838 = EDGE_LOOP ( 'NONE', ( #41407, #48614, #59868, #95959 ) ) ;
#40839 = CARTESIAN_POINT ( 'NONE',  ( 0.3194001229792609031, 3.115132258397515397, -7.999999999999996447 ) ) ;
#40840 = CARTESIAN_POINT ( 'NONE',  ( 22.22836149987962528, 25.59762261593713362, 32.73686270175948465 ) ) ;
#40841 = CARTESIAN_POINT ( 'NONE',  ( -39.85359070619685440, 464.8559547511466690, 17.95180902016827318 ) ) ;
#40842 = ORIENTED_EDGE ( 'NONE', *, *, #81339, .T. ) ;
#40843 = CARTESIAN_POINT ( 'NONE',  ( 9.797936955406314041, 108.4667168977048135, -2.012343231877594896 ) ) ;
#40844 = B_SPLINE_CURVE_WITH_KNOTS ( 'NONE', 3,
 ( #106395, #32557, #26081, #91832, #41681, #73496, #1738, #58940, #33610 ),
 .UNSPECIFIED., .F., .F.,
 ( 4, 2, 1, 2, 4 ),
 ( 0.000000000000000000, 0.002165063509461097931, 0.004330127018922195863, 0.006495190528383293360, 0.008660254037844391725 ),
 .UNSPECIFIED. ) ;
#40845 = VERTEX_POINT ( 'NONE', #1367 ) ;
#40846 = DIRECTION ( 'NONE',  ( 1.000000000000000000, 1.224606353822377258E-16, 0.000000000000000000 ) ) ;
#40847 = CARTESIAN_POINT ( 'NONE',  ( 85.20711124866321029, -38.68836316264033570, 198.6075243859919510 ) ) ;
#40848 = DIRECTION ( 'NONE',  ( 1.000000000000000000, 0.000000000000000000, -0.000000000000000000 ) ) ;
#40849 = CARTESIAN_POINT ( 'NONE',  ( 38.19547087256027851, 310.5571834646071920, 5.681190331431579033 ) ) ;
#40850 =( LENGTH_UNIT ( ) NAMED_UNIT ( * ) SI_UNIT ( .MILLI., .METRE. ) );
#40851 = AXIS2_PLACEMENT_3D ( 'NONE', #68087, #36306, #17958 ) ;
#40852 = B_SPLINE_CURVE_WITH_KNOTS ( 'NONE', 3,
 ( #72742, #24764, #39870, #99688, #65197, #56557, #91615, #40921, #25858, #7469, #89483, #65735, #23704, #57612, #74341, #15578, #416, #91089 ),
 .UNSPECIFIED., .F., .F.,
 ( 4, 2, 2, 2, 2, 2, 2, 2, 4 ),
 ( 0.005148306559854647080, 0.006154786515368266056, 0.006658026493125077279, 0.006909646482003485059, 0.007161266470881893706, 0.007664506448638711000, 0.008167746426395530029, 0.008670986404152347324, 0.009174226381909166353 ),
 .UNSPECIFIED. ) ;
#40853 = CARTESIAN_POINT ( 'NONE',  ( 0.000000000000000000, 0.000000000000000000, -2.296599999999999753 ) ) ;
#40854 = CIRCLE ( 'NONE', #13275, 5.000000000000010658 ) ;
#40855 = CARTESIAN_POINT ( 'NONE',  ( -5.000000000000000000, 0.000000000000000000, -8.553285714285713937 ) ) ;
#40856 = CARTESIAN_POINT ( 'NONE',  ( -4.999999999999993783, -46.00000000000000000, 102.2532056551910387 ) ) ;
#40857 = CARTESIAN_POINT ( 'NONE',  ( -1.000000000000000222, -5.000000000000000000, -14.14213562373095101 ) ) ;
#40858 = EDGE_CURVE ( 'NONE', #96476, #35120, #53116, .T. ) ;
#40859 = CARTESIAN_POINT ( 'NONE',  ( -5.252396211958147099, 5.824410605298178112, 4.999999999999999112 ) ) ;
#40860 = ORIENTED_EDGE ( 'NONE', *, *, #31638, .F. ) ;
#40861 = DIRECTION ( 'NONE',  ( 0.000000000000000000, -1.000000000000000000, 0.000000000000000000 ) ) ;
#40863 = CARTESIAN_POINT ( 'NONE',  ( 5.425084639653764640, 41.91238126396859798, -59.10640578674440349 ) ) ;
#40862 = DIRECTION ( 'NONE',  ( 0.000000000000000000, 1.000000000000000000, 0.000000000000000000 ) ) ;
#40864 = DIRECTION ( 'NONE',  ( 1.000000000000000000, 1.224606353822377258E-16, 0.000000000000000000 ) ) ;
#40865 = UNCERTAINTY_MEASURE_WITH_UNIT (LENGTH_MEASURE( 1.000000000000000082E-05 ), #88312, 'distance_accuracy_value', 'NONE');
#40866 = CARTESIAN_POINT ( 'NONE',  ( -1.469576158976823947E-15, -11.37499999999999289, 8.000000000000000000 ) ) ;
#40867 = AXIS2_PLACEMENT_3D ( 'NONE', #48462, #7462, #40379 ) ;
#40869 = DIRECTION ( 'NONE',  ( 0.000000000000000000, 1.000000000000000000, 0.000000000000000000 ) ) ;
#40868 = AXIS2_PLACEMENT_3D ( 'NONE', #70778, #103150, #36333 ) ;
#40870 = EDGE_CURVE ( 'NONE', #16558, #83521, #57483, .T. ) ;
#40871 = EDGE_CURVE ( 'NONE', #12603, #75687, #14181, .T. ) ;
#40872 = CARTESIAN_POINT ( 'NONE',  ( -7.999885325681428405, 101.0002293487006426, 0.2682325777720032667 ) ) ;
#40873 = AXIS2_PLACEMENT_3D ( 'NONE', #17410, #51873, #76685 ) ;
#40874 = AXIS2_PLACEMENT_3D ( 'NONE', #27827, #13167, #87618 ) ;
#40875 = FILL_AREA_STYLE ('',( #96471 ) ) ;
#40876 = VERTEX_POINT ( 'NONE', #26778 ) ;
#40877 = CARTESIAN_POINT ( 'NONE',  ( 84.23537949901131583, -57.43327086003616699, 191.0502212991270596 ) ) ;
#40878 = SURFACE_STYLE_FILL_AREA ( #31748 ) ;
#40879 = ORIENTED_EDGE ( 'NONE', *, *, #8277, .F. ) ;
#40880 = CARTESIAN_POINT ( 'NONE',  ( 94.71819068412230536, -57.66088136610299841, -7.212791323503675578 ) ) ;
#40881 = CARTESIAN_POINT ( 'NONE',  ( 0.000000000000000000, 0.000000000000000000, 0.000000000000000000 ) ) ;
#40882 = CARTESIAN_POINT ( 'NONE',  ( 0.000000000000000000, 1.999999999999998224, -56.32976553137783782 ) ) ;
#40883 = VECTOR ( 'NONE', #39551, 1000.000000000000000 ) ;
#40884 = LINE ( 'NONE', #15538, #73402 ) ;
#40885 = CONICAL_SURFACE ( 'NONE', #13305, 4.000000000000001776, 0.9599310885968774798 ) ;
#40886 = CARTESIAN_POINT ( 'NONE',  ( -81.00479812864165297, -30.00000000000000355, 3.928959509420340002 ) ) ;
#40887 = EDGE_CURVE ( 'NONE', #30899, #88227, #78899, .T. ) ;
#40888 = CARTESIAN_POINT ( 'NONE',  ( 28.52992520858397185, 16.51490304376833151, 41.35306031657900405 ) ) ;
#40889 = CARTESIAN_POINT ( 'NONE',  ( -4.175893272574848325, -4.999999999999998224, 7.137815226409911951 ) ) ;
#40890 = DIRECTION ( 'NONE',  ( 0.000000000000000000, 0.000000000000000000, 1.000000000000000000 ) ) ;
#40892 = DIRECTION ( 'NONE',  ( -1.000000000000000000, -1.224606353822377258E-16, -0.000000000000000000 ) ) ;
#40891 = DIRECTION ( 'NONE',  ( 0.000000000000000000, 1.000000000000000000, 0.000000000000000000 ) ) ;
#40893 = ADVANCED_FACE ( 'NONE', ( #90408 ), #60000, .T. ) ;
#40894 = CONICAL_SURFACE ( 'NONE', #106310, 5.000000000000001776, 0.9599310885968803664 ) ;
#40895 = SURFACE_SIDE_STYLE ('',( #58134 ) ) ;
#40896 = CARTESIAN_POINT ( 'NONE',  ( -29.28883047145525609, 14.13190579697308813, 42.04354307362330445 ) ) ;
#40897 = DIRECTION ( 'NONE',  ( 1.000000000000000000, 0.000000000000000000, 0.000000000000000000 ) ) ;
#40898 = CARTESIAN_POINT ( 'NONE',  ( 10.00000000000027178, 14.99999999999986500, -3.082707893549384792 ) ) ;
#40899 = CARTESIAN_POINT ( 'NONE',  ( 6.400000000000000355, -9.237604307034013473, 7.924929828396943928E-16 ) ) ;
#40900 = EDGE_CURVE ( 'NONE', #25901, #23946, #61762, .T. ) ;
#40901 = CARTESIAN_POINT ( 'NONE',  ( -99.92473045491273353, -37.99999999999996447, 190.7707991670974934 ) ) ;
#40902 = AXIS2_PLACEMENT_3D ( 'NONE', #84198, #35687, #36222 ) ;
#40903 = ORIENTED_EDGE ( 'NONE', *, *, #14925, .F. ) ;
#40904 = CARTESIAN_POINT ( 'NONE',  ( 0.000000000000000000, -4.000000000000003553, 27.00000000000000000 ) ) ;
#40905 = CARTESIAN_POINT ( 'NONE',  ( -7.414580834929599185, 82.35343719718518685, 3.010264818013834276 ) ) ;
#40906 = CARTESIAN_POINT ( 'NONE',  ( 4.472135954999578722, -65.00000000000000000, 4.000000000000002665 ) ) ;
#40908 = CARTESIAN_POINT ( 'NONE',  ( -35.14829367579218200, -47.40882684376428102, -32.39548210165584408 ) ) ;
#40907 = DIRECTION ( 'NONE',  ( 0.000000000000000000, 1.000000000000000000, 0.000000000000000000 ) ) ;
#40909 = EDGE_LOOP ( 'NONE', ( #63316, #71351 ) ) ;
#40910 = VERTEX_POINT ( 'NONE', #18677 ) ;
#40911 = CARTESIAN_POINT ( 'NONE',  ( -26.03675119807346050, 34.91717499005247305, 9.460920673475355258 ) ) ;
#40912 = AXIS2_PLACEMENT_3D ( 'NONE', #3824, #78750, #4883 ) ;
#40913 = CARTESIAN_POINT ( 'NONE',  ( -8.000000000000001776, -29.65625000000000000, 3.313708498984759387 ) ) ;
#40914 = DIRECTION ( 'NONE',  ( 0.000000000000000000, 0.000000000000000000, 1.000000000000000000 ) ) ;
#40915 = CARTESIAN_POINT ( 'NONE',  ( -87.93412205286334427, -60.00000000000001421, -21.65732652878994102 ) ) ;
#40916 = ORIENTED_EDGE ( 'NONE', *, *, #96837, .T. ) ;
#40917 = CARTESIAN_POINT ( 'NONE',  ( 6.201636426617084574E-15, 39.99999999999999289, -70.00365511371767013 ) ) ;
#40918 = CARTESIAN_POINT ( 'NONE',  ( -3.888269695933030512, 294.8076487912955486, -9.230909423689038107 ) ) ;
#40919 = CARTESIAN_POINT ( 'NONE',  ( 97.07153444841249268, -60.35596137945897510, 196.7631902911030295 ) ) ;
#40921 = CARTESIAN_POINT ( 'NONE',  ( -17.88133836625035755, 45.34897204669928072, 5.215214262617849705 ) ) ;
#40920 = SURFACE_STYLE_FILL_AREA ( #73266 ) ;
#40922 = CIRCLE ( 'NONE', #16848, 5.000000000000011546 ) ;
#40923 = ORIENTED_EDGE ( 'NONE', *, *, #76351, .T. ) ;
#40924 = ORIENTED_EDGE ( 'NONE', *, *, #58122, .T. ) ;
#40925 = ORIENTED_EDGE ( 'NONE', *, *, #5226, .F. ) ;
#40926 = CARTESIAN_POINT ( 'NONE',  ( 31.42024293970219162, 416.1390842372517227, 24.31832173542546371 ) ) ;
#40927 = CARTESIAN_POINT ( 'NONE',  ( -5.000000000000001776, -15.62228920881132055, 13.86359191440428873 ) ) ;
#40928 = EDGE_LOOP ( 'NONE', ( #42277, #94814, #64362, #9100, #106709, #104763 ) ) ;
#40929 = EDGE_CURVE ( 'NONE', #91201, #35207, #84060, .T. ) ;
#40930 = DIRECTION ( 'NONE',  ( 0.5735764363510462704, 0.8191520442889915765, 0.000000000000000000 ) ) ;
#40931 = CARTESIAN_POINT ( 'NONE',  ( 0.000000000000000000, 43.22324503868515677, -36.14046114390016839 ) ) ;
#40932 = CARTESIAN_POINT ( 'NONE',  ( 0.000000000000000000, 6.123233995736770227E-16, -5.000000000000002665 ) ) ;
#40933 = CARTESIAN_POINT ( 'NONE',  ( -46.61116709543701120, -57.68144024183414587, 68.72738526911024337 ) ) ;
#40934 = CARTESIAN_POINT ( 'NONE',  ( -2.977408999572654480, -30.12500000204838813, 7.188101187499999156 ) ) ;
#40935 = CARTESIAN_POINT ( 'NONE',  ( -29.68315524076956535, 13.47185074185901499, 42.10535821593508388 ) ) ;
#40936 = FACE_OUTER_BOUND ( 'NONE', #31943, .T. ) ;
#40937 = CIRCLE ( 'NONE', #44418, 5.000000000000010658 ) ;
#40938 = DIRECTION ( 'NONE',  ( 0.000000000000000000, -0.4999999999999998890, 0.8660254037844385966 ) ) ;
#40939 = CARTESIAN_POINT ( 'NONE',  ( -24.89493309229959195, -29.99999999999998934, -38.80368402536839056 ) ) ;
#40940 = EDGE_CURVE ( 'NONE', #103542, #69385, #72074, .T. ) ;
#40941 = CARTESIAN_POINT ( 'NONE',  ( -8.181074200006944963, -14.21045842199423603, 34.35486773805523342 ) ) ;
#40942 = ADVANCED_FACE ( 'NONE', ( #73675 ), #17058, .T. ) ;
#40943 = CARTESIAN_POINT ( 'NONE',  ( -52.90029590074614418, -39.50658224128886786, 55.98782116498496464 ) ) ;
#40944 = CARTESIAN_POINT ( 'NONE',  ( 36.08349330513379982, 1.593028355512270567E-15, 0.000000000000000000 ) ) ;
#40946 = ORIENTED_EDGE ( 'NONE', *, *, #49370, .T. ) ;
#40945 = STYLED_ITEM ( 'NONE', ( #88541 ), #59141 ) ;
#40947 = AXIS2_PLACEMENT_3D ( 'NONE', #41450, #32858, #66258 ) ;
#40948 = CARTESIAN_POINT ( 'NONE',  ( -101.7223263897890035, -60.22553723381597734, 194.4964868810712630 ) ) ;
#40949 = AXIS2_PLACEMENT_3D ( 'NONE', #2095, #93789, #100275 ) ;
#40950 = CARTESIAN_POINT ( 'NONE',  ( -8.269522720489927536, 294.6925646268865080, -5.661848168111208501 ) ) ;
#40951 = CARTESIAN_POINT ( 'NONE',  ( 9.960026500325596999, -3.066375081864128660, 15.24961307665604870 ) ) ;
#40952 = EDGE_LOOP ( 'NONE', ( #74495, #23566 ) ) ;
#40953 = CARTESIAN_POINT ( 'NONE',  ( 55.74444444444444713, -3.309500000000000774, 0.000000000000000000 ) ) ;
#40954 = CARTESIAN_POINT ( 'NONE',  ( 108.8142615268778002, -38.35658623041307180, 190.7462066422830276 ) ) ;
#40955 = CARTESIAN_POINT ( 'NONE',  ( 43.59756234217316972, 434.3244621007173123, 14.55946156040339368 ) ) ;
#40956 = LINE ( 'NONE', #33962, #25051 ) ;
#40958 = EDGE_CURVE ( 'NONE', #103169, #91741, #74734, .T. ) ;
#40957 = CARTESIAN_POINT ( 'NONE',  ( -8.413883161774244002, 294.6898069128530437, 9.902566082097019162 ) ) ;
#40959 = EDGE_CURVE ( 'NONE', #100664, #47749, #106443, .T. ) ;
#40960 = DIRECTION ( 'NONE',  ( 1.000000000000000000, 1.224606353822377258E-16, 0.000000000000000000 ) ) ;
#40962 = CARTESIAN_POINT ( 'NONE',  ( 84.02542197617383124, -29.99999999999999289, 161.2336401493205642 ) ) ;
#40961 = UNCERTAINTY_MEASURE_WITH_UNIT (LENGTH_MEASURE( 1.000000000000000082E-05 ), #24862, 'distance_accuracy_value', 'NONE');
#40963 = CARTESIAN_POINT ( 'NONE',  ( -10.69671229097623666, 43.19294699247078739, -15.34145577127658910 ) ) ;
#40964 = CARTESIAN_POINT ( 'NONE',  ( -28.49081357557760796, 13.12961590422141533, 40.46799408310435808 ) ) ;
#40965 = CARTESIAN_POINT ( 'NONE',  ( 0.7145311798163195283, -4.618802153516994302, 8.000000000000000000 ) ) ;
#40966 = CIRCLE ( 'NONE', #90942, 7.000000000000000000 ) ;
#40967 = ORIENTED_EDGE ( 'NONE', *, *, #100548, .T. ) ;
#40968 = ORIENTED_EDGE ( 'NONE', *, *, #69857, .F. ) ;
#40969 = CARTESIAN_POINT ( 'NONE',  ( 48.85197278088530481, -49.90039430658988096, 52.23959260655022518 ) ) ;
#40970 = CARTESIAN_POINT ( 'NONE',  ( 6.729774171815768646, 41.69338307640796160, -58.98699303515817149 ) ) ;
#40971 = CARTESIAN_POINT ( 'NONE',  ( 36.49735890537233018, 28.04409535384628782, -12.85845504628349012 ) ) ;
#40972 = ORIENTED_EDGE ( 'NONE', *, *, #61183, .T. ) ;
#40973 = CARTESIAN_POINT ( 'NONE',  ( -108.0292185885723200, -38.35629187912161342, 138.0457264600484280 ) ) ;
#40974 = AXIS2_PLACEMENT_3D ( 'NONE', #104760, #88062, #72391 ) ;
#40975 = ORIENTED_EDGE ( 'NONE', *, *, #39322, .T. ) ;
#40976 = CARTESIAN_POINT ( 'NONE',  ( 27.85332533969027580, 34.47293867589335292, -7.792939749169369712 ) ) ;
#40977 = CARTESIAN_POINT ( 'NONE',  ( 92.04294571132990654, -38.35407588941761503, 35.15094813657322703 ) ) ;
#40978 = CARTESIAN_POINT ( 'NONE',  ( 11.60044415005657825, 15.63502551787816408, -9.650786643963554567 ) ) ;
#40979 = CARTESIAN_POINT ( 'NONE',  ( 97.91740595962181715, -37.84853790336257617, 125.6665356466635188 ) ) ;
#40980 = FACE_OUTER_BOUND ( 'NONE', #61162, .T. ) ;
#40981 = CARTESIAN_POINT ( 'NONE',  ( -31.20516925732897917, 314.7589119991607163, -7.638240531729924676 ) ) ;
#40982 = CARTESIAN_POINT ( 'NONE',  ( 1.907980674488920503, -69.56148085505145673, 12.86680972871674911 ) ) ;
#40983 = PRESENTATION_LAYER_ASSIGNMENT (  '', '', ( #87494 ) ) ;
#40984 = CARTESIAN_POINT ( 'NONE',  ( 74.43575368222239774, -60.00000000000000000, 176.5049923845488706 ) ) ;
#40985 = ORIENTED_EDGE ( 'NONE', *, *, #69857, .T. ) ;
#40986 = CARTESIAN_POINT ( 'NONE',  ( 60.30973395284412675, -42.96154581061870203, 74.70304224304538820 ) ) ;
#40987 = CARTESIAN_POINT ( 'NONE',  ( -26.13808921511803618, 304.4947950084629156, -9.641429296246926128 ) ) ;
#40988 = CARTESIAN_POINT ( 'NONE',  ( 9.819569948016248162, -50.41307743780032524, 28.90708029074982477 ) ) ;
#40989 = CARTESIAN_POINT ( 'NONE',  ( 27.61650669486618881, -3.999999999999998224, 0.000000000000000000 ) ) ;
#40990 = B_SPLINE_CURVE_WITH_KNOTS ( 'NONE', 3,
 ( #34364, #67239, #100116, #26282, #46533, #95620, #96156, #54072, #87014, #13084, #22290, #21239, #78363, #54596, #103706, #62731, #45495, #4485 ),
 .UNSPECIFIED., .F., .F.,
 ( 4, 2, 2, 2, 2, 2, 2, 2, 4 ),
 ( 0.007195729052339221166, 0.007698445262548230493, 0.008201161472757238086, 0.008703877682966246546, 0.009206593893175255006, 0.009709310103384263466, 0.01021202631359327193, 0.01071474252380228039, 0.01121745873401128885 ),
 .UNSPECIFIED. ) ;
#40992 = CARTESIAN_POINT ( 'NONE',  ( -4.189032099075284066, 54.25756583020928048, 6.683507376862777072 ) ) ;
#40991 = CARTESIAN_POINT ( 'NONE',  ( -85.26481701026371240, -38.35926911274526674, -22.62496792076730401 ) ) ;
#40993 = AXIS2_PLACEMENT_3D ( 'NONE', #20266, #29404, #4561 ) ;
#40994 = CARTESIAN_POINT ( 'NONE',  ( -41.79440637192924868, 337.1634255704665293, 12.10213894368624743 ) ) ;
#40995 = CARTESIAN_POINT ( 'NONE',  ( -32.82274108734650753, 485.2606360904492817, 5.822976237827062640 ) ) ;
#40996 = DIRECTION ( 'NONE',  ( -1.000000000000000000, -1.224606353822377258E-16, -0.000000000000000000 ) ) ;
#40997 = CARTESIAN_POINT ( 'NONE',  ( 7.999999999999998224, -32.09374999999999289, 3.313708498984766493 ) ) ;
#40998 = FACE_BOUND ( 'NONE', #22270, .T. ) ;
#40999 = CIRCLE ( 'NONE', #54766, 4.000000000000007105 ) ;
#41000 = EDGE_CURVE ( 'NONE', #90863, #49600, #20296, .T. ) ;
#41001 = DIRECTION ( 'NONE',  ( 0.000000000000000000, -1.000000000000000000, 0.000000000000000000 ) ) ;
#41002 = STYLED_ITEM ( 'NONE', ( #39486 ), #210 ) ;
#41003 = ORIENTED_EDGE ( 'NONE', *, *, #73892, .T. ) ;
#41004 = CARTESIAN_POINT ( 'NONE',  ( 85.16083850732167093, -25.44627968698079101, 168.4994044799329629 ) ) ;
#41005 = DIRECTION ( 'NONE',  ( 0.000000000000000000, 1.000000000000000000, 0.000000000000000000 ) ) ;
#41006 = AXIS2_PLACEMENT_3D ( 'NONE', #82537, #35083, #9694 ) ;
#41007 = CARTESIAN_POINT ( 'NONE',  ( -42.21835935851001409, 436.4384481632507118, 19.62208033733219281 ) ) ;
#41008 = ORIENTED_EDGE ( 'NONE', *, *, #84634, .F. ) ;
#41009 = DIRECTION ( 'NONE',  ( 0.000000000000000000, -1.000000000000000000, 0.000000000000000000 ) ) ;
#41010 = CARTESIAN_POINT ( 'NONE',  ( 6.109877454823632092, -4.349879335532680358, -16.82893417409523806 ) ) ;
#41011 = CARTESIAN_POINT ( 'NONE',  ( -32.87547266101657328, 465.6993878536670195, 10.91512469976128585 ) ) ;
#41012 = CARTESIAN_POINT ( 'NONE',  ( -9.609938133586723552, 50.00000000000000000, -92.36043836067815960 ) ) ;
#41013 = CARTESIAN_POINT ( 'NONE',  ( -38.98600622022465245, 42.04669058375750978, -56.90310263554037817 ) ) ;
#41014 = CARTESIAN_POINT ( 'NONE',  ( 43.30868969682389036, 1.340359594676612611E-15, 0.000000000000000000 ) ) ;
#41015 = EDGE_CURVE ( 'NONE', #86477, #12173, #105503, .T. ) ;
#41016 =( NAMED_UNIT ( * ) PLANE_ANGLE_UNIT ( ) SI_UNIT ( $, .RADIAN. ) );
#41017 = AXIS2_PLACEMENT_3D ( 'NONE', #58171, #82987, #24773 ) ;
#41018 = AXIS2_PLACEMENT_3D ( 'NONE', #106460, #97846, #41207 ) ;
#41019 = MECHANICAL_DESIGN_GEOMETRIC_PRESENTATION_REPRESENTATION (  '', ( #104769 ), #11744 ) ;
#41020 = CARTESIAN_POINT ( 'NONE',  ( 6.499999999999999112, -2.759515168581767153, -5.880113447610368027 ) ) ;
#41021 = CARTESIAN_POINT ( 'NONE',  ( -4.999999999999993783, -46.00000000000000000, 102.2532056551910387 ) ) ;
#41023 = CARTESIAN_POINT ( 'NONE',  ( -13.42978829143733499, 24.48114154733749714, 2.381220245303011573 ) ) ;
#41022 = CARTESIAN_POINT ( 'NONE',  ( -12.38234718253561617, -21.30825843599406255, 35.60706586959262410 ) ) ;
#41024 = CARTESIAN_POINT ( 'NONE',  ( -1.320432766682874540E-15, -12.03125000204838635, 7.188101187500000044 ) ) ;
#41025 = CARTESIAN_POINT ( 'NONE',  ( -28.56680886105565165, 18.54011861096317659, -40.29036177351430581 ) ) ;
#41026 = EDGE_CURVE ( 'NONE', #54099, #4842, #82365, .T. ) ;
#41027 = EDGE_LOOP ( 'NONE', ( #90323, #8061, #93492, #22535 ) ) ;
#41028 = EDGE_CURVE ( 'NONE', #4655, #69148, #65120, .T. ) ;
#41029 = ORIENTED_EDGE ( 'NONE', *, *, #80392, .T. ) ;
#41030 = CARTESIAN_POINT ( 'NONE',  ( -17.49999999999716849, 49.96115704434736671, 61.85088014401372902 ) ) ;
#41031 = LINE ( 'NONE', #23279, #59929 ) ;
#41032 = CARTESIAN_POINT ( 'NONE',  ( -8.002730990595935623, 102.9130261956175758, 2.539912827345902235E-12 ) ) ;
#41033 = DIRECTION ( 'NONE',  ( 0.000000000000000000, -0.9971933454386562312, -0.07486943176531225819 ) ) ;
#41035 = CARTESIAN_POINT ( 'NONE',  ( 63.53569133900827381, -34.58942215426228728, -24.20822403974327486 ) ) ;
#41034 = DIRECTION ( 'NONE',  ( 0.000000000000000000, 1.000000000000000000, 0.000000000000000000 ) ) ;
#41036 = ORIENTED_EDGE ( 'NONE', *, *, #61844, .T. ) ;
#41037 = COLOUR_RGB ( '', 0.31764706, 0.68627451, 0.89019608) ;
#41038 = CARTESIAN_POINT ( 'NONE',  ( -4.658465013329192494, -86.32363879673094686, 3.783534922165390668 ) ) ;
#41039 = CARTESIAN_POINT ( 'NONE',  ( -5.290067270632216712, 51.34639538792298907, 8.531152949374556371 ) ) ;
#41040 = VERTEX_POINT ( 'NONE', #53146 ) ;
#41041 = CARTESIAN_POINT ( 'NONE',  ( 0.000000000000000000, 0.000000000000000000, 0.000000000000000000 ) ) ;
#41042 = DIRECTION ( 'NONE',  ( 0.000000000000000000, 0.000000000000000000, 1.000000000000000000 ) ) ;
#41043 = B_SPLINE_CURVE_WITH_KNOTS ( 'NONE', 3,
 ( #41039, #1068, #98721, #16220, #50691, #34578, #66917, #24874, #84157, #58830, #25418, #49650, #91204, #40504, #82006, #16758, #8126, #83608, #8659, #17310, #57730, #73920, #90652, #4, #65841, #100328 ),
 .UNSPECIFIED., .F., .F.,
 ( 4, 2, 2, 2, 2, 2, 2, 2, 2, 2, 2, 2, 4 ),
 ( 0.002882682986932547098, 0.003134830279789356956, 0.003386977572646166813, 0.003891272158359783927, 0.004395566744073401907, 0.004899861329787020756, 0.005152008622643835384, 0.005404155915500650012, 0.005656303208357464640, 0.005908450501214278401, 0.006412745086927905055, 0.006664892379784719684, 0.006917039672641533445 ),
 .UNSPECIFIED. ) ;
#41044 = CARTESIAN_POINT ( 'NONE',  ( -98.11006555757215608, -60.00000000000000000, 69.60638578265736953 ) ) ;
#41045 = CARTESIAN_POINT ( 'NONE',  ( 29.59231420605901519, 13.59660068169548275, -42.10535821593531836 ) ) ;
#41046 = CARTESIAN_POINT ( 'NONE',  ( 1.492654932474820107E-05, -32.51280158588350133, 29.30845022391629229 ) ) ;
#41047 = DIRECTION ( 'NONE',  ( 0.000000000000000000, 0.000000000000000000, -1.000000000000000000 ) ) ;
#41048 = CARTESIAN_POINT ( 'NONE',  ( 39.83349330513380693, 1.593028355512270567E-15, 0.000000000000000000 ) ) ;
#41050 = CARTESIAN_POINT ( 'NONE',  ( 32.00777521468064890, 486.7707349829203736, 6.765100014220078783 ) ) ;
#41049 = CARTESIAN_POINT ( 'NONE',  ( -9.999999999999996447, -5.000000000000002665, -83.69100306252320820 ) ) ;
#41051 = CARTESIAN_POINT ( 'NONE',  ( -85.24946139480805130, -25.41916126808991194, 169.5220700656399231 ) ) ;
#41052 = VERTEX_POINT ( 'NONE', #69860 ) ;
#41053 = ORIENTED_EDGE ( 'NONE', *, *, #8594, .T. ) ;
#41054 = ORIENTED_EDGE ( 'NONE', *, *, #11292, .F. ) ;
#41055 = DIRECTION ( 'NONE',  ( 0.000000000000000000, 0.000000000000000000, 1.000000000000000000 ) ) ;
#41056 =( BOUNDED_SURFACE ( )  B_SPLINE_SURFACE ( 2, 3, ( 
 ( #95723, #3530, #4592, #102753, #86063, #5641, #45064, #96269, #79528, #71424, #78469, #94683, #95202, #29948, #62832, #4060, #21335, #46118, #36989, #22397, #102217, #55240, #12660, #61243, #46631, #20831, #45591, #13187, #70389, #103289, #13723, #79001, #21863, #5122 ),
 ( #88165, #94126, #69859, #54704, #28914, #61789, #87639, #29435, #14249, #38055, #70912, #47154, #86596, #36469, #20295, #53144, #97833, #15854, #48733, #32603, #39092, #71972, #56288, #98875, #89757, #31545, #7749, #7222, #97297, #64940, #80577, #22919, #105913, #96788 ),
 ( #15322, #89225, #74079, #48209, #73542, #81113, #90816, #40659, #23991, #40132, #47678, #82171, #55757, #33129, #57893, #56833, #81626, #14784, #8288, #65475, #88688, #164, #106446, #73009, #98365, #90278, #6697, #41194, #24519, #57358, #16381, #65999, #49268, #25036 ) ),
 .UNSPECIFIED., .F., .T., .F. ) 
 B_SPLINE_SURFACE_WITH_KNOTS ( ( 3, 3 ),
 ( 4, 2, 2, 2, 2, 2, 2, 2, 2, 2, 2, 2, 2, 2, 2, 2, 4 ),
 ( 0.000000000000000000, 1.000000000000000000 ),
 ( -3.141592653589793116, -2.748893571891068976, -2.356194490192344837, -1.963495408493620697, -1.570796326794896558, -1.178097245096172418, -0.7853981633974482790, -0.3926990816987241395, 0.000000000000000000, 0.3926990816987241395, 0.7853981633974482790, 1.178097245096172418, 1.570796326794896558, 1.963495408493620697, 2.356194490192344837, 2.748893571891068976, 3.141592653589793116 ),
 .UNSPECIFIED. ) 
 GEOMETRIC_REPRESENTATION_ITEM ( )  RATIONAL_B_SPLINE_SURFACE ( (
 ( 1.000000000000000000, 1.000000000000000000, 1.000000000000000000, 1.000000000000000000, 1.000000000000000000, 1.000000000000000000, 1.000000000000000000, 1.000000000000000000, 1.000000000000000000, 1.000000000000000000, 1.000000000000000000, 1.000000000000000000, 1.000000000000000000, 1.000000000000000000, 1.000000000000000000, 1.000000000000000000, 1.000000000000000000, 1.000000000000000000, 1.000000000000000000, 1.000000000000000000, 1.000000000000000000, 1.000000000000000000, 1.000000000000000000, 1.000000000000000000, 1.000000000000000000, 1.000000000000000000, 1.000000000000000000, 1.000000000000000000, 1.000000000000000000, 1.000000000000000000, 1.000000000000000000, 1.000000000000000000, 1.000000000000000000, 1.000000000000000000),
 ( 1.857142857142858317, 1.857142857142858317, 1.857142857142858317, 1.857142857142858317, 1.857142857142858317, 1.857142857142858317, 1.857142857142858317, 1.857142857142858317, 1.857142857142858317, 1.857142857142858317, 1.857142857142858317, 1.857142857142858317, 1.857142857142858317, 1.857142857142858317, 1.857142857142858317, 1.857142857142858317, 1.857142857142858317, 1.857142857142858317, 1.857142857142858317, 1.857142857142858317, 1.857142857142858317, 1.857142857142858317, 1.857142857142858317, 1.857142857142858317, 1.857142857142858317, 1.857142857142858317, 1.857142857142858317, 1.857142857142858317, 1.857142857142858317, 1.857142857142858317, 1.857142857142858317, 1.857142857142858317, 1.857142857142858317, 1.857142857142858317),
 ( 1.000000000000000000, 1.000000000000000000, 1.000000000000000000, 1.000000000000000000, 1.000000000000000000, 1.000000000000000000, 1.000000000000000000, 1.000000000000000000, 1.000000000000000000, 1.000000000000000000, 1.000000000000000000, 1.000000000000000000, 1.000000000000000000, 1.000000000000000000, 1.000000000000000000, 1.000000000000000000, 1.000000000000000000, 1.000000000000000000, 1.000000000000000000, 1.000000000000000000, 1.000000000000000000, 1.000000000000000000, 1.000000000000000000, 1.000000000000000000, 1.000000000000000000, 1.000000000000000000, 1.000000000000000000, 1.000000000000000000, 1.000000000000000000, 1.000000000000000000, 1.000000000000000000, 1.000000000000000000, 1.000000000000000000, 1.000000000000000000) ) ) 
 REPRESENTATION_ITEM ( '' )  SURFACE ( )  );
#41057 = CARTESIAN_POINT ( 'NONE',  ( -8.559508646656389885, 51.55638410492942825, -4.031152949374503081 ) ) ;
#41058 = VERTEX_POINT ( 'NONE', #27317 ) ;
#41059 = CARTESIAN_POINT ( 'NONE',  ( 33.86650669486618881, 1.474610560812782335E-15, 0.000000000000000000 ) ) ;
#41060 = CARTESIAN_POINT ( 'NONE',  ( -28.02803974396783815, -57.67115643259209889, -43.15031372974605972 ) ) ;
#41061 = DIRECTION ( 'NONE',  ( 0.000000000000000000, -1.000000000000000000, 0.000000000000000000 ) ) ;
#41062 = CARTESIAN_POINT ( 'NONE',  ( 47.33349330513379982, 4.000000000000003553, 0.000000000000000000 ) ) ;
#41063 = LINE ( 'NONE', #56697, #73841 ) ;
#41064 = CARTESIAN_POINT ( 'NONE',  ( 12.60460666744324776, -5.000000000000000000, -81.60912347660379851 ) ) ;
#41065 = CARTESIAN_POINT ( 'NONE',  ( -44.08840282922865583, 485.7747746244177165, 4.178803824087112595 ) ) ;
#41066 = ADVANCED_FACE ( 'NONE', ( #93607 ), #101314, .T. ) ;
#41067 = AXIS2_PLACEMENT_3D ( 'NONE', #31584, #97338, #66043 ) ;
#41068 = CARTESIAN_POINT ( 'NONE',  ( 106.9596233951320698, -14.21045842199439591, 171.9689152078629775 ) ) ;
#41069 = CARTESIAN_POINT ( 'NONE',  ( -106.8236106313706699, -14.21045842199435150, 178.1018237235793151 ) ) ;
#41070 = CARTESIAN_POINT ( 'NONE',  ( -63.52003477808261778, -25.58132851056570090, 74.89366634491645414 ) ) ;
#41071 = ORIENTED_EDGE ( 'NONE', *, *, #43951, .T. ) ;
#41072 = CARTESIAN_POINT ( 'NONE',  ( -61.88098488124455088, 38.95394723122979030, 15.25653196629931152 ) ) ;
#41073 = CARTESIAN_POINT ( 'NONE',  ( 114.6122575509365760, -60.00000000000000000, 171.8902597099684613 ) ) ;
#41074 = ORIENTED_EDGE ( 'NONE', *, *, #103543, .T. ) ;
#41075 = CARTESIAN_POINT ( 'NONE',  ( 0.9910821173258683725, -25.54837917066274144, 28.14771315471283586 ) ) ;
#41076 = CARTESIAN_POINT ( 'NONE',  ( -5.082755093536325042, -14.46875000204838457, -5.082755093536325930 ) ) ;
#41077 = AXIS2_PLACEMENT_3D ( 'NONE', #96000, #56573, #88962 ) ;
#41078 = ORIENTED_EDGE ( 'NONE', *, *, #54405, .T. ) ;
#41080 = CARTESIAN_POINT ( 'NONE',  ( -80.00000000000000000, -52.00000000000000000, -21.09707704303352926 ) ) ;
#41079 = CIRCLE ( 'NONE', #82424, 7.000000000000006217 ) ;
#41081 = VERTEX_POINT ( 'NONE', #54172 ) ;
#41082 =( LENGTH_UNIT ( ) NAMED_UNIT ( * ) SI_UNIT ( .MILLI., .METRE. ) );
#41083 = CARTESIAN_POINT ( 'NONE',  ( -103.4937426735914272, -59.99999999999997158, 200.3256067693197906 ) ) ;
#41084 = CARTESIAN_POINT ( 'NONE',  ( -3.718188220749848671, -1.049015004457380495, 104.2423402216923876 ) ) ;
#41085 = CARTESIAN_POINT ( 'NONE',  ( -2.977408999572650039, -22.06250000204838813, -7.188101187500001821 ) ) ;
#41086 = DIRECTION ( 'NONE',  ( 0.000000000000000000, 1.000000000000000000, 0.000000000000000000 ) ) ;
#41088 = EDGE_CURVE ( 'NONE', #95530, #84621, #94478, .T. ) ;
#41087 = CARTESIAN_POINT ( 'NONE',  ( -24.44497366060264909, 27.40106161504759186, -32.24452914909054613 ) ) ;
#41089 = CARTESIAN_POINT ( 'NONE',  ( -12.95148853894511731, 19.13138155041741229, 7.909606116934300601 ) ) ;
#41090 = CARTESIAN_POINT ( 'NONE',  ( 13.50000000000000355, 7.794228634059978233, -11.79422863405993382 ) ) ;
#41091 = CARTESIAN_POINT ( 'NONE',  ( -32.15047201613565164, 464.7337454272254718, 11.12330847294773228 ) ) ;
#41092 = EDGE_CURVE ( 'NONE', #1566, #72949, #29068, .T. ) ;
#41093 = CARTESIAN_POINT ( 'NONE',  ( 11.87102759641705063, -7.549635373525221738, 19.57279676713838157 ) ) ;
#41094 = CARTESIAN_POINT ( 'NONE',  ( -23.54757723015235626, 27.32420764371298461, 33.16469143611122661 ) ) ;
#41095 = CARTESIAN_POINT ( 'NONE',  ( 85.71523080318266352, -59.99999999999998579, -14.67970160156688131 ) ) ;
#41096 = B_SPLINE_CURVE_WITH_KNOTS ( 'NONE', 3,
 ( #26319, #75336, #92059, #58092, #48922 ),
 .UNSPECIFIED., .F., .F.,
 ( 4, 1, 4 ),
 ( 0.000000000000000000, 0.003752776749732563560, 0.007505553499465127121 ),
 .UNSPECIFIED. ) ;
#41097 = CARTESIAN_POINT ( 'NONE',  ( -32.59290073874363713, -29.08836541010333221, 32.21693739891244235 ) ) ;
#41098 = CARTESIAN_POINT ( 'NONE',  ( -0.9999999999999941158, -50.00000000000000000, 101.0455488498966758 ) ) ;
#41099 = AXIS2_PLACEMENT_3D ( 'NONE', #46776, #31160, #78600 ) ;
#41100 = CARTESIAN_POINT ( 'NONE',  ( 39.87495318460441496, -32.60419010241520255, 37.08222683619865734 ) ) ;
#41101 = CARTESIAN_POINT ( 'NONE',  ( 0.000000000000000000, 0.000000000000000000, 0.000000000000000000 ) ) ;
#41102 = ORIENTED_EDGE ( 'NONE', *, *, #15064, .F. ) ;
#41103 = CIRCLE ( 'NONE', #84218, 5.000000000000000888 ) ;
#41104 = CARTESIAN_POINT ( 'NONE',  ( -7.002619243997878051, 86.05007318013815620, -3.868708944012997808 ) ) ;
#41105 = CARTESIAN_POINT ( 'NONE',  ( -76.84105350964979664, -38.44307565171133945, 183.5766925144648667 ) ) ;
#41106 = VERTEX_POINT ( 'NONE', #48210 ) ;
#41108 = CARTESIAN_POINT ( 'NONE',  ( 37.51854390953261742, 313.5286481325095451, 14.45587837336505999 ) ) ;
#41107 = CARTESIAN_POINT ( 'NONE',  ( 4.852941176470590534, 11.33333333333377269, -70.80672828634229177 ) ) ;
#41109 = CARTESIAN_POINT ( 'NONE',  ( -12.58006369834112625, 22.88893462671237344, 5.677102170468417697 ) ) ;
#41110 = CARTESIAN_POINT ( 'NONE',  ( -49.26018567526330827, 7.766323692793265288, -15.83099189872090307 ) ) ;
#41111 = CARTESIAN_POINT ( 'NONE',  ( -7.251694485742912200, 41.54830549313345500, -59.82648083153709706 ) ) ;
#41112 = CARTESIAN_POINT ( 'NONE',  ( 6.463647488011505793, 2.646730816809990561, -6.840026438643560525 ) ) ;
#41113 = CARTESIAN_POINT ( 'NONE',  ( -39.99946440396828251, 437.0919103049818091, 5.547728658188754380 ) ) ;
#41114 = DIRECTION ( 'NONE',  ( 0.000000000000000000, 0.000000000000000000, -1.000000000000000000 ) ) ;
#41115 = CARTESIAN_POINT ( 'NONE',  ( 17.26510143360931693, 45.41334515577720055, 6.504361445977895784 ) ) ;
#41116 = CARTESIAN_POINT ( 'NONE',  ( 103.5527963412081078, -59.99999999999997868, 101.8182540185962495 ) ) ;
#41117 = CARTESIAN_POINT ( 'NONE',  ( 0.3167204509598183226, -5.377136764700210847, -6.686525924292708645 ) ) ;
#41118 = FACE_OUTER_BOUND ( 'NONE', #62422, .T. ) ;
#41119 = ORIENTED_EDGE ( 'NONE', *, *, #28937, .T. ) ;
#41120 = AXIS2_PLACEMENT_3D ( 'NONE', #35112, #34587, #67458 ) ;
#41121 = CARTESIAN_POINT ( 'NONE',  ( -97.91052317031356722, -29.99999999999989342, 190.6167072790179020 ) ) ;
#41122 = ORIENTED_EDGE ( 'NONE', *, *, #14037, .F. ) ;
#41123 = CARTESIAN_POINT ( 'NONE',  ( -9.125013381092353271, -54.52764553280017168, 31.09113645985706142 ) ) ;
#41124 = CARTESIAN_POINT ( 'NONE',  ( -15.94091178690226407, 3.082798537041112841, 0.3736180973001349548 ) ) ;
#41125 = CARTESIAN_POINT ( 'NONE',  ( 9.075140000863360257, 137.9474095045275988, 4.999999999999385381 ) ) ;
#41126 = FACE_OUTER_BOUND ( 'NONE', #99414, .T. ) ;
#41127 = CARTESIAN_POINT ( 'NONE',  ( 9.798380800342661345, 26.53199345684497956, -2.010350564680329910 ) ) ;
#41128 = CIRCLE ( 'NONE', #54886, 56.99999999999999289 ) ;
#41129 = CARTESIAN_POINT ( 'NONE',  ( -5.082755093536326818, -26.09375000204838813, 5.082755093536325042 ) ) ;
#41130 = CARTESIAN_POINT ( 'NONE',  ( 9.165151389911679658, 105.0000000000000000, 4.000000000000001776 ) ) ;
#41131 = CARTESIAN_POINT ( 'NONE',  ( 92.82022815836235452, 6.123233995736582872E-16, -5.000000000000011546 ) ) ;
#41132 = EDGE_LOOP ( 'NONE', ( #41660, #104774, #44496, #101073, #12786 ) ) ;
#41133 = EDGE_CURVE ( 'NONE', #67995, #103302, #25584, .T. ) ;
#41134 = VECTOR ( 'NONE', #23959, 1000.000000000000000 ) ;
#41135 =( REPRESENTATION_RELATIONSHIP ('NONE','NONE', #69581, #22031 ) REPRESENTATION_RELATIONSHIP_WITH_TRANSFORMATION ( #71265 )SHAPE_REPRESENTATION_RELATIONSHIP( ) );
#41136 = AXIS2_PLACEMENT_3D ( 'NONE', #28974, #13246, #55297 ) ;
#41138 = EDGE_LOOP ( 'NONE', ( #86473, #88122, #94185, #14861, #14318 ) ) ;
#41137 = PLANE ( 'NONE',  #14974 ) ;
#41139 = CARTESIAN_POINT ( 'NONE',  ( 81.69469107942758512, -39.49696098175696335, 158.0307039208131812 ) ) ;
#41140 = CARTESIAN_POINT ( 'NONE',  ( 9.699121749566359085, 88.17668760275819295, 2.444499528233560426 ) ) ;
#41141 = ORIENTED_EDGE ( 'NONE', *, *, #71742, .F. ) ;
#41142 = CARTESIAN_POINT ( 'NONE',  ( -58.26710234651028486, 50.00000000000000711, 24.08968871770548503 ) ) ;
#41143 = CARTESIAN_POINT ( 'NONE',  ( 7.000000000000000000, 0.000000000000000000, -13.00000000000000000 ) ) ;
#41144 = CARTESIAN_POINT ( 'NONE',  ( -2.977408999572650039, -11.18750000204838457, -7.188101187500000933 ) ) ;
#41145 = CARTESIAN_POINT ( 'NONE',  ( 0.000000000000000000, -38.00000000000000711, 0.000000000000000000 ) ) ;
#41146 = CARTESIAN_POINT ( 'NONE',  ( -54.50637188337720573, -60.00000000000000000, -31.07177919240839259 ) ) ;
#41147 = CARTESIAN_POINT ( 'NONE',  ( 10.61203977153298439, 46.03732009579940865, 12.94024766200776888 ) ) ;
#41148 = PRESENTATION_STYLE_ASSIGNMENT (( #67024 ) ) ;
#41149 = ADVANCED_FACE ( 'NONE', ( #96789 ), #71425, .T. ) ;
#41150 = EDGE_CURVE ( 'NONE', #54423, #80223, #99603, .T. ) ;
#41151 = ORIENTED_EDGE ( 'NONE', *, *, #98962, .T. ) ;
#41152 = CIRCLE ( 'NONE', #25716, 4.000000000000007105 ) ;
#41153 = CARTESIAN_POINT ( 'NONE',  ( 2.869469304594359560, 87.32891902835181952, 5.000000000000000000 ) ) ;
#41154 = CARTESIAN_POINT ( 'NONE',  ( 7.190574343477907249, 41.61619628126704384, -59.53992283653117568 ) ) ;
#41155 = LINE ( 'NONE', #16887, #55059 ) ;
#41156 = CARTESIAN_POINT ( 'NONE',  ( -7.188101187500001821, -29.00000000204838813, -2.977408999572651371 ) ) ;
#41157 = CARTESIAN_POINT ( 'NONE',  ( 22.06473419488195375, -27.05810140444713241, 37.35228815185911344 ) ) ;
#41158 = DIRECTION ( 'NONE',  ( 0.000000000000000000, 0.000000000000000000, 1.000000000000000000 ) ) ;
#41159 = CARTESIAN_POINT ( 'NONE',  ( 2.141486166123602430, -6.269165884987846660, -0.07763482564822672682 ) ) ;
#41160 = EDGE_CURVE ( 'NONE', #59167, #59362, #47679, .T. ) ;
#41161 = CIRCLE ( 'NONE', #25732, 2.999999999999975131 ) ;
#41162 = DIRECTION ( 'NONE',  ( -1.000000000000000000, -1.224606353822377258E-16, -0.000000000000000000 ) ) ;
#41163 = PRODUCT_CONTEXT ( 'NONE', #4599, 'mechanical' ) ;
#41164 = CARTESIAN_POINT ( 'NONE',  ( 49.15082508851322984, 8.572194610415262872, 15.05005620232393859 ) ) ;
#41165 = ORIENTED_EDGE ( 'NONE', *, *, #13122, .T. ) ;
#41166 = CARTESIAN_POINT ( 'NONE',  ( 43.62593301837074478, 434.3202385713651097, 14.43474084663391288 ) ) ;
#41167 = LINE ( 'NONE', #49778, #46293 ) ;
#41168 = CARTESIAN_POINT ( 'NONE',  ( 0.000000000000000000, 0.000000000000000000, 0.000000000000000000 ) ) ;
#41169 = EDGE_CURVE ( 'NONE', #98221, #9982, #97863, .T. ) ;
#41170 = LINE ( 'NONE', #90787, #39410 ) ;
#41171 = ORIENTED_EDGE ( 'NONE', *, *, #67860, .F. ) ;
#41172 = SURFACE_SIDE_STYLE ('',( #76178 ) ) ;
#41173 = CARTESIAN_POINT ( 'NONE',  ( 111.5704048199732199, -57.67092548021626186, 192.6104883897414197 ) ) ;
#41174 = VECTOR ( 'NONE', #49219, 1000.000000000000000 ) ;
#41175 = CARTESIAN_POINT ( 'NONE',  ( 34.38464471054295757, 463.7420058808928616, 19.22113941038953300 ) ) ;
#41176 = CARTESIAN_POINT ( 'NONE',  ( 1.057586783462449942, 13.98593235112240940, 6.924593311009700436 ) ) ;
#41177 = DIRECTION ( 'NONE',  ( 0.000000000000000000, -0.000000000000000000, 1.000000000000000000 ) ) ;
#41178 = PLANE ( 'NONE',  #64973 ) ;
#41179 = CARTESIAN_POINT ( 'NONE',  ( -75.41869077044756864, -60.00000000000000711, 184.0143711039829384 ) ) ;
#41180 = CARTESIAN_POINT ( 'NONE',  ( -40.73878143178837519, 486.4834083601638213, 16.46716573231486436 ) ) ;
#41181 = DIRECTION ( 'NONE',  ( -1.096832036894112098E-16, 0.000000000000000000, -1.000000000000000000 ) ) ;
#41182 = CARTESIAN_POINT ( 'NONE',  ( -36.91281931599076671, 303.7809130842520631, -7.959270006439831846 ) ) ;
#41183 = EDGE_CURVE ( 'NONE', #58745, #42272, #32067, .T. ) ;
#41184 = CARTESIAN_POINT ( 'NONE',  ( -86.20901956646225983, -24.70671085932096389, 181.2931684475793190 ) ) ;
#41185 = ORIENTED_EDGE ( 'NONE', *, *, #48459, .F. ) ;
#41186 = CARTESIAN_POINT ( 'NONE',  ( 27.93171118006010545, 307.0302625388608249, -9.289381728957501139 ) ) ;
#41187 = EDGE_LOOP ( 'NONE', ( #23862, #61589, #105988, #86536, #106087 ) ) ;
#41188 = CARTESIAN_POINT ( 'NONE',  ( -4.966176470918042263, 41.64999999999998437, -70.47555194646970733 ) ) ;
#41189 = CARTESIAN_POINT ( 'NONE',  ( -84.49020180651892531, -45.26885603981717310, -7.230634734441095723 ) ) ;
#41190 = PRESENTATION_LAYER_ASSIGNMENT (  '', '', ( #63616 ) ) ;
#41191 =( NAMED_UNIT ( * ) SI_UNIT ( $, .STERADIAN. ) SOLID_ANGLE_UNIT ( ) );
#41192 = ORIENTED_EDGE ( 'NONE', *, *, #60152, .F. ) ;
#41193 = CARTESIAN_POINT ( 'NONE',  ( 5.929271423532769703, 41.34548894888533965, -58.36914690832966102 ) ) ;
#41194 = CARTESIAN_POINT ( 'NONE',  ( 14.86825985028009001, 0.000000000000000000, 8.569529079650957115 ) ) ;
#41195 = CARTESIAN_POINT ( 'NONE',  ( -36.35757485292756996, 437.5916776841835372, 4.247500867393831925 ) ) ;
#41196 = CARTESIAN_POINT ( 'NONE',  ( -53.63968661800659277, -29.99999999999997158, -34.46705067659466692 ) ) ;
#41197 = CARTESIAN_POINT ( 'NONE',  ( -75.47494900001981932, -46.43776707097643452, 127.8804621272367257 ) ) ;
#41198 = ORIENTED_EDGE ( 'NONE', *, *, #78401, .F. ) ;
#41199 = CARTESIAN_POINT ( 'NONE',  ( 72.58683006904378487, -60.00000000000011369, 181.3898877100950244 ) ) ;
#41200 = CARTESIAN_POINT ( 'NONE',  ( 7.897196874019792645, 88.79127204167808429, -1.302055520192086702 ) ) ;
#41201 = CARTESIAN_POINT ( 'NONE',  ( 114.2218302459193353, -57.67112208883745694, 174.7537043705229109 ) ) ;
#41202 = ORIENTED_EDGE ( 'NONE', *, *, #9058, .T. ) ;
#41203 = DIRECTION ( 'NONE',  ( -1.000000000000000000, -0.000000000000000000, -0.000000000000000000 ) ) ;
#41204 = CIRCLE ( 'NONE', #87727, 1.000000000000000888 ) ;
#41205 = CARTESIAN_POINT ( 'NONE',  ( 32.94330508143927716, 0.000000000000000000, 5.000000000000002665 ) ) ;
#41206 = ORIENTED_EDGE ( 'NONE', *, *, #33654, .T. ) ;
#41207 = DIRECTION ( 'NONE',  ( 0.000000000000000000, -1.000000000000000000, 0.000000000000000000 ) ) ;
#41208 = CARTESIAN_POINT ( 'NONE',  ( 16.64348903516523848, 43.47556584774768851, 6.657797401561421857 ) ) ;
#41209 = CARTESIAN_POINT ( 'NONE',  ( 5.082755093536325930, -21.96875000204838457, -5.082755093536325042 ) ) ;
#41210 = CARTESIAN_POINT ( 'NONE',  ( 1.249327701957322123, -8.410337540183546068, -7.776713651265729332 ) ) ;
#41211 = ADVANCED_FACE ( 'NONE', ( #89226 ), #51394, .T. ) ;
#41212 = CARTESIAN_POINT ( 'NONE',  ( -17.73803972846099697, 45.30907581182017907, -6.035033385463771438 ) ) ;
#41213 = AXIS2_PLACEMENT_3D ( 'NONE', #27525, #43656, #76545 ) ;
#41214 = ORIENTED_EDGE ( 'NONE', *, *, #516, .T. ) ;
#41215 = CARTESIAN_POINT ( 'NONE',  ( -7.200568795987419612, 40.92548677439322091, -70.61799334047601917 ) ) ;
#41217 = CARTESIAN_POINT ( 'NONE',  ( 29.62289515650491722, -36.01063597977103825, 32.38572331401633875 ) ) ;
#41216 =( NAMED_UNIT ( * ) PLANE_ANGLE_UNIT ( ) SI_UNIT ( $, .RADIAN. ) );
#41218 = CARTESIAN_POINT ( 'NONE',  ( 35.44660262691603947, 372.8063709863593544, 5.056757807262998838 ) ) ;
#41219 = EDGE_CURVE ( 'NONE', #58935, #38837, #94065, .T. ) ;
#41220 = ORIENTED_EDGE ( 'NONE', *, *, #16211, .F. ) ;
#41221 = CARTESIAN_POINT ( 'NONE',  ( -0.6254647405162019336, 13.29659006857841952, 51.58631282303937837 ) ) ;
#41222 = AXIS2_PLACEMENT_3D ( 'NONE', #98896, #90835, #704 ) ;
#41223 = EDGE_LOOP ( 'NONE', ( #16651, #43379, #28928 ) ) ;
#41225 = CARTESIAN_POINT ( 'NONE',  ( 0.7861120053659819140, 51.35458432871589451, 9.985568200469458588 ) ) ;
#41224 = CARTESIAN_POINT ( 'NONE',  ( -9.967460206814975296E-16, 0.3912769055735432766, 8.000000000000000000 ) ) ;
#41226 = DIRECTION ( 'NONE',  ( -1.000000000000000000, -1.224606353822377258E-16, -0.000000000000000000 ) ) ;
#41227 = CARTESIAN_POINT ( 'NONE',  ( -11.46347932110838919, 294.5997472607351142, -10.05357601397031786 ) ) ;
#41228 = DIRECTION ( 'NONE',  ( -1.000000000000000000, 0.000000000000000000, 0.000000000000000000 ) ) ;
#41229 = LINE ( 'NONE', #59022, #46600 ) ;
#41230 = CARTESIAN_POINT ( 'NONE',  ( 1.168327726069034345, 14.76361700775325048, -50.96114577899942333 ) ) ;
#41231 = ORIENTED_EDGE ( 'NONE', *, *, #70933, .F. ) ;
#41232 = CIRCLE ( 'NONE', #3361, 14.00000000000000178 ) ;
#41233 = CARTESIAN_POINT ( 'NONE',  ( 89.49579725498631433, -60.00000000000002132, -19.63851451753554045 ) ) ;
#41234 = DIRECTION ( 'NONE',  ( -0.4165977904505313578, 0.000000000000000000, -0.9090909090909089496 ) ) ;
#41235 = CARTESIAN_POINT ( 'NONE',  ( -15.95421105470541967, -2.592376812160994248, 14.77701819664088845 ) ) ;
#41236 = CARTESIAN_POINT ( 'NONE',  ( 0.000000000000000000, 304.8518027762758038, -10.00000000000000355 ) ) ;
#41237 = CARTESIAN_POINT ( 'NONE',  ( 47.77591036386547074, 12.17665806217427971, -14.37301751662952931 ) ) ;
#41238 = ORIENTED_EDGE ( 'NONE', *, *, #47226, .F. ) ;
#41239 = EDGE_CURVE ( 'NONE', #97550, #9120, #27373, .T. ) ;
#41240 = DIRECTION ( 'NONE',  ( -1.000000000000000000, -1.224606353822377258E-16, -0.000000000000000000 ) ) ;
#41241 = ORIENTED_EDGE ( 'NONE', *, *, #71814, .T. ) ;
#41242 = ORIENTED_EDGE ( 'NONE', *, *, #83343, .T. ) ;
#41243 = DIRECTION ( 'NONE',  ( 0.000000000000000000, 0.000000000000000000, -1.000000000000000000 ) ) ;
#41244 = CARTESIAN_POINT ( 'NONE',  ( 45.37589407622110116, 39.17805204455682144, -45.78238044965556952 ) ) ;
#41245 = DIRECTION ( 'NONE',  ( 0.000000000000000000, -1.000000000000000000, 0.000000000000000000 ) ) ;
#41246 = FACE_OUTER_BOUND ( 'NONE', #95041, .T. ) ;
#41247 = CARTESIAN_POINT ( 'NONE',  ( -34.78631043426883451, 321.1559080357926632, -5.542067064983624114 ) ) ;
#41248 = CARTESIAN_POINT ( 'NONE',  ( -5.043559054062717983, -67.66457034734504816, 13.93851206790711039 ) ) ;
#41249 = CARTESIAN_POINT ( 'NONE',  ( 36.87655955837855259, 438.2068510013161813, 3.933030107424693167 ) ) ;
#41250 = CARTESIAN_POINT ( 'NONE',  ( 12.50000000000000711, 39.83843345462788221, -65.33751927206047583 ) ) ;
#41251 = EDGE_LOOP ( 'NONE', ( #47683, #49856, #30101, #93779, #67797, #54717 ) ) ;
#41252 = CARTESIAN_POINT ( 'NONE',  ( 80.97977184163765685, 1.030564683017419500E-14, 0.000000000000000000 ) ) ;
#41253 = ORIENTED_EDGE ( 'NONE', *, *, #50111, .T. ) ;
#41254 = ADVANCED_FACE ( 'NONE', ( #88689 ), #42617, .F. ) ;
#41255 = CARTESIAN_POINT ( 'NONE',  ( 0.000000000000000000, -38.00000000000000711, 0.000000000000000000 ) ) ;
#41256 = CARTESIAN_POINT ( 'NONE',  ( 0.000000000000000000, 44.00000000000000711, 0.000000000000000000 ) ) ;
#41257 = CARTESIAN_POINT ( 'NONE',  ( 3.857142857142853209, -48.79941684889505638, 103.1763305333244176 ) ) ;
#41258 = CIRCLE ( 'NONE', #30894, 6.999999999999999112 ) ;
#41260 = EDGE_LOOP ( 'NONE', ( #54510, #25984, #68188, #18310, #100872, #85028 ) ) ;
#41259 = CARTESIAN_POINT ( 'NONE',  ( -51.99581617557301172, -60.00000000000000000, 61.82981693614253516 ) ) ;
#41261 = CARTESIAN_POINT ( 'NONE',  ( 65.46944084899945437, -22.10224947482613445, 78.54547059327050818 ) ) ;
#41262 = ORIENTED_EDGE ( 'NONE', *, *, #8211, .T. ) ;
#41263 = CARTESIAN_POINT ( 'NONE',  ( 63.67138272020815748, 38.95383793066860534, 8.334564508068442734 ) ) ;
#41264 = CARTESIAN_POINT ( 'NONE',  ( -6.239770560962896617, 10.55575045314059501, 3.176762229947383886 ) ) ;
#41265 = CARTESIAN_POINT ( 'NONE',  ( -93.85239982658497127, -57.67543968518839392, 9.450824874790988872 ) ) ;
#41266 = EDGE_CURVE ( 'NONE', #104544, #62332, #42246, .T. ) ;
#41267 = ORIENTED_EDGE ( 'NONE', *, *, #105739, .F. ) ;
#41268 = VECTOR ( 'NONE', #92527, 1000.000000000000000 ) ;
#41269 =( LENGTH_UNIT ( ) NAMED_UNIT ( * ) SI_UNIT ( .MILLI., .METRE. ) );
#41270 = DIRECTION ( 'NONE',  ( -1.000000000000000000, -0.000000000000000000, -0.000000000000000000 ) ) ;
#41271 = CARTESIAN_POINT ( 'NONE',  ( -35.31256682049455975, 491.0612481437016754, 12.05460915451396176 ) ) ;
#41272 = CYLINDRICAL_SURFACE ( 'NONE', #103210, 4.000000000000000888 ) ;
#41273 = CARTESIAN_POINT ( 'NONE',  ( 8.000000000000000000, -21.68750000409676915, 0.000000000000000000 ) ) ;
#41274 = CARTESIAN_POINT ( 'NONE',  ( -8.000000000000003553, -3.000000000000000000, -2.094395098902523511 ) ) ;
#41275 = DIRECTION ( 'NONE',  ( 0.000000000000000000, 0.000000000000000000, 1.000000000000000000 ) ) ;
#41276 = COLOUR_RGB ( '', 0.72549020, 0.75294118, 0.79215686) ;
#41277 = CARTESIAN_POINT ( 'NONE',  ( -10.52078253383812267, 6.756245462352919340, 0.000000000000000000 ) ) ;
#41278 = CARTESIAN_POINT ( 'NONE',  ( 14.34999999999999787, 1.533819458162526451E-15, 0.000000000000000000 ) ) ;
#41279 = CARTESIAN_POINT ( 'NONE',  ( -16.64348903516517098, -1.200000000000000030E-05, 5.407797401561653672 ) ) ;
#41280 = ORIENTED_EDGE ( 'NONE', *, *, #106484, .T. ) ;
#41281 = DIRECTION ( 'NONE',  ( 0.000000000000000000, -1.000000000000000000, 0.000000000000000000 ) ) ;
#41282 = DIRECTION ( 'NONE',  ( 0.000000000000000000, -1.000000000000000000, 0.000000000000000000 ) ) ;
#41283 = CARTESIAN_POINT ( 'NONE',  ( 30.00000000000000000, 0.000000000000000000, 0.000000000000000000 ) ) ;
#41284 = AXIS2_PLACEMENT_3D ( 'NONE', #27474, #28003, #77579 ) ;
#41285 = CARTESIAN_POINT ( 'NONE',  ( -97.46380090642580285, -30.00000000000000000, 190.9071124952730827 ) ) ;
#41286 = EDGE_CURVE ( 'NONE', #13350, #20962, #4925, .T. ) ;
#41287 = VECTOR ( 'NONE', #50814, 1000.000000000000000 ) ;
#41288 = CARTESIAN_POINT ( 'NONE',  ( 2.088718892540413652, -49.85129056402630709, 44.71921988607925158 ) ) ;
#41289 = CARTESIAN_POINT ( 'NONE',  ( 70.40533769610152603, -57.68249443943340538, 157.3263788805991794 ) ) ;
#41291 = DIRECTION ( 'NONE',  ( 1.000000000000000000, 0.000000000000000000, 1.871721906610600077E-16 ) ) ;
#41290 = DIRECTION ( 'NONE',  ( 0.000000000000000000, 0.4999999999999991673, -0.8660254037844390407 ) ) ;
#41292 = EDGE_CURVE ( 'NONE', #89220, #36994, #8820, .T. ) ;
#41294 = CARTESIAN_POINT ( 'NONE',  ( 10.19526563809554887, -22.67231299545676038, -38.54255160387786106 ) ) ;
#41293 = AXIS2_PLACEMENT_3D ( 'NONE', #63938, #38600, #37562 ) ;
#41295 = CARTESIAN_POINT ( 'NONE',  ( 6.499999999999999112, -3.752776749732586126, -6.064240316920402663 ) ) ;
#41296 = CARTESIAN_POINT ( 'NONE',  ( -46.00000000000000000, 436.1058985003094222, 16.82352493621296219 ) ) ;
#41297 = CARTESIAN_POINT ( 'NONE',  ( -11.58643080058957331, -60.00000000000000000, 39.67679234348616291 ) ) ;
#41298 = CARTESIAN_POINT ( 'NONE',  ( 13.59061921561113984, 7.494096743409553341, 8.374275364764086405 ) ) ;
#41299 = CIRCLE ( 'NONE', #32794, 4.000000000000007105 ) ;
#41300 = CARTESIAN_POINT ( 'NONE',  ( 0.6424216610451950471, 45.36344480451447936, -18.57546480763770802 ) ) ;
#41301 = CARTESIAN_POINT ( 'NONE',  ( -86.81445332370094548, -39.11233341703805877, 188.7329318314524471 ) ) ;
#41302 = EDGE_CURVE ( 'NONE', #22095, #84655, #17012, .T. ) ;
#41303 = VERTEX_POINT ( 'NONE', #41724 ) ;
#41304 = CARTESIAN_POINT ( 'NONE',  ( 19.03324747453112664, 49.57630456594926471, 61.85387798834953088 ) ) ;
#41305 = CARTESIAN_POINT ( 'NONE',  ( 0.000000000000000000, 304.8518027762758038, -9.000000000000005329 ) ) ;
#41306 = CARTESIAN_POINT ( 'NONE',  ( -10.19412816461805349, -32.51289075256729433, 29.31908308346052650 ) ) ;
#41307 = LINE ( 'NONE', #25157, #27341 ) ;
#41309 = CARTESIAN_POINT ( 'NONE',  ( 5.881047590711852457, -64.51600253823789899, 14.29494541094543081 ) ) ;
#41308 = CYLINDRICAL_SURFACE ( 'NONE', #72384, 4.000000000000000888 ) ;
#41310 = ORIENTED_EDGE ( 'NONE', *, *, #56018, .F. ) ;
#41311 = CARTESIAN_POINT ( 'NONE',  ( -8.447961717372509227, -4.999999999999993783, -16.27270454676588329 ) ) ;
#41312 = CARTESIAN_POINT ( 'NONE',  ( -7.414346147792000075, 32.64589157662263830, -3.010818766110528344 ) ) ;
#41313 = CONICAL_SURFACE ( 'NONE', #101624, 4.172000000000001485, 0.9599310885968750373 ) ;
#41314 = CARTESIAN_POINT ( 'NONE',  ( 31.14007908953173853, 298.5476415064817388, -1.182771435588934938 ) ) ;
#41315 = CARTESIAN_POINT ( 'NONE',  ( 10.41054107240687188, 6.123233995736772199E-16, -5.000000000000001776 ) ) ;
#41316 = DIRECTION ( 'NONE',  ( 0.000000000000000000, 1.000000000000000000, 0.000000000000000000 ) ) ;
#41317 = CARTESIAN_POINT ( 'NONE',  ( 107.0562500300223974, -29.99999999999996803, 141.2193814890308374 ) ) ;
#41318 = CARTESIAN_POINT ( 'NONE',  ( -45.43339346675878687, 430.7348383325900727, 7.234598910837349628 ) ) ;
#41319 = B_SPLINE_CURVE_WITH_KNOTS ( 'NONE', 3,
 ( #104561, #29661, #4286, #12888, #71655, #29145, #62015, #95958, #80275, #94910, #72202, #70617, #62531, #54393, #87339, #105106, #81860, #66226, #80813, #17169, #7443, #89978, #47907, #98590 ),
 .UNSPECIFIED., .F., .F.,
 ( 4, 2, 2, 2, 2, 2, 2, 2, 2, 2, 2, 4 ),
 ( 0.003034767923542890881, 0.003287523117834535193, 0.003540278312126179071, 0.003793033506417823383, 0.004045788700709467695, 0.004551299089292751981, 0.004804054283584394125, 0.005056809477876036268, 0.005562319866459323157, 0.006067830255042610046, 0.006573340643625896935, 0.007078851032209183824 ),
 .UNSPECIFIED. ) ;
#41320 = VERTEX_POINT ( 'NONE', #15855 ) ;
#41321 = LINE ( 'NONE', #63496, #15399 ) ;
#41322 = CARTESIAN_POINT ( 'NONE',  ( -9.482945380845308136, 252.4433305877892337, 3.177595346755267336 ) ) ;
#41323 = FACE_OUTER_BOUND ( 'NONE', #14733, .T. ) ;
#41324 = FACE_OUTER_BOUND ( 'NONE', #3973, .T. ) ;
#41325 = CARTESIAN_POINT ( 'NONE',  ( 43.67962081600994395, 397.2354176719359771, 16.03058559300318464 ) ) ;
#41326 = CARTESIAN_POINT ( 'NONE',  ( 7.500000000000000888, -3.000671055698259870, -20.99923901233272971 ) ) ;
#41327 = ORIENTED_EDGE ( 'NONE', *, *, #101306, .T. ) ;
#41328 = CARTESIAN_POINT ( 'NONE',  ( -1.469576158976823947E-15, -21.87499999999999289, 8.000000000000000000 ) ) ;
#41329 = ORIENTED_EDGE ( 'NONE', *, *, #41989, .T. ) ;
#41330 = DIRECTION ( 'NONE',  ( 1.000000000000000000, 1.224606353822377258E-16, 0.000000000000000000 ) ) ;
#41331 = DIRECTION ( 'NONE',  ( 1.000000000000000000, 0.000000000000000000, 0.000000000000000000 ) ) ;
#41332 = CARTESIAN_POINT ( 'NONE',  ( 9.658640570150787141, 45.55801956750498505, 15.25085205539896727 ) ) ;
#41333 = EDGE_LOOP ( 'NONE', ( #69563, #63656, #12038, #61136 ) ) ;
#41334 = ADVANCED_FACE ( 'NONE', ( #58984 ), #76323, .F. ) ;
#41335 = CARTESIAN_POINT ( 'NONE',  ( 51.78317192862468943, 48.00000000000000000, 39.73656039225600978 ) ) ;
#41336 = CARTESIAN_POINT ( 'NONE',  ( 6.158544544230133866, -12.16561743015171970, 11.88011416285994848 ) ) ;
#41337 = MECHANICAL_DESIGN_GEOMETRIC_PRESENTATION_REPRESENTATION (  '', ( #12082 ), #39670 ) ;
#41338 = CARTESIAN_POINT ( 'NONE',  ( -22.10471256930616946, -59.99999999999009503, 42.93026933855558269 ) ) ;
#41339 = CARTESIAN_POINT ( 'NONE',  ( 45.99999999999999289, 436.0048661157462675, 13.49129311716465907 ) ) ;
#41340 = EDGE_LOOP ( 'NONE', ( #105763, #14194 ) ) ;
#41341 = CARTESIAN_POINT ( 'NONE',  ( 96.59781651622874676, -60.00000000000002842, 202.5112741595065131 ) ) ;
#41343 = CARTESIAN_POINT ( 'NONE',  ( 17.52946471254341532, -22.06958086768002403, 27.84760488160436509 ) ) ;
#41342 = CARTESIAN_POINT ( 'NONE',  ( -103.0033221043092482, -14.21045842199434084, 193.8525198385365798 ) ) ;
#41344 = UNCERTAINTY_MEASURE_WITH_UNIT (LENGTH_MEASURE( 1.000000000000000082E-05 ), #34687, 'distance_accuracy_value', 'NONE');
#41346 = ADVANCED_FACE ( 'NONE', ( #33130 ), #91872, .F. ) ;
#41345 = FACE_OUTER_BOUND ( 'NONE', #101055, .T. ) ;
#41347 = VECTOR ( 'NONE', #95301, 1000.000000000000000 ) ;
#41348 = CARTESIAN_POINT ( 'NONE',  ( -43.59263858471909003, -25.70516687255675237, 38.53872847185795791 ) ) ;
#41349 = CARTESIAN_POINT ( 'NONE',  ( 91.37578371391791165, -5.000000000000000000, 0.000000000000000000 ) ) ;
#41350 = EDGE_LOOP ( 'NONE', ( #96137, #91918, #99906, #65183 ) ) ;
#41351 = CARTESIAN_POINT ( 'NONE',  ( -17.49999999999996803, 47.99999999999997868, 64.09949417230998847 ) ) ;
#41352 = CARTESIAN_POINT ( 'NONE',  ( 37.51854390953261742, 313.5286481325095451, 14.45587837336505999 ) ) ;
#41353 = DIRECTION ( 'NONE',  ( 0.000000000000000000, 1.000000000000000000, 0.000000000000000000 ) ) ;
#41354 = CARTESIAN_POINT ( 'NONE',  ( 6.289812543865804351, 6.246946743711088601, 2.837966828325882318 ) ) ;
#41355 = CARTESIAN_POINT ( 'NONE',  ( -32.16069320047662927, 487.8952013991981289, 8.686498104318150837 ) ) ;
#41356 = ORIENTED_EDGE ( 'NONE', *, *, #86875, .T. ) ;
#41357 = CARTESIAN_POINT ( 'NONE',  ( 4.031080902170580238, -48.62189207507206845, 103.0284855429844555 ) ) ;
#41358 = B_SPLINE_CURVE_WITH_KNOTS ( 'NONE', 3,
 ( #73889, #7032, #32404, #31868, #81435, #73347, #7551, #40465, #106245, #32937, #17800, #52266, #18894, #9146, #91687, #1031, #11266, #43652 ),
 .UNSPECIFIED., .F., .F.,
 ( 4, 2, 2, 2, 2, 2, 2, 2, 4 ),
 ( 0.000000000000000000, 0.05410904812296605387, 0.1082180962459321077, 0.1623271443688981686, 0.2164361924918642155, 0.2705452406148303734, 0.3246542887377965036, 0.3787633368607626894, 0.4328723849837288196 ),
 .UNSPECIFIED. ) ;
#41359 = ORIENTED_EDGE ( 'NONE', *, *, #7536, .F. ) ;
#41360 = CARTESIAN_POINT ( 'NONE',  ( 77.04941373716538067, -29.99999999997682920, 175.5720900168622052 ) ) ;
#41361 = CARTESIAN_POINT ( 'NONE',  ( 47.14545574308352371, 12.03700443135207898, 16.50078943917342755 ) ) ;
#41363 = CARTESIAN_POINT ( 'NONE',  ( 37.38561277374697056, 1.340359594676612611E-15, 0.000000000000000000 ) ) ;
#41362 = MECHANICAL_DESIGN_GEOMETRIC_PRESENTATION_REPRESENTATION (  '', ( #31094 ), #68942 ) ;
#41364 = CARTESIAN_POINT ( 'NONE',  ( 58.67238219402268840, 6.975173280561618775E-15, 0.000000000000000000 ) ) ;
#41365 = CARTESIAN_POINT ( 'NONE',  ( 92.38617115133855862, -30.00000000000000355, 102.4331776802988259 ) ) ;
#41366 =( BOUNDED_SURFACE ( )  B_SPLINE_SURFACE ( 3, 2, ( 
 ( #69953, #94777, #4689 ),
 ( #11690, #54262, #20924 ),
 ( #21422, #53238, #87205 ),
 ( #94230, #21952, #12227 ),
 ( #37622, #30040, #62929 ),
 ( #102850, #79094, #54803 ),
 ( #46209, #76967, #77514 ),
 ( #3627, #36561, #69429 ) ),
 .UNSPECIFIED., .F., .F., .F. ) 
 B_SPLINE_SURFACE_WITH_KNOTS ( ( 4, 2, 2, 4 ),
 ( 3, 3 ),
 ( -2.081668171172168513E-17, 0.003573135830214766578, 0.005359703745322160276, 0.007146271660429553974 ),
 ( 0.000000000000000000, 1.000000000000000000 ),
 .UNSPECIFIED. ) 
 GEOMETRIC_REPRESENTATION_ITEM ( )  RATIONAL_B_SPLINE_SURFACE ( (
 ( 1.000000000000000000, 0.7246213771201909237, 1.000000000000000000),
 ( 1.000000000000000000, 0.7303455725924656861, 1.000000000000000000),
 ( 1.000000000000000000, 0.7358045286937978657, 1.000000000000000000),
 ( 1.000000000000000000, 0.7436032658800217909, 1.000000000000000000),
 ( 1.000000000000000000, 0.7461375964764297430, 1.000000000000000000),
 ( 1.000000000000000000, 0.7510703106232340387, 1.000000000000000000),
 ( 1.000000000000000000, 0.7534558991517000814, 1.000000000000000000),
 ( 1.000000000000000000, 0.7557288854865493732, 1.000000000000000000) ) ) 
 REPRESENTATION_ITEM ( '' )  SURFACE ( )  );
#41367 = AXIS2_PLACEMENT_3D ( 'NONE', #66446, #17386, #41114 ) ;
#41368 = CARTESIAN_POINT ( 'NONE',  ( -20.56738711532560160, 303.9076102621805262, 9.948868387141734715 ) ) ;
#41369 = ORIENTED_EDGE ( 'NONE', *, *, #39019, .T. ) ;
#41370 = ADVANCED_FACE ( 'NONE', ( #98876 ), #104850, .T. ) ;
#41371 = AXIS2_PLACEMENT_3D ( 'NONE', #95035, #105229, #79878 ) ;
#41372 = ORIENTED_EDGE ( 'NONE', *, *, #77485, .T. ) ;
#41373 = VERTEX_POINT ( 'NONE', #24520 ) ;
#41374 = CARTESIAN_POINT ( 'NONE',  ( 0.000000000000000000, 48.50000000000000000, 0.000000000000000000 ) ) ;
#41375 = CARTESIAN_POINT ( 'NONE',  ( -7.000000000000003553, -13.84208499319765195, -5.811933785473016201 ) ) ;
#41376 = PRESENTATION_STYLE_ASSIGNMENT (( #97471 ) ) ;
#41377 = CARTESIAN_POINT ( 'NONE',  ( -30.95825898926416286, 357.0936102330114181, 21.51415573308821294 ) ) ;
#41378 =( NAMED_UNIT ( * ) SI_UNIT ( $, .STERADIAN. ) SOLID_ANGLE_UNIT ( ) );
#41379 = EDGE_LOOP ( 'NONE', ( #59973, #50055, #24813, #48002 ) ) ;
#41380 = CARTESIAN_POINT ( 'NONE',  ( 9.989113211954169458, 108.9729927354899530, 0.5334031035448967284 ) ) ;
#41381 = VECTOR ( 'NONE', #99993, 1000.000000000000000 ) ;
#41382 = ORIENTED_EDGE ( 'NONE', *, *, #86266, .F. ) ;
#41383 = CARTESIAN_POINT ( 'NONE',  ( 5.700000000000000178, 0.000000000000000000, 0.000000000000000000 ) ) ;
#41384 = CARTESIAN_POINT ( 'NONE',  ( 78.95220114007015866, -38.68516239071802687, 190.8228697010661676 ) ) ;
#41385 = CARTESIAN_POINT ( 'NONE',  ( 32.13362087237139519, 435.4431350903298039, 16.29023341600430541 ) ) ;
#41386 = CARTESIAN_POINT ( 'NONE',  ( 30.93291330028446851, 298.5973685216983995, 2.766521101297645391 ) ) ;
#41387 = CARTESIAN_POINT ( 'NONE',  ( 38.09999999999999432, -3.309499999999999886, 4.475777889183790779E-16 ) ) ;
#41388 = STYLED_ITEM ( 'NONE', ( #28384 ), #70943 ) ;
#41389 = LINE ( 'NONE', #97481, #11425 ) ;
#41390 = CARTESIAN_POINT ( 'NONE',  ( -40.86877072095277441, 461.0519673121690403, 2.323807444223201291 ) ) ;
#41391 = CARTESIAN_POINT ( 'NONE',  ( -4.999999999999993783, -46.26205164319887331, 102.2532056550983128 ) ) ;
#41392 = FACE_OUTER_BOUND ( 'NONE', #101398, .T. ) ;
#41393 = DIRECTION ( 'NONE',  ( 0.000000000000000000, -1.000000000000000000, 0.000000000000000000 ) ) ;
#41394 = ORIENTED_EDGE ( 'NONE', *, *, #38891, .T. ) ;
#41396 = CARTESIAN_POINT ( 'NONE',  ( -25.24187064870846697, 295.8089182665369776, 10.14309838663142749 ) ) ;
#41395 = PRESENTATION_STYLE_ASSIGNMENT (( #362 ) ) ;
#41397 = SURFACE_STYLE_USAGE ( .BOTH. , #14987 ) ;
#41398 = CARTESIAN_POINT ( 'NONE',  ( -8.000000000000001776, -10.15624999999999112, 3.313708498984758943 ) ) ;
#41399 = CARTESIAN_POINT ( 'NONE',  ( 38.00103629177208120, -36.97174142536137254, 47.25231011079808496 ) ) ;
#41400 = VECTOR ( 'NONE', #18919, 1000.000000000000000 ) ;
#41401 = CARTESIAN_POINT ( 'NONE',  ( 3.040263676388296421, 300.3110236163819877, 9.529558508250175919 ) ) ;
#41402 = PRESENTATION_LAYER_ASSIGNMENT (  '', '', ( #51779 ) ) ;
#41403 = DIRECTION ( 'NONE',  ( -1.000000000000000000, -0.000000000000000000, -0.000000000000000000 ) ) ;
#41404 = CARTESIAN_POINT ( 'NONE',  ( 85.55019892396339287, -42.90932130096805253, 187.2143489094230233 ) ) ;
#41405 = CARTESIAN_POINT ( 'NONE',  ( -7.000000000000000000, 8.572527594031471218E-16, -13.00000000000000000 ) ) ;
#41406 = CARTESIAN_POINT ( 'NONE',  ( -9.609486011791419813, 143.0915023496522736, 2.602085213965210642E-15 ) ) ;
#41407 = ORIENTED_EDGE ( 'NONE', *, *, #29649, .F. ) ;
#41408 = CARTESIAN_POINT ( 'NONE',  ( 91.48635331273750637, -57.66236828961498873, -20.18083513732546663 ) ) ;
#41409 = DIRECTION ( 'NONE',  ( 0.000000000000000000, 0.000000000000000000, 1.000000000000000000 ) ) ;
#41410 = CARTESIAN_POINT ( 'NONE',  ( -80.77853634343884437, -30.00000000000000000, 9.880813862764185274 ) ) ;
#41411 = ADVANCED_FACE ( 'NONE', ( #45460 ), #53654, .T. ) ;
#41412 = ADVANCED_FACE ( 'NONE', ( #64169 ), #25668, .T. ) ;
#41413 = CARTESIAN_POINT ( 'NONE',  ( -80.70597897318361902, -37.99999999999994316, 148.6524463937931841 ) ) ;
#41414 = DIRECTION ( 'NONE',  ( -0.000000000000000000, -0.000000000000000000, -1.000000000000000000 ) ) ;
#41415 = FACE_OUTER_BOUND ( 'NONE', #103710, .T. ) ;
#41416 = EDGE_CURVE ( 'NONE', #87758, #15859, #93850, .T. ) ;
#41418 = CARTESIAN_POINT ( 'NONE',  ( 4.250000000000000000, 0.000000000000000000, -8.028130060628445364 ) ) ;
#41417 = LINE ( 'NONE', #74310, #39697 ) ;
#41419 = EDGE_CURVE ( 'NONE', #38016, #30532, #37678, .T. ) ;
#41420 = DIRECTION ( 'NONE',  ( 0.000000000000000000, 1.000000000000000000, 1.224646799147353207E-16 ) ) ;
#41421 = DIRECTION ( 'NONE',  ( -1.000000000000000000, -1.224606353822377258E-16, -0.000000000000000000 ) ) ;
#41422 = CARTESIAN_POINT ( 'NONE',  ( 91.37578371391791165, 1.016364837396684119E-14, 0.000000000000000000 ) ) ;
#41423 = CARTESIAN_POINT ( 'NONE',  ( -23.21751746555244722, 25.25267828308493634, 33.20617127781060418 ) ) ;
#41424 = DIRECTION ( 'NONE',  ( 0.000000000000000000, 1.000000000000000000, 0.000000000000000000 ) ) ;
#41425 = CIRCLE ( 'NONE', #55195, 3.309500000000007880 ) ;
#41426 = DIRECTION ( 'NONE',  ( 0.000000000000000000, -1.000000000000000000, 0.000000000000000000 ) ) ;
#41428 = EDGE_CURVE ( 'NONE', #88114, #39330, #53200, .T. ) ;
#41427 = VECTOR ( 'NONE', #45641, 1000.000000000000000 ) ;
#41429 = ORIENTED_EDGE ( 'NONE', *, *, #97494, .F. ) ;
#41430 = CARTESIAN_POINT ( 'NONE',  ( -5.942578734303295640, -0.1159328135225491108, 15.36885066084568408 ) ) ;
#41431 = CARTESIAN_POINT ( 'NONE',  ( 0.000000000000000000, 0.000000000000000000, 0.000000000000000000 ) ) ;
#41432 = CARTESIAN_POINT ( 'NONE',  ( -6.928203230275510549, 85.00000000000000000, 4.000000000000000000 ) ) ;
#41433 = CARTESIAN_POINT ( 'NONE',  ( -44.52380092682520285, -26.14798797473085656, -29.30983052058080673 ) ) ;
#41434 = VECTOR ( 'NONE', #103346, 1000.000000000000000 ) ;
#41436 = DIRECTION ( 'NONE',  ( -1.000000000000000000, 0.000000000000000000, 0.000000000000000000 ) ) ;
#41435 = CARTESIAN_POINT ( 'NONE',  ( -8.673617379884035472E-16, 15.58845726811991561, -1.205771365940065953 ) ) ;
#41437 = ORIENTED_EDGE ( 'NONE', *, *, #3115, .T. ) ;
#41438 = CONICAL_SURFACE ( 'NONE', #84574, 8.000000000000000000, 0.9599310885968911355 ) ;
#41439 = CARTESIAN_POINT ( 'NONE',  ( 36.08349330513379982, 4.898587196589405926E-16, -4.000000000000001776 ) ) ;
#41440 = VERTEX_POINT ( 'NONE', #49548 ) ;
#41441 = CARTESIAN_POINT ( 'NONE',  ( -25.97802892056438040, 35.07837490203588970, 8.259914813157596569 ) ) ;
#41442 = AXIS2_PLACEMENT_3D ( 'NONE', #92191, #18344, #58239 ) ;
#41443 = FILL_AREA_STYLE_COLOUR ( '', #18488 ) ;
#41444 = CARTESIAN_POINT ( 'NONE',  ( -35.89949308352697699, -60.00000000000000000, -40.19304179322571713 ) ) ;
#41445 = VERTEX_POINT ( 'NONE', #8558 ) ;
#41446 = DIRECTION ( 'NONE',  ( 0.000000000000000000, 0.000000000000000000, -1.000000000000000000 ) ) ;
#41447 = CARTESIAN_POINT ( 'NONE',  ( 15.50996574327959721, 2.604740765349685461, -0.8136923573247164532 ) ) ;
#41448 = CARTESIAN_POINT ( 'NONE',  ( 100.4700211219143284, -52.75663466979855798, 193.8560308224012374 ) ) ;
#41450 = CARTESIAN_POINT ( 'NONE',  ( 0.000000000000000000, 0.000000000000000000, -2.575493252495433261 ) ) ;
#41449 =( NAMED_UNIT ( * ) PLANE_ANGLE_UNIT ( ) SI_UNIT ( $, .RADIAN. ) );
#41451 = ORIENTED_EDGE ( 'NONE', *, *, #97181, .F. ) ;
#41452 = ORIENTED_EDGE ( 'NONE', *, *, #3109, .T. ) ;
#41453 = EDGE_LOOP ( 'NONE', ( #85243, #8196, #7158, #93076 ) ) ;
#41454 = CARTESIAN_POINT ( 'NONE',  ( 29.85853377316651347, 330.9760585468098952, 16.31649794843299262 ) ) ;
#41455 = CARTESIAN_POINT ( 'NONE',  ( -4.999999999999960920, -12.67914701491841889, 11.71967441880940797 ) ) ;
#41456 = CARTESIAN_POINT ( 'NONE',  ( 16.32471966984386214, 45.71573795642332527, 6.626903219538378131 ) ) ;
#41457 = ORIENTED_EDGE ( 'NONE', *, *, #42170, .F. ) ;
#41458 = EDGE_CURVE ( 'NONE', #73449, #29452, #103157, .T. ) ;
#41459 = FACE_OUTER_BOUND ( 'NONE', #71143, .T. ) ;
#41460 = CARTESIAN_POINT ( 'NONE',  ( -72.28092228780032258, 43.22324503868516388, 36.14046114390016129 ) ) ;
#41461 = CARTESIAN_POINT ( 'NONE',  ( -9.232659125071873696E-16, -6.534749472788166536, -4.681481898396976149 ) ) ;
#41462 = CARTESIAN_POINT ( 'NONE',  ( -62.53353137064869571, -57.67819947725070051, 116.5065130283015975 ) ) ;
#41463 = CARTESIAN_POINT ( 'NONE',  ( -2.977408999572654480, -31.62500000204838813, 7.188101187499999156 ) ) ;
#41464 = CARTESIAN_POINT ( 'NONE',  ( -30.82780881727108735, 15.25261229662382512, 40.33825946679381502 ) ) ;
#41465 = CARTESIAN_POINT ( 'NONE',  ( 66.00571552735603120, 6.975173280561618775E-15, 0.000000000000000000 ) ) ;
#41466 = CARTESIAN_POINT ( 'NONE',  ( 38.85446894546473828, 460.8903912184138676, 2.218456751109172398 ) ) ;
#41467 = CARTESIAN_POINT ( 'NONE',  ( 52.80879785486305167, -14.21045842199441722, -31.95559855168728092 ) ) ;
#41468 = EDGE_CURVE ( 'NONE', #106610, #80639, #90026, .T. ) ;
#41470 = EDGE_CURVE ( 'NONE', #30636, #50065, #49713, .T. ) ;
#41469 = CARTESIAN_POINT ( 'NONE',  ( 0.000000000000000000, 0.000000000000000000, 4.000000000000000888 ) ) ;
#41471 = CARTESIAN_POINT ( 'NONE',  ( -51.80964144195790055, -22.18443608985152338, 47.83208226989306411 ) ) ;
#41472 = AXIS2_PLACEMENT_3D ( 'NONE', #6764, #65005, #22460 ) ;
#41473 = CARTESIAN_POINT ( 'NONE',  ( 4.000000000000000000, 17.85270131633358304, -5.744562646538043715 ) ) ;
#41474 = EDGE_LOOP ( 'NONE', ( #3029, #19061, #94879, #22266 ) ) ;
#41475 = CARTESIAN_POINT ( 'NONE',  ( -98.08353087601894060, -37.72577662167667256, 192.4636628619757630 ) ) ;
#41476 = DIRECTION ( 'NONE',  ( 0.1957247465660570951, 0.4045265792282223827, 0.8933364821160978408 ) ) ;
#41477 = CARTESIAN_POINT ( 'NONE',  ( 15.94101669773376884, -2.916571449501480284, 14.71579249486925889 ) ) ;
#41478 = ORIENTED_EDGE ( 'NONE', *, *, #94304, .F. ) ;
#41479 = CARTESIAN_POINT ( 'NONE',  ( -17.83350561808738988, 43.17460513785992759, 5.799463800283817250 ) ) ;
#41480 = CARTESIAN_POINT ( 'NONE',  ( 104.7235773805048780, -38.39894542868824345, 197.7612429682840229 ) ) ;
#41481 = CARTESIAN_POINT ( 'NONE',  ( 1.960217980381542535E-15, -7.550815748621879209, -6.286450516131066202 ) ) ;
#41482 = DIRECTION ( 'NONE',  ( -0.000000000000000000, -0.000000000000000000, 1.000000000000000000 ) ) ;
#41483 = DIRECTION ( 'NONE',  ( -0.000000000000000000, -0.000000000000000000, -1.000000000000000000 ) ) ;
#41484 = CARTESIAN_POINT ( 'NONE',  ( 85.38339423818332818, -30.00000000000000355, 173.8457401421241002 ) ) ;
#41485 = CARTESIAN_POINT ( 'NONE',  ( 34.34094660030152824, 491.0078558915772078, 12.00869558947917071 ) ) ;
#41486 = CARTESIAN_POINT ( 'NONE',  ( -28.77725283099251641, 13.66028544304341352, 39.99080474963844267 ) ) ;
#41487 = DIRECTION ( 'NONE',  ( -1.000000000000000000, -1.224606353822377258E-16, -0.000000000000000000 ) ) ;
#41488 = EDGE_CURVE ( 'NONE', #20548, #32543, #18281, .T. ) ;
#41489 = AXIS2_PLACEMENT_3D ( 'NONE', #19402, #35033, #27486 ) ;
#41490 = PRESENTATION_LAYER_ASSIGNMENT (  '', '', ( #88007 ) ) ;
#41491 = ORIENTED_EDGE ( 'NONE', *, *, #93302, .T. ) ;
#41492 = ORIENTED_EDGE ( 'NONE', *, *, #36770, .F. ) ;
#41493 = CARTESIAN_POINT ( 'NONE',  ( 52.77684154638642156, -42.97022567233157275, 57.04277442930182929 ) ) ;
#41494 = CARTESIAN_POINT ( 'NONE',  ( 6.674329244388144566, 41.70627487048766113, -58.97405642351494492 ) ) ;
#41495 = CARTESIAN_POINT ( 'NONE',  ( 36.81595939732522282, 27.89094747516896433, -13.21838899458732897 ) ) ;
#41496 = EDGE_CURVE ( 'NONE', #69309, #75237, #98980, .T. ) ;
#41497 = ORIENTED_EDGE ( 'NONE', *, *, #76408, .T. ) ;
#41498 = CARTESIAN_POINT ( 'NONE',  ( -98.66193420133994607, -38.35555159526315805, 80.57390941483606639 ) ) ;
#41499 = ORIENTED_EDGE ( 'NONE', *, *, #37660, .F. ) ;
#41500 = CARTESIAN_POINT ( 'NONE',  ( 14.44581512912309229, 5.963299184987445933, 7.135127315203210863 ) ) ;
#41501 = CARTESIAN_POINT ( 'NONE',  ( 98.48976283628422834, -38.35583645532683050, 79.54628558377670799 ) ) ;
#41502 = CARTESIAN_POINT ( 'NONE',  ( 13.67390614417971939, 22.79767714195904915, -2.033812096035475303 ) ) ;
#41503 = CARTESIAN_POINT ( 'NONE',  ( 88.74246461038792688, -45.28266603850529037, 62.97167601515477031 ) ) ;
#41504 = FILL_AREA_STYLE ('',( #49593 ) ) ;
#41505 = CARTESIAN_POINT ( 'NONE',  ( -1.778928937981819391, -4.332661967047337193, -18.07496135556788985 ) ) ;
#41506 = CARTESIAN_POINT ( 'NONE',  ( -33.85467187920592380, 321.4589499777674177, -5.706254074088779049 ) ) ;
#41507 = DIRECTION ( 'NONE',  ( -1.000000000000000000, -1.224606353822377258E-16, -0.000000000000000000 ) ) ;
#41508 = ADVANCED_FACE ( 'NONE', ( #10155 ), #51673, .F. ) ;
#41509 = CARTESIAN_POINT ( 'NONE',  ( 74.50857564272573086, -60.00000000000000000, 177.1830442982434306 ) ) ;
#41510 = STYLED_ITEM ( 'NONE', ( #51322 ), #81287 ) ;
#41511 = CARTESIAN_POINT ( 'NONE',  ( -43.22728423988735358, 434.6919775797696843, 9.646941480594554363 ) ) ;
#41512 = AXIS2_PLACEMENT_3D ( 'NONE', #64484, #6760, #23507 ) ;
#41513 = ORIENTED_EDGE ( 'NONE', *, *, #57369, .F. ) ;
#41514 = CARTESIAN_POINT ( 'NONE',  ( 63.23442538735326934, -18.63162660745866006, 70.69744974475220545 ) ) ;
#41515 = CARTESIAN_POINT ( 'NONE',  ( -25.38862679093923802, 295.7342021531224532, -1.810452940856004167 ) ) ;
#41516 = DIRECTION ( 'NONE',  ( 0.000000000000000000, 0.000000000000000000, 1.000000000000000000 ) ) ;
#41517 = CARTESIAN_POINT ( 'NONE',  ( -7.474779730927227028, -5.000000000000000888, -15.57446526240806506 ) ) ;
#41518 = CIRCLE ( 'NONE', #67406, 5.000000000000002665 ) ;
#41520 = CARTESIAN_POINT ( 'NONE',  ( -33.22150838192236932, 484.9899766982439360, 0.3198735837378168800 ) ) ;
#41519 = CARTESIAN_POINT ( 'NONE',  ( -51.92511257527466029, -30.00000000004022027, 69.42736369518064521 ) ) ;
#41521 = CARTESIAN_POINT ( 'NONE',  ( -40.87700745978003170, 434.1252800992320431, 26.33294680167561097 ) ) ;
#41522 = CARTESIAN_POINT ( 'NONE',  ( -32.78741055188853437, 485.3331003366707250, 5.977022408746862858 ) ) ;
#41523 = FACE_OUTER_BOUND ( 'NONE', #79462, .T. ) ;
#41524 = CARTESIAN_POINT ( 'NONE',  ( -5.656854249492381470, -28.06249999999999645, 5.656854249492379694 ) ) ;
#41525 = STYLED_ITEM ( 'NONE', ( #78206 ), #19125 ) ;
#41526 = CARTESIAN_POINT ( 'NONE',  ( -43.00000000000000000, 438.4646224975039672, 9.895601460523741011 ) ) ;
#41527 = ORIENTED_EDGE ( 'NONE', *, *, #5690, .T. ) ;
#41528 = CARTESIAN_POINT ( 'NONE',  ( 85.21729610370397268, -28.80435702628989603, 174.9444428549488180 ) ) ;
#41529 = CARTESIAN_POINT ( 'NONE',  ( 44.11330561868255273, 485.7407100969332419, 4.043737255555224230 ) ) ;
#41530 = B_SPLINE_CURVE_WITH_KNOTS ( 'NONE', 3,
 ( #34233, #83802, #91905, #25621, #58483, #34769 ),
 .UNSPECIFIED., .F., .F.,
 ( 4, 2, 4 ),
 ( 2.380733003146920563E-07, 0.001898835937927383956, 0.003797433802554453248 ),
 .UNSPECIFIED. ) ;
#41531 = CARTESIAN_POINT ( 'NONE',  ( -39.08248342308210965, 438.6092072988694213, 22.97679020934365823 ) ) ;
#41532 = ORIENTED_EDGE ( 'NONE', *, *, #5946, .T. ) ;
#41533 = FACE_OUTER_BOUND ( 'NONE', #75716, .T. ) ;
#41534 = CARTESIAN_POINT ( 'NONE',  ( 5.074726305366539236, -4.333190174238139569, -17.09701513331991407 ) ) ;
#41535 = FACE_OUTER_BOUND ( 'NONE', #20352, .T. ) ;
#41536 = CARTESIAN_POINT ( 'NONE',  ( -14.61924042696621306, -3.000000000000002665, -89.34162378225479983 ) ) ;
#41537 = CARTESIAN_POINT ( 'NONE',  ( -43.54105046090145237, 41.43920833560382988, -50.64095212750816444 ) ) ;
#41538 = CARTESIAN_POINT ( 'NONE',  ( -12.16221469084096540, -2.476455199593412537, 20.68589871816672243 ) ) ;
#41539 = EDGE_CURVE ( 'NONE', #44354, #75817, #56544, .T. ) ;
#41540 = SURFACE_STYLE_USAGE ( .BOTH. , #58255 ) ;
#41541 = PRESENTATION_LAYER_ASSIGNMENT (  '', '', ( #7120 ) ) ;
#41542 = CARTESIAN_POINT ( 'NONE',  ( 39.21813245877796561, -60.00000000000002842, 51.03055488639744652 ) ) ;
#41543 = AXIS2_PLACEMENT_3D ( 'NONE', #96547, #94436, #22680 ) ;
#41544 = CARTESIAN_POINT ( 'NONE',  ( 21.84999999999999787, 1.533819458162526451E-15, 0.000000000000000000 ) ) ;
#41545 = CARTESIAN_POINT ( 'NONE',  ( 1.128978779050344716, 25.81467378070274066, 38.95751801069041420 ) ) ;
#41546 = EDGE_CURVE ( 'NONE', #88345, #92559, #84136, .T. ) ;
#41548 = CARTESIAN_POINT ( 'NONE',  ( -15.37715070606341072, 22.74015324434795460, -2.282816646031935459 ) ) ;
#41547 = CARTESIAN_POINT ( 'NONE',  ( -4.718689085033623165, -18.53111709059378143, 35.08043246123458658 ) ) ;
#41549 = ADVANCED_FACE ( 'NONE', ( #100228 ), #58725, .F. ) ;
#41550 = VECTOR ( 'NONE', #29150, 1000.000000000000000 ) ;
#41551 = CARTESIAN_POINT ( 'NONE',  ( 5.082755093536324154, -14.84375000204838457, 5.082755093536326818 ) ) ;
#41552 = CARTESIAN_POINT ( 'NONE',  ( -0.3351512077620020236, -69.52513701336809504, 12.72773188590259252 ) ) ;
#41553 =( NAMED_UNIT ( * ) PLANE_ANGLE_UNIT ( ) SI_UNIT ( $, .RADIAN. ) );
#41554 = ADVANCED_FACE ( 'NONE', ( #52205 ), #97950, .T. ) ;
#41555 = EDGE_LOOP ( 'NONE', ( #66686, #91002, #8907, #80460, #100806 ) ) ;
#41556 = EDGE_CURVE ( 'NONE', #70327, #1352, #50095, .T. ) ;
#41557 = CARTESIAN_POINT ( 'NONE',  ( -19.50000000000008527, 49.99999999999981526, 59.56761335716138461 ) ) ;
#41558 = ADVANCED_FACE ( 'NONE', ( #79673 ), #795, .T. ) ;
#41559 = CARTESIAN_POINT ( 'NONE',  ( 7.500000000000000000, 3.160172554975069215, -7.231829826456838362 ) ) ;
#41560 = CARTESIAN_POINT ( 'NONE',  ( -42.09158233638504498, 465.7816406625409513, 14.79318349170026892 ) ) ;
#41562 = CARTESIAN_POINT ( 'NONE',  ( 24.94155541167982904, -21.77049003089739188, -29.25405592835566537 ) ) ;
#41561 = CARTESIAN_POINT ( 'NONE',  ( 4.506172367774442300, 54.31195234087692825, 6.292759722430547598 ) ) ;
#41563 = VECTOR ( 'NONE', #79051, 1000.000000000000000 ) ;
#41564 = ORIENTED_EDGE ( 'NONE', *, *, #105237, .F. ) ;
#41565 = CARTESIAN_POINT ( 'NONE',  ( -4.813555570991609578, -86.79473796517322626, -3.584128953194789968 ) ) ;
#41566 = LINE ( 'NONE', #33492, #96213 ) ;
#41567 = EDGE_LOOP ( 'NONE', ( #75541, #78279, #104421, #8705, #39436, #47175, #70851 ) ) ;
#41568 = CARTESIAN_POINT ( 'NONE',  ( 0.000000000000000000, 3.500000000000000000, 0.000000000000000000 ) ) ;
#41569 = CARTESIAN_POINT ( 'NONE',  ( 0.000000000000000000, 6.123233995736767268E-16, -5.000000000000000888 ) ) ;
#41570 = CARTESIAN_POINT ( 'NONE',  ( -24.19259889269783415, 41.60565019191297154, -74.04692782006098639 ) ) ;
#41571 = CARTESIAN_POINT ( 'NONE',  ( -95.53324824102833190, -59.99999999999999289, 52.82992578362362934 ) ) ;
#41572 = DIRECTION ( 'NONE',  ( 0.000000000000000000, -0.9238632370065121835, 0.3827227708248480686 ) ) ;
#41573 = DIRECTION ( 'NONE',  ( 0.000000000000000000, -1.000000000000000000, 0.000000000000000000 ) ) ;
#41574 = LINE ( 'NONE', #2160, #72489 ) ;
#41575 = DIRECTION ( 'NONE',  ( 0.000000000000000000, -1.000000000000000000, 0.000000000000000000 ) ) ;
#41577 = CARTESIAN_POINT ( 'NONE',  ( 30.00000000000000355, 490.5636507777060160, 7.413185101891562212 ) ) ;
#41576 = CARTESIAN_POINT ( 'NONE',  ( -6.043427762771305112, -5.000000000000002665, -95.48543666094731464 ) ) ;
#41578 = CARTESIAN_POINT ( 'NONE',  ( -85.83737659453286994, -18.50073294457022044, 163.5530722848842231 ) ) ;
#41579 = ORIENTED_EDGE ( 'NONE', *, *, #47308, .T. ) ;
#41580 = CARTESIAN_POINT ( 'NONE',  ( 7.500000000000005329, 41.41666666666666430, -68.91429205785459544 ) ) ;
#41581 = AXIS2_PLACEMENT_3D ( 'NONE', #74980, #56127, #89067 ) ;
#41582 = VERTEX_POINT ( 'NONE', #88832 ) ;
#41583 = VECTOR ( 'NONE', #57822, 1000.000000000000000 ) ;
#41584 = ORIENTED_EDGE ( 'NONE', *, *, #66113, .T. ) ;
#41585 = FACE_BOUND ( 'NONE', #21615, .T. ) ;
#41586 = LINE ( 'NONE', #91226, #78377 ) ;
#41587 = ORIENTED_EDGE ( 'NONE', *, *, #101515, .T. ) ;
#41588 = B_SPLINE_CURVE_WITH_KNOTS ( 'NONE', 3,
 ( #100126, #66704, #25762, #26293, #92036, #28406, #28957, #94724, #72404, #22827, #15227, #48640, #64332, #36508, #38991, #97202, #89126, #31966, #64845, #23348, #89660, #37030, #97725, #55659, #94175, #77986, #88596, #40041, #88073, #71868, #48113, #55143, #56188, #47055, #4102, #6066, #81012, #69899, #102797, #6598, #61280, #23892, #31450, #104773, #30922, #105825, #81525, #56735, #102257, #39527, #7130, #80480, #72916, #14151, #15759, #63802, #14678, #79955, #105307, #61828, #96689, #47584, #86104, #69375, #22297, #20341, #53187, #12174, #45106, #16833, #74517, #1138, #66434, #51300, #99315, #33040, #34112, #58896, #82624, #75589, #41105, #82076, #106346, #66983, #73987, #24943, #49171, #58346, #26557, #32508, #83152, #100394, #65906, #26037, #57796, #83669, #91266, #25488, #49716, #33559, #59428, #90720, #1689, #69, #17377, #99864, #9248, #65380, #8195, #50760, #42158, #92291, #7649, #42695, #75039, #91787, #17908, #24429, #9778, #34645, #41634, #50251, #16286, #98271, #98786, #67514, #18445, #40566, #8726, #595, #57261, #73448, #90184, #78247, #11913, #44842, #21126, #61022, #36772, #43233, #61558, #27085, #3301, #84752, #20065, #11367, #76117, #28674, #4359, #2213, #51838, #86372, #62096, #45364, #52369, #68030, #77730, #103066, #93909, #69115, #93385, #29222, #94455, #101468, #37295, #43753, #52914, #69637, #85838, #35163, #10833, #20612, #3841, #94988, #84221, #12438, #102530, #53452, #70162, #100923, #10315, #59972, #92832, #36246, #18996, #76645, #2755, #35707, #68585, #27620, #60501, #19532, #85280, #44295, #77190, #101988, #28145, #88473, #97593, #30791, #6464, #22699, #96564, #103586, #79829, #54470, #55536, #87942, #45886, #105178, #80888, #78765, #21637, #56059, #31837, #15093, #22160, #37831, #47457, #72790, #14548, #55010, #31324, #95494, #87419, #80350, #4900, #70695, #6999, #39397, #14024, #46930, #47981, #64719, #39918, #12964, #72275, #64206, #97076, #23220, #30247, #5934, #53955, #88999, #13495, #38861, #46418, #29735, #71727, #62608, #104638, #79304, #63675, #105695, #86891, #5426, #63134, #38350, #71210, #104104, #96034, #16696, #50628, #16155, #9119, #65248, #996, #56608, #98138, #15624, #50120, #57139, #40973, #24290, #74386, #42556, #48516, #99187, #9646, #49043, #42029, #83029, #74911, #8596, #90052, #73316, #41498, #106212, #98661, #81940, #24812, #57663, #58763, #8062, #32905, #90587, #17248, #82495, #67386, #465, #73862, #106757, #33975, #65782, #66847, #89533, #49586, #81407, #99737, #33433, #66307, #25350, #58212, #75457, #7518, #91138, #1552, #25907, #91661, #17775, #83546, #34517, #23759, #40436, #32375, #3717, #10712, #94322, #59833, #3172, #85704, #68987, #18316, #100792, #36647, #101863, #78121, #100267, #28547, #28022, #77599, #10189, #19940, #69511, #27495, #35041, #102397, #43627, #75990, #51708, #45241, #101342, #44710, #51168, #61428, #60371, #84089, #35575, #59295, #11779, #20486, #77057, #52781, #92168, #53324, #36118, #86242, #12316, #2089, #26430, #76518, #4235, #93245, #67905, #37170, #43103, #68448, #26953, #60892, #2628, #93780, #92705, #18865, #84626, #19410, #52243, #85151, #11242, #44170, #53841, #63011, #12839, #104512, #45757, #95909 ),
 .UNSPECIFIED., .F., .F.,
 ( 4, 2, 2, 2, 2, 1, 1, 1, 2, 2, 1, 1, 2, 2, 2, 2, 2, 1, 1, 2, 2, 1, 2, 2, 2, 2, 2, 1, 1, 1, 2, 2, 1, 1, 2, 2, 2, 2, 2, 1, 1, 2, 2, 1, 2, 2, 2, 2, 2, 1, 2, 2, 2, 2, 1, 1, 1, 1, 1, 1, 1, 2, 2, 2, 2, 1, 2, 2, 1, 1, 2, 2, 2, 1, 1, 2, 2, 1, 2, 2, 2, 2, 2, 2, 1, 2, 2, 1, 1, 2, 2, 2, 1, 1, 1, 1, 2, 2, 2, 1, 1, 2, 2, 1, 2, 2, 2, 2, 2, 2, 1, 1, 2, 2, 1, 2, 2, 2, 2, 2, 2, 2, 2, 2, 2, 1, 1, 1, 2, 2, 2, 2, 2, 1, 1, 2, 2, 1, 1, 2, 2, 2, 2, 2, 2, 1, 1, 1, 1, 1, 2, 2, 2, 2, 2, 2, 2, 1, 1, 2, 2, 2, 2, 1, 2, 2, 2, 2, 2, 2, 1, 2, 2, 2, 2, 2, 2, 1, 1, 1, 1, 2, 2, 1, 2, 2, 2, 2, 1, 1, 1, 2, 2, 2, 2, 2, 2, 2, 2, 1, 1, 1, 2, 2, 1, 2, 2, 2, 2, 1, 1, 2, 2, 1, 1, 2, 2, 2, 2, 1, 2, 2, 1, 2, 2, 2, 1, 1, 1, 1, 2, 2, 1, 1, 2, 2, 2, 2, 4 ),
 ( 0.000000000000000000, 0.01562500000017991511, 0.03125000000035977471, 0.06250000000071946615, 0.09375000000107916454, 0.09765625000112419796, 0.09960937500114669385, 0.09985351562614952492, 0.09997558593865092658, 0.1000976562511523282, 0.1005859375011582263, 0.1015625000011698836, 0.1093750000012639056, 0.1250000000014519219, 0.1562500000018279822, 0.1875000000022040703, 0.1953125000022981617, 0.1992187500023451519, 0.1997070312523510360, 0.1999511718773539504, 0.2001953125023568647, 0.2011718750023685776, 0.2031250000023920033, 0.2187500000025786595, 0.2500000000029521385, 0.2812500000033256176, 0.2968750000035121350, 0.2988281250035352832, 0.2998046875035465519, 0.2999267578160477732, 0.2999877929722987169, 0.3000488281285496606, 0.3002929687535534908, 0.3007812500035613734, 0.3046875000036236014, 0.3125000000037479464, 0.3281250000039964698, 0.3437500000042449932, 0.3476562500043071657, 0.3496093750043382520, 0.3498535156293420822, 0.3499755859418440807, 0.3500976562543460235, 0.3505859375043537396, 0.3515625000043693382, 0.3593750000044939052, 0.3613281250045251025, 0.3623046875045407567, 0.3625488281295446424, 0.3627929687545484727, 0.3632812500045560777, 0.3671875000046159743, 0.3710937500046758708, 0.3730468750047058468, 0.3740234375047207793, 0.3745117187547281068, 0.3747558593797318816, 0.3748779296922336579, 0.3749389648484845461, 0.3749694824266098792, 0.3749847412156725457, 0.3749923706102039067, 0.3750000000047352677, 0.3789062500047620241, 0.3808593750047754023, 0.3811035156297769011, 0.3812255859422775672, 0.3812561035204025672, 0.3812866210985276227, 0.3813476562547776227, 0.3818359375047775672, 0.3828125000047774007, 0.3837890625047772342, 0.3842773437547771231, 0.3843383789110271231, 0.3843688964891520676, 0.3843994140672770121, 0.3845214843797769011, 0.3847656250047766235, 0.3867187500047745141, 0.3872070312547740145, 0.3874511718797736815, 0.3876953125047734039, 0.3886718750047721271, 0.3889160156297718496, 0.3890380859422716275, 0.3890686035203966275, 0.3890991210985215720, 0.3891601562547715165, 0.3896484375047711834, 0.3901367187547708504, 0.3903808593797707394, 0.3905029296922706283, 0.3905639648485206283, 0.3905944824266456283, 0.3906097412157081283, 0.3906173706102394338, 0.3906250000047707394, 0.3925781250047735149, 0.3935546875047748472, 0.3936767578172750692, 0.3937377929735251247, 0.3937988281297752358, 0.3940429687547757354, 0.3945312500047768456, 0.3964843750047810644, 0.3984375000047852833, 0.3994140625047873927, 0.3999023437547884474, 0.4000244140672886695, 0.4001464843797889470, 0.4003906250047893911, 0.4023437500047932769, 0.4042968750047971627, 0.4045410156297976623, 0.4046630859422979398, 0.4047851562547982729, 0.4052734375047992721, 0.4062500000048012705, 0.4072265625048032134, 0.4082031250048052118, 0.4091796875048071547, 0.4093017578173074322, 0.4093627929735575433, 0.4093780517626200433, 0.4093933105516825988, 0.4094238281298077653, 0.4096679687548091531, 0.4101562500048119841, 0.4121093750048231419, 0.4140625000048342996, 0.4179687500048566151, 0.4184570312548593907, 0.4187011718798607229, 0.4187316894579859450, 0.4187469482470485560, 0.4187622070361111670, 0.4188232421923611115, 0.4189453125048605564, 0.4199218750048568927, 0.4218750000048491211, 0.4296875000048183679, 0.4335937500048029358, 0.4355468750047952198, 0.4365234375047912785, 0.4370117187547892801, 0.4372558593797882809, 0.4373779296922877258, 0.4374389648485373927, 0.4374694824266622262, 0.4374847412157246707, 0.4375000000047870596, 0.4531250000046511683, 0.4687500000045152770, 0.4726562500044813042, 0.4746093750044643178, 0.4750976562544601545, 0.4755859375044559356, 0.4765625000044472759, 0.4843750000043788861, 0.5000000000042420512, 0.5312500000039681591, 0.5468750000038312686, 0.5488281250038139492, 0.5498046875038054004, 0.5507812500037969627, 0.5546875000037631009, 0.5625000000036955994, 0.6250000000031556979, 0.6875000000026157965, 0.6953125000025484059, 0.6992187500025146552, 0.7031250000024809044, 0.7187500000023461233, 0.7500000000020765611, 0.7812500000018071100, 0.8125000000015376589, 0.8164062500015040191, 0.8183593750014871437, 0.8193359375014788171, 0.8198242187514745982, 0.8199462890639735990, 0.8200683593764725998, 0.8203125000014704904, 0.8281250000014037660, 0.8437500000012704282, 0.8750000000010035306, 0.9062500000007366330, 0.9082031250007198686, 0.9091796875007116530, 0.9096679687507074341, 0.9099121093757054357, 0.9101562500007033263, 0.9140625000006702416, 0.9218750000006040723, 0.9296875000005380141, 0.9375000000004718448, 0.9453125000004056755, 0.9531250000003395062, 0.9541015625003312906, 0.9545898437503270717, 0.9548339843753250733, 0.9549560546878239631, 0.9550170898440735190, 0.9550781250003229639, 0.9570312500003061995, 0.9609375000002724487, 0.9648437500002386980, 0.9658203125002302603, 0.9660644531252281508, 0.9661865234377271516, 0.9662475585939765965, 0.9662628173830389855, 0.9662780761721013745, 0.9663085937502260414, 0.9667968750002211564, 0.9687500000002018385, 0.9707031250001825207, 0.9716796875001727507, 0.9718017578126714184, 0.9718627929689208633, 0.9719238281251701972, 0.9721679687501676437, 0.9726562500001626477, 0.9746093750001423306, 0.9765625000001219025, 0.9770507812501169065, 0.9772949218751143530, 0.9774169921876131317, 0.9774780273438624656, 0.9774932861329248546, 0.9775009155274559935, 0.9775085449219870215, 0.9775390625001119105, 0.9785156250001071365, 0.9804687500000973666, 0.9843750000000778266, 0.9921875000000389688, 1.000000000000000000 ),
 .UNSPECIFIED. ) ;
#41589 = CIRCLE ( 'NONE', #96493, 4.000000000000001776 ) ;
#41590 = DIRECTION ( 'NONE',  ( 0.000000000000000000, 1.000000000000000000, 0.000000000000000000 ) ) ;
#41591 = DIRECTION ( 'NONE',  ( -1.000000000000000000, -1.224606353822377258E-16, -0.000000000000000000 ) ) ;
#41592 = FACE_OUTER_BOUND ( 'NONE', #81239, .T. ) ;
#41593 = DIRECTION ( 'NONE',  ( -1.000000000000000000, -1.224606353822377258E-16, -0.000000000000000000 ) ) ;
#41594 = CARTESIAN_POINT ( 'NONE',  ( 46.08349330513379982, 1.593028355512270567E-15, 0.000000000000000000 ) ) ;
#41595 = DIRECTION ( 'NONE',  ( 0.000000000000000000, 1.000000000000000000, 0.000000000000000000 ) ) ;
#41596 = CARTESIAN_POINT ( 'NONE',  ( -43.18011688719700913, 485.8502513091206083, 5.262111696809587791 ) ) ;
#41597 = AXIS2_PLACEMENT_3D ( 'NONE', #11197, #61386, #101304 ) ;
#41598 = CARTESIAN_POINT ( 'NONE',  ( 109.0466504562702141, -30.00000000000000355, 159.8086616330221830 ) ) ;
#41599 = ADVANCED_FACE ( 'NONE', ( #15462 ), #79793, .F. ) ;
#41600 = CONICAL_SURFACE ( 'NONE', #53695, 4.172000000000001485, 0.9599310885968750373 ) ;
#41601 = CARTESIAN_POINT ( 'NONE',  ( -106.9108898249343156, -14.21045842199431242, 176.0583478801969193 ) ) ;
#41602 = CARTESIAN_POINT ( 'NONE',  ( -62.44653457475159541, -42.96348183423683054, 80.59091618468615081 ) ) ;
#41603 = VERTEX_POINT ( 'NONE', #35415 ) ;
#41604 = CARTESIAN_POINT ( 'NONE',  ( -2.897774986000545283, 38.95261239556568000, 63.66823351328071112 ) ) ;
#41605 = CARTESIAN_POINT ( 'NONE',  ( 106.2951369877889221, -59.99999999999133848, 201.2543869268758101 ) ) ;
#41606 = EDGE_LOOP ( 'NONE', ( #97772, #85, #95334, #20039 ) ) ;
#41607 = CARTESIAN_POINT ( 'NONE',  ( 2.979342351834940228, -22.06717662120162871, 27.56309061281193706 ) ) ;
#41608 = CARTESIAN_POINT ( 'NONE',  ( -104.9289101731156961, -60.15511913292260004, 149.1721339770082295 ) ) ;
#41609 = CARTESIAN_POINT ( 'NONE',  ( 5.082755093536325930, -16.34375000204838813, -5.082755093536325042 ) ) ;
#41610 = CARTESIAN_POINT ( 'NONE',  ( -13.50000000000000178, -5.228219631169439552, -0.5328967677612923559 ) ) ;
#41611 = ORIENTED_EDGE ( 'NONE', *, *, #36061, .T. ) ;
#41612 = CARTESIAN_POINT ( 'NONE',  ( 37.06956559601371737, 463.9941799042751427, 19.59960652757460409 ) ) ;
#41613 = ORIENTED_EDGE ( 'NONE', *, *, #42155, .F. ) ;
#41614 = CARTESIAN_POINT ( 'NONE',  ( 0.000000000000000000, 0.000000000000000000, 24.55262289886175964 ) ) ;
#41615 = CARTESIAN_POINT ( 'NONE',  ( -35.19798225690215787, -60.00000000000001421, 46.55359730984257283 ) ) ;
#41616 = CARTESIAN_POINT ( 'NONE',  ( 10.00250692948970865, -58.00047262059107567, 26.86088010484640165 ) ) ;
#41617 = CARTESIAN_POINT ( 'NONE',  ( 5.082755093536325930, -19.34375000204838457, -5.082755093536325042 ) ) ;
#41618 = CARTESIAN_POINT ( 'NONE',  ( 89.99999999999997158, -38.00000000001091394, 196.0238439516549818 ) ) ;
#41619 = SURFACE_SIDE_STYLE ('',( #34097 ) ) ;
#41620 = CARTESIAN_POINT ( 'NONE',  ( 12.81923949848201971, -0.000000000000000000, 11.24494283604525080 ) ) ;
#41621 = CYLINDRICAL_SURFACE ( 'NONE', #92533, 4.000000000000000000 ) ;
#41622 = CARTESIAN_POINT ( 'NONE',  ( 32.15969615473760257, 464.7082453577105525, 10.94011554326026037 ) ) ;
#41623 = DIRECTION ( 'NONE',  ( -1.000000000000000000, -0.000000000000000000, -0.000000000000000000 ) ) ;
#41624 = CARTESIAN_POINT ( 'NONE',  ( -23.62741386766555962, 27.31466638971095406, 33.14007574073351492 ) ) ;
#41625 = CARTESIAN_POINT ( 'NONE',  ( 86.19989974210415085, -60.00000000000000711, 6.707520835489996003 ) ) ;
#41626 = CARTESIAN_POINT ( 'NONE',  ( -32.55836021993020779, -39.49469638261044935, 34.14499934634533673 ) ) ;
#41627 = AXIS2_PLACEMENT_3D ( 'NONE', #48606, #90146, #39489 ) ;
#41628 = SURFACE_SIDE_STYLE ('',( #65373 ) ) ;
#41629 = CARTESIAN_POINT ( 'NONE',  ( 42.02483648120990978, -36.06897935197377336, 39.65630586122958334 ) ) ;
#41630 = FACE_OUTER_BOUND ( 'NONE', #71935, .T. ) ;
#41631 = ORIENTED_EDGE ( 'NONE', *, *, #92924, .T. ) ;
#41632 = CARTESIAN_POINT ( 'NONE',  ( 43.28401190480957439, 435.3393147692861476, 9.722488360065341340 ) ) ;
#41633 =( GEOMETRIC_REPRESENTATION_CONTEXT ( 3 ) GLOBAL_UNCERTAINTY_ASSIGNED_CONTEXT ( ( #15960 ) ) GLOBAL_UNIT_ASSIGNED_CONTEXT ( ( #96358, #23006, #97921 ) ) REPRESENTATION_CONTEXT ( 'NONE', 'WORKASPACE' ) );
#41634 = CARTESIAN_POINT ( 'NONE',  ( -81.53445610154220446, -38.84159544557321908, 195.3185924584556687 ) ) ;
#41635 = ORIENTED_EDGE ( 'NONE', *, *, #1210, .F. ) ;
#41637 = CARTESIAN_POINT ( 'NONE',  ( 40.88293604215247967, 432.5779639752643675, 26.56799667982232549 ) ) ;
#41636 = DIRECTION ( 'NONE',  ( 0.000000000000000000, 1.000000000000000000, 0.000000000000000000 ) ) ;
#41638 = CARTESIAN_POINT ( 'NONE',  ( 78.44240119052240345, -60.00000000000003553, 159.1745854876873238 ) ) ;
#41639 = CARTESIAN_POINT ( 'NONE',  ( 16.12754063828955609, 36.56084451123473400, 24.14283378817819070 ) ) ;
#41640 = CARTESIAN_POINT ( 'NONE',  ( 5.980097492742490140, -2.767486787162143802, 6.499999999999999112 ) ) ;
#41641 = CARTESIAN_POINT ( 'NONE',  ( 37.87043015219848030, 460.2235823560122867, 2.222860475111648970 ) ) ;
#41642 = CARTESIAN_POINT ( 'NONE',  ( -38.18937913013400731, 25.28116514224970146, 13.30224098674663580 ) ) ;
#41643 = CARTESIAN_POINT ( 'NONE',  ( 5.999787407977321685, -88.99968111184452368, 0.2740427891043037412 ) ) ;
#41644 = DIRECTION ( 'NONE',  ( 0.9730146112118936985, 0.000000000000000000, -0.2307435077486851283 ) ) ;
#41645 = EDGE_CURVE ( 'NONE', #26618, #74653, #98984, .T. ) ;
#41646 = CARTESIAN_POINT ( 'NONE',  ( 109.4407305757422222, -60.00000000000002132, 139.1494640894100030 ) ) ;
#41647 = CARTESIAN_POINT ( 'NONE',  ( -3.848469685774049243, -52.98046562515381197, 40.46677497459211992 ) ) ;
#41648 = CARTESIAN_POINT ( 'NONE',  ( 9.999999999999998224, 15.00000000000000000, -1.734723475976806897E-15 ) ) ;
#41649 = VERTEX_POINT ( 'NONE', #58599 ) ;
#41650 = CARTESIAN_POINT ( 'NONE',  ( -94.96020567939359580, -29.99999999999991473, 191.3500368583484885 ) ) ;
#41651 = ORIENTED_EDGE ( 'NONE', *, *, #1046, .F. ) ;
#41652 = CARTESIAN_POINT ( 'NONE',  ( 26.16506696227845552, 37.17214248418269307, -7.978832041202565506 ) ) ;
#41653 = CARTESIAN_POINT ( 'NONE',  ( 43.51233770555737124, 462.0554640178511931, 4.320559117861924037 ) ) ;
#41654 = CARTESIAN_POINT ( 'NONE',  ( 4.651269564039822946, -4.999999999999991118, -15.66707428873065311 ) ) ;
#41655 = CARTESIAN_POINT ( 'NONE',  ( -22.43989698835522262, 28.20716416251315195, -30.97385700653319773 ) ) ;
#41656 = CARTESIAN_POINT ( 'NONE',  ( 5.082755093536324154, -16.71875000204838813, 5.082755093536326818 ) ) ;
#41657 = CARTESIAN_POINT ( 'NONE',  ( 16.58710573300756508, 37.15623819652538629, -21.80698433968624528 ) ) ;
#41658 = PRODUCT_RELATED_PRODUCT_CATEGORY ( 'part', '', ( #101508 ) ) ;
#41660 = ORIENTED_EDGE ( 'NONE', *, *, #70621, .T. ) ;
#41659 = CARTESIAN_POINT ( 'NONE',  ( -41.49039443806330496, 469.1026463824607617, 1.097952796331059799 ) ) ;
#41661 = CARTESIAN_POINT ( 'NONE',  ( 81.51636251900598040, -49.93621807469046558, 172.6898897633368222 ) ) ;
#41662 = CIRCLE ( 'NONE', #38009, 10.00000000000000178 ) ;
#41663 = CARTESIAN_POINT ( 'NONE',  ( 9.948181520647857212, 88.86892802760380050, 1.049088206181487459 ) ) ;
#41664 = ORIENTED_EDGE ( 'NONE', *, *, #4403, .F. ) ;
#41665 = VECTOR ( 'NONE', #96732, 1000.000000000000227 ) ;
#41666 = CYLINDRICAL_SURFACE ( 'NONE', #44505, 2.000000000000001776 ) ;
#41667 = CARTESIAN_POINT ( 'NONE',  ( -47.14730021652961511, 17.20087926883181240, 16.50246546963050776 ) ) ;
#41668 = CARTESIAN_POINT ( 'NONE',  ( 38.32995719435926674, 27.37220640332429511, -13.21005651354133015 ) ) ;
#41669 = CYLINDRICAL_SURFACE ( 'NONE', #14078, 4.000000000000000000 ) ;
#41670 = TOROIDAL_SURFACE ( 'NONE', #89864, 11.18527996897366528, 1.000000000000000000 ) ;
#41671 = CARTESIAN_POINT ( 'NONE',  ( 33.77031889322872615, -60.00000000000001421, -34.68851707423049646 ) ) ;
#41672 = CARTESIAN_POINT ( 'NONE',  ( -32.28733632729606740, 338.4947552595653519, 18.46383803629149867 ) ) ;
#41673 = CARTESIAN_POINT ( 'NONE',  ( -32.70896709465985452, 434.6719836098827159, 17.16937924263439541 ) ) ;
#41674 = ORIENTED_EDGE ( 'NONE', *, *, #58086, .T. ) ;
#41675 = EDGE_CURVE ( 'NONE', #76319, #11128, #64529, .T. ) ;
#41676 = CARTESIAN_POINT ( 'NONE',  ( -1.128077836147719282, 302.8478239976500390, 9.936168295454388399 ) ) ;
#41677 = CARTESIAN_POINT ( 'NONE',  ( -5.656854249492379694, -19.43749999999999289, -5.656854249492380582 ) ) ;
#41678 = CARTESIAN_POINT ( 'NONE',  ( 86.85191061701388548, -31.73550785420024312, 186.9884310306377699 ) ) ;
#41679 = EDGE_CURVE ( 'NONE', #104099, #72660, #85227, .T. ) ;
#41680 = VECTOR ( 'NONE', #2009, 1000.000000000000000 ) ;
#41681 = CARTESIAN_POINT ( 'NONE',  ( -3.750000000000002665, 6.495190528383289141, -6.991905250253755533 ) ) ;
#41682 = CARTESIAN_POINT ( 'NONE',  ( 5.082755093536324154, -32.84375000204838813, 5.082755093536326818 ) ) ;
#41683 = DIRECTION ( 'NONE',  ( 0.000000000000000000, 0.000000000000000000, -1.000000000000000000 ) ) ;
#41684 = CARTESIAN_POINT ( 'NONE',  ( 7.338420317991889874, 52.18300848749867527, 2.465250910119829442 ) ) ;
#41685 = DIRECTION ( 'NONE',  ( 0.000000000000000000, 0.000000000000000000, 1.000000000000000000 ) ) ;
#41686 = ITEM_DEFINED_TRANSFORMATION ( 'NONE', 'NONE', #86908,  #10728 ) ;
#41687 = CARTESIAN_POINT ( 'NONE',  ( 48.26727629737668934, 11.05468605157633455, 14.37283805632272404 ) ) ;
#41688 = ORIENTED_EDGE ( 'NONE', *, *, #8544, .F. ) ;
#41689 = CARTESIAN_POINT ( 'NONE',  ( 43.59756234217316972, 434.3244621007173123, 14.55946156040339368 ) ) ;
#41690 = EDGE_CURVE ( 'NONE', #90250, #12821, #75831, .T. ) ;
#41691 = LINE ( 'NONE', #65965, #3247 ) ;
#41692 = DIRECTION ( 'NONE',  ( -8.400342417351198358E-11, -1.000000000000000000, 0.000000000000000000 ) ) ;
#41693 =( BOUNDED_SURFACE ( )  B_SPLINE_SURFACE ( 3, 2, ( 
 ( #30336, #80443, #97160 ),
 ( #6552, #7608, #88032 ),
 ( #72361, #65337, #71826 ),
 ( #23308, #79917, #89087 ),
 ( #6025, #31927, #40527 ),
 ( #14638, #89619, #15717 ) ),
 .UNSPECIFIED., .F., .F., .F. ) 
 B_SPLINE_SURFACE_WITH_KNOTS ( ( 4, 2, 4 ),
 ( 3, 3 ),
 ( -1.626303258728256651E-18, 0.001801542390204181844, 0.003603084780408365422 ),
 ( 0.000000000000000000, 1.000000000000000000 ),
 .UNSPECIFIED. ) 
 GEOMETRIC_REPRESENTATION_ITEM ( )  RATIONAL_B_SPLINE_SURFACE ( (
 ( 1.000000000000000000, 0.9115707425106669426, 1.000000000000000000),
 ( 1.000000000000000000, 0.9032011672211383013, 1.000000000000000000),
 ( 1.000000000000000000, 0.8933560653591404721, 1.000000000000000000),
 ( 1.000000000000000000, 0.8671388017650408786, 1.000000000000000000),
 ( 1.000000000000000000, 0.8506934603554324736, 1.000000000000000000),
 ( 1.000000000000000000, 0.8291561975888571689, 1.000000000000000000) ) ) 
 REPRESENTATION_ITEM ( '' )  SURFACE ( )  );
#41694 = EDGE_CURVE ( 'NONE', #35586, #17242, #68057, .T. ) ;
#41695 = DIRECTION ( 'NONE',  ( 0.000000000000000000, 1.000000000000000000, 0.000000000000000000 ) ) ;
#41696 = AXIS2_PLACEMENT_3D ( 'NONE', #34488, #35544, #42527 ) ;
#41697 = ORIENTED_EDGE ( 'NONE', *, *, #38243, .F. ) ;
#41698 = EDGE_CURVE ( 'NONE', #77950, #72376, #19844, .T. ) ;
#41699 = SURFACE_STYLE_FILL_AREA ( #91329 ) ;
#41700 = CARTESIAN_POINT ( 'NONE',  ( 46.00000000000000000, 450.0000000000002274, 18.20242257375371153 ) ) ;
#41701 = CARTESIAN_POINT ( 'NONE',  ( 109.1940635787650251, -57.66566924721494303, 197.4402562130856609 ) ) ;
#41702 = AXIS2_PLACEMENT_3D ( 'NONE', #33162, #56863, #42282 ) ;
#41703 = CARTESIAN_POINT ( 'NONE',  ( 37.56086443614415060, 463.3607749238105384, 20.02088289192820625 ) ) ;
#41704 = STYLED_ITEM ( 'NONE', ( #79512 ), #104825 ) ;
#41705 = CARTESIAN_POINT ( 'NONE',  ( 9.999999999999998224, -15.00000000000000000, -9.999999999999998224 ) ) ;
#41706 = CARTESIAN_POINT ( 'NONE',  ( 4.205882352941182845, -5.000000000000000000, -72.69916451482998809 ) ) ;
#41707 = DIRECTION ( 'NONE',  ( 0.000000000000000000, -1.000000000000000000, 0.000000000000000000 ) ) ;
#41708 = CARTESIAN_POINT ( 'NONE',  ( -82.81552959430850080, -60.00000000000000000, 198.6933800083513404 ) ) ;
#41709 = CARTESIAN_POINT ( 'NONE',  ( -45.43339346675878687, 430.7348383325900727, 7.234598910837349628 ) ) ;
#41710 = VERTEX_POINT ( 'NONE', #85540 ) ;
#41711 = CARTESIAN_POINT ( 'NONE',  ( -40.73878142687892279, 503.7113041876743864, 10.19672445236252045 ) ) ;
#41712 = CARTESIAN_POINT ( 'NONE',  ( -84.97692457071781291, -42.95386403672870301, 185.6637990199461115 ) ) ;
#41713 = ORIENTED_EDGE ( 'NONE', *, *, #50693, .T. ) ;
#41714 = CARTESIAN_POINT ( 'NONE',  ( 24.60261549097931422, 305.9904144327904874, -8.752652469573394711 ) ) ;
#41715 = ORIENTED_EDGE ( 'NONE', *, *, #48345, .T. ) ;
#41716 = CARTESIAN_POINT ( 'NONE',  ( -7.150053860865849487, -11.78265453913977545, 3.590189269391290683 ) ) ;
#41717 = CARTESIAN_POINT ( 'NONE',  ( -87.03223608452462656, -60.20541530288490861, -7.697531398653797652 ) ) ;
#41718 = CARTESIAN_POINT ( 'NONE',  ( -6.999999995588868984, -13.84708942052845870, -5.798489586938165630 ) ) ;
#41719 = LINE ( 'NONE', #51392, #84265 ) ;
#41720 = CARTESIAN_POINT ( 'NONE',  ( 92.82022815836235452, 1.016364837396684119E-14, 0.000000000000000000 ) ) ;
#41721 = CARTESIAN_POINT ( 'NONE',  ( 57.45015997180046696, 4.000000000000013323, 0.000000000000000000 ) ) ;
#41722 = CARTESIAN_POINT ( 'NONE',  ( 11.29173574096709309, 20.04892995410248702, -8.410943388600204074 ) ) ;
#41723 = CARTESIAN_POINT ( 'NONE',  ( -6.738183602098732403E-15, 17.51648154115788714, 55.02144460582525909 ) ) ;
#41724 = CARTESIAN_POINT ( 'NONE',  ( 54.03872891708841308, -1.232595164407830946E-29, 4.000000000000007105 ) ) ;
#41725 = EDGE_CURVE ( 'NONE', #27343, #75403, #11081, .T. ) ;
#41726 = CARTESIAN_POINT ( 'NONE',  ( -24.50860473033056053, -14.21045842199433018, -36.19504829128915446 ) ) ;
#41727 = CARTESIAN_POINT ( 'NONE',  ( -76.85289103080442885, -53.37786451256174303, 140.9389337355551106 ) ) ;
#41728 = ORIENTED_EDGE ( 'NONE', *, *, #61910, .T. ) ;
#41729 = CARTESIAN_POINT ( 'NONE',  ( 73.20681906048392307, -14.21045842199435150, 129.4971587772804185 ) ) ;
#41730 = CARTESIAN_POINT ( 'NONE',  ( 7.150931910075643216, 86.78625798522261903, -3.588457848165357067 ) ) ;
#41731 = CARTESIAN_POINT ( 'NONE',  ( 96.62604160751135396, -57.67146650215429560, 46.51347612679317223 ) ) ;
#41732 = ORIENTED_EDGE ( 'NONE', *, *, #98234, .T. ) ;
#41733 = DIRECTION ( 'NONE',  ( -1.000000000000000000, -1.224606353822377258E-16, -0.000000000000000000 ) ) ;
#41734 = DIRECTION ( 'NONE',  ( 1.000000000000000000, 1.224606353822377258E-16, 0.000000000000000000 ) ) ;
#41735 = VERTEX_POINT ( 'NONE', #52611 ) ;
#41736 = CIRCLE ( 'NONE', #354, 15.00000000000000711 ) ;
#41737 = CARTESIAN_POINT ( 'NONE',  ( 15.89347175675500523, 43.76110554583822676, 6.420484938539215314 ) ) ;
#41738 = CARTESIAN_POINT ( 'NONE',  ( 2.977408999572651815, -10.43750000204838457, 7.188101187500000933 ) ) ;
#41739 = CARTESIAN_POINT ( 'NONE',  ( 5.276498195232712796, -6.073236878018009044, -7.633618187056885773 ) ) ;
#41740 = PRESENTATION_LAYER_ASSIGNMENT (  '', '', ( #31383 ) ) ;
#41741 = DIRECTION ( 'NONE',  ( -0.000000000000000000, 1.000000000000000000, 0.000000000000000000 ) ) ;
#41742 = DIRECTION ( 'NONE',  ( 0.000000000000000000, 1.000000000000000000, 0.000000000000000000 ) ) ;
#41743 = EDGE_CURVE ( 'NONE', #70219, #26294, #43887, .T. ) ;
#41744 = CARTESIAN_POINT ( 'NONE',  ( -17.39146662423148371, 45.59957931493300265, -4.393505531746719761 ) ) ;
#41745 = CARTESIAN_POINT ( 'NONE',  ( 42.37751841893198446, 435.9440627571722757, 7.948837343527291210 ) ) ;
#41746 = VERTEX_POINT ( 'NONE', #37012 ) ;
#41747 = CARTESIAN_POINT ( 'NONE',  ( -7.096116585352607586, 40.56175661586830472, -70.95279415358434960 ) ) ;
#41749 = CARTESIAN_POINT ( 'NONE',  ( 28.52458533298364429, -25.58352184121855899, 30.19512149105761978 ) ) ;
#41748 = DIRECTION ( 'NONE',  ( 0.000000000000000000, 0.000000000000000000, 1.000000000000000000 ) ) ;
#41750 = CARTESIAN_POINT ( 'NONE',  ( 23.08346828195956135, 305.3972529807544447, -8.882845993008418262 ) ) ;
#41751 = ORIENTED_EDGE ( 'NONE', *, *, #22779, .F. ) ;
#41752 = CARTESIAN_POINT ( 'NONE',  ( -0.2967723360979330205, 12.99353012863888956, 51.71639748483603682 ) ) ;
#41753 = EDGE_LOOP ( 'NONE', ( #17458, #75452, #48197, #45925 ) ) ;
#41754 = DIRECTION ( 'NONE',  ( 1.000000000000000000, 0.000000000000000000, 0.000000000000000000 ) ) ;
#41755 = CARTESIAN_POINT ( 'NONE',  ( 4.881098022930994595, 41.14559726925936900, -70.72437870144329963 ) ) ;
#41756 = DIRECTION ( 'NONE',  ( -1.000000000000000000, -1.224606353822377258E-16, -0.000000000000000000 ) ) ;
#41757 = APPLICATION_CONTEXT ( 'automotive_design' ) ;
#41758 = CARTESIAN_POINT ( 'NONE',  ( -4.966176470918042263, 41.64999999999998437, -70.47555194646970733 ) ) ;
#41759 = CARTESIAN_POINT ( 'NONE',  ( 0.000000000000000000, 0.000000000000000000, -9.974599999999998801 ) ) ;
#41760 = CARTESIAN_POINT ( 'NONE',  ( 17.50000000000002842, 45.00000000000000711, -500000.0000000000582 ) ) ;
#41761 = EDGE_LOOP ( 'NONE', ( #81363, #87672, #39431, #83914, #62911 ) ) ;
#41762 = EDGE_CURVE ( 'NONE', #66436, #84701, #7678, .T. ) ;
#41763 = CARTESIAN_POINT ( 'NONE',  ( 77.39690536252481934, -60.00000000000001421, -29.37461049562547544 ) ) ;
#41764 = CARTESIAN_POINT ( 'NONE',  ( -11.51386276761305005, 45.40501555918416443, -14.44555604779044522 ) ) ;
#41765 = CARTESIAN_POINT ( 'NONE',  ( 30.00000000000000355, 461.9590195980686076, 14.34002891080987574 ) ) ;
#41766 = CARTESIAN_POINT ( 'NONE',  ( 41.86260695335559490, 487.3392455165184742, 9.527470086610451361 ) ) ;
#41767 = EDGE_CURVE ( 'NONE', #27681, #45098, #39814, .T. ) ;
#41768 = CARTESIAN_POINT ( 'NONE',  ( -47.14764774813726689, 18.53760837137019024, -14.71662980465877091 ) ) ;
#41769 = EDGE_LOOP ( 'NONE', ( #29890, #59382, #73331, #36585, #24393 ) ) ;
#41770 =( GEOMETRIC_REPRESENTATION_CONTEXT ( 3 ) GLOBAL_UNCERTAINTY_ASSIGNED_CONTEXT ( ( #34571 ) ) GLOBAL_UNIT_ASSIGNED_CONTEXT ( ( #84528, #99627, #17666 ) ) REPRESENTATION_CONTEXT ( 'NONE', 'WORKASPACE' ) );
#41771 = CARTESIAN_POINT ( 'NONE',  ( 8.099999999999999645, 0.000000000000000000, 0.000000000000000000 ) ) ;
#41772 = VERTEX_POINT ( 'NONE', #27874 ) ;
#41773 = ORIENTED_EDGE ( 'NONE', *, *, #41416, .F. ) ;
#41774 = DIRECTION ( 'NONE',  ( -1.000000000000000000, 0.000000000000000000, 0.000000000000000000 ) ) ;
#41775 = SURFACE_STYLE_FILL_AREA ( #91408 ) ;
#41776 = CARTESIAN_POINT ( 'NONE',  ( 0.9999999999999954481, -54.00000000000000711, 44.97220075561143204 ) ) ;
#41777 = CARTESIAN_POINT ( 'NONE',  ( 71.14984002819953446, 6.856755485862130937E-15, 0.000000000000000000 ) ) ;
#41778 = CARTESIAN_POINT ( 'NONE',  ( 85.75250664619655083, -52.74283471586529259, -6.162475269740077088 ) ) ;
#41779 = TOROIDAL_SURFACE ( 'NONE', #89971, 12.00000000000001066, 3.000000000000000000 ) ;
#41780 = CARTESIAN_POINT ( 'NONE',  ( -33.45340520273420282, 315.3731966014437944, -7.001726257038141554 ) ) ;
#41781 = CARTESIAN_POINT ( 'NONE',  ( -5.414402257315187761, -66.65695130796692069, 14.08782732736250942 ) ) ;
#41782 = CARTESIAN_POINT ( 'NONE',  ( 12.50000000000000355, 40.11561338586450631, -66.43777432280938910 ) ) ;
#41783 = VERTEX_POINT ( 'NONE', #76893 ) ;
#41784 = CARTESIAN_POINT ( 'NONE',  ( -9.041068741337817016, 43.82601327531473601, 14.35289375551374391 ) ) ;
#41785 = ORIENTED_EDGE ( 'NONE', *, *, #77636, .F. ) ;
#41786 = CARTESIAN_POINT ( 'NONE',  ( 17.23461538461538467, 1.411358822780289120E-15, 0.000000000000000000 ) ) ;
#41787 = CARTESIAN_POINT ( 'NONE',  ( -77.01522031534267398, -38.45872817139124322, 184.5006283049931994 ) ) ;
#41788 = CARTESIAN_POINT ( 'NONE',  ( -3.352941176470600304, -1.200583151104954283, 104.5794940929807524 ) ) ;
#41790 = ORIENTED_EDGE ( 'NONE', *, *, #69088, .F. ) ;
#41789 = CARTESIAN_POINT ( 'NONE',  ( -52.84572055339269525, -60.00000000000001421, 63.71983262547996674 ) ) ;
#41791 = CARTESIAN_POINT ( 'NONE',  ( 64.67324255147873657, -60.33694573152096297, 96.31390942180495074 ) ) ;
#41792 = EDGE_CURVE ( 'NONE', #35657, #94819, #86084, .T. ) ;
#41793 = ORIENTED_EDGE ( 'NONE', *, *, #101815, .F. ) ;
#41794 = CARTESIAN_POINT ( 'NONE',  ( 7.188101187500000044, -26.65625000204838813, 0.000000000000000000 ) ) ;
#41795 = CARTESIAN_POINT ( 'NONE',  ( -106.6432006776756083, -57.67119647726944009, 107.9924613694791589 ) ) ;
#41796 = ORIENTED_EDGE ( 'NONE', *, *, #21945, .F. ) ;
#41797 = CARTESIAN_POINT ( 'NONE',  ( 0.000000000000000000, 8.500000000000000000, 0.000000000000000000 ) ) ;
#41798 = CARTESIAN_POINT ( 'NONE',  ( -35.91982565306560105, 490.8454349930416925, 12.40602332252255380 ) ) ;
#41799 = CARTESIAN_POINT ( 'NONE',  ( 0.000000000000000000, 52.29617335651133914, -13.27631144943088692 ) ) ;
#41800 = CARTESIAN_POINT ( 'NONE',  ( -8.000000000000001776, -23.84375000409677270, 3.313708498984758943 ) ) ;
#41801 = CARTESIAN_POINT ( 'NONE',  ( 0.2578475836320717196, 6.890627091270373761, 1.065083781909172522 ) ) ;
#41802 = CARTESIAN_POINT ( 'NONE',  ( 9.253500431420448535, 248.7022845008229126, 3.792688295761959871 ) ) ;
#41803 = VECTOR ( 'NONE', #15599, 999.9999999999998863 ) ;
#41804 = CARTESIAN_POINT ( 'NONE',  ( -7.251694485742912200, 41.54830549313345500, -59.82648083153709706 ) ) ;
#41805 = CARTESIAN_POINT ( 'NONE',  ( -10.04820350651657890, 7.431158258250313509, 0.000000000000000000 ) ) ;
#41806 = CARTESIAN_POINT ( 'NONE',  ( -11.93255308427328565, 294.5886021379643580, 9.881054392645332030 ) ) ;
#41807 =( GEOMETRIC_REPRESENTATION_CONTEXT ( 3 ) GLOBAL_UNCERTAINTY_ASSIGNED_CONTEXT ( ( #44561 ) ) GLOBAL_UNIT_ASSIGNED_CONTEXT ( ( #7305, #47764, #79615 ) ) REPRESENTATION_CONTEXT ( 'NONE', 'WORKASPACE' ) );
#41808 = PRESENTATION_STYLE_ASSIGNMENT (( #8906 ) ) ;
#41809 = VERTEX_POINT ( 'NONE', #35959 ) ;
#41810 = DIRECTION ( 'NONE',  ( 0.000000000000000000, -0.9523642049635228091, 0.3049629831704120941 ) ) ;
#41811 = DIRECTION ( 'NONE',  ( -1.000000000000000000, -1.224606353822377258E-16, -0.000000000000000000 ) ) ;
#41812 = ADVANCED_FACE ( 'NONE', ( #45615 ), #94151, .T. ) ;
#41813 = CARTESIAN_POINT ( 'NONE',  ( 11.17393077666423373, -60.00000000000000711, 39.66661916941054500 ) ) ;
#41814 = CARTESIAN_POINT ( 'NONE',  ( -95.45231390711828112, -29.99999999999999645, 191.3292026307100286 ) ) ;
#41815 = EDGE_CURVE ( 'NONE', #66259, #40330, #38750, .T. ) ;
#41816 = ORIENTED_EDGE ( 'NONE', *, *, #14219, .T. ) ;
#41817 = ORIENTED_EDGE ( 'NONE', *, *, #39623, .F. ) ;
#41818 = CARTESIAN_POINT ( 'NONE',  ( 38.66222440567811702, 25.17349152328067419, -12.83126464919931564 ) ) ;
#41819 = CIRCLE ( 'NONE', #78026, 1.000000000000001110 ) ;
#41820 = CARTESIAN_POINT ( 'NONE',  ( 63.37667947266371726, -57.67874266049060594, 119.9838882821124173 ) ) ;
#41821 = EDGE_CURVE ( 'NONE', #103934, #31692, #70935, .T. ) ;
#41823 = CARTESIAN_POINT ( 'NONE',  ( -8.425387792203615334, 6.357088691644186440, 3.972068509340369147 ) ) ;
#41822 = CARTESIAN_POINT ( 'NONE',  ( 6.492511067189947305, 41.78432740739263096, -59.03547063838888675 ) ) ;
#41824 = CARTESIAN_POINT ( 'NONE',  ( 20.17806256124487874, -25.90288594722162330, -38.48045932952570070 ) ) ;
#41825 = CARTESIAN_POINT ( 'NONE',  ( -0.5688039300739448079, 43.22114551779936420, 18.61622414936086045 ) ) ;
#41826 = FACE_OUTER_BOUND ( 'NONE', #29271, .T. ) ;
#41827 = CARTESIAN_POINT ( 'NONE',  ( -36.09010194260303450, -60.00000000000000000, 47.44087383398635893 ) ) ;
#41828 = CARTESIAN_POINT ( 'NONE',  ( 12.59151156833761220, 9.285187046072287842, 9.290575386839268646 ) ) ;
#41829 = CARTESIAN_POINT ( 'NONE',  ( 1.010192736754801146, 46.02235752558536319, -16.74599088214888454 ) ) ;
#41830 = CARTESIAN_POINT ( 'NONE',  ( -87.02599616935226834, -35.40601924051522076, 188.2192322684356895 ) ) ;
#41831 = VERTEX_POINT ( 'NONE', #70415 ) ;
#41832 = CARTESIAN_POINT ( 'NONE',  ( 4.387778976649723378E-15, 0.000000000000000000, -35.82893434829263413 ) ) ;
#41833 = CARTESIAN_POINT ( 'NONE',  ( -7.056147190753457643, -29.03107994581888107, 28.71850030171957258 ) ) ;
#41834 = CYLINDRICAL_SURFACE ( 'NONE', #53241, 5.000000000000000888 ) ;
#41835 = CARTESIAN_POINT ( 'NONE',  ( -2.514199206790655783, -49.70878148651267026, 102.6057069765799099 ) ) ;
#41836 = COLOUR_RGB ( '', 0.66274510, 0.83137255, 0.94901961) ;
#41838 = CARTESIAN_POINT ( 'NONE',  ( 5.044949049065960089, -67.63307031760351151, 13.94001772754543644 ) ) ;
#41837 = CARTESIAN_POINT ( 'NONE',  ( -98.04235954153416799, -59.99999999999997868, 196.5000328139588532 ) ) ;
#41839 = ORIENTED_EDGE ( 'NONE', *, *, #105871, .T. ) ;
#41840 = CARTESIAN_POINT ( 'NONE',  ( 5.313748243244007519, 41.99394926078451107, -69.45901782876110531 ) ) ;
#41841 = CARTESIAN_POINT ( 'NONE',  ( 33.09999999999999432, -3.309499999999999886, 0.000000000000000000 ) ) ;
#41842 = CARTESIAN_POINT ( 'NONE',  ( -7.934883677559682269, 33.86839177937552137, 1.051380792122687646 ) ) ;
#41843 = CARTESIAN_POINT ( 'NONE',  ( 27.49230554713799535, 305.3620761542157425, -9.445234096144215385 ) ) ;
#41844 = CARTESIAN_POINT ( 'NONE',  ( 4.999999999999992006, -46.27603786271895814, 102.2532056551910387 ) ) ;
#41845 =( BOUNDED_SURFACE ( )  B_SPLINE_SURFACE ( 2, 3, ( 
 ( #51396, #27172, #99953, #43321, #59514, #76203, #3394, #2306, #50332, #60063, #17995, #50856, #77283, #83762, #102075, #35254, #44387, #9870, #2846, #42783, #68677, #17468, #75674, #83240, #10924, #1775, #34733, #67604, #92923, #69206, #9333, #19088, #28236, #92387 ),
 ( #35798, #101557, #85376, #91353, #93476, #42243, #19626, #51927, #75132, #84841, #52459, #1228, #34196, #85929, #61656, #104195, #62700, #38951, #102618, #79396, #45982, #28777, #95074, #37920, #69727, #54037, #21207, #94546, #38437, #78332, #12000, #22256, #55105, #37392 ),
 ( #70253, #95592, #20698, #103154, #4448, #29822, #53536, #44932, #87506, #70782, #86466, #63232, #30339, #12524, #21728, #86982, #54569, #103677, #3926, #13051, #45457, #13586, #78861, #53006, #5513, #88035, #77817, #29300, #96124, #71828, #14115, #62188, #36859, #46502 ) ),
 .UNSPECIFIED., .F., .T., .F. ) 
 B_SPLINE_SURFACE_WITH_KNOTS ( ( 3, 3 ),
 ( 4, 2, 2, 2, 2, 2, 2, 2, 2, 2, 2, 2, 2, 2, 2, 2, 4 ),
 ( 0.000000000000000000, 1.000000000000000000 ),
 ( 3.141592653589793116, 3.534291735288517700, 3.926990816987241395, 4.319689898685965090, 4.712388980384689674, 5.105088062083414258, 5.497787143782137953, 5.890486225480861648, 6.283185307179586232, 6.675884388878310816, 7.068583470577034511, 7.461282552275758206, 7.853981633974482790, 8.246680715673207374, 8.639379797371930181, 9.032078879070654764, 9.424777960769379348 ),
 .UNSPECIFIED. ) 
 GEOMETRIC_REPRESENTATION_ITEM ( )  RATIONAL_B_SPLINE_SURFACE ( (
 ( 1.000000000000000000, 1.000000000000000000, 1.000000000000000000, 1.000000000000000000, 1.000000000000000000, 1.000000000000000000, 1.000000000000000000, 1.000000000000000000, 1.000000000000000000, 1.000000000000000000, 1.000000000000000000, 1.000000000000000000, 1.000000000000000000, 1.000000000000000000, 1.000000000000000000, 1.000000000000000000, 1.000000000000000000, 1.000000000000000000, 1.000000000000000000, 1.000000000000000000, 1.000000000000000000, 1.000000000000000000, 1.000000000000000000, 1.000000000000000000, 1.000000000000000000, 1.000000000000000000, 1.000000000000000000, 1.000000000000000000, 1.000000000000000000, 1.000000000000000000, 1.000000000000000000, 1.000000000000000000, 1.000000000000000000, 1.000000000000000000),
 ( 1.857142857142858317, 1.857142857142858317, 1.857142857142860981, 1.857142857142860981, 1.857142857142858317, 1.857142857142858317, 1.857142857142858317, 1.857142857142858317, 1.857142857142858317, 1.857142857142858317, 1.857142857142858317, 1.857142857142858317, 1.857142857142858317, 1.857142857142858317, 1.857142857142858317, 1.857142857142858317, 1.857142857142858317, 1.857142857142858317, 1.857142857142858317, 1.857142857142858317, 1.857142857142858317, 1.857142857142858317, 1.857142857142858317, 1.857142857142858317, 1.857142857142858317, 1.857142857142858317, 1.857142857142858317, 1.857142857142858317, 1.857142857142858317, 1.857142857142858317, 1.857142857142858317, 1.857142857142858317, 1.857142857142858317, 1.857142857142858317),
 ( 1.000000000000000000, 1.000000000000000000, 1.000000000000000000, 1.000000000000000000, 1.000000000000000000, 1.000000000000000000, 1.000000000000000000, 1.000000000000000000, 1.000000000000000000, 1.000000000000000000, 1.000000000000000000, 1.000000000000000000, 1.000000000000000000, 1.000000000000000000, 1.000000000000000000, 1.000000000000000000, 1.000000000000000000, 1.000000000000000000, 1.000000000000000000, 1.000000000000000000, 1.000000000000000000, 1.000000000000000000, 1.000000000000000000, 1.000000000000000000, 1.000000000000000000, 1.000000000000000000, 1.000000000000000000, 1.000000000000000000, 1.000000000000000000, 1.000000000000000000, 1.000000000000000000, 1.000000000000000000, 1.000000000000000000, 1.000000000000000000) ) ) 
 REPRESENTATION_ITEM ( '' )  SURFACE ( )  );
#41846 = PLANE ( 'NONE',  #96077 ) ;
#41847 = CARTESIAN_POINT ( 'NONE',  ( 80.97977184163765685, 1.030564683017419500E-14, 0.000000000000000000 ) ) ;
#41848 = ADVANCED_FACE ( 'NONE', ( #13210 ), #46139, .F. ) ;
#41849 = CARTESIAN_POINT ( 'NONE',  ( 106.4976671120242173, -30.00000000000003553, 137.1020467228335349 ) ) ;
#41850 = ORIENTED_EDGE ( 'NONE', *, *, #34019, .F. ) ;
#41851 = LINE ( 'NONE', #90955, #17183 ) ;
#41852 = CARTESIAN_POINT ( 'NONE',  ( -10.00004721872061353, 254.0001180468113944, -0.2617599822266347687 ) ) ;
#41853 = DIRECTION ( 'NONE',  ( 0.2246406655633822746, 0.2919586099461945472, 0.9296756108737748159 ) ) ;
#41854 = CARTESIAN_POINT ( 'NONE',  ( 5.833333333333327708, -3.728231135448883737, 103.8776713793258324 ) ) ;
#41855 =( BOUNDED_SURFACE ( )  B_SPLINE_SURFACE ( 3, 2, ( 
 ( #61691, #61138, #33965 ),
 ( #41485, #72779, #16685 ),
 ( #33423, #90038, #65770 ),
 ( #985, #83016, #17238 ),
 ( #49576, #9109, #64710 ),
 ( #23749, #66836, #82485 ),
 ( #89519, #56050, #91128 ),
 ( #6987, #23212, #66296 ),
 ( #15084, #58202, #50108 ),
 ( #7507, #25339, #32364 ),
 ( #99178, #49033, #105686 ),
 ( #81931, #106745, #31825 ),
 ( #40427, #42017, #15613 ),
 ( #98650, #24800, #88985 ),
 ( #74901, #57654, #47969 ),
 ( #80878, #90575, #452 ) ),
 .UNSPECIFIED., .F., .F., .T. ) 
 B_SPLINE_SURFACE_WITH_KNOTS ( ( 4, 2, 2, 2, 2, 2, 2, 4 ),
 ( 3, 3 ),
 ( 2.545706700995964411E-16, 0.001044086800740991585, 0.001566130201111359983, 0.002088173601481728599, 0.002610217001852097214, 0.003132260402222465396, 0.003654303802592833578, 0.004176347202963202193 ),
 ( 0.000000000000000000, 1.000000000000000000 ),
 .UNSPECIFIED. ) 
 GEOMETRIC_REPRESENTATION_ITEM ( )  RATIONAL_B_SPLINE_SURFACE ( (
 ( 1.000000000000000000, 0.8350736500407900387, 1.000000000000000000),
 ( 1.000000000000000000, 0.8489954227499153516, 1.000000000000000000),
 ( 1.000000000000000000, 0.8615675893698659937, 1.000000000000000000),
 ( 1.000000000000000000, 0.8776574663914948893, 1.000000000000000000),
 ( 1.000000000000000000, 0.8825492266254932883, 1.000000000000000000),
 ( 1.000000000000000000, 0.8909252284681432599, 1.000000000000000000),
 ( 1.000000000000000000, 0.8944578560788611910, 1.000000000000000000),
 ( 1.000000000000000000, 0.9000429021731324308, 1.000000000000000000),
 ( 1.000000000000000000, 0.9020681612885971257, 1.000000000000000000),
 ( 1.000000000000000000, 0.9043430709035563675, 1.000000000000000000),
 ( 1.000000000000000000, 0.9046293304020973647, 1.000000000000000000),
 ( 1.000000000000000000, 0.9034445554302690251, 1.000000000000000000),
 ( 1.000000000000000000, 0.9019515008114564747, 1.000000000000000000),
 ( 1.000000000000000000, 0.8973842636250342064, 1.000000000000000000),
 ( 1.000000000000000000, 0.8943059481781064912, 1.000000000000000000),
 ( 1.000000000000000000, 0.8904848454315665851, 1.000000000000000000) ) ) 
 REPRESENTATION_ITEM ( '' )  SURFACE ( )  );
#41856 = CARTESIAN_POINT ( 'NONE',  ( 45.46270652965668546, 379.8533979750452545, 7.113780170705016559 ) ) ;
#41857 = ADVANCED_FACE ( 'NONE', ( #47702 ), #24011, .F. ) ;
#41858 = CARTESIAN_POINT ( 'NONE',  ( 22.25669491856071858, 1.482358050883964840E-15, 0.000000000000000000 ) ) ;
#41859 = ORIENTED_EDGE ( 'NONE', *, *, #81717, .F. ) ;
#41860 = UNCERTAINTY_MEASURE_WITH_UNIT (LENGTH_MEASURE( 1.000000000000000082E-05 ), #4728, 'distance_accuracy_value', 'NONE');
#41861 = DIRECTION ( 'NONE',  ( -1.000000000000000000, -1.224606353822377258E-16, -0.000000000000000000 ) ) ;
#41862 = VERTEX_POINT ( 'NONE', #97321 ) ;
#41863 = LINE ( 'NONE', #830, #93134 ) ;
#41864 = CARTESIAN_POINT ( 'NONE',  ( 29.00000000000001066, 0.000000000000000000, 9.000000000000000000 ) ) ;
#41865 = ADVANCED_FACE ( 'NONE', ( #72518 ), #54183, .T. ) ;
#41866 = CARTESIAN_POINT ( 'NONE',  ( 39.04923757935661399, 48.00000000000000000, 52.30342408741256577 ) ) ;
#41867 = CARTESIAN_POINT ( 'NONE',  ( 5.000000000000001776, -14.45898243499974711, 13.52154848216171068 ) ) ;
#41868 = DIRECTION ( 'NONE',  ( -1.224646799147353454E-16, 0.000000000000000000, -1.000000000000000000 ) ) ;
#41869 = ORIENTED_EDGE ( 'NONE', *, *, #87460, .F. ) ;
#41870 = CARTESIAN_POINT ( 'NONE',  ( 92.06880798540581168, -60.00000000000002842, 4.793930753321646421 ) ) ;
#41872 = CARTESIAN_POINT ( 'NONE',  ( 19.25484014596467830, -49.91514199782810124, 32.66260667748945679 ) ) ;
#41871 = CARTESIAN_POINT ( 'NONE',  ( -82.63253876390992048, -60.00000000000011369, 201.7050754921980911 ) ) ;
#41873 = CARTESIAN_POINT ( 'NONE',  ( 36.23910820157426826, 462.2855794318964513, 3.478784509830200822 ) ) ;
#41874 = CARTESIAN_POINT ( 'NONE',  ( 37.62251730745840916, 437.3427388312647395, 4.535622330043188377 ) ) ;
#41875 = CARTESIAN_POINT ( 'NONE',  ( -40.48074807841378231, -46.43598188464789445, 40.68275167793495228 ) ) ;
#41876 = CARTESIAN_POINT ( 'NONE',  ( -26.50079164160752399, 18.64284798593038772, 27.83217509638362586 ) ) ;
#41877 = ORIENTED_EDGE ( 'NONE', *, *, #7059, .T. ) ;
#41878 = CARTESIAN_POINT ( 'NONE',  ( -20.05453516056602581, -4.285714285714295357, 15.38541618194246929 ) ) ;
#41879 = CARTESIAN_POINT ( 'NONE',  ( 7.938522632820759206, 54.17484897284736434, 1.684095682798675497 ) ) ;
#41880 = CARTESIAN_POINT ( 'NONE',  ( 5.961320375100143565, -13.36618214390661841, 13.51689209302652728 ) ) ;
#41881 = AXIS2_PLACEMENT_3D ( 'NONE', #26880, #76978, #61348 ) ;
#41882 = CARTESIAN_POINT ( 'NONE',  ( 27.61650669486618881, -3.851859888774471706E-31, 4.000000000000000888 ) ) ;
#41883 = CARTESIAN_POINT ( 'NONE',  ( 98.59800593614012598, 1.016364837396684119E-14, 0.000000000000000000 ) ) ;
#41884 = CARTESIAN_POINT ( 'NONE',  ( 0.000000000000000000, -14.49999999999999822, 0.000000000000000000 ) ) ;
#41885 = VERTEX_POINT ( 'NONE', #63400 ) ;
#41886 = CARTESIAN_POINT ( 'NONE',  ( 4.999999999999993783, -46.00000000000000000, 102.2532056551910387 ) ) ;
#41887 = DIRECTION ( 'NONE',  ( -1.000000000000000000, -1.224606353822377258E-16, -0.000000000000000000 ) ) ;
#41888 = ORIENTED_EDGE ( 'NONE', *, *, #71793, .F. ) ;
#41889 = CARTESIAN_POINT ( 'NONE',  ( 75.22651015812265030, -30.00000000013189805, 158.5714180975027432 ) ) ;
#41890 = CARTESIAN_POINT ( 'NONE',  ( 20.59266090671921745, 41.82625683843084374, -78.90645973795369628 ) ) ;
#41891 = AXIS2_PLACEMENT_3D ( 'NONE', #31911, #46103, #20817 ) ;
#41892 = DIRECTION ( 'NONE',  ( 0.000000000000000000, -1.000000000000000000, 0.000000000000000000 ) ) ;
#41893 = CARTESIAN_POINT ( 'NONE',  ( 12.21253585067004543, 5.000000000000004441, 6.123233995736770227E-16 ) ) ;
#41894 = CARTESIAN_POINT ( 'NONE',  ( 80.93729537171422805, -29.99999999999999645, 5.168379641639776700 ) ) ;
#41895 = COLOUR_RGB ( '', 0.09019608, 0.27058824, 0.51372549) ;
#41896 = EDGE_CURVE ( 'NONE', #81173, #102469, #79166, .T. ) ;
#41897 = CARTESIAN_POINT ( 'NONE',  ( 0.000000000000000000, -30.00000000000000000, 8.000000000000000000 ) ) ;
#41898 = ORIENTED_EDGE ( 'NONE', *, *, #99066, .T. ) ;
#41899 = ORIENTED_EDGE ( 'NONE', *, *, #45110, .F. ) ;
#41900 = VERTEX_POINT ( 'NONE', #14274 ) ;
#41901 = CARTESIAN_POINT ( 'NONE',  ( 0.000000000000000000, -1.500000000000000000, 0.000000000000000000 ) ) ;
#41902 = CARTESIAN_POINT ( 'NONE',  ( 43.58619280597294221, 434.9882623928568819, 14.52865984557667112 ) ) ;
#41903 = CARTESIAN_POINT ( 'NONE',  ( 0.000000000000000000, 0.000000000000000000, -9.078441367943003826 ) ) ;
#41904 = MECHANICAL_DESIGN_GEOMETRIC_PRESENTATION_REPRESENTATION (  '', ( #12631 ), #16034 ) ;
#41905 = CARTESIAN_POINT ( 'NONE',  ( -38.54161147518751562, 464.3852313890828327, 18.95019507570325246 ) ) ;
#41906 = CARTESIAN_POINT ( 'NONE',  ( -32.16711761884142362, 380.6411173872397740, 24.65392784832810946 ) ) ;
#41907 =( NAMED_UNIT ( * ) PLANE_ANGLE_UNIT ( ) SI_UNIT ( $, .RADIAN. ) );
#41908 = ORIENTED_EDGE ( 'NONE', *, *, #20735, .F. ) ;
#41909 =( NAMED_UNIT ( * ) PLANE_ANGLE_UNIT ( ) SI_UNIT ( $, .RADIAN. ) );
#41910 = ORIENTED_EDGE ( 'NONE', *, *, #7664, .T. ) ;
#41911 = DIRECTION ( 'NONE',  ( 0.000000000000000000, -1.000000000000000000, 0.000000000000000000 ) ) ;
#41912 = CARTESIAN_POINT ( 'NONE',  ( 67.25431336777386093, -38.33468234247306583, 122.2200866910623489 ) ) ;
#41913 = FACE_OUTER_BOUND ( 'NONE', #85127, .T. ) ;
#41914 = CARTESIAN_POINT ( 'NONE',  ( 27.08164365510018357, 307.1447734948634434, 10.92944225879553244 ) ) ;
#41915 = CARTESIAN_POINT ( 'NONE',  ( 46.00000000000000000, 450.0000000000002274, 8.202422573753707979 ) ) ;
#41916 = PRESENTATION_STYLE_ASSIGNMENT (( #80776 ) ) ;
#41917 = CIRCLE ( 'NONE', #59183, 4.000000000000000888 ) ;
#41918 = CARTESIAN_POINT ( 'NONE',  ( -40.42601080768528732, 460.8348341399804440, 2.184598410783807676 ) ) ;
#41919 = CARTESIAN_POINT ( 'NONE',  ( 46.84999999999999432, -3.309499999999999886, 4.475777889183790779E-16 ) ) ;
#41920 = AXIS2_PLACEMENT_3D ( 'NONE', #52520, #5049, #85436 ) ;
#41921 = LINE ( 'NONE', #11132, #39427 ) ;
#41922 = MECHANICAL_DESIGN_GEOMETRIC_PRESENTATION_REPRESENTATION (  '', ( #526 ), #97121 ) ;
#41924 = ORIENTED_EDGE ( 'NONE', *, *, #67566, .T. ) ;
#41923 = PRESENTATION_LAYER_ASSIGNMENT (  '', '', ( #81542 ) ) ;
#41925 = CARTESIAN_POINT ( 'NONE',  ( 0.000000000000000000, 6.123233995736767268E-16, -5.000000000000000888 ) ) ;
#41926 = DIRECTION ( 'NONE',  ( -0.000000000000000000, -1.000000000000000000, -0.000000000000000000 ) ) ;
#41927 = UNCERTAINTY_MEASURE_WITH_UNIT (LENGTH_MEASURE( 1.000000000000000082E-05 ), #10877, 'distance_accuracy_value', 'NONE');
#41928 = DIRECTION ( 'NONE',  ( 1.224646799147353207E-16, 0.000000000000000000, -1.000000000000000000 ) ) ;
#41929 = CARTESIAN_POINT ( 'NONE',  ( -7.968863443239236233, -4.547634245050486079, -8.057411785091790790 ) ) ;
#41930 = AXIS2_PLACEMENT_3D ( 'NONE', #51728, #27512, #20501 ) ;
#41931 = DIRECTION ( 'NONE',  ( -1.000000000000000000, -0.000000000000000000, -0.000000000000000000 ) ) ;
#41932 = CARTESIAN_POINT ( 'NONE',  ( -7.551892080562057963, 101.9901229746061802, 2.647003822403975803 ) ) ;
#41933 = CARTESIAN_POINT ( 'NONE',  ( 46.00000000000000000, 461.6622277975422435, 10.18145404766786655 ) ) ;
#41934 = CARTESIAN_POINT ( 'NONE',  ( 84.54053991961795589, -53.81834405645398789, 189.9383315222177373 ) ) ;
#41935 = CARTESIAN_POINT ( 'NONE',  ( 17.83130206369999726, 36.70573752982816274, -22.40672895700094358 ) ) ;
#41936 = CARTESIAN_POINT ( 'NONE',  ( 0.000000000000000000, 0.000000000000000000, 0.000000000000000000 ) ) ;
#41937 = EDGE_LOOP ( 'NONE', ( #96596, #87562, #15932, #56476, #52194, #28995 ) ) ;
#41938 = CARTESIAN_POINT ( 'NONE',  ( 93.07376397780032562, -57.65571088614280626, -17.03660586601905180 ) ) ;
#41939 = CARTESIAN_POINT ( 'NONE',  ( 0.000000000000000000, 274.9999999999999432, -10.00000000000000533 ) ) ;
#41940 = DIRECTION ( 'NONE',  ( 1.000000000000000000, 1.224606353822377258E-16, 0.000000000000000000 ) ) ;
#41941 = CARTESIAN_POINT ( 'NONE',  ( 5.656854249492380582, -18.31249999999999289, -5.656854249492379694 ) ) ;
#41942 = CARTESIAN_POINT ( 'NONE',  ( -81.57252369435565242, -30.00000000000000711, -8.038432599570381143 ) ) ;
#41943 = EDGE_CURVE ( 'NONE', #63078, #51593, #14604, .T. ) ;
#41944 = DIRECTION ( 'NONE',  ( 0.000000000000000000, -1.000000000000000000, 0.000000000000000000 ) ) ;
#41945 = CARTESIAN_POINT ( 'NONE',  ( 22.22792991547093422, 27.72626095856945128, -32.73621634624677057 ) ) ;
#41946 = DIRECTION ( 'NONE',  ( -0.5735764363510494901, -0.8191520442889894671, 0.000000000000000000 ) ) ;
#41947 = ADVANCED_FACE ( 'NONE', ( #29972 ), #62861, .T. ) ;
#41949 = DIRECTION ( 'NONE',  ( 1.160749806054361473E-16, 0.000000000000000000, -1.000000000000000000 ) ) ;
#41948 = DIRECTION ( 'NONE',  ( 0.000000000000000000, -1.000000000000000000, 0.000000000000000000 ) ) ;
#41950 = DIRECTION ( 'NONE',  ( -0.5735764363510512664, 0.8191520442889881348, 1.003171929053520309E-16 ) ) ;
#41951 = SURFACE_STYLE_FILL_AREA ( #32829 ) ;
#41952 = CARTESIAN_POINT ( 'NONE',  ( 105.5353273971932140, 5.000000000000021316, 0.000000000000000000 ) ) ;
#41953 = CARTESIAN_POINT ( 'NONE',  ( 22.33349330513380337, 1.593028355512270567E-15, 0.000000000000000000 ) ) ;
#41954 = DIRECTION ( 'NONE',  ( 1.000000000000000000, 1.224606353822377258E-16, 0.000000000000000000 ) ) ;
#41955 = AXIS2_PLACEMENT_3D ( 'NONE', #80026, #13165, #86572 ) ;
#41956 = DIRECTION ( 'NONE',  ( 0.000000000000000000, -1.000000000000000000, 0.000000000000000000 ) ) ;
#41957 = B_SPLINE_CURVE_WITH_KNOTS ( 'NONE', 3,
 ( #8511, #58129, #59213, #45034, #91055, #41945, #17163, #50034, #82941, #74830, #43021, #77920, #4028, #92090, #98585, #67826, #24730, #100712, #51087, #91580 ),
 .UNSPECIFIED., .F., .F.,
 ( 4, 2, 2, 2, 2, 2, 2, 2, 2, 4 ),
 ( 0.0009445086018700385531, 0.001449274952876526343, 0.001954041303883013916, 0.002458807654889501489, 0.002963574005895989495, 0.003468340356902476634, 0.003973106707908964641, 0.004225489883412212114, 0.004477873058915460454, 0.004982639409921950195 ),
 .UNSPECIFIED. ) ;
#41958 = AXIS2_PLACEMENT_3D ( 'NONE', #4184, #94808, #37657 ) ;
#41959 = ORIENTED_EDGE ( 'NONE', *, *, #76773, .F. ) ;
#41960 = CARTESIAN_POINT ( 'NONE',  ( 0.000000000000000000, 0.000000000000000000, -3.725171428571429022 ) ) ;
#41961 = SURFACE_SIDE_STYLE ('',( #33910 ) ) ;
#41962 = CARTESIAN_POINT ( 'NONE',  ( 1.312288883421210306, 21.64033319957477985, 6.880324608108087325 ) ) ;
#41963 = CARTESIAN_POINT ( 'NONE',  ( -67.76098042632558816, -29.91089683381006026, -21.83674399635897956 ) ) ;
#41965 = CARTESIAN_POINT ( 'NONE',  ( -64.12014087452101307, -21.77003452523452154, -21.74776922628243980 ) ) ;
#41964 = DIRECTION ( 'NONE',  ( 0.000000000000000000, -1.000000000000000000, 0.000000000000000000 ) ) ;
#41966 = EDGE_CURVE ( 'NONE', #46431, #20, #46652, .T. ) ;
#41967 = ORIENTED_EDGE ( 'NONE', *, *, #40350, .T. ) ;
#41968 = FACE_OUTER_BOUND ( 'NONE', #92724, .T. ) ;
#41969 = EDGE_LOOP ( 'NONE', ( #45348, #5376, #11254, #9640, #52775 ) ) ;
#41970 = CARTESIAN_POINT ( 'NONE',  ( 42.36808196472505017, 461.6713445545161107, 3.771400599639998852 ) ) ;
#41971 = CARTESIAN_POINT ( 'NONE',  ( 40.02102699515286588, 489.9193542772574688, 11.11924804287039947 ) ) ;
#41972 = CARTESIAN_POINT ( 'NONE',  ( -89.46289319159794218, -59.99999999999998579, -19.71868189584859721 ) ) ;
#41973 = ORIENTED_EDGE ( 'NONE', *, *, #67216, .F. ) ;
#41974 = FACE_OUTER_BOUND ( 'NONE', #31033, .T. ) ;
#41975 = CARTESIAN_POINT ( 'NONE',  ( 101.6143094094037167, -60.22772872295755064, 194.6033318209078402 ) ) ;
#41977 = CARTESIAN_POINT ( 'NONE',  ( -47.77591036386557732, 12.17665806217422286, 14.37301751662919003 ) ) ;
#41976 = CARTESIAN_POINT ( 'NONE',  ( 2.255773162242571850, 294.8363355346813819, -9.758683423828378167 ) ) ;
#41978 = B_SPLINE_CURVE_WITH_KNOTS ( 'NONE', 3,
 ( #59121, #1916, #92004, #17603, #68815, #18685 ),
 .UNSPECIFIED., .F., .F.,
 ( 4, 2, 4 ),
 ( 2.475503369199568371E-07, 0.002222330217055625001, 0.004444412883774330643 ),
 .UNSPECIFIED. ) ;
#41979 = ORIENTED_EDGE ( 'NONE', *, *, #45267, .T. ) ;
#41980 = AXIS2_PLACEMENT_3D ( 'NONE', #29773, #11546, #76819 ) ;
#41981 = ORIENTED_EDGE ( 'NONE', *, *, #47308, .F. ) ;
#41982 = VERTEX_POINT ( 'NONE', #96293 ) ;
#41984 =( BOUNDED_SURFACE ( )  B_SPLINE_SURFACE ( 3, 2, ( 
 ( #99398, #58440, #2300 ),
 ( #68114, #10920, #41718 ),
 ( #17463, #683, #1224 ),
 ( #49804, #18529, #84305 ),
 ( #66526, #43840, #26122 ),
 ( #82710, #51390, #2842 ),
 ( #50328, #83235, #98870 ),
 ( #10401, #25030, #57886 ),
 ( #67068, #74602, #99949 ),
 ( #42777, #58978, #91865 ),
 ( #17991, #75670, #3923 ),
 ( #37388, #95070, #20694 ),
 ( #13583, #53532, #53003 ),
 ( #54034, #44383, #3389 ) ),
 .UNSPECIFIED., .F., .F., .F. ) 
 B_SPLINE_SURFACE_WITH_KNOTS ( ( 4, 2, 2, 2, 2, 2, 4 ),
 ( 3, 3 ),
 ( 1.301042606982605321E-18, 0.002028361404254498158, 0.004056722808508994582, 0.006085084212763491006, 0.008113445617017987430, 0.01217016842552698028, 0.01622689123403597486 ),
 ( 0.000000000000000000, 1.000000000000000000 ),
 .UNSPECIFIED. ) 
 GEOMETRIC_REPRESENTATION_ITEM ( )  RATIONAL_B_SPLINE_SURFACE ( (
 ( 1.000000000000000000, 0.7071067811865473507, 1.000000000000000000),
 ( 1.000000000000000000, 0.7270538103684565101, 1.000000000000000000),
 ( 1.000000000000000000, 0.7474775509998854428, 1.000000000000000000),
 ( 1.000000000000000000, 0.7877120837788209595, 1.000000000000000000),
 ( 1.000000000000000000, 0.8076198138825669837, 1.000000000000000000),
 ( 1.000000000000000000, 0.8446812442347624295, 1.000000000000000000),
 ( 1.000000000000000000, 0.8620019270875391992, 1.000000000000000000),
 ( 1.000000000000000000, 0.8939173377915974328, 1.000000000000000000),
 ( 1.000000000000000000, 0.9085622752434662219, 1.000000000000000000),
 ( 1.000000000000000000, 0.9477746975872610724, 1.000000000000000000),
 ( 1.000000000000000000, 0.9672053386934328367, 1.000000000000000000),
 ( 1.000000000000000000, 0.9933317393956891950, 1.000000000000000000),
 ( 1.000000000000000000, 1.000004063029967805, 1.000000000000000000),
 ( 1.000000000000000000, 1.000000000000000000, 1.000000000000000000) ) ) 
 REPRESENTATION_ITEM ( '' )  SURFACE ( )  );
#41983 = CARTESIAN_POINT ( 'NONE',  ( 32.18022392672646959, 410.2513953074889628, 25.67977927016873352 ) ) ;
#41985 = AXIS2_PLACEMENT_3D ( 'NONE', #26853, #50526, #1985 ) ;
#41986 = CARTESIAN_POINT ( 'NONE',  ( -8.000000000000001776, -28.15624999999999645, 3.313708498984759387 ) ) ;
#41987 = CARTESIAN_POINT ( 'NONE',  ( 16.48350313421783753, 45.65798623861609684, 6.657797401561500017 ) ) ;
#41989 = EDGE_CURVE ( 'NONE', #9118, #94433, #102480, .T. ) ;
#41988 = ORIENTED_EDGE ( 'NONE', *, *, #64692, .F. ) ;
#41990 = CARTESIAN_POINT ( 'NONE',  ( 32.33349330513380693, 4.000000000000002665, 0.000000000000000000 ) ) ;
#41991 = CARTESIAN_POINT ( 'NONE',  ( 0.000000000000000000, 0.000000000000000000, -7.424942857142857733 ) ) ;
#41992 = AXIS2_PLACEMENT_3D ( 'NONE', #9800, #91809, #43779 ) ;
#41993 = DIRECTION ( 'NONE',  ( 1.000000000000000000, 0.000000000000000000, 0.000000000000000000 ) ) ;
#41994 = CARTESIAN_POINT ( 'NONE',  ( 4.154708322984343386E-08, -57.67120202538960427, 41.61186700422869933 ) ) ;
#41995 = CARTESIAN_POINT ( 'NONE',  ( -5.082755093536326818, -31.71875000204838457, 5.082755093536325042 ) ) ;
#41996 = CARTESIAN_POINT ( 'NONE',  ( -30.90663305326248889, 14.69720259819712815, 40.57123681776395330 ) ) ;
#41997 = CIRCLE ( 'NONE', #55751, 3.309500000000001663 ) ;
#41998 = FACE_BOUND ( 'NONE', #30613, .T. ) ;
#41999 = CARTESIAN_POINT ( 'NONE',  ( -7.090506018371190322, 41.24767894959148151, -58.61600934880981839 ) ) ;
#42000 = CARTESIAN_POINT ( 'NONE',  ( -89.90470572912276737, -30.00000000000002842, -11.15078749779565825 ) ) ;
#42001 = DIRECTION ( 'NONE',  ( 0.000000000000000000, 1.000000000000000000, 0.000000000000000000 ) ) ;
#42002 = CARTESIAN_POINT ( 'NONE',  ( -51.62104046282875203, -29.11573342958205757, 49.92149681681622297 ) ) ;
#42003 = CARTESIAN_POINT ( 'NONE',  ( 0.000000000000000000, 69.00000000000000000, 0.000000000000000000 ) ) ;
#42004 = ORIENTED_EDGE ( 'NONE', *, *, #42902, .F. ) ;
#42005 = CARTESIAN_POINT ( 'NONE',  ( -96.57186187874448535, -45.25305379375232206, 194.0755569586996216 ) ) ;
#42006 = CARTESIAN_POINT ( 'NONE',  ( -6.864655157840108046, 294.7328080983203336, -7.282300053873971279 ) ) ;
#42007 = CARTESIAN_POINT ( 'NONE',  ( 15.44560561439838331, -0.7538990090809657429, 14.98284401175013336 ) ) ;
#42008 = EDGE_LOOP ( 'NONE', ( #19933, #16191, #103666, #47926 ) ) ;
#42009 = CARTESIAN_POINT ( 'NONE',  ( -17.89161720275079759, 34.22760597788447257, -23.57693812718947513 ) ) ;
#42010 = CARTESIAN_POINT ( 'NONE',  ( 103.6076551382766979, -38.41969712729913766, 198.6980867907736297 ) ) ;
#42011 = DIRECTION ( 'NONE',  ( 0.000000000000000000, -1.000000000000000000, 0.000000000000000000 ) ) ;
#42012 = CARTESIAN_POINT ( 'NONE',  ( -5.290067270632269114, 51.34639538792298907, -8.531152949374520844 ) ) ;
#42013 = CARTESIAN_POINT ( 'NONE',  ( 9.250997389131581983, 0.000000000000000000, 5.000000000000002665 ) ) ;
#42014 = CARTESIAN_POINT ( 'NONE',  ( -41.92130353528092002, 485.3101580674256184, -3.082360575756684984 ) ) ;
#42015 = CARTESIAN_POINT ( 'NONE',  ( 91.62648505185801184, -30.00000000000000711, 190.7393155417504715 ) ) ;
#42016 = B_SPLINE_SURFACE_WITH_KNOTS ( 'NONE', 3, 3, ( 
 ( #55483, #73265, #64668, #98089 ),
 ( #40919, #7467, #15039, #48468 ),
 ( #71677, #90536, #97540, #24763 ),
 ( #89481, #98612, #32856, #73811 ),
 ( #106163, #56010, #57610, #23702 ),
 ( #15576, #47406, #24239, #40384 ),
 ( #14493, #23167, #72228, #72740 ),
 ( #16645, #8009, #65196, #6950 ),
 ( #57088, #81356, #47930, #6411 ),
 ( #88421, #49534, #38811, #90002 ),
 ( #16107, #64155, #31271, #80300 ),
 ( #48990, #104585, #105644, #97026 ),
 ( #31784, #88943, #106705, #30742 ),
 ( #63627, #39349, #96516, #22649 ),
 ( #105129, #10663, #84039, #91613 ),
 ( #100216, #41448, #60323, #34467 ),
 ( #41975, #26382, #68400, #2577 ),
 ( #59245, #75945, #25856, #35525 ),
 ( #67338, #92121, #17194, #100742 ),
 ( #83497, #26906, #76465, #59781 ),
 ( #52190, #101294, #51659, #2043 ),
 ( #17719, #84582, #43577, #27443 ),
 ( #33926, #414, #25301, #93196 ),
 ( #75406, #99140, #18266, #51121 ),
 ( #10142, #92656, #8543, #9597 ),
 ( #91087, #19362, #50068, #74340 ),
 ( #33381, #42509, #99686, #43056 ),
 ( #67856, #82976, #34988, #58712 ),
 ( #66256, #9070, #1503, #18817 ),
 ( #58159, #74859, #947, #66798 ),
 ( #50580, #69982, #61375, #78069 ),
 ( #28492, #102884, #3122, #60842 ),
 ( #93731, #19886, #29049, #77546 ),
 ( #45196, #12266, #4185, #36596 ),
 ( #52726, #37121, #3664, #85650 ),
 ( #85102, #69460, #61918, #11723 ),
 ( #94809, #86192, #78590, #94266 ),
 ( #20957, #53790, #53272, #86717 ),
 ( #12789, #45706, #11188, #44121 ),
 ( #77005, #36067, #68937, #101812 ),
 ( #44662, #27976, #102346, #20429 ),
 ( #101106, #10492, #1859, #9963 ),
 ( #92473, #27265, #43409, #84928 ),
 ( #1314, #60149, #34816, #93014 ),
 ( #50938, #35885, #75218, #74685 ),
 ( #35346, #19178, #67683, #18622 ),
 ( #52014, #42866, #59063, #100035 ),
 ( #33734, #83852, #93558, #84398 ),
 ( #2400, #100566, #91948, #59599 ),
 ( #17549, #26728, #91435, #51482 ),
 ( #50407, #68208, #11014, #26203 ),
 ( #76821, #76290, #75764, #43933 ),
 ( #767, #19706, #2930, #60671 ),
 ( #68763, #27800, #101643, #52542 ),
 ( #85462, #18079, #11547, #66611 ),
 ( #99491, #83320, #25669, #58532 ),
 ( #9412, #42328, #34275, #67151 ),
 ( #32910, #80894, #32382, #7005 ),
 ( #73322, #56614, #47987, #6471 ),
 ( #88479, #98665, #16701, #15629 ),
 ( #81413, #64212, #31330, #47463 ),
 ( #39925, #48522, #49049, #72281 ),
 ( #7524, #73867, #72797, #81946 ),
 ( #8069, #40442, #97082, #30796 ),
 ( #106762, #106219, #105701, #22705 ),
 ( #65254, #89538, #97600, #24296 ),
 ( #31844, #23225, #14554, #40979 ),
 ( #24817, #65787, #57669, #64726 ),
 ( #23766, #98144, #57145, #80356 ),
 ( #56065, #39403, #90592, #105184 ),
 ( #90058, #49592, #82500, #38867 ),
 ( #71734, #16162, #89006, #15100 ),
 ( #104644, #63682, #96570, #55542 ),
 ( #9124, #67910, #42034, #74916 ),
 ( #1000, #8601, #35046, #75995 ),
 ( #42562, #26435, #66853, #100797 ),
 ( #99742, #33982, #41503, #17780 ),
 ( #25912, #83033, #84630, #51173 ),
 ( #34522, #60376, #76522, #50633 ),
 ( #59838, #74391, #83551, #58768 ),
 ( #43107, #67391, #26957, #66312 ),
 ( #33438, #100273, #91666, #9651 ),
 ( #75464, #1557, #10717, #59300 ),
 ( #470, #35579, #18322, #68453 ),
 ( #2633, #99194, #92172, #84095 ),
 ( #10195, #2093, #92711, #101347 ),
 ( #18871, #51715, #43633, #27501 ),
 ( #93251, #19414, #52248, #58218 ),
 ( #25355, #91143, #17253, #50124 ),
 ( #93786, #11246, #95914, #95378 ),
 ( #45246, #13371, #94328, #21515 ),
 ( #52786, #87292, #28028, #38232 ),
 ( #61974, #12321, #21006, #3722 ),
 ( #19946, #79187, #12845, #53330 ),
 ( #54350, #11785, #46299, #94865 ),
 ( #53846, #5312, #86777, #71096 ),
 ( #30129, #103986, #102941, #45763 ),
 ( #63016, #78639, #4775, #44175 ),
 ( #85158, #29106, #102403, #85709 ),
 ( #77063, #86249, #69517, #44715 ),
 ( #77604, #3178, #70036, #22038 ),
 ( #37716, #36652, #28552, #62487 ),
 ( #36124, #70579, #103466, #68993 ),
 ( #29615, #101868, #61433, #60897 ),
 ( #20492, #78125, #4242, #37175 ),
 ( #75193, #66055, #6339, #90873 ),
 ( #72159, #39807, #55424, #104517 ),
 ( #71615, #80771, #16987, #30669 ),
 ( #33712, #39281, #105067, #74661 ),
 ( #79716, #6886, #31207, #47342 ),
 ( #22587, #64092, #58506, #96968 ),
 ( #50386, #91411, #219, #49865 ),
 ( #83299, #74135, #33183, #98932 ),
 ( #82771, #88879, #23103, #25092 ),
 ( #63557, #57949, #96450, #8874 ),
 ( #88357, #41778, #746, #66588 ),
 ( #17524, #99469, #55939, #25643 ),
 ( #87826, #1290, #9388, #42306 ),
 ( #34256, #67127, #100012, #54895 ),
 ( #13905, #14968, #46819, #5824 ),
 ( #38745, #14433, #80235, #47864 ),
 ( #1835, #10466, #59578, #68184 ),
 ( #20219, #101080, #19683, #27239 ),
 ( #60650, #43908, #35320, #100541 ),
 ( #75739, #85991, #3990, #2901 ),
 ( #68737, #51460, #18600, #34792 ),
 ( #93537, #60126, #35861, #36401 ),
 ( #61170, #101621, #44450, #27777 ),
 ( #52522, #94056, #85438, #77878 ),
 ( #67661, #10991, #43384, #26705 ),
 ( #92443, #92989, #76796, #53070 ),
 ( #84375, #59040, #91927, #19152 ),
 ( #76267, #12063, #2374, #18058 ),
 ( #69268, #9937, #51988, #11521 ),
 ( #84905, #3456, #77345, #36918 ),
 ( #102141, #28295, #44993, #69786 ),
 ( #26181, #42844, #50916, #83827 ),
 ( #61719, #94610, #78926, #14707 ),
 ( #87566, #39014, #86526, #103214 ),
 ( #29359, #62249, #79978, #70845 ),
 ( #104258, #63292, #6094, #70319 ),
 ( #54103, #22321, #103737, #87046 ) ),
 .UNSPECIFIED., .F., .F., .F.,
 ( 4, 3, 3, 3, 3, 3, 3, 3, 3, 3, 3, 3, 3, 3, 3, 3, 3, 3, 3, 3, 3, 3, 3, 3, 3, 3, 3, 3, 3, 3, 3, 3, 3, 3, 3, 3, 3, 3, 3, 3, 3, 3, 3, 3, 3, 3, 3, 4 ),
 ( 4, 4 ),
 ( 0.1961500227600059265, 0.1978441673325853079, 0.1995383119051646892, 0.2029266010503234796, 0.2046207456229028887, 0.2054678179091925794, 0.2063148901954822700, 0.2071619624817719607, 0.2080090347680616514, 0.2088561070543513420, 0.2097031793406410327, 0.2113973239132204140, 0.2130914684857998231, 0.2164797576309586136, 0.2181739022035379949, 0.2198680467761173762, 0.2232563359212761667, 0.2300329142115937198, 0.2368094925019113006, 0.2435860707922288537, 0.2503626490825464068, 0.2639158056631815130, 0.2774689622438166747, 0.2910221188244517809, 0.3045752754050868871, 0.3316815885663570995, 0.3452347451469922057, 0.3587879017276273119, 0.3655644800179448373, 0.3723410583082624181, 0.3791176365985799990, 0.3825059257437387616, 0.3858942148888975243, 0.3875883594614769057, 0.3892825040340562870, 0.3909766486066357238, 0.3926707931792151052, 0.3960590823243739234, 0.3977532268969533047, 0.3994473714695326860, 0.4011415160421120674, 0.4028356606146914487, 0.4062239497598502114, 0.4079180943324295927, 0.4096122389050089740, 0.4104593111912986925, 0.4113063834775884109, 0.4130005280501677922 ),
 ( 0.03879960281305409181, 0.7822234871750797236 ),
 .UNSPECIFIED. ) ;
#42017 = CARTESIAN_POINT ( 'NONE',  ( 37.08530234602800135, 491.4084519804410434, 12.30481897466681218 ) ) ;
#42018 = CARTESIAN_POINT ( 'NONE',  ( -35.96984888422242221, 491.2799073994592618, 12.80368214530777848 ) ) ;
#42019 = ADVANCED_FACE ( 'NONE', ( #104351 ), #55262, .F. ) ;
#42020 = CARTESIAN_POINT ( 'NONE',  ( -18.99999999999999289, 4.000000000000000888, 25.00000000000000000 ) ) ;
#42021 = VECTOR ( 'NONE', #89108, 1000.000000000000000 ) ;
#42022 = ORIENTED_EDGE ( 'NONE', *, *, #88752, .F. ) ;
#42023 = ORIENTED_EDGE ( 'NONE', *, *, #51531, .T. ) ;
#42024 = CARTESIAN_POINT ( 'NONE',  ( 51.93105796537405894, -53.37078366791337913, 59.21816737527645813 ) ) ;
#42025 = CARTESIAN_POINT ( 'NONE',  ( 6.338673411933466895, 41.81695763293575396, -59.02782193812689115 ) ) ;
#42026 = CARTESIAN_POINT ( 'NONE',  ( 36.35746645901171803, 28.12773496632032533, -12.56232177387087212 ) ) ;
#42027 = ADVANCED_FACE ( 'NONE', ( #18562 ), #99547, .T. ) ;
#42028 = VERTEX_POINT ( 'NONE', #17492 ) ;
#42029 = CARTESIAN_POINT ( 'NONE',  ( -101.2361249591687482, -38.35621429768038837, 95.68744428954927628 ) ) ;
#42030 = ORIENTED_EDGE ( 'NONE', *, *, #29658, .F. ) ;
#42031 = CARTESIAN_POINT ( 'NONE',  ( 16.14595037822608958, 7.274337365584589321, 6.616591826375514351 ) ) ;
#42032 = CARTESIAN_POINT ( 'NONE',  ( 91.93880928415951814, -38.35394051711806895, 34.15909317860170091 ) ) ;
#42033 = CARTESIAN_POINT ( 'NONE',  ( 13.79123284555586082, 22.99122672343318285, 0.4943395215415997135 ) ) ;
#42034 = CARTESIAN_POINT ( 'NONE',  ( 92.71638314794412850, -45.28274863744896095, 87.13263043128905849 ) ) ;
#42035 = CARTESIAN_POINT ( 'NONE',  ( 109.3513501059324255, -38.00000000000000000, 179.6549720493207190 ) ) ;
#42036 = CARTESIAN_POINT ( 'NONE',  ( 34.50120583711849775, 434.4753093497994314, 9.494494844945867484 ) ) ;
#42037 = CARTESIAN_POINT ( 'NONE',  ( -27.64766936045855772, 308.1634638491052556, -9.255587232834342259 ) ) ;
#42038 = AXIS2_PLACEMENT_3D ( 'NONE', #16761, #22766, #52311 ) ;
#42039 = CARTESIAN_POINT ( 'NONE',  ( 4.856731536730760190, -63.85066234079124570, 12.98722588752802309 ) ) ;
#42040 = CARTESIAN_POINT ( 'NONE',  ( 76.36008957498899008, -59.99999999999998579, 188.3857483048130916 ) ) ;
#42041 = CARTESIAN_POINT ( 'NONE',  ( -34.26493447578224760, 490.0907185571355740, 11.27927472376731544 ) ) ;
#42042 = EDGE_CURVE ( 'NONE', #23078, #62090, #75162, .T. ) ;
#42043 = CARTESIAN_POINT ( 'NONE',  ( 18.02665060324837398, 45.00000000000000711, 62.54981906107154543 ) ) ;
#42044 = VERTEX_POINT ( 'NONE', #16407 ) ;
#42045 = CARTESIAN_POINT ( 'NONE',  ( 60.96321612378304877, -18.64603658371650852, 64.94373476075919882 ) ) ;
#42046 = CARTESIAN_POINT ( 'NONE',  ( -25.53351597638959092, 295.7776190944981067, -1.801019599846679142 ) ) ;
#42047 = CARTESIAN_POINT ( 'NONE',  ( 12.33349330513380337, 1.593028355512270567E-15, 0.000000000000000000 ) ) ;
#42048 = CARTESIAN_POINT ( 'NONE',  ( -9.366761589750341344, -5.000000000000001776, -18.69503824872587572 ) ) ;
#42050 = CARTESIAN_POINT ( 'NONE',  ( -35.04037255257541972, 484.2364580523164932, -0.9782185570580150813 ) ) ;
#42049 = CARTESIAN_POINT ( 'NONE',  ( -60.77962921676822816, -30.00000000004004974, 94.17698026533876998 ) ) ;
#42051 = CARTESIAN_POINT ( 'NONE',  ( -39.28811459529073602, 326.5013068576240585, 17.64810832725432022 ) ) ;
#42052 = CARTESIAN_POINT ( 'NONE',  ( -32.80441372020654711, 485.2966253772736991, 5.899827864538937483 ) ) ;
#42053 = CARTESIAN_POINT ( 'NONE',  ( 0.000000000000000000, -5.629165124598843661, 3.250000000000011990 ) ) ;
#42054 = CARTESIAN_POINT ( 'NONE',  ( -3.313708498984765161, -26.46874999999999645, 7.999999999999998224 ) ) ;
#42055 = CARTESIAN_POINT ( 'NONE',  ( -18.91791044776116237, 46.94999999999998153, 62.18611311450883505 ) ) ;
#42056 = CARTESIAN_POINT ( 'NONE',  ( -7.500000000000002665, -4.999999999999998224, -68.91429205908086431 ) ) ;
#42057 = ORIENTED_EDGE ( 'NONE', *, *, #63462, .T. ) ;
#42058 = CARTESIAN_POINT ( 'NONE',  ( 85.42082578164037443, -25.35066044882315950, 171.5601627925657340 ) ) ;
#42059 = CARTESIAN_POINT ( 'NONE',  ( 43.49287295680601773, 484.8086259266613069, 4.190157679464852514 ) ) ;
#42060 = DIRECTION ( 'NONE',  ( 0.000000000000000000, -1.000000000000000000, 0.000000000000000000 ) ) ;
#42061 = EDGE_LOOP ( 'NONE', ( #61794, #88, #105406, #52217 ) ) ;
#42062 = DIRECTION ( 'NONE',  ( -0.5735764363510459374, -0.8191520442889919096, 0.000000000000000000 ) ) ;
#42063 = CIRCLE ( 'NONE', #14475, 5.000000000000001776 ) ;
#42064 = CARTESIAN_POINT ( 'NONE',  ( 42.20041562234358423, 435.2369744135583574, 7.788607701745476675 ) ) ;
#42065 = CARTESIAN_POINT ( 'NONE',  ( 15.17227823171669243, -3.000000000000002665, -86.54073391195466058 ) ) ;
#42066 = CARTESIAN_POINT ( 'NONE',  ( -14.96496930756238619, -24.06842715425924339, -38.53085418151248831 ) ) ;
#42067 = CARTESIAN_POINT ( 'NONE',  ( -6.905560911067180285, -0.02023367412855946526, 19.00754324974943188 ) ) ;
#42068 = AXIS2_PLACEMENT_3D ( 'NONE', #74951, #49624, #67423 ) ;
#42069 = EDGE_CURVE ( 'NONE', #67861, #33365, #27248, .T. ) ;
#42070 = AXIS2_PLACEMENT_3D ( 'NONE', #22357, #45553, #87074 ) ;
#42071 = CARTESIAN_POINT ( 'NONE',  ( 53.63744806657462760, -60.00000000000000000, 81.41419112139796255 ) ) ;
#42072 = CARTESIAN_POINT ( 'NONE',  ( 7.344361273354512498, 107.4456053058852518, -3.175733139645587677 ) ) ;
#42073 = CARTESIAN_POINT ( 'NONE',  ( 11.01895070290840017, -14.02256158417551468, 31.84177124770781120 ) ) ;
#42074 = EDGE_CURVE ( 'NONE', #55179, #24268, #42660, .T. ) ;
#42075 = EDGE_CURVE ( 'NONE', #10653, #81483, #106396, .T. ) ;
#42077 = CARTESIAN_POINT ( 'NONE',  ( -12.53238701598708182, 20.76954288979780117, -6.334205635054888539 ) ) ;
#42076 = CARTESIAN_POINT ( 'NONE',  ( -22.02381810701088227, -27.03152908169614577, 37.34294290578310438 ) ) ;
#42078 = CARTESIAN_POINT ( 'NONE',  ( 33.00000000000000000, 500.0000000000002274, 0.000000000000000000 ) ) ;
#42079 = CARTESIAN_POINT ( 'NONE',  ( -7.188101187500002709, -15.31250000204838457, 2.977408999572648707 ) ) ;
#42080 = DIRECTION ( 'NONE',  ( 0.000000000000000000, 0.000000000000000000, 1.000000000000000000 ) ) ;
#42081 = ORIENTED_EDGE ( 'NONE', *, *, #42575, .T. ) ;
#42082 = CARTESIAN_POINT ( 'NONE',  ( -17.50000000000917311, 50.03760136707322204, 61.20291971386541263 ) ) ;
#42083 = CARTESIAN_POINT ( 'NONE',  ( -9.389245980427300964, -2.447416405268218131, 14.81682632889905626 ) ) ;
#42084 = CARTESIAN_POINT ( 'NONE',  ( -37.54559764570181812, 464.1143081516144662, 19.43664670202813838 ) ) ;
#42086 = CARTESIAN_POINT ( 'NONE',  ( 28.41466101814540579, -34.58967673365405204, -31.03063672134422291 ) ) ;
#42085 = CARTESIAN_POINT ( 'NONE',  ( 4.063294091762369220, 54.18592360713469702, 6.990124018066343758 ) ) ;
#42087 = EDGE_CURVE ( 'NONE', #72021, #25938, #11498, .T. ) ;
#42088 = EDGE_LOOP ( 'NONE', ( #101201, #21306, #44538, #28417, #82383 ) ) ;
#42089 = CARTESIAN_POINT ( 'NONE',  ( -5.911778709945830101, -88.86661839416575503, 1.058844270818174227 ) ) ;
#42090 = CARTESIAN_POINT ( 'NONE',  ( 0.000000000000000000, -4.000000000000003553, 27.00000000000000000 ) ) ;
#42091 = EDGE_LOOP ( 'NONE', ( #26913, #53915, #35941, #96761 ) ) ;
#42092 = EDGE_CURVE ( 'NONE', #35042, #42028, #96101, .T. ) ;
#42093 = DIRECTION ( 'NONE',  ( 1.000000000000000000, 0.000000000000000000, 0.000000000000000000 ) ) ;
#42094 = DIRECTION ( 'NONE',  ( -1.000000000000000000, -0.000000000000000000, -0.000000000000000000 ) ) ;
#42095 = CARTESIAN_POINT ( 'NONE',  ( -14.91271302809441401, 41.98564543112699710, -86.62215342991694911 ) ) ;
#42096 = AXIS2_PLACEMENT_3D ( 'NONE', #18608, #76806, #77887 ) ;
#42097 = CARTESIAN_POINT ( 'NONE',  ( -100.8778939643891022, -59.99999999999999289, 86.18389089348301013 ) ) ;
#42098 = CARTESIAN_POINT ( 'NONE',  ( 17.50000000000000711, 2.500000000000000444, 25.00000000000000000 ) ) ;
#42099 = AXIS2_PLACEMENT_3D ( 'NONE', #56596, #47446, #99587 ) ;
#42100 = DIRECTION ( 'NONE',  ( 0.000000000000000000, -1.000000000000000000, 0.000000000000000000 ) ) ;
#42101 = DIRECTION ( 'NONE',  ( 0.000000000000000000, 0.000000000000000000, 1.000000000000000000 ) ) ;
#42102 = CARTESIAN_POINT ( 'NONE',  ( 42.00989057911306190, 460.5566595377485442, 2.543045191523135351 ) ) ;
#42104 = CARTESIAN_POINT ( 'NONE',  ( 30.00000000000077094, 487.0612273928530840, 5.833475372789068025 ) ) ;
#42103 = CARTESIAN_POINT ( 'NONE',  ( -9.739726766104286781, -3.000000000000002665, -87.61747884499033034 ) ) ;
#42105 = CARTESIAN_POINT ( 'NONE',  ( -86.03581629327824487, -18.41222013102441224, 166.1572250011447238 ) ) ;
#42106 = ORIENTED_EDGE ( 'NONE', *, *, #89195, .F. ) ;
#42107 = CIRCLE ( 'NONE', #62850, 5.000000000000011546 ) ;
#42108 = CARTESIAN_POINT ( 'NONE',  ( 7.000000000000000000, 0.000000000000000000, -2.575493252495433261 ) ) ;
#42109 = ORIENTED_EDGE ( 'NONE', *, *, #76115, .T. ) ;
#42110 = ORIENTED_EDGE ( 'NONE', *, *, #1490, .T. ) ;
#42111 = FACE_OUTER_BOUND ( 'NONE', #88215, .T. ) ;
#42112 = PRESENTATION_STYLE_ASSIGNMENT (( #35124 ) ) ;
#42113 = ORIENTED_EDGE ( 'NONE', *, *, #84282, .F. ) ;
#42114 = CARTESIAN_POINT ( 'NONE',  ( 31.95108112711128001, 486.7719899256358644, 6.757615638381732737 ) ) ;
#42115 = DIRECTION ( 'NONE',  ( -1.000000000000000000, -0.000000000000000000, -0.000000000000000000 ) ) ;
#42116 = DIRECTION ( 'NONE',  ( 0.000000000000000000, -1.000000000000000000, 0.000000000000000000 ) ) ;
#42117 = CARTESIAN_POINT ( 'NONE',  ( 16.36650669486618881, 1.474610560812782335E-15, 0.000000000000000000 ) ) ;
#42118 = CARTESIAN_POINT ( 'NONE',  ( -13.38090213880806978, -54.00000000000000711, 31.11721482942554928 ) ) ;
#42119 = LINE ( 'NONE', #27589, #65722 ) ;
#42120 = CARTESIAN_POINT ( 'NONE',  ( 108.8020855619825653, -30.00000000000001066, 184.6883589252716433 ) ) ;
#42121 = EDGE_CURVE ( 'NONE', #12685, #35979, #84010, .T. ) ;
#42122 = CARTESIAN_POINT ( 'NONE',  ( -105.3891558216856339, -14.21045842199431064, 188.2119682431835486 ) ) ;
#42123 = CARTESIAN_POINT ( 'NONE',  ( -59.28942817012108435, -60.34107446338563108, 80.30105261389887517 ) ) ;
#42124 = ORIENTED_EDGE ( 'NONE', *, *, #71955, .T. ) ;
#42125 = DIRECTION ( 'NONE',  ( 0.000000000000000000, 0.000000000000000000, 1.000000000000000000 ) ) ;
#42126 = CARTESIAN_POINT ( 'NONE',  ( 99.44641300720719812, -60.00000000003898748, 63.07692230255130283 ) ) ;
#42127 = ORIENTED_EDGE ( 'NONE', *, *, #73180, .T. ) ;
#42128 = CARTESIAN_POINT ( 'NONE',  ( 5.121475308325913467, -49.91563172172032381, 32.19864153987534650 ) ) ;
#42129 = CARTESIAN_POINT ( 'NONE',  ( -102.4774247092255735, -37.82049968165720344, 163.3363480242135211 ) ) ;
#42130 = CARTESIAN_POINT ( 'NONE',  ( 7.188101187500000933, -16.43750000204838813, -2.977408999572650483 ) ) ;
#42131 = CARTESIAN_POINT ( 'NONE',  ( -5.902907888919633805, -5.000000000000000888, -73.20788160634965891 ) ) ;
#42132 = CARTESIAN_POINT ( 'NONE',  ( 0.000000000000000000, 1.500000000000000888, 0.000000000000000000 ) ) ;
#42133 = ORIENTED_EDGE ( 'NONE', *, *, #67138, .T. ) ;
#42134 = LINE ( 'NONE', #41614, #30395 ) ;
#42135 = CARTESIAN_POINT ( 'NONE',  ( -27.99608589347343823, -60.00000000000002132, 42.10196603562540218 ) ) ;
#42136 = CARTESIAN_POINT ( 'NONE',  ( 9.423772032809306864, -56.01307627480206008, 23.65101655106710510 ) ) ;
#42137 = CARTESIAN_POINT ( 'NONE',  ( 7.188101187500000044, -19.53125000204838457, 0.000000000000000000 ) ) ;
#42138 = DIRECTION ( 'NONE',  ( -1.000000000000000000, -0.000000000000000000, -0.000000000000000000 ) ) ;
#42139 = FILL_AREA_STYLE_COLOUR ( '', #13339 ) ;
#42140 = CIRCLE ( 'NONE', #102440, 4.000000000000000888 ) ;
#42141 = DIRECTION ( 'NONE',  ( -1.000000000000000000, -1.224606353822377258E-16, -0.000000000000000000 ) ) ;
#42142 = CARTESIAN_POINT ( 'NONE',  ( 33.58349330513380693, 4.898587196589411843E-16, -4.000000000000001776 ) ) ;
#42143 = FACE_OUTER_BOUND ( 'NONE', #6546, .T. ) ;
#42144 = CARTESIAN_POINT ( 'NONE',  ( 3.808169938200466120, -9.155691705081260068, 13.42225449006559579 ) ) ;
#42145 = CARTESIAN_POINT ( 'NONE',  ( -24.23707248033654693, 27.31414015027108277, 32.69896640055586090 ) ) ;
#42146 = ADVANCED_FACE ( 'NONE', ( #10433 ), #72235, .F. ) ;
#42147 = CARTESIAN_POINT ( 'NONE',  ( 105.0341561612351455, -60.00000000000000000, 150.3407643626507024 ) ) ;
#42148 = CIRCLE ( 'NONE', #38029, 10.00000000000000178 ) ;
#42149 = CARTESIAN_POINT ( 'NONE',  ( -32.17252970384051736, -49.90654965793798681, 35.87652722567293040 ) ) ;
#42150 = ADVANCED_FACE ( 'NONE', ( #36366 ), #58213, .T. ) ;
#42151 = CARTESIAN_POINT ( 'NONE',  ( -0.9999999999999941158, -50.00000000000000000, 101.0455488498966758 ) ) ;
#42152 = CARTESIAN_POINT ( 'NONE',  ( 44.27463941397954272, -56.79608921835394142, 47.30910395297117077 ) ) ;
#42153 = CARTESIAN_POINT ( 'NONE',  ( -32.84444940698905668, 439.0476299206102340, 24.86213004146479122 ) ) ;
#42154 = ORIENTED_EDGE ( 'NONE', *, *, #26967, .T. ) ;
#42155 = EDGE_CURVE ( 'NONE', #60873, #50065, #2339, .T. ) ;
#42156 = CARTESIAN_POINT ( 'NONE',  ( 43.63899620156486492, 434.3182181978404515, 14.37213632273144448 ) ) ;
#42157 = EDGE_CURVE ( 'NONE', #10334, #62320, #22060, .T. ) ;
#42158 = CARTESIAN_POINT ( 'NONE',  ( -80.09466378707983836, -38.78899114093880485, 193.1579810679791365 ) ) ;
#42159 = ORIENTED_EDGE ( 'NONE', *, *, #47226, .T. ) ;
#42161 = DIRECTION ( 'NONE',  ( 0.5735764363510554853, 0.8191520442889852482, 0.000000000000000000 ) ) ;
#42160 = CARTESIAN_POINT ( 'NONE',  ( 4.852941176470587870, 25.66666666666755248, -70.80672828634229177 ) ) ;
#42162 = CARTESIAN_POINT ( 'NONE',  ( 31.81267353152397703, -59.99999999999999289, 37.51807302839154801 ) ) ;
#42163 = CARTESIAN_POINT ( 'NONE',  ( 8.866506694866188809, 1.474610560812782335E-15, 0.000000000000000000 ) ) ;
#42164 = CARTESIAN_POINT ( 'NONE',  ( 6.338278980374676408, -2.729992536301781403, 6.499999999999998224 ) ) ;
#42165 = CARTESIAN_POINT ( 'NONE',  ( 9.090909090909089940, 16.00000000000000000, -4.165977904505312246 ) ) ;
#42166 = DIRECTION ( 'NONE',  ( 0.000000000000000000, 1.000000000000000000, 0.000000000000000000 ) ) ;
#42167 = CARTESIAN_POINT ( 'NONE',  ( 5.910690929868580135, -88.86495906093198016, -1.065041252563905028 ) ) ;
#42168 = CARTESIAN_POINT ( 'NONE',  ( 106.3905019650464396, -60.00000000000000711, 118.8348382975589885 ) ) ;
#42169 = CARTESIAN_POINT ( 'NONE',  ( -5.911697307506504906, -50.52686870766020633, 39.69124793001901708 ) ) ;
#42170 = EDGE_CURVE ( 'NONE', #15028, #77225, #12030, .T. ) ;
#42171 = SURFACE_STYLE_USAGE ( .BOTH. , #610 ) ;
#42172 = EDGE_LOOP ( 'NONE', ( #91592, #65395, #27667, #72675 ) ) ;
#42173 = CONICAL_SURFACE ( 'NONE', #45582, 5.000000000000010658, 0.9599310885968697082 ) ;
#42174 = CARTESIAN_POINT ( 'NONE',  ( -97.88751494666014707, -30.00000000000000711, 190.6366788456940924 ) ) ;
#42175 = VERTEX_POINT ( 'NONE', #84870 ) ;
#42176 = DIRECTION ( 'NONE',  ( -1.000000000000000000, -1.224606353822377258E-16, -0.000000000000000000 ) ) ;
#42177 = CARTESIAN_POINT ( 'NONE',  ( 18.58349330513380693, -4.000000000000000888, 4.898587196589416773E-16 ) ) ;
#42178 = SURFACE_SIDE_STYLE ('',( #59450 ) ) ;
#42179 = CARTESIAN_POINT ( 'NONE',  ( 9.253583916535172094, 28.70196091994965570, 3.792462592445553948 ) ) ;
#42180 = CARTESIAN_POINT ( 'NONE',  ( -2.977408999572654480, -21.50000000204839168, 7.188101187499999156 ) ) ;
#42181 = CIRCLE ( 'NONE', #61143, 4.000000000000001776 ) ;
#42182 = AXIS2_PLACEMENT_3D ( 'NONE', #58614, #76367, #100120 ) ;
#42183 = AXIS2_PLACEMENT_3D ( 'NONE', #32057, #82164, #99396 ) ;
#42184 = CARTESIAN_POINT ( 'NONE',  ( 30.06732394248781048, 17.62925877149445597, -39.66393268825159879 ) ) ;
#42185 = VECTOR ( 'NONE', #38585, 1000.000000000000000 ) ;
#42187 = EDGE_LOOP ( 'NONE', ( #62481, #5388 ) ) ;
#42186 = FILL_AREA_STYLE ('',( #92326 ) ) ;
#42188 = CARTESIAN_POINT ( 'NONE',  ( 85.01890593301797594, -22.07538763286781602, 160.8954594108710126 ) ) ;
#42189 = DIRECTION ( 'NONE',  ( 1.000000000000000000, 0.000000000000000000, 0.000000000000000000 ) ) ;
#42190 = STYLED_ITEM ( 'NONE', ( #70558 ), #86403 ) ;
#42191 = CARTESIAN_POINT ( 'NONE',  ( 9.381394091586569672, 87.01349605581610547, 3.465950112474255551 ) ) ;
#42192 = VERTEX_POINT ( 'NONE', #37419 ) ;
#42193 = CARTESIAN_POINT ( 'NONE',  ( -6.999999999999993783, -50.00000000000000000, 102.2532056551910387 ) ) ;
#42194 =( NAMED_UNIT ( * ) PLANE_ANGLE_UNIT ( ) SI_UNIT ( $, .RADIAN. ) );
#42195 = DIRECTION ( 'NONE',  ( -1.000000000000000000, -0.000000000000000000, -0.000000000000000000 ) ) ;
#42196 = CARTESIAN_POINT ( 'NONE',  ( 19.00000000000001421, -4.999999999999999112, -1.500000000000000000 ) ) ;
#42197 = DIRECTION ( 'NONE',  ( -0.5735764363510497121, 0.8191520442889892450, 1.003171929053521665E-16 ) ) ;
#42198 = CARTESIAN_POINT ( 'NONE',  ( -27.50149470030765286, 307.8944781523804863, 11.11325752724550497 ) ) ;
#42199 = FACE_OUTER_BOUND ( 'NONE', #9813, .T. ) ;
#42200 = ORIENTED_EDGE ( 'NONE', *, *, #85294, .F. ) ;
#42201 = ADVANCED_FACE ( 'NONE', ( #70284 ), #44960, .F. ) ;
#42202 = SHAPE_REPRESENTATION_RELATIONSHIP ( 'NONE' , 'NONE' ,  #81203, #34531 ) ;
#42203 = CARTESIAN_POINT ( 'NONE',  ( -1.700304210406924588, 301.6922864547469203, 9.856359514573828307 ) ) ;
#42204 = CARTESIAN_POINT ( 'NONE',  ( 14.89104587296188242, 23.12241641510997070, 0.2537601492100622913 ) ) ;
#42205 = ADVANCED_FACE ( 'NONE', ( #14666 ), #89117, .T. ) ;
#42206 = ADVANCED_FACE ( 'NONE', ( #78890 ), #56177, .T. ) ;
#42207 = CARTESIAN_POINT ( 'NONE',  ( 6.849999999999999645, 4.618802153517004960, 7.999999999999998224 ) ) ;
#42208 = CARTESIAN_POINT ( 'NONE',  ( -7.188101187500001821, -32.00000000204838813, -2.977408999572651371 ) ) ;
#42209 = CARTESIAN_POINT ( 'NONE',  ( 20.34580746390948747, 294.7747570175440615, -2.016376581567297155 ) ) ;
#42210 = CARTESIAN_POINT ( 'NONE',  ( 8.400221614534629566, 51.89221066646364022, 1.531152949373683958 ) ) ;
#42211 = ITEM_DEFINED_TRANSFORMATION ( 'NONE', 'NONE', #57599,  #10728 ) ;
#42212 = CARTESIAN_POINT ( 'NONE',  ( 49.27082696441105014, 7.795205586015218735, 15.75806003941683109 ) ) ;
#42213 = ORIENTED_EDGE ( 'NONE', *, *, #16066, .T. ) ;
#42214 = DIRECTION ( 'NONE',  ( 0.000000000000000000, -1.000000000000000000, 0.000000000000000000 ) ) ;
#42215 = DIRECTION ( 'NONE',  ( 0.000000000000000000, 0.000000000000000000, -1.000000000000000000 ) ) ;
#42216 = LINE ( 'NONE', #9842, #58405 ) ;
#42217 = ADVANCED_FACE ( 'NONE', ( #72117 ), #48601, .T. ) ;
#42218 = VERTEX_POINT ( 'NONE', #63791 ) ;
#42219 = DIRECTION ( 'NONE',  ( -0.000000000000000000, -0.000000000000000000, -1.000000000000000000 ) ) ;
#42220 = CARTESIAN_POINT ( 'NONE',  ( 107.5689571876914385, -57.67123018601353834, 113.8109351001579341 ) ) ;
#42221 = ADVANCED_FACE ( 'NONE', ( #39516 ), #46529, .F. ) ;
#42222 = CARTESIAN_POINT ( 'NONE',  ( 33.97359119245065529, 434.1099241184708148, 11.80501937577158245 ) ) ;
#42223 = CARTESIAN_POINT ( 'NONE',  ( 0.2692838627284316333, 13.85270131633357593, 7.000000000000015099 ) ) ;
#42224 = CARTESIAN_POINT ( 'NONE',  ( 38.86650669486618881, -3.851859888774471706E-31, 4.000000000000000888 ) ) ;
#42225 = CARTESIAN_POINT ( 'NONE',  ( 23.15769230769230802, 1.411358822780289120E-15, 0.000000000000000000 ) ) ;
#42226 = CARTESIAN_POINT ( 'NONE',  ( -79.72788990572331613, -60.00000000000000711, 195.6396468098284345 ) ) ;
#42227 = CARTESIAN_POINT ( 'NONE',  ( -7.500000000000003553, 18.65452285268246513, -40.72535638071818909 ) ) ;
#42228 = DIRECTION ( 'NONE',  ( 0.000000000000000000, -1.000000000000000000, 0.000000000000000000 ) ) ;
#42229 = EDGE_CURVE ( 'NONE', #105636, #87282, #35869, .T. ) ;
#42230 = CARTESIAN_POINT ( 'NONE',  ( -44.43774958859658142, 337.2802145563449017, 0.2445019049555710311 ) ) ;
#42231 = CARTESIAN_POINT ( 'NONE',  ( -83.99837553685419778, -46.55898069261829164, 184.5992319689315195 ) ) ;
#42232 = ORIENTED_EDGE ( 'NONE', *, *, #63842, .T. ) ;
#42233 = ORIENTED_EDGE ( 'NONE', *, *, #16509, .F. ) ;
#42234 = DIRECTION ( 'NONE',  ( -1.000000000000000000, -1.224606353822377258E-16, -0.000000000000000000 ) ) ;
#42236 = CARTESIAN_POINT ( 'NONE',  ( -1.370335905996620722E-14, 22.97884757028485225, 55.94820918777160301 ) ) ;
#42235 = AXIS2_PLACEMENT_3D ( 'NONE', #44308, #30805, #63151 ) ;
#42237 = CARTESIAN_POINT ( 'NONE',  ( -84.44893624074092031, -45.27054077215418459, -4.593890189075327868 ) ) ;
#42238 = SURFACE_STYLE_FILL_AREA ( #76729 ) ;
#42239 = CARTESIAN_POINT ( 'NONE',  ( 1.255263095696489281E-15, 51.26930509877138320, 10.24999999999999822 ) ) ;
#42240 = AXIS2_PLACEMENT_3D ( 'NONE', #106090, #90458, #33307 ) ;
#42241 = CARTESIAN_POINT ( 'NONE',  ( 0.000000000000000000, 70.00000000000000000, 0.000000000000000000 ) ) ;
#42242 = CARTESIAN_POINT ( 'NONE',  ( -23.21751746555280249, 27.38103382803677022, -33.20617127781034839 ) ) ;
#42243 = CARTESIAN_POINT ( 'NONE',  ( -47.37019975542479955, 42.00000000008224532, -36.40416150956886554 ) ) ;
#42244 = CARTESIAN_POINT ( 'NONE',  ( 8.349999999999999645, 1.411358822780289120E-15, 0.000000000000000000 ) ) ;
#42245 = CARTESIAN_POINT ( 'NONE',  ( 1.425929562426998531, -60.00000000000000000, 41.99999999999999289 ) ) ;
#42246 = LINE ( 'NONE', #57359, #65187 ) ;
#42247 = CARTESIAN_POINT ( 'NONE',  ( 25.62974135805828979, -60.00000000000002132, -43.76006462505735328 ) ) ;
#42248 = CARTESIAN_POINT ( 'NONE',  ( -68.29106402824945121, -42.96295712507508568, 98.34947639744338233 ) ) ;
#42249 = ORIENTED_EDGE ( 'NONE', *, *, #35850, .F. ) ;
#42250 = CARTESIAN_POINT ( 'NONE',  ( 66.35352848486118660, -59.99999999999995737, 134.7740243497364645 ) ) ;
#42251 = CARTESIAN_POINT ( 'NONE',  ( 7.619753052866894194, 88.17451502807173824, -2.447276542590444137 ) ) ;
#42252 = CARTESIAN_POINT ( 'NONE',  ( 114.0552712960643618, -57.67113080223169419, 166.1762645039309803 ) ) ;
#42253 = MECHANICAL_DESIGN_GEOMETRIC_PRESENTATION_REPRESENTATION (  '', ( #18199 ), #52573 ) ;
#42255 = ORIENTED_EDGE ( 'NONE', *, *, #100036, .F. ) ;
#42254 = CIRCLE ( 'NONE', #56009, 2.000000000000000000 ) ;
#42256 = CARTESIAN_POINT ( 'NONE',  ( 6.999999999999998224, -12.54465221550629472, 8.223849511755000563 ) ) ;
#42257 = CARTESIAN_POINT ( 'NONE',  ( 0.000000000000000000, 0.000000000000000000, -5.000000000000003553 ) ) ;
#42258 = ORIENTED_EDGE ( 'NONE', *, *, #95099, .T. ) ;
#42259 = CARTESIAN_POINT ( 'NONE',  ( 0.9250510724394636064, 13.95888890799997384, -6.939834513072449695 ) ) ;
#42260 = PRESENTATION_STYLE_ASSIGNMENT (( #27191 ) ) ;
#42261 = DIRECTION ( 'NONE',  ( -0.000000000000000000, -1.000000000000000000, -0.000000000000000000 ) ) ;
#42262 = CARTESIAN_POINT ( 'NONE',  ( 7.188101187500000044, -13.15625000204838280, 0.000000000000000000 ) ) ;
#42263 = CARTESIAN_POINT ( 'NONE',  ( 43.59536836154811823, 485.3411848763689704, 3.528079522877425322 ) ) ;
#42264 = CIRCLE ( 'NONE', #59469, 4.000000000000001776 ) ;
#42265 = CARTESIAN_POINT ( 'NONE',  ( 24.41571844174603356, -4.285714285714295357, -6.539732759932822326 ) ) ;
#42266 = CARTESIAN_POINT ( 'NONE',  ( 27.10511071441176867, -1.200000000000000030E-05, -10.05698433968634653 ) ) ;
#42267 = CARTESIAN_POINT ( 'NONE',  ( 12.39854599882998976, 8.430153398135438181, -12.16137996778342334 ) ) ;
#42268 = DIRECTION ( 'NONE',  ( 0.000000000000000000, 0.000000000000000000, 1.000000000000000000 ) ) ;
#42269 = CARTESIAN_POINT ( 'NONE',  ( 7.855360403618686149, 47.99999999999999289, -97.83275449052108286 ) ) ;
#42271 = EDGE_CURVE ( 'NONE', #93202, #82322, #71329, .T. ) ;
#42270 = UNCERTAINTY_MEASURE_WITH_UNIT (LENGTH_MEASURE( 1.000000000000000082E-05 ), #5767, 'distance_accuracy_value', 'NONE');
#42272 = VERTEX_POINT ( 'NONE', #87531 ) ;
#42273 = CARTESIAN_POINT ( 'NONE',  ( -7.226138746538454782, 41.34018742858377493, -70.07054302848561633 ) ) ;
#42275 = CARTESIAN_POINT ( 'NONE',  ( 33.29269151129017956, -53.36740787830309074, 37.05142291644975217 ) ) ;
#42274 = CARTESIAN_POINT ( 'NONE',  ( 16.75187969033515145, -1.200000000000000030E-05, -23.05698433968624528 ) ) ;
#42276 = CARTESIAN_POINT ( 'NONE',  ( 35.30917598036950267, 361.3009821353402344, 3.520162773547422574 ) ) ;
#42277 = ORIENTED_EDGE ( 'NONE', *, *, #19505, .T. ) ;
#42278 = ADVANCED_FACE ( 'NONE', ( #30909 ), #51271, .T. ) ;
#42279 = CARTESIAN_POINT ( 'NONE',  ( -0.1549699029642897519, 12.93291415108713771, 51.74244959244378350 ) ) ;
#42280 = EDGE_CURVE ( 'NONE', #27128, #87574, #74548, .T. ) ;
#42281 = ORIENTED_EDGE ( 'NONE', *, *, #13425, .T. ) ;
#42283 = CARTESIAN_POINT ( 'NONE',  ( -6.145819459793597339, -5.000000000000000000, -7.996135855215887212 ) ) ;
#42282 = DIRECTION ( 'NONE',  ( 0.000000000000000000, 0.000000000000000000, 1.000000000000000000 ) ) ;
#42284 = DIRECTION ( 'NONE',  ( -1.000000000000000000, -1.224606353822377258E-16, -0.000000000000000000 ) ) ;
#42285 = CARTESIAN_POINT ( 'NONE',  ( -19.13075804668806512, 294.6725005060797571, -2.037659674250595909 ) ) ;
#42286 = SURFACE_STYLE_FILL_AREA ( #23487 ) ;
#42287 = CARTESIAN_POINT ( 'NONE',  ( 1.220765430959100062, 45.62969692430660018, 17.81327028958127912 ) ) ;
#42288 = CARTESIAN_POINT ( 'NONE',  ( 1.231544126066453693, 16.44631351882073034, -50.25343537072281208 ) ) ;
#42289 = VERTEX_POINT ( 'NONE', #33029 ) ;
#42290 = CARTESIAN_POINT ( 'NONE',  ( 87.44554515300957576, -60.00000000000001421, -22.19960419083119874 ) ) ;
#42291 = CARTESIAN_POINT ( 'NONE',  ( 32.20627048526277036, 464.6794164287632611, 10.68709986547568391 ) ) ;
#42292 =( NAMED_UNIT ( * ) PLANE_ANGLE_UNIT ( ) SI_UNIT ( $, .RADIAN. ) );
#42293 = EDGE_CURVE ( 'NONE', #104203, #92815, #34670, .T. ) ;
#42294 = CARTESIAN_POINT ( 'NONE',  ( 3.493042281569127550, 304.8518027749427119, -10.00000000028269298 ) ) ;
#42295 =( BOUNDED_SURFACE ( )  B_SPLINE_SURFACE ( 3, 2, ( 
 ( #41098, #42151, #57789 ),
 ( #89652, #99858, #73443 ),
 ( #50755, #24420, #56729 ),
 ( #83662, #50244, #16281 ),
 ( #62, #66426, #48635 ),
 ( #9773, #58338, #99310 ),
 ( #81519, #7644, #40560 ),
 ( #83146, #33033, #65899 ),
 ( #9243, #75034, #90716 ),
 ( #74512, #98782, #24938 ) ),
 .UNSPECIFIED., .F., .F., .F. ) 
 B_SPLINE_SURFACE_WITH_KNOTS ( ( 4, 2, 2, 2, 4 ),
 ( 3, 3 ),
 ( -1.185673698477996893E-05, 0.001057471059733232615, 0.002126798856451245050, 0.003196126653169257485, 0.004265454449887269919 ),
 ( 0.000000000000000000, 1.000000000000000000 ),
 .UNSPECIFIED. ) 
 GEOMETRIC_REPRESENTATION_ITEM ( )  RATIONAL_B_SPLINE_SURFACE ( (
 ( 1.000000000000000000, 1.000000000000000000, 1.000000000000000000),
 ( 1.000000000000000000, 0.9999925199711559021, 1.000000000000000000),
 ( 1.000000000000000000, 0.9961033022470029419, 1.000000000000000000),
 ( 1.000000000000000000, 0.9800616282253082900, 1.000000000000000000),
 ( 1.000000000000000000, 0.9678427155943769566, 1.000000000000000000),
 ( 1.000000000000000000, 0.9345111840696140870, 1.000000000000000000),
 ( 1.000000000000000000, 0.9135791977930803887, 1.000000000000000000),
 ( 1.000000000000000000, 0.8625981283151610279, 1.000000000000000000),
 ( 1.000000000000000000, 0.8325406200924377886, 1.000000000000000000),
 ( 1.000000000000000000, 0.7974033994357117017, 1.000000000000000000) ) ) 
 REPRESENTATION_ITEM ( '' )  SURFACE ( )  );
#42296 = CIRCLE ( 'NONE', #87059, 2.000000000000000000 ) ;
#42297 = LINE ( 'NONE', #76259, #97694 ) ;
#42298 = ORIENTED_EDGE ( 'NONE', *, *, #52278, .F. ) ;
#42299 = DIRECTION ( 'NONE',  ( 0.000000000000000000, -0.3420201433256733758, -0.9396926207859066515 ) ) ;
#42300 = ORIENTED_EDGE ( 'NONE', *, *, #67936, .F. ) ;
#42301 = ORIENTED_EDGE ( 'NONE', *, *, #5690, .F. ) ;
#42302 = CARTESIAN_POINT ( 'NONE',  ( 7.414346147791996522, 82.35410842337738302, -3.010818766110532785 ) ) ;
#42303 =( LENGTH_UNIT ( ) NAMED_UNIT ( * ) SI_UNIT ( .MILLI., .METRE. ) );
#42304 = DIRECTION ( 'NONE',  ( -1.000000000000000000, -0.000000000000000000, -0.000000000000000000 ) ) ;
#42305 = CARTESIAN_POINT ( 'NONE',  ( 0.000000000000000000, -1.200583151104953394, 120.1428571428571388 ) ) ;
#42306 = CARTESIAN_POINT ( 'NONE',  ( 83.23779423147905732, -37.82500537476536806, -5.216929617203576619 ) ) ;
#42307 = CARTESIAN_POINT ( 'NONE',  ( -41.98925252415875065, 316.9863883246551381, -4.665354603801200817 ) ) ;
#42308 = CARTESIAN_POINT ( 'NONE',  ( 10.28624191511809371, 43.99263840937192782, -12.90779740156171407 ) ) ;
#42309 = FILL_AREA_STYLE ('',( #67664 ) ) ;
#42310 = ORIENTED_EDGE ( 'NONE', *, *, #65307, .F. ) ;
#42311 = CARTESIAN_POINT ( 'NONE',  ( -6.815701034932152957, -1.328907527193361693, -6.169383458210041304 ) ) ;
#42312 = ORIENTED_EDGE ( 'NONE', *, *, #61343, .T. ) ;
#42313 = CARTESIAN_POINT ( 'NONE',  ( 9.554945014158674255, 51.29116508586518108, -3.541826056265481970 ) ) ;
#42314 = CARTESIAN_POINT ( 'NONE',  ( 40.46237499442743513, 464.0765077733557860, 18.40249546253095758 ) ) ;
#42316 = VERTEX_POINT ( 'NONE', #91258 ) ;
#42315 = DIRECTION ( 'NONE',  ( 0.000000000000000000, -1.000000000000000000, 0.000000000000000000 ) ) ;
#42317 = CARTESIAN_POINT ( 'NONE',  ( 73.71512049594772975, -32.54216154817675033, 110.4876667498937479 ) ) ;
#42318 = VECTOR ( 'NONE', #101657, 1000.000000000000000 ) ;
#42319 = VERTEX_POINT ( 'NONE', #7640 ) ;
#42320 = CARTESIAN_POINT ( 'NONE',  ( 2.977408999572652260, -25.43750000204838457, 7.188101187500000044 ) ) ;
#42321 =( BOUNDED_SURFACE ( )  B_SPLINE_SURFACE ( 3, 2, ( 
 ( #73505, #89717, #40098 ),
 ( #7183, #83203, #72973 ),
 ( #23406, #64904, #57850 ),
 ( #23952, #48697, #81584 ),
 ( #49228, #65960, #7709 ),
 ( #98840, #74573, #90239 ),
 ( #33615, #99368, #106404 ),
 ( #25547, #58406, #16343 ),
 ( #32563, #9300, #57321 ),
 ( #98329, #65435, #90779 ),
 ( #24485, #49774, #72457 ),
 ( #105365, #82133, #64386 ),
 ( #8248, #56249, #125 ),
 ( #82675, #2811, #91836 ),
 ( #34160, #58945, #77247 ),
 ( #11424, #59483, #26610 ),
 ( #60028, #100982, #27678 ),
 ( #35219, #9835, #3362 ) ),
 .UNSPECIFIED., .F., .F., .F. ) 
 B_SPLINE_SURFACE_WITH_KNOTS ( ( 4, 2, 2, 2, 2, 2, 2, 2, 4 ),
 ( 3, 3 ),
 ( -2.862293735361731706E-17, 0.001555391903720538442, 0.003110783807441105508, 0.004666175711161672790, 0.006221567614882239639, 0.007776959518602806487, 0.009332351422323373336, 0.01088774332604394018, 0.01244313522976450877 ),
 ( 0.000000000000000000, 1.000000000000000000 ),
 .UNSPECIFIED. ) 
 GEOMETRIC_REPRESENTATION_ITEM ( )  RATIONAL_B_SPLINE_SURFACE ( (
 ( 1.000000000000000000, 0.9028401456532985092, 1.000000000000000000),
 ( 1.000000000000000000, 0.9067516630662485477, 1.000000000000000000),
 ( 1.000000000000000000, 0.9091058375364423627, 1.000000000000000000),
 ( 1.000000000000000000, 0.9105595566477392433, 1.000000000000000000),
 ( 1.000000000000000000, 0.9096051370505221501, 1.000000000000000000),
 ( 1.000000000000000000, 0.9045241161555340748, 1.000000000000000000),
 ( 1.000000000000000000, 0.9004407328802259691, 1.000000000000000000),
 ( 1.000000000000000000, 0.8894899492097501081, 1.000000000000000000),
 ( 1.000000000000000000, 0.8827450154233547064, 1.000000000000000000),
 ( 1.000000000000000000, 0.8674022177617248808, 1.000000000000000000),
 ( 1.000000000000000000, 0.8587750089643293450, 1.000000000000000000),
 ( 1.000000000000000000, 0.8400002396215728862, 1.000000000000000000),
 ( 1.000000000000000000, 0.8300505958792420147, 1.000000000000000000),
 ( 1.000000000000000000, 0.8096117823345528874, 1.000000000000000000),
 ( 1.000000000000000000, 0.7991063331010617166, 1.000000000000000000),
 ( 1.000000000000000000, 0.7781243022290107447, 1.000000000000000000),
 ( 1.000000000000000000, 0.7679211400719462288, 1.000000000000000000),
 ( 1.000000000000000000, 0.7583909709667225885, 1.000000000000000000) ) ) 
 REPRESENTATION_ITEM ( '' )  SURFACE ( )  );
#42322 = CARTESIAN_POINT ( 'NONE',  ( -87.28812347660355897, -57.67005709194983609, -25.16891244813248818 ) ) ;
#42323 = PRESENTATION_LAYER_ASSIGNMENT (  '', '', ( #87083 ) ) ;
#42324 = ORIENTED_EDGE ( 'NONE', *, *, #31191, .F. ) ;
#42325 = SHAPE_REPRESENTATION_RELATIONSHIP ( 'NONE' , 'NONE' ,  #55690, #39669 ) ;
#42326 = CARTESIAN_POINT ( 'NONE',  ( 0.000000000000000000, 0.000000000000000000, 4.000000000000000000 ) ) ;
#42327 = STYLED_ITEM ( 'NONE', ( #72130 ), #11749 ) ;
#42328 = CARTESIAN_POINT ( 'NONE',  ( 104.9727926896761545, -52.71702872129058903, 163.4617720493101274 ) ) ;
#42329 = CARTESIAN_POINT ( 'NONE',  ( 27.33349330513380693, 4.000000000000002665, 0.000000000000000000 ) ) ;
#42330 = EDGE_CURVE ( 'NONE', #39221, #43420, #56421, .T. ) ;
#42331 = DIRECTION ( 'NONE',  ( -0.5735764363510494901, -0.8191520442889894671, 0.000000000000000000 ) ) ;
#42332 = AXIS2_PLACEMENT_3D ( 'NONE', #39120, #64965, #63928 ) ;
#42333 = CARTESIAN_POINT ( 'NONE',  ( 4.898587196589412829E-16, -22.81250000409677270, -8.000000000000000000 ) ) ;
#42334 = STYLED_ITEM ( 'NONE', ( #9522 ), #23472 ) ;
#42335 = CARTESIAN_POINT ( 'NONE',  ( 106.4000000000000057, 0.000000000000000000, 0.000000000000000000 ) ) ;
#42336 = AXIS2_PLACEMENT_3D ( 'NONE', #55379, #47291, #31157 ) ;
#42337 = CARTESIAN_POINT ( 'NONE',  ( -36.31864149993810287, 26.04191782070092032, 12.31453629475708667 ) ) ;
#42338 = AXIS2_PLACEMENT_3D ( 'NONE', #32463, #57747, #90139 ) ;
#42339 = CARTESIAN_POINT ( 'NONE',  ( 31.90195216159137814, 465.6468698803305983, 10.69263942007829549 ) ) ;
#42340 = CARTESIAN_POINT ( 'NONE',  ( -7.981862520314372489, 9.786068389958022714E-16, -0.01269999999999830292 ) ) ;
#42341 = CARTESIAN_POINT ( 'NONE',  ( -19.70764564238367100, 304.7954121406193053, 9.925013215726757210 ) ) ;
#42342 = CARTESIAN_POINT ( 'NONE',  ( 26.88291765283142354, 410.1183258646225909, 267.1969486013078949 ) ) ;
#42343 = CARTESIAN_POINT ( 'NONE',  ( 0.000000000000000000, 15.00000000000000000, -9.999999999999998224 ) ) ;
#42344 = ORIENTED_EDGE ( 'NONE', *, *, #3236, .F. ) ;
#42345 = DIRECTION ( 'NONE',  ( 0.000000000000000000, -1.000000000000000000, 0.000000000000000000 ) ) ;
#42346 = CONICAL_SURFACE ( 'NONE', #66451, 4.000000000000007105, 0.9599310885968835860 ) ;
#42347 = CARTESIAN_POINT ( 'NONE',  ( -5.000000000000000000, -15.93202192939577344, -5.930487099830192399 ) ) ;
#42348 = CARTESIAN_POINT ( 'NONE',  ( -84.86054889550955238, -30.00000000000000000, 169.0023419988235105 ) ) ;
#42349 = EDGE_CURVE ( 'NONE', #25389, #37427, #106334, .T. ) ;
#42350 = VERTEX_POINT ( 'NONE', #75580 ) ;
#42351 = ORIENTED_EDGE ( 'NONE', *, *, #22249, .F. ) ;
#42352 = CARTESIAN_POINT ( 'NONE',  ( 4.769810751601300858, -47.36241918932975636, 42.84708261346381164 ) ) ;
#42353 = CARTESIAN_POINT ( 'NONE',  ( 72.27211704050357355, -57.67031449669786269, 174.7872370686350223 ) ) ;
#42355 = CARTESIAN_POINT ( 'NONE',  ( -9.636065190160278959, 53.53714903547604820, 2.125145488933209759 ) ) ;
#42354 = CARTESIAN_POINT ( 'NONE',  ( -14.90280835358831268, 2.161282233151506915, -1.653369514881387836 ) ) ;
#42356 = CARTESIAN_POINT ( 'NONE',  ( -38.51502786940007184, 460.0233756673457606, 2.043034587342192676 ) ) ;
#42357 = CARTESIAN_POINT ( 'NONE',  ( -1.011673908906385311, 43.34673389873664462, 18.25206967576084693 ) ) ;
#42358 = CARTESIAN_POINT ( 'NONE',  ( -43.40156817618215968, 435.0518544017560316, 15.31415127474093651 ) ) ;
#42359 = CARTESIAN_POINT ( 'NONE',  ( -38.95621058113182045, -60.00000000000000711, 50.68831809153677170 ) ) ;
#42360 = FACE_OUTER_BOUND ( 'NONE', #42008, .T. ) ;
#42361 = EDGE_CURVE ( 'NONE', #5164, #70645, #58886, .T. ) ;
#42362 = DIRECTION ( 'NONE',  ( 0.000000000000000000, 0.000000000000000000, -1.000000000000000000 ) ) ;
#42363 = CARTESIAN_POINT ( 'NONE',  ( -85.67725297654990868, -46.54890279682108911, 188.9755717729104845 ) ) ;
#42364 = ORIENTED_EDGE ( 'NONE', *, *, #80737, .T. ) ;
#42365 = CARTESIAN_POINT ( 'NONE',  ( 6.849999999999999645, -9.237604307034018802, 3.355146209984123968E-17 ) ) ;
#42366 = CARTESIAN_POINT ( 'NONE',  ( -8.026063634138786540, -22.06789999752070486, 27.56027737331870497 ) ) ;
#42367 = AXIS2_PLACEMENT_3D ( 'NONE', #72509, #56301, #89769 ) ;
#42368 = CARTESIAN_POINT ( 'NONE',  ( 0.000000000000000000, 0.000000000000000000, 0.000000000000000000 ) ) ;
#42369 = FILL_AREA_STYLE ('',( #50445 ) ) ;
#42371 = CARTESIAN_POINT ( 'NONE',  ( 2.267203695418912091, -69.44328133798735792, 12.91314673039722294 ) ) ;
#42370 = CARTESIAN_POINT ( 'NONE',  ( -35.25991156925849879, 303.5722148236554858, 3.944335390694383214 ) ) ;
#42372 = ORIENTED_EDGE ( 'NONE', *, *, #15723, .T. ) ;
#42373 = CARTESIAN_POINT ( 'NONE',  ( -9.109994089937119455, -4.999999999999461764, -17.31936419814998374 ) ) ;
#42374 = CARTESIAN_POINT ( 'NONE',  ( -30.06815944328915435, 12.45816842452743067, -39.66421731453383615 ) ) ;
#42375 = CARTESIAN_POINT ( 'NONE',  ( 33.66264974566500712, 300.0834067526730564, -8.832479651548673871 ) ) ;
#42376 = DIRECTION ( 'NONE',  ( -1.000000000000000000, -1.224606353822377258E-16, -0.000000000000000000 ) ) ;
#42377 =( NAMED_UNIT ( * ) SI_UNIT ( $, .STERADIAN. ) SOLID_ANGLE_UNIT ( ) );
#42378 = FILL_AREA_STYLE ('',( #38288 ) ) ;
#42379 = CARTESIAN_POINT ( 'NONE',  ( 108.8241408383580193, -29.99999999999998224, 157.0475695436092565 ) ) ;
#42380 = CARTESIAN_POINT ( 'NONE',  ( -80.88873720124335875, -49.92061108326104346, 166.5754553910332447 ) ) ;
#42381 = ORIENTED_EDGE ( 'NONE', *, *, #40350, .F. ) ;
#42382 = DIRECTION ( 'NONE',  ( 0.000000000000000000, -1.000000000000000000, 0.000000000000000000 ) ) ;
#42383 = CARTESIAN_POINT ( 'NONE',  ( -9.381394091586582107, 252.0134960558159776, 3.465950112474283085 ) ) ;
#42384 = DIRECTION ( 'NONE',  ( 0.000000000000000000, 0.000000000000000000, 1.000000000000000000 ) ) ;
#42385 = CARTESIAN_POINT ( 'NONE',  ( 6.326416241096634252, -1.324101276589546794, -6.831531844319976621 ) ) ;
#42386 = CARTESIAN_POINT ( 'NONE',  ( 2.869469963220364406, 87.32917479646899039, -4.999999999999998224 ) ) ;
#42387 = CARTESIAN_POINT ( 'NONE',  ( -27.99999999999999645, 0.000000000000000000, 0.000000000000000000 ) ) ;
#42388 = VERTEX_POINT ( 'NONE', #50751 ) ;
#42389 = STYLED_ITEM ( 'NONE', ( #2684 ), #65440 ) ;
#42390 = CARTESIAN_POINT ( 'NONE',  ( -22.47298735892809418, 305.4392088308884468, 10.06407263457672663 ) ) ;
#42391 = ORIENTED_EDGE ( 'NONE', *, *, #82481, .T. ) ;
#42392 = CARTESIAN_POINT ( 'NONE',  ( 37.53110860859745657, 485.4504903723462235, -3.702833747837409373 ) ) ;
#42393 = CARTESIAN_POINT ( 'NONE',  ( 6.249999999999998224, -9.237604307034018802, 0.000000000000000000 ) ) ;
#42394 = CARTESIAN_POINT ( 'NONE',  ( 32.80551872593247253, 486.0171861992463391, 5.671217483526194592 ) ) ;
#42395 = COLOUR_RGB ( '', 0.40784314, 0.44705882, 0.49803922) ;
#42396 = CARTESIAN_POINT ( 'NONE',  ( 60.66923414622826982, 50.00000000000000000, 17.93278245653309710 ) ) ;
#42397 = CARTESIAN_POINT ( 'NONE',  ( 5.000000000000000000, -13.96166769376080374, 11.51022196660214370 ) ) ;
#42398 = CARTESIAN_POINT ( 'NONE',  ( 44.13152524673034094, 435.3762053705510766, 10.68396593870416567 ) ) ;
#42399 = ORIENTED_EDGE ( 'NONE', *, *, #258, .T. ) ;
#42400 = CARTESIAN_POINT ( 'NONE',  ( 112.2509120385887655, -59.99999999999998579, 171.9075463260369361 ) ) ;
#42401 = CONICAL_SURFACE ( 'NONE', #54466, 8.000000000000000000, 0.9599310885968911355 ) ;
#42403 = CARTESIAN_POINT ( 'NONE',  ( 25.36379536694408543, -53.39101624669748958, 34.18967480269854065 ) ) ;
#42402 = CARTESIAN_POINT ( 'NONE',  ( -76.85442806461188070, -14.21045842199432663, 149.6320961301125578 ) ) ;
#42405 = CARTESIAN_POINT ( 'NONE',  ( 83.30842096339651448, -37.99999999999997868, -6.385845932050894902 ) ) ;
#42404 = UNCERTAINTY_MEASURE_WITH_UNIT (LENGTH_MEASURE( 1.000000000000000082E-05 ), #38267, 'distance_accuracy_value', 'NONE');
#42406 = CARTESIAN_POINT ( 'NONE',  ( 4.699999999999999289, 3.752776749732553263, -6.499999999999999112 ) ) ;
#42407 = CARTESIAN_POINT ( 'NONE',  ( -41.32835128475512221, -42.98145676455503406, 40.63877246576411295 ) ) ;
#42408 = LINE ( 'NONE', #83934, #60843 ) ;
#42409 = CONICAL_SURFACE ( 'NONE', #7984, 5.000000000000010658, 0.9599310885968697082 ) ;
#42410 = ORIENTED_EDGE ( 'NONE', *, *, #42462, .T. ) ;
#42411 = MECHANICAL_DESIGN_GEOMETRIC_PRESENTATION_REPRESENTATION (  '', ( #42334 ), #101001 ) ;
#42412 = CYLINDRICAL_SURFACE ( 'NONE', #102950, 5.000000000000001776 ) ;
#42413 = CIRCLE ( 'NONE', #21738, 8.000000000000000000 ) ;
#42414 = CARTESIAN_POINT ( 'NONE',  ( 7.350509712866862166, 54.21962849041422317, 3.138265851615306801 ) ) ;
#42415 = CARTESIAN_POINT ( 'NONE',  ( 22.91885868373643831, 305.6172567281201964, 10.10309701371861912 ) ) ;
#42416 = CARTESIAN_POINT ( 'NONE',  ( 69.18888888888888289, 3.309500000000014541, 4.052968581778174646E-16 ) ) ;
#42417 = CARTESIAN_POINT ( 'NONE',  ( 35.11650669486618170, 1.474610560812782335E-15, 0.000000000000000000 ) ) ;
#42418 = CARTESIAN_POINT ( 'NONE',  ( -32.11957450231075484, 486.1307089099603331, 5.366351229208995655 ) ) ;
#42419 = ORIENTED_EDGE ( 'NONE', *, *, #56454, .T. ) ;
#42420 = CARTESIAN_POINT ( 'NONE',  ( -16.34886101041462680, 36.48569306717566008, -24.24298062968071932 ) ) ;
#42421 = ORIENTED_EDGE ( 'NONE', *, *, #35152, .T. ) ;
#42422 = CARTESIAN_POINT ( 'NONE',  ( 80.93574383532660477, -30.00000000000004619, -12.06234416543689392 ) ) ;
#42423 = DIRECTION ( 'NONE',  ( 0.000000000000000000, 0.000000000000000000, -1.000000000000000000 ) ) ;
#42424 = VECTOR ( 'NONE', #95600, 1000.000000000000000 ) ;
#42425 = DIRECTION ( 'NONE',  ( -1.000000000000000000, -1.224606353822377258E-16, -0.000000000000000000 ) ) ;
#42426 = ADVANCED_FACE ( 'NONE', ( #59418 ), #83656, .F. ) ;
#42427 = CARTESIAN_POINT ( 'NONE',  ( 80.95826188147296421, -29.99999999999999645, 4.765542408442753342 ) ) ;
#42428 = EDGE_CURVE ( 'NONE', #66517, #35102, #78237, .T. ) ;
#42429 =( NAMED_UNIT ( * ) PLANE_ANGLE_UNIT ( ) SI_UNIT ( $, .RADIAN. ) );
#42430 = EDGE_LOOP ( 'NONE', ( #23131, #34007, #32099, #43318 ) ) ;
#42431 = VERTEX_POINT ( 'NONE', #101459 ) ;
#42432 = ORIENTED_EDGE ( 'NONE', *, *, #29989, .F. ) ;
#42433 = CARTESIAN_POINT ( 'NONE',  ( -47.03691741412927030, 13.53106325772394669, -14.84138715777564066 ) ) ;
#42434 = SURFACE_STYLE_USAGE ( .BOTH. , #68864 ) ;
#42435 = FACE_OUTER_BOUND ( 'NONE', #51701, .T. ) ;
#42436 = AXIS2_PLACEMENT_3D ( 'NONE', #64213, #22706, #87949 ) ;
#42437 = CARTESIAN_POINT ( 'NONE',  ( 5.477578620271508214, -13.16501439016104236, -2.459398706554656755 ) ) ;
#42438 = CARTESIAN_POINT ( 'NONE',  ( 6.169949891409288512, 4.949864754178546100, -4.426582755169667927 ) ) ;
#42439 = DIRECTION ( 'NONE',  ( 0.000000000000000000, -1.000000000000000000, 0.000000000000000000 ) ) ;
#42440 = ORIENTED_EDGE ( 'NONE', *, *, #89056, .F. ) ;
#42441 = CARTESIAN_POINT ( 'NONE',  ( -9.999999999999989342, 49.99999999999999289, -83.69100306251235111 ) ) ;
#42442 = ORIENTED_EDGE ( 'NONE', *, *, #25686, .F. ) ;
#42443 = CARTESIAN_POINT ( 'NONE',  ( 11.08349330513380160, 4.898587196589405926E-16, -4.000000000000001776 ) ) ;
#42444 = CARTESIAN_POINT ( 'NONE',  ( 64.38843716681957119, -38.33834301559899416, 111.1500240642540263 ) ) ;
#42445 = CARTESIAN_POINT ( 'NONE',  ( 1.224646799147354440E-15, 300.0000000000000568, 10.00000000000000178 ) ) ;
#42446 = CARTESIAN_POINT ( 'NONE',  ( 33.40626526979832533, 300.9755454843282223, 3.321175472843470367 ) ) ;
#42447 = VECTOR ( 'NONE', #20934, 1000.000000000000000 ) ;
#42448 = CARTESIAN_POINT ( 'NONE',  ( -5.382057749264597568, 247.0017320159604992, -2.659775980967104658 ) ) ;
#42449 = VERTEX_POINT ( 'NONE', #37287 ) ;
#42450 = AXIS2_PLACEMENT_3D ( 'NONE', #14655, #105285, #88051 ) ;
#42451 = CARTESIAN_POINT ( 'NONE',  ( 6.750000000000016875, -11.69134295108991495, -13.00000000000000000 ) ) ;
#42452 = DIRECTION ( 'NONE',  ( 0.000000000000000000, 0.000000000000000000, 1.000000000000000000 ) ) ;
#42453 = FACE_OUTER_BOUND ( 'NONE', #26672, .T. ) ;
#42454 = CARTESIAN_POINT ( 'NONE',  ( 15.45234973294653003, 2.833591715789641974, -2.076776216656130991 ) ) ;
#42455 = ORIENTED_EDGE ( 'NONE', *, *, #97354, .T. ) ;
#42456 = CARTESIAN_POINT ( 'NONE',  ( -26.05698008878660588, 296.0953443834534369, 10.20571257035117618 ) ) ;
#42457 = CARTESIAN_POINT ( 'NONE',  ( 7.357155954586323432, 54.21801673151467327, -3.132771341046588720 ) ) ;
#42458 = CARTESIAN_POINT ( 'NONE',  ( 43.00000000000000000, 436.5989882784185738, 19.94133085611158407 ) ) ;
#42459 = CARTESIAN_POINT ( 'NONE',  ( -3.080866544137897289, -6.881514909249071721, -7.026396753507436976 ) ) ;
#42460 = CARTESIAN_POINT ( 'NONE',  ( 32.94330508143927716, 1.340359594676612611E-15, 0.000000000000000000 ) ) ;
#42461 = CARTESIAN_POINT ( 'NONE',  ( -7.151597709147946347, 103.2107073494778575, 3.587174531012139678 ) ) ;
#42462 = EDGE_CURVE ( 'NONE', #56403, #33365, #92500, .T. ) ;
#42463 = CARTESIAN_POINT ( 'NONE',  ( 58.67238219402268840, 6.975173280561618775E-15, 0.000000000000000000 ) ) ;
#42464 = CARTESIAN_POINT ( 'NONE',  ( 85.95818388483708361, -31.98290817333131031, 183.5996520270772976 ) ) ;
#42465 = FILL_AREA_STYLE_COLOUR ( '', #65275 ) ;
#42466 = VERTEX_POINT ( 'NONE', #93901 ) ;
#42467 = CARTESIAN_POINT ( 'NONE',  ( 94.58506785723692190, -57.65556415943643032, -10.24388704223456692 ) ) ;
#42468 = PLANE ( 'NONE',  #17725 ) ;
#42469 = CARTESIAN_POINT ( 'NONE',  ( -2.690931834596291594, 5.951943280390036506, 1.837214462594576647E-15 ) ) ;
#42470 = CARTESIAN_POINT ( 'NONE',  ( 0.000000000000000000, 5.629165124598848102, 3.250000000000005329 ) ) ;
#42471 = CARTESIAN_POINT ( 'NONE',  ( -81.59120001829518287, -29.99999999999999645, -7.233253355891588576 ) ) ;
#42472 = EDGE_CURVE ( 'NONE', #61957, #85320, #4869, .T. ) ;
#42473 = CIRCLE ( 'NONE', #74946, 6.000000000000001776 ) ;
#42474 = CIRCLE ( 'NONE', #99274, 4.172000000000009479 ) ;
#42475 = CARTESIAN_POINT ( 'NONE',  ( 27.02022815836235026, 1.340359594676612611E-15, 0.000000000000000000 ) ) ;
#42476 = MECHANICAL_DESIGN_GEOMETRIC_PRESENTATION_REPRESENTATION (  '', ( #27215 ), #70056 ) ;
#42477 = CARTESIAN_POINT ( 'NONE',  ( 8.572527594031486009E-16, 0.000000000000000000, 7.000000000000011546 ) ) ;
#42478 = CARTESIAN_POINT ( 'NONE',  ( -7.779103221381271638, 4.168986698926019585, -7.929128246061903695 ) ) ;
#42480 = DIRECTION ( 'NONE',  ( 1.000000000000000000, 0.000000000000000000, 0.000000000000000000 ) ) ;
#42479 = CARTESIAN_POINT ( 'NONE',  ( 35.55347100935683358, 490.6492510279384760, 12.31610217058555534 ) ) ;
#42481 = CARTESIAN_POINT ( 'NONE',  ( -17.49999999999997513, 50.00000000000000000, 63.82142195434425958 ) ) ;
#42482 = CARTESIAN_POINT ( 'NONE',  ( 0.000000000000000000, 0.000000000000000000, -0.02540000000000007530 ) ) ;
#42483 = CARTESIAN_POINT ( 'NONE',  ( -13.50000000000000000, -7.794228634059985339, -1.205771365940065953 ) ) ;
#42484 = CARTESIAN_POINT ( 'NONE',  ( 0.000000000000000000, -3.035766082959412415E-15, 0.000000000000000000 ) ) ;
#42485 = CARTESIAN_POINT ( 'NONE',  ( -71.17284327374473207, -38.00000000000000711, -21.88481141223168436 ) ) ;
#42486 = DIRECTION ( 'NONE',  ( -1.000000000000000000, 0.000000000000000000, 0.000000000000000000 ) ) ;
#42487 = PRESENTATION_LAYER_ASSIGNMENT (  '', '', ( #2912 ) ) ;
#42488 = CARTESIAN_POINT ( 'NONE',  ( 47.65524110203897123, -26.94530822553867822, -28.56564397192451565 ) ) ;
#42489 = EDGE_CURVE ( 'NONE', #94793, #59320, #101238, .T. ) ;
#42490 = CARTESIAN_POINT ( 'NONE',  ( -22.80451126749514401, -49.91919812353112462, 33.12644376951882208 ) ) ;
#42491 = VERTEX_POINT ( 'NONE', #85827 ) ;
#42492 = CARTESIAN_POINT ( 'NONE',  ( 6.321595794353348730, 10.35635176133114577, 3.012682989575210524 ) ) ;
#42493 =( NAMED_UNIT ( * ) SI_UNIT ( $, .STERADIAN. ) SOLID_ANGLE_UNIT ( ) );
#42494 = AXIS2_PLACEMENT_3D ( 'NONE', #4571, #39073, #86576 ) ;
#42495 = CARTESIAN_POINT ( 'NONE',  ( -7.344361273354514275, 82.55439469411476239, -3.175733139645586345 ) ) ;
#42496 = CARTESIAN_POINT ( 'NONE',  ( -63.77693750556839802, -29.65005726330078062, -23.56308934115906339 ) ) ;
#42497 = ADVANCED_FACE ( 'NONE', ( #92280 ), #73762, .T. ) ;
#42499 = CARTESIAN_POINT ( 'NONE',  ( 34.10284876471455817, 3.851859888774471706E-31, 5.000000000000001776 ) ) ;
#42498 = FACE_OUTER_BOUND ( 'NONE', #99043, .T. ) ;
#42500 = ORIENTED_EDGE ( 'NONE', *, *, #70472, .F. ) ;
#42501 = FACE_OUTER_BOUND ( 'NONE', #36072, .T. ) ;
#42502 = ORIENTED_EDGE ( 'NONE', *, *, #104401, .T. ) ;
#42503 = DIRECTION ( 'NONE',  ( -1.000000000000000000, -0.000000000000000000, -0.000000000000000000 ) ) ;
#42504 = EDGE_CURVE ( 'NONE', #83087, #65902, #101496, .T. ) ;
#42505 = CARTESIAN_POINT ( 'NONE',  ( -81.52927428744742144, -59.99999999999999289, -27.00541479453063332 ) ) ;
#42507 = EDGE_CURVE ( 'NONE', #23008, #4416, #106476, .T. ) ;
#42506 = EDGE_LOOP ( 'NONE', ( #31836, #20981, #96275, #101572, #91171 ) ) ;
#42508 = CARTESIAN_POINT ( 'NONE',  ( 11.08349330513380515, 4.000000000000002665, 0.000000000000000000 ) ) ;
#42509 = CARTESIAN_POINT ( 'NONE',  ( 101.5045788610895130, -52.73011406855718519, 192.7905639140061567 ) ) ;
#42511 = CARTESIAN_POINT ( 'NONE',  ( -7.986468734911285949, -6.026863202769209060, 0.5341897780976081478 ) ) ;
#42510 = LINE ( 'NONE', #67857, #100924 ) ;
#42512 = AXIS2_PLACEMENT_3D ( 'NONE', #176, #67084, #40668 ) ;
#42513 = VERTEX_POINT ( 'NONE', #12954 ) ;
#42514 = ADVANCED_FACE ( 'NONE', ( #55525 ), #70684, .T. ) ;
#42515 = EDGE_LOOP ( 'NONE', ( #102699, #96935, #9082, #83028, #95602 ) ) ;
#42516 = ORIENTED_EDGE ( 'NONE', *, *, #13823, .T. ) ;
#42517 = CARTESIAN_POINT ( 'NONE',  ( 29.19175403363693988, 323.8406402827946522, 14.62108096419524728 ) ) ;
#42518 = CARTESIAN_POINT ( 'NONE',  ( 36.84999999999999432, 1.533819458162526451E-15, 0.000000000000000000 ) ) ;
#42519 = DIRECTION ( 'NONE',  ( -1.000000000000000000, -1.224606353822377258E-16, -0.000000000000000000 ) ) ;
#42520 = ORIENTED_EDGE ( 'NONE', *, *, #64129, .F. ) ;
#42521 = DIRECTION ( 'NONE',  ( -1.000000000000000000, -1.224606353822377258E-16, -0.000000000000000000 ) ) ;
#42522 = FILL_AREA_STYLE_COLOUR ( '', #7681 ) ;
#42523 = DIRECTION ( 'NONE',  ( -3.673940397442057649E-17, 0.000000000000000000, -1.000000000000000000 ) ) ;
#42524 = CARTESIAN_POINT ( 'NONE',  ( -43.09316981551443604, -57.68566503113564892, 61.19926976090692960 ) ) ;
#42525 = DIRECTION ( 'NONE',  ( -0.5735764363510494901, -0.8191520442889894671, 0.000000000000000000 ) ) ;
#42526 = CARTESIAN_POINT ( 'NONE',  ( -19.70764564238371719, 304.7954121406193622, 9.925013215726785631 ) ) ;
#42527 = DIRECTION ( 'NONE',  ( 0.000000000000000000, -1.000000000000000000, 0.000000000000000000 ) ) ;
#42528 = CARTESIAN_POINT ( 'NONE',  ( -89.80806051762600362, -30.00000000000005684, 26.19611557095339904 ) ) ;
#42529 = CARTESIAN_POINT ( 'NONE',  ( 0.000000000000000000, 0.000000000000000000, 0.000000000000000000 ) ) ;
#42530 = CARTESIAN_POINT ( 'NONE',  ( -49.74770505191611392, -32.59159611762328268, 48.06925685492829814 ) ) ;
#42531 = CARTESIAN_POINT ( 'NONE',  ( -0.1342739691912682998, 21.85270131633359725, 7.000000000000020428 ) ) ;
#42532 = VERTEX_POINT ( 'NONE', #21114 ) ;
#42533 = CARTESIAN_POINT ( 'NONE',  ( 15.11650669486618881, -3.851859888774471706E-31, 4.000000000000000888 ) ) ;
#42534 = COLOUR_RGB ( '', 0.09019608, 0.27058824, 0.51372549) ;
#42535 = CARTESIAN_POINT ( 'NONE',  ( 20.59999999999999787, 3.309500000000003439, 4.052968581778167743E-16 ) ) ;
#42536 = CARTESIAN_POINT ( 'NONE',  ( 12.38975795024176918, -3.228398025805478078, 20.63738045662677223 ) ) ;
#42537 = ORIENTED_EDGE ( 'NONE', *, *, #86640, .T. ) ;
#42538 = FILL_AREA_STYLE_COLOUR ( '', #102830 ) ;
#42539 = CARTESIAN_POINT ( 'NONE',  ( 104.4676181534481856, -38.40404783520960308, 197.9968809589744296 ) ) ;
#42540 = CARTESIAN_POINT ( 'NONE',  ( 1.688352148327314640E-15, 8.895721644649736248, -7.917989418073286600 ) ) ;
#42541 = DIRECTION ( 'NONE',  ( 0.5735764363510470476, -0.8191520442889911324, 1.003171929053524007E-16 ) ) ;
#42542 = CARTESIAN_POINT ( 'NONE',  ( -16.16328599919005526, 302.5659913735702844, 9.876334255033473397 ) ) ;
#42543 = CARTESIAN_POINT ( 'NONE',  ( -42.19179521602266902, 485.4956273777415277, -3.824025998169080953 ) ) ;
#42544 = CARTESIAN_POINT ( 'NONE',  ( 87.04597188044493805, -29.99999999999999645, 183.8866158033205522 ) ) ;
#42545 = CARTESIAN_POINT ( 'NONE',  ( 23.21751746555220564, 25.98869614573808917, -30.70617127781077116 ) ) ;
#42546 = CARTESIAN_POINT ( 'NONE',  ( -28.71516359314619393, 10.50242333429326713, 41.65501769021843614 ) ) ;
#42547 = EDGE_CURVE ( 'NONE', #48471, #1725, #42745, .T. ) ;
#42548 = ORIENTED_EDGE ( 'NONE', *, *, #6613, .F. ) ;
#42549 = ORIENTED_EDGE ( 'NONE', *, *, #106052, .T. ) ;
#42550 = CARTESIAN_POINT ( 'NONE',  ( 52.96824733631504500, -22.17278515511078041, 49.74370119324648698 ) ) ;
#42551 = CIRCLE ( 'NONE', #106279, 7.000000000000000000 ) ;
#42552 = CARTESIAN_POINT ( 'NONE',  ( 6.955654034292342303, 41.30888721648646822, -58.54628189783632308 ) ) ;
#42553 = EDGE_CURVE ( 'NONE', #87110, #55862, #20487, .T. ) ;
#42554 = CARTESIAN_POINT ( 'NONE',  ( -5.500000000000007994, 42.00000000000000000, -71.41947339646975479 ) ) ;
#42555 = EDGE_LOOP ( 'NONE', ( #93647, #58741, #31937, #44025 ) ) ;
#42556 = CARTESIAN_POINT ( 'NONE',  ( -107.6814678764850015, -38.35635315369628984, 135.5461783006386725 ) ) ;
#42557 = ORIENTED_EDGE ( 'NONE', *, *, #85211, .F. ) ;
#42558 = CARTESIAN_POINT ( 'NONE',  ( 15.72218280906592369, 5.595371698624338919, 6.516822309427269033 ) ) ;
#42559 = CARTESIAN_POINT ( 'NONE',  ( 108.2524867605244339, -38.35773384716500090, 192.2673139560903053 ) ) ;
#42560 = CARTESIAN_POINT ( 'NONE',  ( 13.59240052242509655, 24.77055383530022681, -0.6222571633745787034 ) ) ;
#42562 = CARTESIAN_POINT ( 'NONE',  ( 91.82244223932920590, -60.15085423987636659, 66.55118452451621636 ) ) ;
#42561 = AXIS2_PLACEMENT_3D ( 'NONE', #30815, #22722, #72296 ) ;
#42563 = AXIS2_PLACEMENT_3D ( 'NONE', #83477, #9576, #1481 ) ;
#42564 = CIRCLE ( 'NONE', #2992, 5.000000000000002665 ) ;
#42565 = CARTESIAN_POINT ( 'NONE',  ( 27.99999999999999645, 1.102182119232617714E-15, -9.000000000000000000 ) ) ;
#42567 = AXIS2_PLACEMENT_3D ( 'NONE', #41465, #16125, #88441 ) ;
#42566 = CARTESIAN_POINT ( 'NONE',  ( -20.21880305278368439, 304.8280059657581660, -9.005058168222323189 ) ) ;
#42568 = CARTESIAN_POINT ( 'NONE',  ( 0.000000000000000000, 0.000000000000000000, 4.000000000000000888 ) ) ;
#42569 = B_SPLINE_CURVE_WITH_KNOTS ( 'NONE', 3,
 ( #72286, #38360, #71224, #30262, #105191, #31337, #1565, #58776, #8608, #25367, #91672, #477, #49599, #42043, #57152, #7533, #16711, #73330, #1008, #33993, #90065, #82507, #91152, #58224, #24305, #83039, #50131, #34527, #16171, #9658, #40450, #65261, #98150, #106229, #9131, #42571, #98670 ),
 .UNSPECIFIED., .F., .F.,
 ( 4, 1, 1, 1, 1, 1, 2, 2, 1, 1, 1, 2, 2, 2, 1, 1, 1, 2, 2, 1, 1, 1, 1, 2, 2, 4 ),
 ( 0.000000000000000000, 0.1250000000000957567, 0.1875000000001431355, 0.2187500000001631750, 0.2343750000001732225, 0.2421875000001741385, 0.2460937500001765532, 0.2500000000001789680, 0.3125000000001895706, 0.3437500000002005063, 0.3593750000002058909, 0.3671875000002068345, 0.3750000000002077782, 0.5000000000001820766, 0.5625000000001837419, 0.5937500000001907363, 0.6093750000001949552, 0.6171875000001970646, 0.6250000000001990630, 0.6875000000002183809, 0.7187500000002283729, 0.7343750000002405853, 0.7421875000002466916, 0.7460937500002428058, 0.7500000000002389200, 1.000000000000000000 ),
 .UNSPECIFIED. ) ;
#42570 = CIRCLE ( 'NONE', #33992, 4.000000000000001776 ) ;
#42571 = CARTESIAN_POINT ( 'NONE',  ( 17.50000000000001066, 45.00000000000000711, 63.82889773232136577 ) ) ;
#42572 = AXIS2_PLACEMENT_3D ( 'NONE', #85511, #69330, #45584 ) ;
#42573 = ORIENTED_EDGE ( 'NONE', *, *, #69083, .T. ) ;
#42574 = CARTESIAN_POINT ( 'NONE',  ( 60.56782644199743260, -25.59334256455847623, 67.17203146199634034 ) ) ;
#42575 = EDGE_CURVE ( 'NONE', #49860, #67806, #89256, .T. ) ;
#42576 = FACE_OUTER_BOUND ( 'NONE', #31808, .T. ) ;
#42577 = DIRECTION ( 'NONE',  ( -0.000000000000000000, -0.000000000000000000, -1.000000000000000000 ) ) ;
#42578 = CARTESIAN_POINT ( 'NONE',  ( -34.88410131646318746, 485.0165076724375126, -0.9913809214317844676 ) ) ;
#42579 = CARTESIAN_POINT ( 'NONE',  ( -32.95623456616201707, 360.3788937733320381, 22.49516265375592994 ) ) ;
#42580 = CARTESIAN_POINT ( 'NONE',  ( -17.49999999999999645, 2.500000000000000444, 0.000000000000000000 ) ) ;
#42581 = DIRECTION ( 'NONE',  ( 0.000000000000000000, -1.000000000000000000, 0.000000000000000000 ) ) ;
#42582 = CARTESIAN_POINT ( 'NONE',  ( 4.898587196589412829E-16, -27.12499999999999645, -8.000000000000000000 ) ) ;
#42583 = CARTESIAN_POINT ( 'NONE',  ( -2.457247124321397802, -12.61078973057452224, 32.17714155548836175 ) ) ;
#42584 = EDGE_CURVE ( 'NONE', #4171, #11109, #105308, .T. ) ;
#42585 = AXIS2_PLACEMENT_3D ( 'NONE', #63816, #31465, #104787 ) ;
#42586 = CARTESIAN_POINT ( 'NONE',  ( 95.70911704725124025, 5.000000000000042633, 6.123233995736805725E-16 ) ) ;
#42587 = VERTEX_POINT ( 'NONE', #79294 ) ;
#42588 = CARTESIAN_POINT ( 'NONE',  ( 86.25750675377733501, -18.23617246516705137, 169.8376886073401124 ) ) ;
#42590 =( GEOMETRIC_REPRESENTATION_CONTEXT ( 3 ) GLOBAL_UNCERTAINTY_ASSIGNED_CONTEXT ( ( #59144 ) ) GLOBAL_UNIT_ASSIGNED_CONTEXT ( ( #11342, #26533, #93885 ) ) REPRESENTATION_CONTEXT ( 'NONE', 'WORKASPACE' ) );
#42589 = CYLINDRICAL_SURFACE ( 'NONE', #54977, 5.000000000000002665 ) ;
#42591 = DIRECTION ( 'NONE',  ( -0.7071067811865555663, 8.659560562354833018E-17, -0.7071067811865393571 ) ) ;
#42592 = ORIENTED_EDGE ( 'NONE', *, *, #21994, .T. ) ;
#42593 = CARTESIAN_POINT ( 'NONE',  ( 0.000000000000000000, -19.99999999999998934, 0.000000000000000000 ) ) ;
#42594 = CARTESIAN_POINT ( 'NONE',  ( 43.71217423904101196, 435.6632154632235370, 9.092528312217412534 ) ) ;
#42595 = CARTESIAN_POINT ( 'NONE',  ( -32.91772945487021929, 464.9199415683336838, 10.91424143556015736 ) ) ;
#42596 = DIRECTION ( 'NONE',  ( 0.000000000000000000, 0.000000000000000000, 1.000000000000000000 ) ) ;
#42597 = CARTESIAN_POINT ( 'NONE',  ( -5.293743209235371339, -3.000000000000002665, -99.09939186120345767 ) ) ;
#42598 = CIRCLE ( 'NONE', #58071, 2.000000000000011102 ) ;
#42599 = CARTESIAN_POINT ( 'NONE',  ( -37.09836459488442273, -32.02632169008326457, -37.70790170121769336 ) ) ;
#42600 = CARTESIAN_POINT ( 'NONE',  ( -12.35738183340122553, -3.035458518230857106, 20.66409048039636076 ) ) ;
#42601 = ADVANCED_FACE ( 'NONE', ( #72265 ), #49654, .T. ) ;
#42602 = CARTESIAN_POINT ( 'NONE',  ( 44.74468937180378703, -60.00000000000000000, 60.10084534102561804 ) ) ;
#42603 = CARTESIAN_POINT ( 'NONE',  ( 30.56153846153846132, 4.172000000000003261, 0.000000000000000000 ) ) ;
#42604 = CARTESIAN_POINT ( 'NONE',  ( 5.384078575322348570, -12.92596998821031029, 32.09213580060114879 ) ) ;
#42605 = AXIS2_PLACEMENT_3D ( 'NONE', #78232, #4347, #62082 ) ;
#42607 = CARTESIAN_POINT ( 'NONE',  ( -12.32388454875233386, 22.37570981292809691, -6.328626427332589621 ) ) ;
#42606 = CARTESIAN_POINT ( 'NONE',  ( -13.36855599018907625, -21.80728118859962805, 35.71938858332402589 ) ) ;
#42608 = CARTESIAN_POINT ( 'NONE',  ( -9.482856158761270748, 87.44307115854722667, 3.177891129109650770 ) ) ;
#42609 = CARTESIAN_POINT ( 'NONE',  ( 31.08349330513380337, 4.000000000000003553, 0.000000000000000000 ) ) ;
#42610 = CARTESIAN_POINT ( 'NONE',  ( 46.00000000000000000, 450.0000000000002274, 13.20242257375370976 ) ) ;
#42611 = SURFACE_STYLE_FILL_AREA ( #25407 ) ;
#42612 = ORIENTED_EDGE ( 'NONE', *, *, #25850, .T. ) ;
#42613 = LINE ( 'NONE', #67442, #45043 ) ;
#42614 = AXIS2_PLACEMENT_3D ( 'NONE', #2787, #10864, #92861 ) ;
#42615 = CARTESIAN_POINT ( 'NONE',  ( -19.16305615217759950, 49.74182397839572900, 61.63059818732714490 ) ) ;
#42616 = CARTESIAN_POINT ( 'NONE',  ( 0.7145311798163198613, -4.618802153516998743, 7.999999999999998224 ) ) ;
#42617 =( BOUNDED_SURFACE ( )  B_SPLINE_SURFACE ( 3, 2, ( 
 ( #80050, #71973, #23993 ),
 ( #79003, #5123, #38056 ),
 ( #104881, #55758, #31021 ),
 ( #29949, #62833, #63902 ) ),
 .UNSPECIFIED., .F., .F., .F. ) 
 B_SPLINE_SURFACE_WITH_KNOTS ( ( 4, 4 ),
 ( 3, 3 ),
 ( -1.994931997373328159E-17, 0.003511371752234733381 ),
 ( 0.000000000000000000, 1.000000000000000000 ),
 .UNSPECIFIED. ) 
 GEOMETRIC_REPRESENTATION_ITEM ( )  RATIONAL_B_SPLINE_SURFACE ( (
 ( 1.000000000000000000, 0.7409272757993310421, 1.000000000000000000),
 ( 1.000000000000000000, 0.7572402302192458023, 1.000000000000000000),
 ( 1.000000000000000000, 0.7731133056331223052, 1.000000000000000000),
 ( 1.000000000000000000, 0.7888522786294931421, 1.000000000000000000) ) ) 
 REPRESENTATION_ITEM ( '' )  SURFACE ( )  );
#42618 = EDGE_CURVE ( 'NONE', #58946, #12676, #46216, .T. ) ;
#42620 = CARTESIAN_POINT ( 'NONE',  ( 46.51529756520770320, -21.77006784196455413, -26.23302849808148807 ) ) ;
#42619 = CARTESIAN_POINT ( 'NONE',  ( 4.524538969695734991, 53.69347865467890557, 8.282048616735908197 ) ) ;
#42621 = ORIENTED_EDGE ( 'NONE', *, *, #20965, .F. ) ;
#42622 = CARTESIAN_POINT ( 'NONE',  ( -5.725004243152312711, -88.57519148255366304, -1.812899781754687911 ) ) ;
#42623 = CARTESIAN_POINT ( 'NONE',  ( 24.05868969682389036, 6.123233995736770227E-16, -5.000000000000002665 ) ) ;
#42624 = CIRCLE ( 'NONE', #75352, 4.172000000000001485 ) ;
#42625 = CIRCLE ( 'NONE', #71969, 3.000000000000018208 ) ;
#42626 = ORIENTED_EDGE ( 'NONE', *, *, #24029, .T. ) ;
#42627 = EDGE_CURVE ( 'NONE', #100209, #43603, #61586, .T. ) ;
#42628 = CARTESIAN_POINT ( 'NONE',  ( -10.00000000000000000, 0.000000000000000000, 10.00000000000000000 ) ) ;
#42629 = DIRECTION ( 'NONE',  ( -0.5735764363510497121, 0.8191520442889892450, 1.003171929053521665E-16 ) ) ;
#42630 = CARTESIAN_POINT ( 'NONE',  ( -25.18435656174467141, 41.53024528245975944, -72.71459547366467291 ) ) ;
#42631 = CARTESIAN_POINT ( 'NONE',  ( -104.1877734966528379, -60.00000000000001421, 105.5540295569807654 ) ) ;
#42632 = AXIS2_PLACEMENT_3D ( 'NONE', #65454, #8264, #41177 ) ;
#42633 =( GEOMETRIC_REPRESENTATION_CONTEXT ( 3 ) GLOBAL_UNCERTAINTY_ASSIGNED_CONTEXT ( ( #23290 ) ) GLOBAL_UNIT_ASSIGNED_CONTEXT ( ( #19208, #67711, #11042 ) ) REPRESENTATION_CONTEXT ( 'NONE', 'WORKASPACE' ) );
#42634 = CARTESIAN_POINT ( 'NONE',  ( -16.07917213302881621, 5.118112109480979832, 4.258304778710242822 ) ) ;
#42635 = CONICAL_SURFACE ( 'NONE', #70216, 4.172000000000001485, 0.9599310885968750373 ) ;
#42636 = LINE ( 'NONE', #58839, #64135 ) ;
#42637 = CARTESIAN_POINT ( 'NONE',  ( 41.35951450183790712, 460.7308729162546683, 2.709719765170301109 ) ) ;
#42639 = CARTESIAN_POINT ( 'NONE',  ( -15.43348245327105062, 2.792842261934127990, -2.002630087548765925 ) ) ;
#42638 = CARTESIAN_POINT ( 'NONE',  ( -33.26776902584375506, 435.2199417381641524, 10.58436218359535985 ) ) ;
#42640 = CARTESIAN_POINT ( 'NONE',  ( -80.80365086073496173, -60.48046949481216217, 181.9398151766872616 ) ) ;
#42641 = EDGE_LOOP ( 'NONE', ( #105689, #2165, #25862, #2082, #96329 ) ) ;
#42642 = CARTESIAN_POINT ( 'NONE',  ( 0.000000000000000000, 0.000000000000000000, -25.03750572909317285 ) ) ;
#42643 = EDGE_CURVE ( 'NONE', #88814, #30156, #11780, .T. ) ;
#42644 = ORIENTED_EDGE ( 'NONE', *, *, #55966, .T. ) ;
#42645 = VERTEX_POINT ( 'NONE', #72781 ) ;
#42646 = COLOUR_RGB ( '', 0.08235294, 0.09019608, 0.10196078) ;
#42647 = CARTESIAN_POINT ( 'NONE',  ( -4.369287899246183215, -1.129960224643866251, 104.3947014718172142 ) ) ;
#42648 = CARTESIAN_POINT ( 'NONE',  ( 0.01372220897661698483, 5.948365447239581272, 2.697128823393880381 ) ) ;
#42649 = EDGE_LOOP ( 'NONE', ( #99219, #41979 ) ) ;
#42650 = CARTESIAN_POINT ( 'NONE',  ( -72.95843482080444176, -52.66112468364584487, -23.75230364563115515 ) ) ;
#42651 = DIRECTION ( 'NONE',  ( 0.8191520442889881348, 0.000000000000000000, 0.5735764363510513775 ) ) ;
#42652 = LINE ( 'NONE', #16245, #21579 ) ;
#42653 = CARTESIAN_POINT ( 'NONE',  ( -3.461462603046343123, 15.83153173276467385, 6.086477152069783791 ) ) ;
#42654 = CARTESIAN_POINT ( 'NONE',  ( 90.51111111111110574, 4.172000000000019249, 5.109226446042768454E-16 ) ) ;
#42655 =( LENGTH_UNIT ( ) NAMED_UNIT ( * ) SI_UNIT ( .MILLI., .METRE. ) );
#42656 = DIRECTION ( 'NONE',  ( 1.000000000000000000, 0.000000000000000000, 0.000000000000000000 ) ) ;
#42657 = CARTESIAN_POINT ( 'NONE',  ( 101.8005042720997864, -59.99999999999995026, 77.51357286062189189 ) ) ;
#42658 = CARTESIAN_POINT ( 'NONE',  ( -78.18420296597048491, -29.99999999999999645, 185.0796872551976548 ) ) ;
#42659 = CARTESIAN_POINT ( 'NONE',  ( -60.17200676404426929, -32.54305267341962349, 69.40168963351582931 ) ) ;
#42660 = CIRCLE ( 'NONE', #25542, 4.172000000000009479 ) ;
#42661 = ORIENTED_EDGE ( 'NONE', *, *, #18103, .T. ) ;
#42662 = CARTESIAN_POINT ( 'NONE',  ( 6.013174582917088173, 14.79219749984193477, 3.585507868043892987 ) ) ;
#42663 = CARTESIAN_POINT ( 'NONE',  ( 79.18410244169839984, -60.00000000000243006, -31.08583709693218822 ) ) ;
#42664 = ORIENTED_EDGE ( 'NONE', *, *, #12758, .T. ) ;
#42665 = CARTESIAN_POINT ( 'NONE',  ( 4.019035380416646319, -32.51031334268923700, 29.30096715606009283 ) ) ;
#42666 = CARTESIAN_POINT ( 'NONE',  ( -104.4037492068304260, -60.15596781628350698, 189.8437866221127024 ) ) ;
#42667 = CARTESIAN_POINT ( 'NONE',  ( 5.947762761376476526, 4.378239541354659536, -5.416666666666666075 ) ) ;
#42668 = SURFACE_STYLE_FILL_AREA ( #2192 ) ;
#42669 = AXIS2_PLACEMENT_3D ( 'NONE', #8317, #99442, #57926 ) ;
#42670 =( NAMED_UNIT ( * ) PLANE_ANGLE_UNIT ( ) SI_UNIT ( $, .RADIAN. ) );
#42671 = ORIENTED_EDGE ( 'NONE', *, *, #6324, .T. ) ;
#42672 = CARTESIAN_POINT ( 'NONE',  ( -1.104211576045346144, -14.95094041744786750, -0.8377008405913687339 ) ) ;
#42673 = CARTESIAN_POINT ( 'NONE',  ( -32.39506591613324815, -60.00000000000001421, 44.41584490438672361 ) ) ;
#42674 = CARTESIAN_POINT ( 'NONE',  ( -3.604576940039238675, -1.047841513645850098, 104.3731177596920787 ) ) ;
#42675 = CARTESIAN_POINT ( 'NONE',  ( 7.188101187500001821, -19.43750000204838457, -2.977408999572650483 ) ) ;
#42676 = CARTESIAN_POINT ( 'NONE',  ( 0.000000000000000000, 0.000000000000000000, 0.000000000000000000 ) ) ;
#42677 = CIRCLE ( 'NONE', #58142, 2.999999999999999112 ) ;
#42678 = CARTESIAN_POINT ( 'NONE',  ( 33.00000000000000000, 464.3970849722209095, 17.41240408234224191 ) ) ;
#42679 = CARTESIAN_POINT ( 'NONE',  ( 0.000000000000000000, -8.673617379884035472E-16, -17.01589776168603407 ) ) ;
#42680 = CARTESIAN_POINT ( 'NONE',  ( -11.53688828317231874, -4.929764295086950021, -12.56596437507229247 ) ) ;
#42681 =( NAMED_UNIT ( * ) SI_UNIT ( $, .STERADIAN. ) SOLID_ANGLE_UNIT ( ) );
#42682 = CARTESIAN_POINT ( 'NONE',  ( 5.892857268295339068, -15.73409625558654135, 14.28797240113282818 ) ) ;
#42683 = CARTESIAN_POINT ( 'NONE',  ( -24.20637929534487398, 27.76268499971478931, 31.17501708768064717 ) ) ;
#42684 = ADVANCED_FACE ( 'NONE', ( #105687 ), #46728, .T. ) ;
#42685 = CARTESIAN_POINT ( 'NONE',  ( 106.0683871028796688, -60.00000000000002132, 161.6282514473857077 ) ) ;
#42686 = UNCERTAINTY_MEASURE_WITH_UNIT (LENGTH_MEASURE( 1.000000000000000082E-05 ), #58899, 'distance_accuracy_value', 'NONE');
#42687 = CARTESIAN_POINT ( 'NONE',  ( -30.31278797052050678, -25.59859917315953481, 30.73255412779541373 ) ) ;
#42688 = CARTESIAN_POINT ( 'NONE',  ( 0.000000000000000000, 0.000000000000000000, 4.000000000000000000 ) ) ;
#42689 = CARTESIAN_POINT ( 'NONE',  ( 43.76121681010938858, -32.61635124531981234, 40.47551691563658238 ) ) ;
#42690 = PRESENTATION_STYLE_ASSIGNMENT (( #74514 ) ) ;
#42691 = EDGE_LOOP ( 'NONE', ( #80619, #80324, #80549, #59596 ) ) ;
#42692 = EDGE_CURVE ( 'NONE', #74150, #3192, #25489, .T. ) ;
#42694 = CIRCLE ( 'NONE', #58238, 4.000000000000000888 ) ;
#42693 = CARTESIAN_POINT ( 'NONE',  ( 43.71675722381548468, 435.0430370927871309, 11.37024750953607288 ) ) ;
#42695 = CARTESIAN_POINT ( 'NONE',  ( -80.28562564763434750, -38.80141483586817230, 193.4884166117294910 ) ) ;
#42696 = ORIENTED_EDGE ( 'NONE', *, *, #31661, .T. ) ;
#42697 = CARTESIAN_POINT ( 'NONE',  ( 76.12557658274099026, -38.35599704320051018, -28.58424740099938077 ) ) ;
#42698 = CARTESIAN_POINT ( 'NONE',  ( 16.69491137615832699, -59.99999999999998579, 34.10659378815499565 ) ) ;
#42699 = DIRECTION ( 'NONE',  ( -1.000000000000000000, 0.000000000000000000, 0.000000000000000000 ) ) ;
#42700 = CARTESIAN_POINT ( 'NONE',  ( -7.182275917706625101, 41.30104301296705671, -58.77094024890655533 ) ) ;
#42701 = CARTESIAN_POINT ( 'NONE',  ( 9.380169522195144438, 15.95824666716552009, -3.484756791224365990 ) ) ;
#42702 = DIRECTION ( 'NONE',  ( -1.000000000000000000, -1.224606353822377258E-16, -0.000000000000000000 ) ) ;
#42703 = CARTESIAN_POINT ( 'NONE',  ( -24.83963492381722915, 307.1563561209093223, 9.458452572052934215 ) ) ;
#42704 = AXIS2_PLACEMENT_3D ( 'NONE', #59391, #99824, #100884 ) ;
#42705 = CARTESIAN_POINT ( 'NONE',  ( 108.9327471971628540, -60.00000000000001421, 135.4986037201063596 ) ) ;
#42707 = AXIS2_PLACEMENT_3D ( 'NONE', #87721, #102837, #13803 ) ;
#42706 = B_SPLINE_CURVE_WITH_KNOTS ( 'NONE', 3,
 ( #52898, #97451, #73166, #6856, #45869, #106071 ),
 .UNSPECIFIED., .F., .F.,
 ( 4, 2, 4 ),
 ( 2.380733003136001779E-07, 0.001898835937927382872, 0.003797433802554452380 ),
 .UNSPECIFIED. ) ;
#42708 = LINE ( 'NONE', #75603, #89007 ) ;
#42709 = DIRECTION ( 'NONE',  ( 1.000000000000000000, 1.224606353822377258E-16, 0.000000000000000000 ) ) ;
#42710 = EDGE_LOOP ( 'NONE', ( #53840, #20880, #34697 ) ) ;
#42711 = EDGE_CURVE ( 'NONE', #59047, #6978, #3173, .T. ) ;
#42712 = CARTESIAN_POINT ( 'NONE',  ( -100.2311398323353018, -29.99999999999999289, 184.5300451475501688 ) ) ;
#42713 = ORIENTED_EDGE ( 'NONE', *, *, #94792, .F. ) ;
#42714 = DIRECTION ( 'NONE',  ( 1.000000000000000000, 0.000000000000000000, 0.000000000000000000 ) ) ;
#42715 =( NAMED_UNIT ( * ) PLANE_ANGLE_UNIT ( ) SI_UNIT ( $, .RADIAN. ) );
#42716 = CARTESIAN_POINT ( 'NONE',  ( 23.71188932895429247, 304.9123084062130147, 10.16850580752430133 ) ) ;
#42718 = CARTESIAN_POINT ( 'NONE',  ( 0.000000000000000000, 0.000000000000000000, 0.000000000000000000 ) ) ;
#42717 =( GEOMETRIC_REPRESENTATION_CONTEXT ( 3 ) GLOBAL_UNCERTAINTY_ASSIGNED_CONTEXT ( ( #102247 ) ) GLOBAL_UNIT_ASSIGNED_CONTEXT ( ( #54432, #31795, #6423 ) ) REPRESENTATION_CONTEXT ( 'NONE', 'WORKASPACE' ) );
#42719 = CIRCLE ( 'NONE', #11742, 5.000000000000001776 ) ;
#42720 = CARTESIAN_POINT ( 'NONE',  ( 4.401442555609581635E-16, -20.65625000204838813, -7.188101187500000044 ) ) ;
#42721 = CARTESIAN_POINT ( 'NONE',  ( -6.902527771671634227, -4.675077770780910136, -0.7026937717022843088 ) ) ;
#42722 = CONICAL_SURFACE ( 'NONE', #25519, 4.172000000000009479, 0.9599310885968813656 ) ;
#42723 = UNCERTAINTY_MEASURE_WITH_UNIT (LENGTH_MEASURE( 1.000000000000000082E-05 ), #82239, 'distance_accuracy_value', 'NONE');
#42724 = VECTOR ( 'NONE', #52665, 1000.000000000000000 ) ;
#42725 = DIRECTION ( 'NONE',  ( 0.000000000000000000, -1.000000000000000000, 0.000000000000000000 ) ) ;
#42726 = ORIENTED_EDGE ( 'NONE', *, *, #39358, .F. ) ;
#42727 = CARTESIAN_POINT ( 'NONE',  ( 81.53240055878744386, -46.44585284538660375, 167.1415864390550041 ) ) ;
#42728 = DIRECTION ( 'NONE',  ( -0.5735764363510510444, -0.8191520442889883569, 0.000000000000000000 ) ) ;
#42729 = FACE_OUTER_BOUND ( 'NONE', #8316, .T. ) ;
#42730 = EDGE_LOOP ( 'NONE', ( #33639, #47337, #2772, #103749, #59504, #87987 ) ) ;
#42731 = CARTESIAN_POINT ( 'NONE',  ( 67.22793774957824553, 6.975173280561618775E-15, 0.000000000000000000 ) ) ;
#42732 = CARTESIAN_POINT ( 'NONE',  ( -47.90297653514730314, 15.22282649863647919, 16.85535821593517269 ) ) ;
#42733 = DIRECTION ( 'NONE',  ( 0.000000000000000000, 0.000000000000000000, 1.000000000000000000 ) ) ;
#42734 = CARTESIAN_POINT ( 'NONE',  ( 30.00000000000000355, 488.7105343895291298, 4.072475192012525724 ) ) ;
#42735 = CARTESIAN_POINT ( 'NONE',  ( -5.909155701201250110, 253.8626168018873273, 1.073778020691660062 ) ) ;
#42736 = CARTESIAN_POINT ( 'NONE',  ( -33.14436125469611483, 382.5759126738042255, 24.99667975960740307 ) ) ;
#42737 = DIRECTION ( 'NONE',  ( -1.000000000000000000, -1.224606353822377258E-16, -0.000000000000000000 ) ) ;
#42738 = ORIENTED_EDGE ( 'NONE', *, *, #38175, .F. ) ;
#42739 = PRESENTATION_STYLE_ASSIGNMENT (( #58392 ) ) ;
#42740 = CARTESIAN_POINT ( 'NONE',  ( -6.500000000000000000, -0.6456425506958787253, 3.045930478326464019E-15 ) ) ;
#42741 = CARTESIAN_POINT ( 'NONE',  ( 32.23780387954349891, 18.64284798592760239, 20.91998874883894644 ) ) ;
#42742 = CARTESIAN_POINT ( 'NONE',  ( 87.29696987635691130, -42.74777952954144666, 190.3637657847306457 ) ) ;
#42743 = CYLINDRICAL_SURFACE ( 'NONE', #25873, 8.000000000000000000 ) ;
#42744 = B_SPLINE_CURVE_WITH_KNOTS ( 'NONE', 3,
 ( #24962, #57816, #91806, #74538, #67535, #10336, #100415, #99885, #83171, #50780, #66457, #8744, #17927, #82644, #83692, #26580, #41652, #59448, #43252, #17394, #9269, #100947 ),
 .UNSPECIFIED., .F., .F.,
 ( 4, 2, 2, 2, 2, 2, 2, 2, 2, 2, 4 ),
 ( 0.007124701767327336864, 0.007629109439095383555, 0.008133517110863429378, 0.008385720946747459228, 0.008637924782631487344, 0.009142332454399534902, 0.009646740126167582460, 0.009898943962051603637, 0.01015114779793562655, 0.01065555546970366890, 0.01115996314147171299 ),
 .UNSPECIFIED. ) ;
#42745 = CIRCLE ( 'NONE', #99637, 1.000000000000005329 ) ;
#42746 = CARTESIAN_POINT ( 'NONE',  ( 2.977408999572651815, -29.93750000204839523, 7.188101187500000933 ) ) ;
#42747 = CARTESIAN_POINT ( 'NONE',  ( 0.000000000000000000, 47.00000000000000000, 0.000000000000000000 ) ) ;
#42748 = CARTESIAN_POINT ( 'NONE',  ( 7.803955644651615842, 52.08656169318132356, 1.781976911754487913 ) ) ;
#42749 = CARTESIAN_POINT ( 'NONE',  ( 33.00000000000000000, 450.0000000000002274, 13.20242257375370976 ) ) ;
#42750 = ORIENTED_EDGE ( 'NONE', *, *, #53839, .T. ) ;
#42751 = CARTESIAN_POINT ( 'NONE',  ( 1.101948812519610632, 43.39583042475737784, 18.11144527318901254 ) ) ;
#42752 = SURFACE_SIDE_STYLE ('',( #72463 ) ) ;
#42753 = DIRECTION ( 'NONE',  ( -1.000000000000000000, -0.000000000000000000, -0.000000000000000000 ) ) ;
#42754 = EDGE_CURVE ( 'NONE', #79974, #69611, #51217, .T. ) ;
#42755 = ORIENTED_EDGE ( 'NONE', *, *, #29584, .T. ) ;
#42756 = AXIS2_PLACEMENT_3D ( 'NONE', #5491, #105762, #6530 ) ;
#42757 = DIRECTION ( 'NONE',  ( -0.000000000000000000, -1.000000000000000000, -0.000000000000000000 ) ) ;
#42758 = ORIENTED_EDGE ( 'NONE', *, *, #75137, .F. ) ;
#42759 = STYLED_ITEM ( 'NONE', ( #77332 ), #2839 ) ;
#42760 = EDGE_CURVE ( 'NONE', #32993, #85882, #66923, .T. ) ;
#42761 = CARTESIAN_POINT ( 'NONE',  ( 32.10720520530002631, 436.4653991243506539, 19.53468662359128771 ) ) ;
#42762 = DIRECTION ( 'NONE',  ( -1.000000000000000000, -1.224606353822377258E-16, -0.000000000000000000 ) ) ;
#42763 = FILL_AREA_STYLE_COLOUR ( '', #53050 ) ;
#42764 = CARTESIAN_POINT ( 'NONE',  ( -76.02354287597104587, -59.99999999999999289, 187.0617520462423329 ) ) ;
#42765 = CARTESIAN_POINT ( 'NONE',  ( -45.40507512465600115, 439.2794387026467575, 6.273370203490043373 ) ) ;
#42767 = CONICAL_SURFACE ( 'NONE', #101369, 11.27631144943088337, 1.221730476396025722 ) ;
#42766 = DIRECTION ( 'NONE',  ( 1.000000000000000000, 0.000000000000000000, 0.000000000000000000 ) ) ;
#42768 = CARTESIAN_POINT ( 'NONE',  ( -45.40507512465600115, 439.2794387026467575, 6.273370203490043373 ) ) ;
#42769 = CIRCLE ( 'NONE', #54779, 3.309500000000001663 ) ;
#42770 = CARTESIAN_POINT ( 'NONE',  ( -83.13823174912079139, -60.94556865090731179, 190.8875103384814054 ) ) ;
#42771 = ORIENTED_EDGE ( 'NONE', *, *, #16415, .T. ) ;
#42772 = ADVANCED_FACE ( 'NONE', ( #453 ), #101343, .T. ) ;
#42773 = ORIENTED_EDGE ( 'NONE', *, *, #84570, .F. ) ;
#42774 = CARTESIAN_POINT ( 'NONE',  ( 16.03934073995819531, 4.450581328273877979, -3.145353196822298969 ) ) ;
#42775 = CARTESIAN_POINT ( 'NONE',  ( 3.801077171203083527, -1.110903940591797090, 104.1059035333591112 ) ) ;
#42776 = CARTESIAN_POINT ( 'NONE',  ( -83.25012535261359403, -37.79396785790730462, -5.748279069099496041 ) ) ;
#42777 = CARTESIAN_POINT ( 'NONE',  ( -3.208180356138712330, -10.20788741807813516, -11.61546768905594185 ) ) ;
#42778 = STYLED_ITEM ( 'NONE', ( #33271 ), #27337 ) ;
#42779 = CARTESIAN_POINT ( 'NONE',  ( -30.00000000000000000, 461.8423635046866025, 11.25802415799497247 ) ) ;
#42780 = CARTESIAN_POINT ( 'NONE',  ( -43.00000000000000000, 500.0000000000002274, 0.000000000000000000 ) ) ;
#42782 = LINE ( 'NONE', #61107, #18267 ) ;
#42781 = AXIS2_PLACEMENT_3D ( 'NONE', #39625, #47155, #87113 ) ;
#42783 = CARTESIAN_POINT ( 'NONE',  ( 45.60838156032635027, 42.00000000000000000, 79.13121736029046360 ) ) ;
#42784 = CIRCLE ( 'NONE', #85866, 5.000000000000011546 ) ;
#42785 = DIRECTION ( 'NONE',  ( 0.000000000000000000, -1.000000000000000000, 0.000000000000000000 ) ) ;
#42786 = CARTESIAN_POINT ( 'NONE',  ( 77.10949051821226874, -30.00000000000007461, 176.8385238405566326 ) ) ;
#42787 = CARTESIAN_POINT ( 'NONE',  ( -36.50546997061886856, 437.5879066196182521, 4.249723241245790817 ) ) ;
#42788 = CARTESIAN_POINT ( 'NONE',  ( -2.770043159915164477, -30.00000000000000355, -40.00000000000000000 ) ) ;
#42789 = CARTESIAN_POINT ( 'NONE',  ( -69.71213741151544241, -22.11141246496202939, 91.06144798064602242 ) ) ;
#42790 = ORIENTED_EDGE ( 'NONE', *, *, #83951, .T. ) ;
#42791 = CARTESIAN_POINT ( 'NONE',  ( 68.01663869669266660, -29.99999999999994316, 119.4502877181080862 ) ) ;
#42792 = CARTESIAN_POINT ( 'NONE',  ( 64.12443038224847669, 40.83928227018758861, -11.04305639294624264 ) ) ;
#42793 = CARTESIAN_POINT ( 'NONE',  ( 36.87124630340465359, -59.99999999999258193, 51.79591773974985358 ) ) ;
#42794 = CIRCLE ( 'NONE', #87549, 4.171999999999999709 ) ;
#42795 = ORIENTED_EDGE ( 'NONE', *, *, #67403, .T. ) ;
#42796 = CARTESIAN_POINT ( 'NONE',  ( 12.32179744594563608, -10.26684526391957952, 10.94526264208287181 ) ) ;
#42797 = CARTESIAN_POINT ( 'NONE',  ( 4.401442555609581635E-16, -25.15625000204838813, -7.188101187500000044 ) ) ;
#42798 = CARTESIAN_POINT ( 'NONE',  ( 25.11650669486618881, 1.474610560812782335E-15, 0.000000000000000000 ) ) ;
#42799 = ORIENTED_EDGE ( 'NONE', *, *, #16962, .F. ) ;
#42800 = PLANE ( 'NONE',  #66512 ) ;
#42801 = DIRECTION ( 'NONE',  ( 1.000000000000000000, -0.000000000000000000, 1.224646799147353207E-16 ) ) ;
#42802 = CARTESIAN_POINT ( 'NONE',  ( 31.90667051052400183, 313.6962960773610689, -7.665056271795368303 ) ) ;
#42803 = CARTESIAN_POINT ( 'NONE',  ( -7.188101187500000044, -15.40625000204838635, -8.802885111219163269E-16 ) ) ;
#42804 = CARTESIAN_POINT ( 'NONE',  ( -49.25896281664908827, 12.93370316445966317, 15.83749202751426033 ) ) ;
#42805 = DIRECTION ( 'NONE',  ( -0.000000000000000000, -0.000000000000000000, -1.000000000000000000 ) ) ;
#42806 = DIRECTION ( 'NONE',  ( -1.000000000000000000, -1.224606353822377258E-16, -0.000000000000000000 ) ) ;
#42807 = CARTESIAN_POINT ( 'NONE',  ( 11.28790243858419906, 9.071383756617064975, -12.46447053051442744 ) ) ;
#42808 = CARTESIAN_POINT ( 'NONE',  ( -33.00000000000000000, 439.0771093100264011, 24.89389206971033630 ) ) ;
#42809 = CARTESIAN_POINT ( 'NONE',  ( -11.43775816216262697, 48.00000000000000711, -94.77568223238722567 ) ) ;
#42810 = EDGE_CURVE ( 'NONE', #2343, #54954, #986, .T. ) ;
#42811 = AXIS2_PLACEMENT_3D ( 'NONE', #100336, #26500, #100866 ) ;
#42812 = ORIENTED_EDGE ( 'NONE', *, *, #94239, .T. ) ;
#42813 = CARTESIAN_POINT ( 'NONE',  ( -7.311409912948124479, 40.00000000004124701, -70.68780158692078430 ) ) ;
#42814 = CARTESIAN_POINT ( 'NONE',  ( 32.86303424572704301, -39.49211861081180786, 34.27957772689813254 ) ) ;
#42815 = CARTESIAN_POINT ( 'NONE',  ( 35.49008156062310348, 378.5703878965198896, 5.677488699590466759 ) ) ;
#42816 = ORIENTED_EDGE ( 'NONE', *, *, #70438, .F. ) ;
#42817 = ADVANCED_FACE ( 'NONE', ( #20342 ), #18678, .T. ) ;
#42818 = ADVANCED_FACE ( 'NONE', ( #54212 ), #87374, .T. ) ;
#42819 = CARTESIAN_POINT ( 'NONE',  ( -0.9432938954576324253, 17.83686411059527899, 49.67615204089843672 ) ) ;
#42820 = AXIS2_PLACEMENT_3D ( 'NONE', #47120, #71394, #6665 ) ;
#42821 = ORIENTED_EDGE ( 'NONE', *, *, #14379, .F. ) ;
#42822 = CARTESIAN_POINT ( 'NONE',  ( 0.000000000000000000, 70.00000000000000000, 0.000000000000000000 ) ) ;
#42823 = CARTESIAN_POINT ( 'NONE',  ( 4.933292146132942868, 41.54835750584369691, -70.57172791956975288 ) ) ;
#42824 = CARTESIAN_POINT ( 'NONE',  ( -44.26028122668987663, 485.3157014729772527, 1.872110468834934371 ) ) ;
#42825 = FILL_AREA_STYLE ('',( #91392 ) ) ;
#42826 = DIRECTION ( 'NONE',  ( 0.000000000000000000, 0.000000000000000000, 1.000000000000000000 ) ) ;
#42827 = CARTESIAN_POINT ( 'NONE',  ( 1.115733355096011570, 14.48162342373252720, -51.08071913610608306 ) ) ;
#42829 = ORIENTED_EDGE ( 'NONE', *, *, #43845, .T. ) ;
#42828 = CIRCLE ( 'NONE', #97942, 15.00000000000000711 ) ;
#42830 = CARTESIAN_POINT ( 'NONE',  ( 91.68327619457986088, -59.99999999999998579, -15.06735680088440965 ) ) ;
#42831 = CARTESIAN_POINT ( 'NONE',  ( -9.721687949930888806, 46.20860120156269346, 13.03939565591211469 ) ) ;
#42832 = CARTESIAN_POINT ( 'NONE',  ( 42.08762648273149409, 487.0030674539048618, 9.106351919857861077 ) ) ;
#42833 = CARTESIAN_POINT ( 'NONE',  ( -47.18437091044132359, 18.47854193719484428, -14.68206053360911945 ) ) ;
#42834 = ORIENTED_EDGE ( 'NONE', *, *, #18821, .T. ) ;
#42835 = ADVANCED_FACE ( 'NONE', ( #70434 ), #75459, .T. ) ;
#42836 = DIRECTION ( 'NONE',  ( 0.000000000000000000, -1.000000000000000000, 0.000000000000000000 ) ) ;
#42837 = VERTEX_POINT ( 'NONE', #38094 ) ;
#42838 = VECTOR ( 'NONE', #35739, 1000.000000000000000 ) ;
#42839 = ORIENTED_EDGE ( 'NONE', *, *, #56547, .T. ) ;
#42840 = CARTESIAN_POINT ( 'NONE',  ( 0.000000000000000000, 0.000000000000000000, -7.424942857142857733 ) ) ;
#42841 = FILL_AREA_STYLE_COLOUR ( '', #76983 ) ;
#42842 = DIRECTION ( 'NONE',  ( 0.000000000000000000, -1.000000000000000000, 0.000000000000000000 ) ) ;
#42843 = DIRECTION ( 'NONE',  ( -1.000000000000000000, -1.224606353822377258E-16, -0.000000000000000000 ) ) ;
#42844 = CARTESIAN_POINT ( 'NONE',  ( 84.05867435070005911, -52.73583259645541688, -15.15229210315370167 ) ) ;
#42845 = CARTESIAN_POINT ( 'NONE',  ( -40.50844031276214707, 311.4578814011395593, -6.061433927898559837 ) ) ;
#42846 = CARTESIAN_POINT ( 'NONE',  ( -3.389927784054740378, 303.8518027742029517, -9.999999999492535707 ) ) ;
#42847 = CARTESIAN_POINT ( 'NONE',  ( 12.50000000000000533, 32.24110320235760696, -50.45876292934040208 ) ) ;
#42848 = ORIENTED_EDGE ( 'NONE', *, *, #72420, .F. ) ;
#42849 = EDGE_CURVE ( 'NONE', #105603, #18398, #13468, .T. ) ;
#42850 = CARTESIAN_POINT ( 'NONE',  ( 6.499999999999999112, 3.149025070564777984, -0.5705737632551077798 ) ) ;
#42851 = ORIENTED_EDGE ( 'NONE', *, *, #104754, .T. ) ;
#42852 = CARTESIAN_POINT ( 'NONE',  ( 0.000000000000000000, 0.000000000000000000, 5.000000000000002665 ) ) ;
#42853 = SURFACE_STYLE_FILL_AREA ( #48799 ) ;
#42854 = EDGE_CURVE ( 'NONE', #15159, #63037, #97445, .T. ) ;
#42856 = EDGE_LOOP ( 'NONE', ( #45, #65114, #9283, #105571, #30953 ) ) ;
#42855 = CARTESIAN_POINT ( 'NONE',  ( 0.000000000000000000, 0.000000000000000000, 0.000000000000000000 ) ) ;
#42857 = CARTESIAN_POINT ( 'NONE',  ( 73.37940478702553548, -60.31994814604785660, 129.0810991085878925 ) ) ;
#42858 = AXIS2_PLACEMENT_3D ( 'NONE', #32034, #17437, #105375 ) ;
#42859 = VERTEX_POINT ( 'NONE', #78504 ) ;
#42860 = CARTESIAN_POINT ( 'NONE',  ( 6.999999998637613352, -46.54042759438532784, 39.12435565376871693 ) ) ;
#42861 = DIRECTION ( 'NONE',  ( -1.000000000000000000, -1.224606353822377258E-16, -0.000000000000000000 ) ) ;
#42862 = CARTESIAN_POINT ( 'NONE',  ( -2.977408999572650039, -24.68750000204838813, -7.188101187500000933 ) ) ;
#42863 = CARTESIAN_POINT ( 'NONE',  ( -91.26204144827082132, -57.66323380191850845, -20.53964676755072105 ) ) ;
#42864 = ORIENTED_EDGE ( 'NONE', *, *, #50118, .F. ) ;
#42865 = LINE ( 'NONE', #90895, #31702 ) ;
#42866 = CARTESIAN_POINT ( 'NONE',  ( 104.5564995939975574, -52.71703362910472634, 183.8354400015944918 ) ) ;
#42867 = AXIS2_PLACEMENT_3D ( 'NONE', #76407, #83441, #18755 ) ;
#42868 = CARTESIAN_POINT ( 'NONE',  ( 6.488302422815169557, 51.35002353678540743, -7.646734246321329032 ) ) ;
#42869 = DIRECTION ( 'NONE',  ( -1.000000000000000000, 0.000000000000000000, 0.000000000000000000 ) ) ;
#42870 = CARTESIAN_POINT ( 'NONE',  ( -8.000000000000000000, -25.43750000409677270, -9.797174393178825657E-16 ) ) ;
#42871 = CARTESIAN_POINT ( 'NONE',  ( 0.000000000000000000, 60.00000000000000000, 6.999999999999992895 ) ) ;
#42872 = PRESENTATION_LAYER_ASSIGNMENT (  '', '', ( #106612 ) ) ;
#42873 = CARTESIAN_POINT ( 'NONE',  ( 13.86650669486618881, 1.474610560812782335E-15, 0.000000000000000000 ) ) ;
#42874 = FILL_AREA_STYLE ('',( #9970 ) ) ;
#42875 = FACE_OUTER_BOUND ( 'NONE', #47098, .T. ) ;
#42876 = B_SPLINE_CURVE_WITH_KNOTS ( 'NONE', 3,
 ( #84880, #78372, #10966, #93516 ),
 .UNSPECIFIED., .F., .F.,
 ( 4, 4 ),
 ( 1.110764993427085326E-17, 0.002190562081029153070 ),
 .UNSPECIFIED. ) ;
#42877 = DIRECTION ( 'NONE',  ( -0.000000000000000000, -0.000000000000000000, -1.000000000000000000 ) ) ;
#42878 = DIRECTION ( 'NONE',  ( 4.233437538138742344E-17, 0.1845977156002912289, 0.9828141652393672656 ) ) ;
#42879 = CARTESIAN_POINT ( 'NONE',  ( -2.701558353794590861, 15.00000000000000000, -9.999999999999998224 ) ) ;
#42880 = VERTEX_POINT ( 'NONE', #31582 ) ;
#42881 = DIRECTION ( 'NONE',  ( -0.000000000000000000, -1.000000000000000000, -0.000000000000000000 ) ) ;
#42882 = CARTESIAN_POINT ( 'NONE',  ( 22.61650669486618526, 1.474610560812782335E-15, 0.000000000000000000 ) ) ;
#42883 = CARTESIAN_POINT ( 'NONE',  ( 1.250953595776213900, 10.43180450791889413, 50.60765994387645605 ) ) ;
#42884 = CARTESIAN_POINT ( 'NONE',  ( -90.11912501425099720, -29.99999999999998934, 189.9661090405622019 ) ) ;
#42885 = EDGE_CURVE ( 'NONE', #39611, #83184, #87571, .T. ) ;
#42886 = ORIENTED_EDGE ( 'NONE', *, *, #102744, .T. ) ;
#42887 = EDGE_LOOP ( 'NONE', ( #8880, #56253, #73446, #87895, #100511, #104051, #56096, #68860, #14149 ) ) ;
#42888 = CARTESIAN_POINT ( 'NONE',  ( 38.19004552306619615, 25.28097608663575357, -13.30190894607149055 ) ) ;
#42889 = CARTESIAN_POINT ( 'NONE',  ( 71.47040382032911054, -57.67974827251811831, 166.7399757312242912 ) ) ;
#42891 = DIRECTION ( 'NONE',  ( 0.000000000000000000, 0.000000000000000000, 1.000000000000000000 ) ) ;
#42890 = CARTESIAN_POINT ( 'NONE',  ( -14.61305944212192109, 1.672740767017481422, -3.460733717101187157 ) ) ;
#42892 = ORIENTED_EDGE ( 'NONE', *, *, #71019, .F. ) ;
#42893 = EDGE_CURVE ( 'NONE', #95128, #53428, #54813, .T. ) ;
#42894 = AXIS2_PLACEMENT_3D ( 'NONE', #3309, #85288, #91794 ) ;
#42895 = EDGE_CURVE ( 'NONE', #95250, #55983, #64467, .T. ) ;
#42896 = CARTESIAN_POINT ( 'NONE',  ( 56.46206238374516317, -36.80706823966558972, -34.96395283256453723 ) ) ;
#42897 =( NAMED_UNIT ( * ) SI_UNIT ( $, .STERADIAN. ) SOLID_ANGLE_UNIT ( ) );
#42898 = CARTESIAN_POINT ( 'NONE',  ( -43.03880698781986780, 435.3545807224046484, 16.83573131045131177 ) ) ;
#42899 = CARTESIAN_POINT ( 'NONE',  ( -47.26640296552387355, -60.00000000000000711, 65.37368657561523833 ) ) ;
#42900 = CARTESIAN_POINT ( 'NONE',  ( 2.449293598294720219E-16, 195.0000000000000000, -2.000000000000011102 ) ) ;
#42901 = VECTOR ( 'NONE', #54725, 1000.000000000000000 ) ;
#42902 = EDGE_CURVE ( 'NONE', #57955, #37002, #68640, .T. ) ;
#42903 = CARTESIAN_POINT ( 'NONE',  ( -86.32370589824974161, -31.86242971515645905, 185.2303844998847637 ) ) ;
#42904 = ORIENTED_EDGE ( 'NONE', *, *, #91324, .T. ) ;
#42905 = CARTESIAN_POINT ( 'NONE',  ( 30.87886018709244240, 13.47971040000132525, 41.23243855231577015 ) ) ;
#42906 = CARTESIAN_POINT ( 'NONE',  ( -4.981455796065745290, -22.06768210089109772, 27.55828346185036892 ) ) ;
#42907 = EDGE_CURVE ( 'NONE', #102908, #94469, #100154, .T. ) ;
#42908 = EDGE_CURVE ( 'NONE', #36732, #88025, #8381, .T. ) ;
#42909 = CARTESIAN_POINT ( 'NONE',  ( -6.690415133250795954, 41.73276121203647904, -59.04972748448755482 ) ) ;
#42910 = CARTESIAN_POINT ( 'NONE',  ( -37.49021801792793696, 468.5024337580119891, 18.51843040749166036 ) ) ;
#42912 = CARTESIAN_POINT ( 'NONE',  ( 4.551278563468414085, -67.07315913433207299, 13.74478386570468658 ) ) ;
#42911 = CARTESIAN_POINT ( 'NONE',  ( -42.77015032893616109, 384.6486852084936459, 19.22311796600492428 ) ) ;
#42913 = EDGE_LOOP ( 'NONE', ( #78833, #98637, #65489, #45636 ) ) ;
#42914 = CARTESIAN_POINT ( 'NONE',  ( -33.19749974117156910, 318.2248943830853705, -6.522189075947168568 ) ) ;
#42915 = AXIS2_PLACEMENT_3D ( 'NONE', #34820, #50410, #83322 ) ;
#42916 = CARTESIAN_POINT ( 'NONE',  ( 0.3345852822193742804, 28.19046229938386006, 38.29267374853493777 ) ) ;
#42917 = CARTESIAN_POINT ( 'NONE',  ( 8.099999999999999645, 0.000000000000000000, 0.000000000000000000 ) ) ;
#42918 = CARTESIAN_POINT ( 'NONE',  ( 24.04676408874582094, 303.6130512030635487, -9.836050131052919809 ) ) ;
#42919 = CARTESIAN_POINT ( 'NONE',  ( 34.72474116627837759, 338.3618661353910966, -1.881472242819908436 ) ) ;
#42920 = CLOSED_SHELL ( 'NONE', ( #19950, #74164, #87845, #32759, #69298, #93386, #57848, #93490, #78669, #69395, #30161, #27337, #38431, #27914, #33066, #47135, #65288, #25798, #27116, #77737, #96508, #40818, #70975, #4960, #11158, #76291, #23190, #6345, #34024, #23817, #47680, #32934, #105888, #51070, #70542, #21210, #39919, #83037, #19730, #12828, #2228, #67722, #85386, #62766, #76505, #106687, #30614, #72666, #41554, #45074, #46730, #12512, #75713, #100252, #68552, #62444, #59337, #69099, #101920, #96260, #33641, #27260, #52538, #24876, #100763, #7550, #68281, #101388, #87591, #50189, #94497, #75757, #68626, #57542, #23751, #53283, #54693, #85465, #16884, #73129, #19013, #102995, #64682, #51131, #65343, #42818, #44467 ) ) ;
#42921 = CARTESIAN_POINT ( 'NONE',  ( 0.000000000000000000, 0.000000000000000000, 0.000000000000000000 ) ) ;
#42922 = DIRECTION ( 'NONE',  ( -1.000000000000000000, 0.000000000000000000, 0.000000000000000000 ) ) ;
#42923 = CARTESIAN_POINT ( 'NONE',  ( 109.5128197388708031, -29.99999999999998934, 168.1051457340969932 ) ) ;
#42924 = CARTESIAN_POINT ( 'NONE',  ( -78.52498540956069917, -60.31789553525856462, 160.5482536355575860 ) ) ;
#42925 = VERTEX_POINT ( 'NONE', #7844 ) ;
#42926 = CARTESIAN_POINT ( 'NONE',  ( 0.000000000000000000, 0.000000000000000000, 0.000000000000000000 ) ) ;
#42927 = CARTESIAN_POINT ( 'NONE',  ( 5.476751506168977102, 253.1635712286698947, -2.461144630687876145 ) ) ;
#42928 = FILL_AREA_STYLE ('',( #1373 ) ) ;
#42929 = DIRECTION ( 'NONE',  ( 0.000000000000000000, 0.000000000000000000, 1.000000000000000000 ) ) ;
#42930 = CARTESIAN_POINT ( 'NONE',  ( 45.39396809536891197, 371.0197163396430255, 6.150425833335645187 ) ) ;
#42931 = AXIS2_PLACEMENT_3D ( 'NONE', #45429, #88003, #103126 ) ;
#42932 = CARTESIAN_POINT ( 'NONE',  ( 7.500000000000005329, -3.000000000000000888, -52.94236561372726868 ) ) ;
#42933 = ORIENTED_EDGE ( 'NONE', *, *, #28052, .F. ) ;
#42934 = UNCERTAINTY_MEASURE_WITH_UNIT (LENGTH_MEASURE( 1.000000000000000082E-05 ), #59490, 'distance_accuracy_value', 'NONE');
#42935 = CARTESIAN_POINT ( 'NONE',  ( -3.313708498984688333, -21.96874999999999289, 8.000000000000074607 ) ) ;
#42936 = ORIENTED_EDGE ( 'NONE', *, *, #74493, .T. ) ;
#42938 = FACE_OUTER_BOUND ( 'NONE', #85514, .T. ) ;
#42937 =( BOUNDED_CURVE ( )  B_SPLINE_CURVE ( 2, ( #19925, #36629, #46801 ),
 .UNSPECIFIED., .F., .F. ) 
 B_SPLINE_CURVE_WITH_KNOTS ( ( 3, 3 ),
 ( 0.000000000000000000, 1.000000000000000000 ),
 .UNSPECIFIED. ) 
 CURVE ( )  GEOMETRIC_REPRESENTATION_ITEM ( )  RATIONAL_B_SPLINE_CURVE ( ( 1.000000000000000000, 1.857142857142858317, 1.000000000000000000 ) ) 
 REPRESENTATION_ITEM ( '' )  );
#42939 = CARTESIAN_POINT ( 'NONE',  ( 38.09999999999998721, 0.000000000000000000, 0.000000000000000000 ) ) ;
#42940 = CARTESIAN_POINT ( 'NONE',  ( 103.5111111111111057, -4.171999999999998820, 0.000000000000000000 ) ) ;
#42941 = CARTESIAN_POINT ( 'NONE',  ( -5.393385909618478635, 41.67668960927788646, -58.73074311017365545 ) ) ;
#42942 = DIRECTION ( 'NONE',  ( -1.000000000000000000, -1.224606353822377258E-16, -0.000000000000000000 ) ) ;
#42943 = CARTESIAN_POINT ( 'NONE',  ( 36.48461538461538822, 1.411358822780289120E-15, 0.000000000000000000 ) ) ;
#42944 = ORIENTED_EDGE ( 'NONE', *, *, #45812, .T. ) ;
#42945 = CARTESIAN_POINT ( 'NONE',  ( 107.2890547746881822, -60.00000000000001421, 124.3984078847621788 ) ) ;
#42947 = CARTESIAN_POINT ( 'NONE',  ( 21.23040246788248808, -35.99409632868995601, 30.53834131912143945 ) ) ;
#42946 = CARTESIAN_POINT ( 'NONE',  ( -78.68906450541477682, -14.21045842199436926, 170.0145061391070271 ) ) ;
#42948 =( GEOMETRIC_REPRESENTATION_CONTEXT ( 3 ) GLOBAL_UNCERTAINTY_ASSIGNED_CONTEXT ( ( #14010 ) ) GLOBAL_UNIT_ASSIGNED_CONTEXT ( ( #80653, #31614, #38640 ) ) REPRESENTATION_CONTEXT ( 'NONE', 'WORKASPACE' ) );
#42949 = CYLINDRICAL_SURFACE ( 'NONE', #4228, 4.000000000000000000 ) ;
#42950 = DIRECTION ( 'NONE',  ( -0.000000000000000000, 0.5000000000000018874, 0.8660254037844375974 ) ) ;
#42951 = EDGE_CURVE ( 'NONE', #12254, #88009, #56371, .T. ) ;
#42952 = CARTESIAN_POINT ( 'NONE',  ( -42.93444061617797303, -36.07314741104291045, 40.55327348855406910 ) ) ;
#42953 = CARTESIAN_POINT ( 'NONE',  ( -27.57459505077822470, 18.64284798593290660, -26.76870628202681246 ) ) ;
#42954 = UNCERTAINTY_MEASURE_WITH_UNIT (LENGTH_MEASURE( 1.000000000000000082E-05 ), #82482, 'distance_accuracy_value', 'NONE');
#42955 = ORIENTED_EDGE ( 'NONE', *, *, #3608, .T. ) ;
#42956 = CARTESIAN_POINT ( 'NONE',  ( -1.544427540536530316E-15, -4.285714285714290916, 25.22241582816893057 ) ) ;
#42957 = CARTESIAN_POINT ( 'NONE',  ( 7.465939481983455472, 54.30095352640775275, 2.152531556884869524 ) ) ;
#42958 = CARTESIAN_POINT ( 'NONE',  ( 7.149999999999997691, 41.65000000000000568, -59.82695526683420439 ) ) ;
#42959 = AXIS2_PLACEMENT_3D ( 'NONE', #92431, #44980, #3975 ) ;
#42960 = DIRECTION ( 'NONE',  ( -1.000000000000000000, 0.000000000000000000, 0.000000000000000000 ) ) ;
#42961 = LINE ( 'NONE', #75853, #37948 ) ;
#42962 = CARTESIAN_POINT ( 'NONE',  ( -30.00000000000004263, 488.6881500922590931, 8.886576284446979557 ) ) ;
#42963 = ORIENTED_EDGE ( 'NONE', *, *, #66206, .F. ) ;
#42964 = CARTESIAN_POINT ( 'NONE',  ( -16.75187969033554936, 36.38380281757302015, -24.30698433968596106 ) ) ;
#42965 = EDGE_LOOP ( 'NONE', ( #92341, #18318, #68411, #37926, #14712, #104019 ) ) ;
#42966 = CARTESIAN_POINT ( 'NONE',  ( 80.79101083364855640, -30.00000000000003553, 8.603092420626881065 ) ) ;
#42967 = CARTESIAN_POINT ( 'NONE',  ( 27.61861779010158457, 41.31838093711942150, -69.45717397145128302 ) ) ;
#42968 = UNCERTAINTY_MEASURE_WITH_UNIT (LENGTH_MEASURE( 1.000000000000000082E-05 ), #6246, 'distance_accuracy_value', 'NONE');
#42969 = CARTESIAN_POINT ( 'NONE',  ( 15.11650669486618881, 1.474610560812782335E-15, 0.000000000000000000 ) ) ;
#42970 = CARTESIAN_POINT ( 'NONE',  ( 1.249999999999999556, 7.938566201357357244, -7.198902722707429369 ) ) ;
#42971 = CARTESIAN_POINT ( 'NONE',  ( 83.28443596042880870, -29.99999999999998934, 45.16978209542076428 ) ) ;
#42972 = EDGE_CURVE ( 'NONE', #88975, #53736, #73092, .T. ) ;
#42973 = CARTESIAN_POINT ( 'NONE',  ( -30.93853997290534252, 332.3618051370746116, 16.87088913439686166 ) ) ;
#42974 = ORIENTED_EDGE ( 'NONE', *, *, #94585, .T. ) ;
#42975 = CONICAL_SURFACE ( 'NONE', #6776, 4.172000000000001485, 0.9599310885968750373 ) ;
#42976 = ORIENTED_EDGE ( 'NONE', *, *, #97411, .F. ) ;
#42977 = ORIENTED_EDGE ( 'NONE', *, *, #59285, .T. ) ;
#42979 = COLOUR_RGB ( '', 0.66274510, 0.83137255, 0.94901961) ;
#42978 = CARTESIAN_POINT ( 'NONE',  ( -46.83715889037884494, 13.71037705486507363, -15.21858309684217936 ) ) ;
#42980 = CARTESIAN_POINT ( 'NONE',  ( 0.000000000000000000, 0.000000000000000000, -11.12471428571428689 ) ) ;
#42981 = CARTESIAN_POINT ( 'NONE',  ( -36.49061380186538628, 25.91753039342102127, -12.86327411670220222 ) ) ;
#42982 = CARTESIAN_POINT ( 'NONE',  ( 41.93118512340635107, 437.4679042107824785, 21.45618714866054688 ) ) ;
#42983 = CARTESIAN_POINT ( 'NONE',  ( -32.19453080399548384, 398.3975244587722386, 25.63225119969380472 ) ) ;
#42984 = PRESENTATION_STYLE_ASSIGNMENT (( #6475 ) ) ;
#42985 = ORIENTED_EDGE ( 'NONE', *, *, #510, .F. ) ;
#42986 = CARTESIAN_POINT ( 'NONE',  ( -9.596002107494335576, 50.00000000000000000, -77.62543935900903591 ) ) ;
#42987 = ORIENTED_EDGE ( 'NONE', *, *, #106389, .T. ) ;
#42988 = CARTESIAN_POINT ( 'NONE',  ( 33.00795325653179901, 439.3958174160654266, 23.82489859418954836 ) ) ;
#42989 = CARTESIAN_POINT ( 'NONE',  ( 75.60688728915584988, -38.35697057576400937, 175.1550484948807593 ) ) ;
#42990 = CARTESIAN_POINT ( 'NONE',  ( 92.82022815836235452, -5.000000000000000000, 0.000000000000000000 ) ) ;
#42991 = CARTESIAN_POINT ( 'NONE',  ( 32.90571795128548871, 300.4295626401157620, 3.192642666177045285 ) ) ;
#42992 = AXIS2_PLACEMENT_3D ( 'NONE', #88581, #8183, #73437 ) ;
#42993 = ADVANCED_FACE ( 'NONE', ( #106542 ), #13549, .T. ) ;
#42994 = CARTESIAN_POINT ( 'NONE',  ( -5.980543423763066357, 246.0290359249892163, -0.5500789318242816917 ) ) ;
#42995 = ORIENTED_EDGE ( 'NONE', *, *, #50182, .T. ) ;
#42996 = CARTESIAN_POINT ( 'NONE',  ( 17.27438113373175455, 45.65101552804005536, -4.281429632575810551 ) ) ;
#42997 = DIRECTION ( 'NONE',  ( -0.000000000000000000, 1.000000000000000000, 0.000000000000000000 ) ) ;
#42998 = CARTESIAN_POINT ( 'NONE',  ( 48.02835407290544367, 11.61227450977237829, 14.35535821593427386 ) ) ;
#42999 = CARTESIAN_POINT ( 'NONE',  ( 15.51358515996928489, 2.608314655050632425, 0.4154586159794320666 ) ) ;
#43000 = EDGE_LOOP ( 'NONE', ( #84300, #98906, #35090, #68861, #76006, #93486 ) ) ;
#43001 = AXIS2_PLACEMENT_3D ( 'NONE', #91173, #41005, #16728 ) ;
#43002 = DIRECTION ( 'NONE',  ( -1.000000000000000000, -0.000000000000000000, -0.000000000000000000 ) ) ;
#43003 = UNCERTAINTY_MEASURE_WITH_UNIT (LENGTH_MEASURE( 1.000000000000000082E-05 ), #26301, 'distance_accuracy_value', 'NONE');
#43004 = DIRECTION ( 'NONE',  ( -1.000000000000000000, -0.000000000000000000, -0.000000000000000000 ) ) ;
#43005 = CARTESIAN_POINT ( 'NONE',  ( 8.000000000000000000, -10.99999999999999289, 0.000000000000000000 ) ) ;
#43006 = CARTESIAN_POINT ( 'NONE',  ( 0.9627154012949672435, 294.8487549602114086, 9.936351565176062550 ) ) ;
#43007 = PLANE ( 'NONE',  #104675 ) ;
#43008 = AXIS2_PLACEMENT_3D ( 'NONE', #63396, #54192, #39646 ) ;
#43009 = PRODUCT_DEFINITION ( 'UNKNOWN', '', #59420, #6848 ) ;
#43010 = CARTESIAN_POINT ( 'NONE',  ( 31.36650669486618881, -3.999999999999998224, 0.000000000000000000 ) ) ;
#43011 = CARTESIAN_POINT ( 'NONE',  ( 86.02951077547139391, -28.36966621159877278, 182.1157798530540504 ) ) ;
#43012 = CARTESIAN_POINT ( 'NONE',  ( 16.91846161659815806, 36.35180932965545253, -24.29864124313492013 ) ) ;
#43013 = AXIS2_PLACEMENT_3D ( 'NONE', #94870, #87831, #64096 ) ;
#43014 = CARTESIAN_POINT ( 'NONE',  ( -7.939583658500668939, 97.05573068118653168, 5.000000000002541078 ) ) ;
#43015 = EDGE_LOOP ( 'NONE', ( #78706, #44162, #1116 ) ) ;
#43016 = DIRECTION ( 'NONE',  ( 0.000000000000000000, 0.000000000000000000, 1.000000000000000000 ) ) ;
#43017 = CYLINDRICAL_SURFACE ( 'NONE', #21226, 4.000000000000000888 ) ;
#43018 = CARTESIAN_POINT ( 'NONE',  ( 33.09999999999999432, 1.533819458162526451E-15, 0.000000000000000000 ) ) ;
#43019 = CARTESIAN_POINT ( 'NONE',  ( -90.04170925992697505, -29.99999999999999645, 88.73563477756640339 ) ) ;
#43020 = SURFACE_STYLE_USAGE ( .BOTH. , #27414 ) ;
#43021 = CARTESIAN_POINT ( 'NONE',  ( 21.98976603507215088, 28.09591002020466988, -31.66807300705254491 ) ) ;
#43022 = DIRECTION ( 'NONE',  ( 1.000000000000000000, 0.000000000000000000, 0.000000000000000000 ) ) ;
#43023 = CIRCLE ( 'NONE', #101534, 5.000000000000010658 ) ;
#43025 = CARTESIAN_POINT ( 'NONE',  ( 0.3157512944461042803, -3.097794232780332724, -8.000000000000001776 ) ) ;
#43024 = FACE_OUTER_BOUND ( 'NONE', #3936, .T. ) ;
#43026 = EDGE_CURVE ( 'NONE', #96644, #26726, #24602, .T. ) ;
#43027 = CARTESIAN_POINT ( 'NONE',  ( 3.644838609763359827, -53.10562036962778620, 40.51873384035687309 ) ) ;
#43028 = CARTESIAN_POINT ( 'NONE',  ( -7.716871247394699651, -19.87863916820204224, 27.19415443154595025 ) ) ;
#43029 = CARTESIAN_POINT ( 'NONE',  ( -35.48628994100880618, 491.6413678155955722, 12.45547902532470275 ) ) ;
#43030 = CARTESIAN_POINT ( 'NONE',  ( 4.815811321232738251, -83.19923292302624418, 3.581116321197038044 ) ) ;
#43031 = CARTESIAN_POINT ( 'NONE',  ( -59.77583462350965959, -37.36469198411606385, -25.82931845235342294 ) ) ;
#43032 = CARTESIAN_POINT ( 'NONE',  ( 0.01372220897662087928, -5.948365447239591042, -2.697128823393874164 ) ) ;
#43033 = CARTESIAN_POINT ( 'NONE',  ( 62.51601690671169820, -29.54383159792558189, -24.06554947217484752 ) ) ;
#43034 = B_SPLINE_CURVE_WITH_KNOTS ( 'NONE', 3,
 ( #98907, #69242, #29336, #44968, #94587, #102115, #77318, #2350, #3963, #61142, #94031, #95109 ),
 .UNSPECIFIED., .F., .F.,
 ( 4, 2, 2, 2, 2, 4 ),
 ( 0.000000000000000000, 0.0009583675032029950139, 0.001916735006405990028, 0.003833470012811976586, 0.005750205019217962711, 0.007666940025623949703 ),
 .UNSPECIFIED. ) ;
#43035 = CARTESIAN_POINT ( 'NONE',  ( -23.24060281120672755, -25.55958343567869306, 29.06070736075156447 ) ) ;
#43036 = ORIENTED_EDGE ( 'NONE', *, *, #102153, .F. ) ;
#43037 = DIRECTION ( 'NONE',  ( -1.000000000000000000, 0.000000000000000000, 0.000000000000000000 ) ) ;
#43038 = CARTESIAN_POINT ( 'NONE',  ( -9.999945253488242258, 108.9998631337053467, -0.2662901834230876896 ) ) ;
#43039 = CARTESIAN_POINT ( 'NONE',  ( -10.00000000000000178, -15.00000000000000000, -9.999999999999998224 ) ) ;
#43040 = EDGE_CURVE ( 'NONE', #38295, #170, #63552, .T. ) ;
#43041 = CARTESIAN_POINT ( 'NONE',  ( -67.84377369674911051, -29.91451005171677124, -21.79787842944304188 ) ) ;
#43042 = EDGE_CURVE ( 'NONE', #28854, #60867, #104883, .T. ) ;
#43044 = CARTESIAN_POINT ( 'NONE',  ( -70.85373708857285635, -60.22816841820291245, -26.05913268935715621 ) ) ;
#43043 = CARTESIAN_POINT ( 'NONE',  ( -0.8412040808739075226, 27.41052785484215448, 40.42819026091922296 ) ) ;
#43045 = ORIENTED_EDGE ( 'NONE', *, *, #41150, .T. ) ;
#43046 = PRESENTATION_LAYER_ASSIGNMENT (  '', '', ( #12082 ) ) ;
#43047 = DIRECTION ( 'NONE',  ( -1.000000000000000000, -1.224606353822377258E-16, -0.000000000000000000 ) ) ;
#43048 = ORIENTED_EDGE ( 'NONE', *, *, #97623, .F. ) ;
#43049 = DIRECTION ( 'NONE',  ( 0.000000000000000000, 0.000000000000000000, 1.000000000000000000 ) ) ;
#43050 = VECTOR ( 'NONE', #32293, 1000.000000000000227 ) ;
#43051 = CARTESIAN_POINT ( 'NONE',  ( 15.50133110405595183, 2.625676835717284607, 0.7746791666779427876 ) ) ;
#43052 = FACE_BOUND ( 'NONE', #69935, .T. ) ;
#43053 = ORIENTED_EDGE ( 'NONE', *, *, #43290, .T. ) ;
#43054 = CARTESIAN_POINT ( 'NONE',  ( 51.01037695545453232, 500.0000000000002274, 0.000000000000000000 ) ) ;
#43055 = CARTESIAN_POINT ( 'NONE',  ( -7.500000000000006217, 152.0000000000000000, -5.000000000000000000 ) ) ;
#43056 = CARTESIAN_POINT ( 'NONE',  ( 99.29975701822439760, -37.82025374434009279, 191.5887330688091197 ) ) ;
#43057 = EDGE_CURVE ( 'NONE', #104952, #93305, #18768, .T. ) ;
#43059 = CARTESIAN_POINT ( 'NONE',  ( -7.344133061198930612, -7.555056073194249322, 3.176267128233874804 ) ) ;
#43058 = CARTESIAN_POINT ( 'NONE',  ( 3.156890235121763588, -18.90203136034843823, 27.03526591455209882 ) ) ;
#43060 = MECHANICAL_DESIGN_GEOMETRIC_PRESENTATION_REPRESENTATION (  '', ( #24151 ), #79002 ) ;
#43061 = EDGE_LOOP ( 'NONE', ( #22195, #26828, #90214, #38105 ) ) ;
#43062 = ORIENTED_EDGE ( 'NONE', *, *, #86941, .F. ) ;
#43063 = ORIENTED_EDGE ( 'NONE', *, *, #23903, .F. ) ;
#43064 = CARTESIAN_POINT ( 'NONE',  ( 30.47457020840358055, 336.9194354044551574, 16.65755050439408080 ) ) ;
#43065 = CARTESIAN_POINT ( 'NONE',  ( -5.656854249492379694, -28.43749999999999289, -5.656854249492380582 ) ) ;
#43066 = CARTESIAN_POINT ( 'NONE',  ( 9.803790402534414028, 53.40454157566192350, 2.927104633565267733 ) ) ;
#43067 = ORIENTED_EDGE ( 'NONE', *, *, #43375, .F. ) ;
#43068 = CARTESIAN_POINT ( 'NONE',  ( 0.000000000000000000, 0.000000000000000000, -11.12471428571428689 ) ) ;
#43069 = LINE ( 'NONE', #33941, #27287 ) ;
#43070 = CARTESIAN_POINT ( 'NONE',  ( -71.40526007946631637, -57.68007955256489083, 166.0300312729133623 ) ) ;
#43071 = VECTOR ( 'NONE', #104826, 1000.000000000000000 ) ;
#43072 = CARTESIAN_POINT ( 'NONE',  ( -30.48723010194668603, 12.91713162683278249, 41.81530375792740983 ) ) ;
#43073 = CARTESIAN_POINT ( 'NONE',  ( -35.59667163540026280, 463.9592197885497171, -0.04846191499040426731 ) ) ;
#43074 = DIRECTION ( 'NONE',  ( 0.000000000000000000, -1.000000000000000000, 0.000000000000000000 ) ) ;
#43075 = CARTESIAN_POINT ( 'NONE',  ( -94.21206122632280255, -59.99999999999995737, 9.571777650087724965 ) ) ;
#43076 = CARTESIAN_POINT ( 'NONE',  ( -7.807627842885899838, 51.84081132806975489, 3.792411731296619237 ) ) ;
#43077 = EDGE_CURVE ( 'NONE', #34348, #56853, #76304, .T. ) ;
#43078 = CARTESIAN_POINT ( 'NONE',  ( -49.98687195071457978, -49.90673118800283703, 54.21811667533064139 ) ) ;
#43079 = CARTESIAN_POINT ( 'NONE',  ( 8.000000000000000000, -27.40624999999999645, -3.313708498984761164 ) ) ;
#43080 = ORIENTED_EDGE ( 'NONE', *, *, #28023, .T. ) ;
#43081 = CARTESIAN_POINT ( 'NONE',  ( -95.75100734234322886, -52.81753470501251257, 195.4603346401156045 ) ) ;
#43082 = CARTESIAN_POINT ( 'NONE',  ( -5.645355559288413261, 301.6283892719433197, -10.01771515669004309 ) ) ;
#43083 = MECHANICAL_DESIGN_GEOMETRIC_PRESENTATION_REPRESENTATION (  '', ( #96454 ), #101752 ) ;
#43084 = CARTESIAN_POINT ( 'NONE',  ( 9.693539536716441418, -2.245191209186759185, 15.45402435566443700 ) ) ;
#43085 = ORIENTED_EDGE ( 'NONE', *, *, #28750, .F. ) ;
#43086 = CARTESIAN_POINT ( 'NONE',  ( 44.11327388758692081, 464.4313852428372797, 9.822198357557351045 ) ) ;
#43087 = CARTESIAN_POINT ( 'NONE',  ( 75.23893846245226769, -38.34369258312232631, 171.8379571195157496 ) ) ;
#43088 = CARTESIAN_POINT ( 'NONE',  ( 49.22356967707742115, 12.91018829712011140, 15.97913688295796852 ) ) ;
#43089 = DIRECTION ( 'NONE',  ( -1.000000000000000000, -1.224606353822377258E-16, -0.000000000000000000 ) ) ;
#43090 = CARTESIAN_POINT ( 'NONE',  ( -16.33234527380769663, 294.5674836605464293, 1.876698257015430027 ) ) ;
#43091 = FILL_AREA_STYLE ('',( #67371 ) ) ;
#43092 = CARTESIAN_POINT ( 'NONE',  ( 91.70700314268253805, -30.00000000000000355, 190.7673246573001506 ) ) ;
#43093 = DIRECTION ( 'NONE',  ( 1.000000000000000000, 0.000000000000000000, 0.000000000000000000 ) ) ;
#43094 = ADVANCED_FACE ( 'NONE', ( #93574 ), #15325, .F. ) ;
#43095 = CARTESIAN_POINT ( 'NONE',  ( -0.7856127335827165492, 37.10997504226060784, 27.51427648435862494 ) ) ;
#43096 = EDGE_LOOP ( 'NONE', ( #22555, #45144, #19367, #52430, #2501, #96829 ) ) ;
#43097 = VERTEX_POINT ( 'NONE', #18094 ) ;
#43098 = CARTESIAN_POINT ( 'NONE',  ( 50.93739997076023229, -53.36856766373855265, 57.23326497631002496 ) ) ;
#43099 = CARTESIAN_POINT ( 'NONE',  ( -46.00000000000000000, 437.8943772434384414, 13.39121328441609471 ) ) ;
#43100 = CIRCLE ( 'NONE', #58578, 4.250000000000000000 ) ;
#43101 = CYLINDRICAL_SURFACE ( 'NONE', #72012, 61.50000000000000000 ) ;
#43102 = EDGE_LOOP ( 'NONE', ( #50202, #49289, #49337, #63307, #55787 ) ) ;
#43103 = CARTESIAN_POINT ( 'NONE',  ( -85.85159476380036381, -38.36072881479658747, -22.04725531320800869 ) ) ;
#43104 = EDGE_LOOP ( 'NONE', ( #100068, #68128, #54284, #69224 ) ) ;
#43105 = CARTESIAN_POINT ( 'NONE',  ( 110.3745291010071128, -38.35605052085741562, 158.9613384561761222 ) ) ;
#43106 = CARTESIAN_POINT ( 'NONE',  ( 13.32459112348717589, 24.29133014533524104, -2.966397270190748614 ) ) ;
#43107 = CARTESIAN_POINT ( 'NONE',  ( 88.26228835492393898, -60.14943515912076322, 41.81636722779243343 ) ) ;
#43108 = DIRECTION ( 'NONE',  ( -1.000000000000000000, -0.000000000000000000, -0.000000000000000000 ) ) ;
#43109 = CARTESIAN_POINT ( 'NONE',  ( -26.59921953414089657, 305.9461108162179244, -9.538870392573779000 ) ) ;
#43110 = CARTESIAN_POINT ( 'NONE',  ( 1.688865360071264643, -5.975540627543329819, -13.79722992720151709 ) ) ;
#43111 = EDGE_CURVE ( 'NONE', #100497, #67401, #52031, .T. ) ;
#43112 = CARTESIAN_POINT ( 'NONE',  ( -23.38230688380519595, 25.22066353262445304, -33.19807408660797421 ) ) ;
#43113 = FACE_OUTER_BOUND ( 'NONE', #34336, .T. ) ;
#43114 = CARTESIAN_POINT ( 'NONE',  ( 3.646260779474320035, 129.8050105372081475, 5.000000000000000888 ) ) ;
#43115 = ORIENTED_EDGE ( 'NONE', *, *, #49507, .T. ) ;
#43116 = CARTESIAN_POINT ( 'NONE',  ( 59.29040008912359383, -60.33413133801057171, 80.30034514049579286 ) ) ;
#43117 = EDGE_CURVE ( 'NONE', #39006, #12821, #56581, .T. ) ;
#43118 = CARTESIAN_POINT ( 'NONE',  ( 0.4150645071567997668, 36.32396184902202663, 29.68202632210200065 ) ) ;
#43119 = AXIS2_PLACEMENT_3D ( 'NONE', #74763, #60226, #29327 ) ;
#43120 = CARTESIAN_POINT ( 'NONE',  ( 0.000000000000000000, 34.00000000000000000, 7.000000000000000000 ) ) ;
#43121 = ORIENTED_EDGE ( 'NONE', *, *, #18809, .F. ) ;
#43122 = CARTESIAN_POINT ( 'NONE',  ( -37.53250272162412671, 485.4507222580152757, -3.703678762838515048 ) ) ;
#43123 = CARTESIAN_POINT ( 'NONE',  ( -33.14071268597706421, 415.4777461792551208, 25.72715652696946620 ) ) ;
#43124 = DIRECTION ( 'NONE',  ( -1.000000000000000000, -1.224606353822377258E-16, -0.000000000000000000 ) ) ;
#43125 = DIRECTION ( 'NONE',  ( 0.000000000000000000, -1.000000000000000000, 0.000000000000000000 ) ) ;
#43126 = CARTESIAN_POINT ( 'NONE',  ( -8.000000000000000000, -29.74999999999999645, -9.797174393178825657E-16 ) ) ;
#43127 = CARTESIAN_POINT ( 'NONE',  ( 37.66449544891585788, -25.29918219771590415, 34.61108901143979466 ) ) ;
#43128 = CIRCLE ( 'NONE', #53450, 4.000000000000000888 ) ;
#43129 = DIRECTION ( 'NONE',  ( -0.4165977904505304696, -3.915074853572114378E-16, 0.9090909090909092827 ) ) ;
#43131 = ORIENTED_EDGE ( 'NONE', *, *, #2365, .F. ) ;
#43130 =( BOUNDED_SURFACE ( )  B_SPLINE_SURFACE ( 3, 2, ( 
 ( #58930, #59468, #50804 ),
 ( #83708, #9817, #42734 ),
 ( #75625, #1728, #67553 ),
 ( #95534, #44880, #12472 ) ),
 .UNSPECIFIED., .F., .F., .F. ) 
 B_SPLINE_SURFACE_WITH_KNOTS ( ( 4, 4 ),
 ( 3, 3 ),
 ( 0.01376892490370373347, 0.01435419950459405729 ),
 ( 0.1691075354860943070, 1.000000000000000000 ),
 .UNSPECIFIED. ) 
 GEOMETRIC_REPRESENTATION_ITEM ( )  RATIONAL_B_SPLINE_SURFACE ( (
 ( 0.9176910440068992703, 0.7566372315801705994, 1.000000000000000000),
 ( 0.9194425871098819147, 0.7618160164815883650, 1.000000000000000000),
 ( 0.9211696495200940582, 0.7669224193549075697, 1.000000000000000000),
 ( 0.9228729927664841570, 0.7719586918116432273, 1.000000000000000000) ) ) 
 REPRESENTATION_ITEM ( '' )  SURFACE ( )  );
#43132 = CARTESIAN_POINT ( 'NONE',  ( 83.88228782411839290, -42.97938930064833585, 181.2417429171390211 ) ) ;
#43133 = DIRECTION ( 'NONE',  ( 0.000000000000000000, -1.000000000000000000, 0.000000000000000000 ) ) ;
#43134 = ADVANCED_FACE ( 'NONE', ( #69306 ), #89415, .T. ) ;
#43135 = CYLINDRICAL_SURFACE ( 'NONE', #45254, 1.250000000000001110 ) ;
#43136 = ORIENTED_EDGE ( 'NONE', *, *, #66593, .F. ) ;
#43137 = CARTESIAN_POINT ( 'NONE',  ( -18.00000000000001776, -20.00000000000001776, -9.000000000000003553 ) ) ;
#43138 = EDGE_CURVE ( 'NONE', #33789, #49838, #59078, .T. ) ;
#43139 = CIRCLE ( 'NONE', #50045, 5.000000000000001776 ) ;
#43140 = DIRECTION ( 'NONE',  ( 0.000000000000000000, 0.000000000000000000, -1.000000000000000000 ) ) ;
#43141 =( NAMED_UNIT ( * ) SI_UNIT ( $, .STERADIAN. ) SOLID_ANGLE_UNIT ( ) );
#43142 = CARTESIAN_POINT ( 'NONE',  ( 13.73780227957887057, -3.000000000000002665, -78.37846873787221114 ) ) ;
#43143 = DIRECTION ( 'NONE',  ( -1.000000000000000000, -1.224606353822377258E-16, -0.000000000000000000 ) ) ;
#43144 = CARTESIAN_POINT ( 'NONE',  ( -17.45596745549606510, -24.91941539423173069, -38.51372130895111212 ) ) ;
#43145 = VECTOR ( 'NONE', #70303, 1000.000000000000000 ) ;
#43146 = AXIS2_PLACEMENT_3D ( 'NONE', #58131, #48959, #25826 ) ;
#43147 = CARTESIAN_POINT ( 'NONE',  ( 42.77053763280976284, -60.00000000000001421, 56.45409730004357840 ) ) ;
#43148 = CARTESIAN_POINT ( 'NONE',  ( 27.84859843015495073, -30.99258014239854830, 39.44613863972335821 ) ) ;
#43149 = LINE ( 'NONE', #76032, #22088 ) ;
#43150 = CARTESIAN_POINT ( 'NONE',  ( 22.35000867505471334, -18.10629870634155125, 31.47582638679958933 ) ) ;
#43152 = CARTESIAN_POINT ( 'NONE',  ( -12.93917161702704099, 23.58243205744838278, -4.610450678648994050 ) ) ;
#43151 = CARTESIAN_POINT ( 'NONE',  ( -30.59712220650429870, -32.84545843662240827, 40.92599255917917844 ) ) ;
#43153 = CIRCLE ( 'NONE', #51683, 4.000000000000007105 ) ;
#43154 = CARTESIAN_POINT ( 'NONE',  ( -9.989285784994814676, 88.97342427445701674, 0.5301777604595948601 ) ) ;
#43155 = CARTESIAN_POINT ( 'NONE',  ( 45.48126212248870814, 413.7349014071057240, 8.309231847991947362 ) ) ;
#43156 = CARTESIAN_POINT ( 'NONE',  ( 25.18061011279516137, 295.6585344082096185, -1.827081243610339634 ) ) ;
#43157 = CARTESIAN_POINT ( 'NONE',  ( 4.370066673350165409, -1.130272197109061239, 104.3945758574409695 ) ) ;
#43158 = ORIENTED_EDGE ( 'NONE', *, *, #2580, .T. ) ;
#43159 = DIRECTION ( 'NONE',  ( -0.000000000000000000, -0.000000000000000000, -1.000000000000000000 ) ) ;
#43160 = FACE_BOUND ( 'NONE', #86788, .T. ) ;
#43161 = DIRECTION ( 'NONE',  ( -1.000000000000000000, -0.000000000000000000, -0.000000000000000000 ) ) ;
#43162 = CARTESIAN_POINT ( 'NONE',  ( 100.6222222222222200, 1.023464760207051730E-14, 0.000000000000000000 ) ) ;
#43163 = EDGE_CURVE ( 'NONE', #80415, #37125, #3692, .T. ) ;
#43165 = CARTESIAN_POINT ( 'NONE',  ( 52.54835918530902461, -21.76994055301013375, -25.01027266287611539 ) ) ;
#43164 = CARTESIAN_POINT ( 'NONE',  ( 9.165151389911699198, 249.9999999999999432, 4.000000000000002665 ) ) ;
#43166 = VERTEX_POINT ( 'NONE', #100583 ) ;
#43167 = CARTESIAN_POINT ( 'NONE',  ( 27.10511071441198894, 36.88665068479745912, 7.556984339683237906 ) ) ;
#43168 = CARTESIAN_POINT ( 'NONE',  ( 0.000000000000000000, -30.00000000000000000, 0.000000000000000000 ) ) ;
#43169 = EDGE_LOOP ( 'NONE', ( #19485, #84576, #42851, #20987, #73115 ) ) ;
#43170 = VECTOR ( 'NONE', #79358, 1000.000000000000000 ) ;
#43171 = ADVANCED_FACE ( 'NONE', ( #43422 ), #102181, .T. ) ;
#43172 = CARTESIAN_POINT ( 'NONE',  ( 5.000000000000002665, 152.0000000000000000, 5.000000000000000000 ) ) ;
#43173 = CARTESIAN_POINT ( 'NONE',  ( 24.34999999999999787, 1.533819458162526451E-15, 0.000000000000000000 ) ) ;
#43174 = LINE ( 'NONE', #67976, #73493 ) ;
#43175 = CARTESIAN_POINT ( 'NONE',  ( -100.8861591709492984, -59.99999999999999289, 86.23238314539901239 ) ) ;
#43176 = LINE ( 'NONE', #58837, #87630 ) ;
#43177 = CARTESIAN_POINT ( 'NONE',  ( -16.14595037822608603, 7.274337365578172232, 6.616591826369962348 ) ) ;
#43178 = CARTESIAN_POINT ( 'NONE',  ( 28.21644434148578640, 308.7733337496239301, -9.112255642778062992 ) ) ;
#43179 = CARTESIAN_POINT ( 'NONE',  ( 38.83326880619124921, 459.9245326792457149, 1.954253696936976370 ) ) ;
#43180 = CARTESIAN_POINT ( 'NONE',  ( -34.02564419663974604, 436.1159546367792359, 7.420618519801049473 ) ) ;
#43181 = CARTESIAN_POINT ( 'NONE',  ( -83.79266685549821148, -35.97651932943645647, 171.8138913702506443 ) ) ;
#43182 = EDGE_LOOP ( 'NONE', ( #45733, #65861, #105927, #105840, #57941 ) ) ;
#43183 = EDGE_LOOP ( 'NONE', ( #87454, #60009, #75230 ) ) ;
#43184 = VERTEX_POINT ( 'NONE', #3496 ) ;
#43185 = DIRECTION ( 'NONE',  ( 0.000000000000000000, 1.000000000000000000, 0.000000000000000000 ) ) ;
#43186 = EDGE_CURVE ( 'NONE', #86888, #55752, #95015, .T. ) ;
#43187 = CARTESIAN_POINT ( 'NONE',  ( 2.920238372941035660E-16, -8.660254037844401509, -7.564338275809348033 ) ) ;
#43188 = EDGE_LOOP ( 'NONE', ( #38821, #62256 ) ) ;
#43189 = PRESENTATION_LAYER_ASSIGNMENT (  '', '', ( #48327 ) ) ;
#43190 = CARTESIAN_POINT ( 'NONE',  ( 32.28930913498017929, 488.2717154064768579, 9.213726894932253941 ) ) ;
#43191 = CARTESIAN_POINT ( 'NONE',  ( -6.928203230275508773, -85.00000000000000000, 4.000000000000001776 ) ) ;
#43192 = AXIS2_PLACEMENT_3D ( 'NONE', #40167, #88204, #49302 ) ;
#43193 = CARTESIAN_POINT ( 'NONE',  ( -2.448089827929017304, 14.67886088499936292, 6.561838588348337886 ) ) ;
#43194 = CARTESIAN_POINT ( 'NONE',  ( -0.6467460089013201685, 53.45139368308109340, 10.08288459130510439 ) ) ;
#43195 = DIRECTION ( 'NONE',  ( -1.000000000000000000, -1.224606353822377258E-16, -0.000000000000000000 ) ) ;
#43196 = CARTESIAN_POINT ( 'NONE',  ( 88.48689482502902592, 1.016364837396684119E-14, 0.000000000000000000 ) ) ;
#43197 = CARTESIAN_POINT ( 'NONE',  ( 98.75715858346298148, -14.21045842199428222, 105.0403869495405331 ) ) ;
#43198 = CARTESIAN_POINT ( 'NONE',  ( -77.87378252178784521, -14.21045842199420228, 157.7502635463301317 ) ) ;
#43199 = ADVANCED_FACE ( 'NONE', ( #2947 ), #23922, .F. ) ;
#43200 = CARTESIAN_POINT ( 'NONE',  ( -60.71664721387831776, -36.01558240415723589, 72.46505467556380609 ) ) ;
#43201 = ORIENTED_EDGE ( 'NONE', *, *, #40651, .F. ) ;
#43202 = DIRECTION ( 'NONE',  ( -0.000000000000000000, -0.000000000000000000, 1.000000000000000000 ) ) ;
#43203 = ORIENTED_EDGE ( 'NONE', *, *, #38615, .T. ) ;
#43204 = CARTESIAN_POINT ( 'NONE',  ( -103.7500182398446924, -60.16060988300274914, 191.4285943361837781 ) ) ;
#43205 =( NAMED_UNIT ( * ) SI_UNIT ( $, .STERADIAN. ) SOLID_ANGLE_UNIT ( ) );
#43206 = CARTESIAN_POINT ( 'NONE',  ( -30.04058829887638282, 13.07764605659131796, -42.05455409923744270 ) ) ;
#43207 = EDGE_CURVE ( 'NONE', #85705, #11400, #64060, .T. ) ;
#43208 = CARTESIAN_POINT ( 'NONE',  ( 14.33580415461469570, 42.00000000000010658, -89.41414988890622340 ) ) ;
#43209 = ORIENTED_EDGE ( 'NONE', *, *, #57003, .F. ) ;
#43210 = CARTESIAN_POINT ( 'NONE',  ( 9.432319653620828248, -4.999999999999999112, -70.68463330170209247 ) ) ;
#43212 = VECTOR ( 'NONE', #70233, 1000.000000000000000 ) ;
#43211 = CARTESIAN_POINT ( 'NONE',  ( -73.36908011962465537, -59.99999999999998579, 165.8270234517137567 ) ) ;
#43213 = CARTESIAN_POINT ( 'NONE',  ( 36.58606824315381800, 25.86842935218156825, -12.99751704779520267 ) ) ;
#43214 = CARTESIAN_POINT ( 'NONE',  ( 2.977408999572651815, -22.81250000204838813, 7.188101187500000933 ) ) ;
#43215 = CIRCLE ( 'NONE', #69098, 3.309500000000001663 ) ;
#43216 = CARTESIAN_POINT ( 'NONE',  ( -46.00000000000000000, 461.9428920847514632, 12.03309428281624172 ) ) ;
#43217 = FILL_AREA_STYLE ('',( #42139 ) ) ;
#43218 = CARTESIAN_POINT ( 'NONE',  ( 1.113195845631288261, -0.000000000000000000, -17.01584901092319058 ) ) ;
#43219 = CARTESIAN_POINT ( 'NONE',  ( 84.20870358801302302, -52.67313341312099340, -14.85892719433468123 ) ) ;
#43220 = CARTESIAN_POINT ( 'NONE',  ( 7.347880794884120722E-16, 299.9999999999999432, -6.000000000000000888 ) ) ;
#43221 = CARTESIAN_POINT ( 'NONE',  ( 6.598176363461978333, -7.008098997476053249, 13.88231573857982326 ) ) ;
#43222 = EDGE_CURVE ( 'NONE', #68944, #54096, #67010, .T. ) ;
#43223 = CARTESIAN_POINT ( 'NONE',  ( -15.70492864000498301, 46.17438344839472819, -4.577980962366806850 ) ) ;
#43224 = PRESENTATION_STYLE_ASSIGNMENT (( #10307 ) ) ;
#43225 = CARTESIAN_POINT ( 'NONE',  ( -31.24728166932320050, -56.85591377269362567, 36.70157539563093962 ) ) ;
#43226 = CIRCLE ( 'NONE', #82793, 9.000000000000000000 ) ;
#43227 = CARTESIAN_POINT ( 'NONE',  ( 3.191145750007355009, 20.31792217114059795, 6.242773338886944856 ) ) ;
#43228 = CARTESIAN_POINT ( 'NONE',  ( 44.43361187226474129, -22.24703502879481221, 38.44165449124453460 ) ) ;
#43229 = CARTESIAN_POINT ( 'NONE',  ( 68.70539558375507738, 4.898587196589294500E-16, -4.000000000000007105 ) ) ;
#43230 = MECHANICAL_DESIGN_GEOMETRIC_PRESENTATION_REPRESENTATION (  '', ( #19177 ), #39770 ) ;
#43231 = CARTESIAN_POINT ( 'NONE',  ( -0.5694748022185723846, 45.34960206111118453, 18.61592841094030604 ) ) ;
#43232 = AXIS2_PLACEMENT_3D ( 'NONE', #82524, #72820, #56089 ) ;
#43233 = CARTESIAN_POINT ( 'NONE',  ( -85.87617615289288153, -38.64955979039224587, 198.9927000956684537 ) ) ;
#43234 = ORIENTED_EDGE ( 'NONE', *, *, #16127, .T. ) ;
#43235 = CARTESIAN_POINT ( 'NONE',  ( 42.35645304355708163, 435.3801053262068308, 19.45913382674007508 ) ) ;
#43236 = CARTESIAN_POINT ( 'NONE',  ( 31.33832728500611609, -60.00000000000000711, 37.30313604653941439 ) ) ;
#43237 = CARTESIAN_POINT ( 'NONE',  ( 15.50007054317050681, 37.03005157377465650, 23.01145510268004912 ) ) ;
#43238 = CARTESIAN_POINT ( 'NONE',  ( -7.294238536526225225, 41.09454800505173466, -58.80184262229552417 ) ) ;
#43239 = CARTESIAN_POINT ( 'NONE',  ( 7.036764705882358584, 40.00000000373366049, -71.06385277390856459 ) ) ;
#43240 = CARTESIAN_POINT ( 'NONE',  ( 33.58349330513379982, 1.593028355512270567E-15, 0.000000000000000000 ) ) ;
#43241 = CARTESIAN_POINT ( 'NONE',  ( 43.33388476020373048, 464.9733321035772065, 13.99141793829583236 ) ) ;
#43242 = DIRECTION ( 'NONE',  ( 0.000000000000000000, 0.000000000000000000, -1.000000000000000000 ) ) ;
#43243 = CARTESIAN_POINT ( 'NONE',  ( 101.9353215183635939, -60.00000000000000000, 92.36758675646822780 ) ) ;
#43244 = B_SPLINE_CURVE_WITH_KNOTS ( 'NONE', 3,
 ( #14795, #5651, #62848, #64436, #63912, #73018 ),
 .UNSPECIFIED., .F., .F.,
 ( 4, 2, 4 ),
 ( 0.000000000000000000, 0.001670251840629987045, 0.003340503681259974090 ),
 .UNSPECIFIED. ) ;
#43245 = DIRECTION ( 'NONE',  ( 0.000000000000000000, 1.000000000000000000, 0.000000000000000000 ) ) ;
#43246 = CARTESIAN_POINT ( 'NONE',  ( -7.896571385775231100, -68.78997999345754977, 1.305932416347435954 ) ) ;
#43247 = EDGE_LOOP ( 'NONE', ( #101794, #76494, #74704, #34579, #91076 ) ) ;
#43248 = ADVANCED_FACE ( 'NONE', ( #28882 ), #22363, .T. ) ;
#43249 = CARTESIAN_POINT ( 'NONE',  ( 34.89857526195121551, 437.7187790665914235, 4.586527422594350867 ) ) ;
#43250 = DIRECTION ( 'NONE',  ( -1.000000000000000000, -0.000000000000000000, -0.000000000000000000 ) ) ;
#43251 = ORIENTED_EDGE ( 'NONE', *, *, #59625, .F. ) ;
#43252 = CARTESIAN_POINT ( 'NONE',  ( 26.48366646117538536, 37.08895952672338581, -7.710263864458167582 ) ) ;
#43253 = DIRECTION ( 'NONE',  ( -1.000000000000000000, -0.000000000000000000, -0.000000000000000000 ) ) ;
#43254 = CARTESIAN_POINT ( 'NONE',  ( 9.221249107921748234, 28.95178628501513529, 3.869340886054257300 ) ) ;
#43255 = CARTESIAN_POINT ( 'NONE',  ( 5.082755093536325930, -22.34375000204838457, -5.082755093536325042 ) ) ;
#43256 = AXIS2_PLACEMENT_3D ( 'NONE', #45607, #34873, #39641 ) ;
#43257 = EDGE_CURVE ( 'NONE', #77600, #65506, #36021, .T. ) ;
#43258 = CIRCLE ( 'NONE', #81117, 4.000000000000007105 ) ;
#43259 = CARTESIAN_POINT ( 'NONE',  ( 29.77121734509575290, 18.16596778899118902, -39.60535821593530414 ) ) ;
#43261 = VERTEX_POINT ( 'NONE', #70355 ) ;
#43260 = CARTESIAN_POINT ( 'NONE',  ( 0.000000000000000000, 0.000000000000000000, 0.000000000000000000 ) ) ;
#43262 = CARTESIAN_POINT ( 'NONE',  ( 82.61890608584070606, -39.49166873427294178, 166.2326186401752466 ) ) ;
#43263 = CARTESIAN_POINT ( 'NONE',  ( -3.801077171203083971, -1.110903940591794203, 104.1059035333591254 ) ) ;
#43264 = ORIENTED_EDGE ( 'NONE', *, *, #22220, .F. ) ;
#43265 = DIRECTION ( 'NONE',  ( -1.000000000000000000, -1.224606353822377258E-16, -0.000000000000000000 ) ) ;
#43266 = EDGE_CURVE ( 'NONE', #57728, #52946, #51435, .T. ) ;
#43267 = CARTESIAN_POINT ( 'NONE',  ( -47.55680477683402785, 16.06931990738296889, 16.76905664007686880 ) ) ;
#43268 = CARTESIAN_POINT ( 'NONE',  ( 37.88489815392355808, 27.77121267130071303, -10.98707414366107926 ) ) ;
#43269 = CARTESIAN_POINT ( 'NONE',  ( 87.04245038058458306, 1.016364837396684119E-14, 0.000000000000000000 ) ) ;
#43270 =( NAMED_UNIT ( * ) SI_UNIT ( $, .STERADIAN. ) SOLID_ANGLE_UNIT ( ) );
#43271 =( BOUNDED_SURFACE ( )  B_SPLINE_SURFACE ( 3, 2, ( 
 ( #20618, #93916, #11920 ),
 ( #28684, #95502, #20073 ),
 ( #37838, #12971, #86898 ),
 ( #28154, #29229, #94461 ),
 ( #62103, #21131, #38869 ),
 ( #61030, #45897, #62616 ),
 ( #46426, #86379, #12445 ),
 ( #63144, #70169, #102537 ),
 ( #85845, #22169, #45372 ),
 ( #21645, #5434, #78773 ),
 ( #52920, #54481, #70702 ),
 ( #87428, #96041, #13503 ),
 ( #46937, #94995, #103592 ),
 ( #79311, #44847, #77738 ) ),
 .UNSPECIFIED., .F., .F., .F. ) 
 B_SPLINE_SURFACE_WITH_KNOTS ( ( 4, 2, 2, 2, 2, 2, 4 ),
 ( 3, 3 ),
 ( -3.556183125752454544E-17, 0.003030258808122785353, 0.004545388212184195594, 0.006060517616245606268, 0.007575647020307016942, 0.009090776424368427616, 0.01212103523249124723 ),
 ( 0.000000000000000000, 1.000000000000000000 ),
 .UNSPECIFIED. ) 
 GEOMETRIC_REPRESENTATION_ITEM ( )  RATIONAL_B_SPLINE_SURFACE ( (
 ( 1.000000000000000000, 0.7246213771202291154, 1.000000000000000000),
 ( 1.000000000000000000, 0.7389031614989468588, 1.000000000000000000),
 ( 1.000000000000000000, 0.7528478292017520834, 1.000000000000000000),
 ( 1.000000000000000000, 0.7735487450444836766, 1.000000000000000000),
 ( 1.000000000000000000, 0.7804537612899002941, 1.000000000000000000),
 ( 1.000000000000000000, 0.7939987057269957127, 1.000000000000000000),
 ( 1.000000000000000000, 0.8006397256199081491, 1.000000000000000000),
 ( 1.000000000000000000, 0.8137168943989200320, 1.000000000000000000),
 ( 1.000000000000000000, 0.8201529051482028265, 1.000000000000000000),
 ( 1.000000000000000000, 0.8328685173623544546, 1.000000000000000000),
 ( 1.000000000000000000, 0.8391819167394514167, 1.000000000000000000),
 ( 1.000000000000000000, 0.8576788219182877038, 1.000000000000000000),
 ( 1.000000000000000000, 0.8693707786496762679, 1.000000000000000000),
 ( 1.000000000000000000, 0.8805984182416946027, 1.000000000000000000) ) ) 
 REPRESENTATION_ITEM ( '' )  SURFACE ( )  );
#43272 = CARTESIAN_POINT ( 'NONE',  ( -33.10942428023948025, 427.0948870615109172, 25.12333264783021036 ) ) ;
#43273 = ORIENTED_EDGE ( 'NONE', *, *, #93544, .F. ) ;
#43274 = VECTOR ( 'NONE', #20878, 1000.000000000000000 ) ;
#43275 = DIRECTION ( 'NONE',  ( 0.000000000000000000, -1.000000000000000000, 0.000000000000000000 ) ) ;
#43276 = CARTESIAN_POINT ( 'NONE',  ( -1.000000000000000000, -63.35894816181920675, 9.450637109072113518 ) ) ;
#43277 = CARTESIAN_POINT ( 'NONE',  ( 14.29190075645216496, 21.26710225494213802, 5.626279437277409201 ) ) ;
#43278 = LINE ( 'NONE', #69683, #24164 ) ;
#43279 = CARTESIAN_POINT ( 'NONE',  ( -5.082755093536325042, -27.59375000204838457, -5.082755093536325930 ) ) ;
#43280 = CARTESIAN_POINT ( 'NONE',  ( 0.000000000000000000, 70.00000000000000000, 0.000000000000000000 ) ) ;
#43281 = CARTESIAN_POINT ( 'NONE',  ( 7.465531072436692561, 52.17264765254623171, 2.153407880170176814 ) ) ;
#43282 = CARTESIAN_POINT ( 'NONE',  ( 15.05785784214676326, 3.824195276769950969, 4.604276673498415740 ) ) ;
#43283 = ITEM_DEFINED_TRANSFORMATION ( 'NONE', 'NONE', #33552,  #10728 ) ;
#43284 = VERTEX_POINT ( 'NONE', #29913 ) ;
#43285 = CARTESIAN_POINT ( 'NONE',  ( 0.000000000000000000, 0.000000000000000000, 4.000000000000000000 ) ) ;
#43286 = DIRECTION ( 'NONE',  ( -0.5735764363510494901, -0.8191520442889894671, 0.000000000000000000 ) ) ;
#43287 = AXIS2_PLACEMENT_3D ( 'NONE', #47081, #63295, #38498 ) ;
#43288 = CARTESIAN_POINT ( 'NONE',  ( -10.54230344465946345, 6.725510416460146246, 0.000000000000000000 ) ) ;
#43289 = CARTESIAN_POINT ( 'NONE',  ( 0.000000000000000000, 4.898587196589412829E-16, -4.000000000000000000 ) ) ;
#43290 = EDGE_CURVE ( 'NONE', #21895, #89487, #20369, .T. ) ;
#43291 = ORIENTED_EDGE ( 'NONE', *, *, #94079, .T. ) ;
#43292 = AXIS2_PLACEMENT_3D ( 'NONE', #53384, #11302, #86301 ) ;
#43293 = CARTESIAN_POINT ( 'NONE',  ( 35.97769024725786124, 482.2773069761253169, 15.66015945297581169 ) ) ;
#43294 = CARTESIAN_POINT ( 'NONE',  ( -4.852941176470593199, 42.83333333333328596, -70.80672828634229177 ) ) ;
#43295 = MECHANICAL_DESIGN_GEOMETRIC_PRESENTATION_REPRESENTATION (  '', ( #45016 ), #20950 ) ;
#43296 = ADVANCED_FACE ( 'NONE', ( #53628 ), #38533, .T. ) ;
#43298 = CARTESIAN_POINT ( 'NONE',  ( 33.16766815328914930, 434.2046602808906073, 15.25519444545857262 ) ) ;
#43297 = AXIS2_PLACEMENT_3D ( 'NONE', #45268, #45784, #61457 ) ;
#43299 = CARTESIAN_POINT ( 'NONE',  ( -1.248763605186368197, 10.99880023176083021, -50.36974636785474502 ) ) ;
#43300 = DIRECTION ( 'NONE',  ( 0.5735764363510554853, 0.8191520442889852482, 0.000000000000000000 ) ) ;
#43301 = DIRECTION ( 'NONE',  ( 0.000000000000000000, -1.000000000000000000, 0.000000000000000000 ) ) ;
#43302 = CARTESIAN_POINT ( 'NONE',  ( -77.02578345189107267, -59.99999999999998579, 190.5239158944286828 ) ) ;
#43303 = SURFACE_STYLE_USAGE ( .BOTH. , #27694 ) ;
#43304 = CYLINDRICAL_SURFACE ( 'NONE', #91451, 4.000000000000000000 ) ;
#43305 = DIRECTION ( 'NONE',  ( 0.000000000000000000, -1.000000000000000000, 0.000000000000000000 ) ) ;
#43306 = EDGE_CURVE ( 'NONE', #44463, #92310, #39592, .T. ) ;
#43307 = CARTESIAN_POINT ( 'NONE',  ( 6.400000000000000355, 0.000000000000000000, 0.000000000000000000 ) ) ;
#43308 = CARTESIAN_POINT ( 'NONE',  ( -86.40597577314841260, -17.76547941803659114, 175.7363829004051468 ) ) ;
#43309 = FACE_OUTER_BOUND ( 'NONE', #14714, .T. ) ;
#43310 = VERTEX_POINT ( 'NONE', #102719 ) ;
#43311 = CARTESIAN_POINT ( 'NONE',  ( -18.39955510352875834, 302.6496531622213979, 9.894388872991537909 ) ) ;
#43312 = EDGE_CURVE ( 'NONE', #98268, #68407, #96272, .T. ) ;
#43313 = CARTESIAN_POINT ( 'NONE',  ( 3.460324465711511088, -1.165480915309818011, 104.5902739981127212 ) ) ;
#43314 = CARTESIAN_POINT ( 'NONE',  ( -82.76973596104315334, -37.82754287118251568, 2.360074632004959927 ) ) ;
#43315 = CONICAL_SURFACE ( 'NONE', #82895, 5.000000000000001776, 0.9599310885968803664 ) ;
#43316 = SURFACE_STYLE_USAGE ( .BOTH. , #35794 ) ;
#43317 = CARTESIAN_POINT ( 'NONE',  ( -20.24579557674108088, 304.8297271373347144, -10.00469232190996927 ) ) ;
#43318 = ORIENTED_EDGE ( 'NONE', *, *, #4531, .F. ) ;
#43319 = DIRECTION ( 'NONE',  ( -1.000000000000000000, -1.224606353822377258E-16, -0.000000000000000000 ) ) ;
#43320 = CARTESIAN_POINT ( 'NONE',  ( 28.35655838125921946, 36.31484077510918951, -8.865061771931141976 ) ) ;
#43321 = CARTESIAN_POINT ( 'NONE',  ( -45.60838156036751201, 42.00000000000000000, -79.13121736029046360 ) ) ;
#43322 = CARTESIAN_POINT ( 'NONE',  ( -23.05268216894211974, 28.15323590773658680, 30.70617127781061839 ) ) ;
#43323 = CARTESIAN_POINT ( 'NONE',  ( 73.20681906048392307, -14.21045842199435150, 129.4971587772804185 ) ) ;
#43324 = CARTESIAN_POINT ( 'NONE',  ( 0.000000000000000000, 61.34242035161803841, -9.357204421225127078 ) ) ;
#43325 = CARTESIAN_POINT ( 'NONE',  ( -88.18129031808710749, -59.99999999999997158, -24.85705915495453411 ) ) ;
#43326 = CONICAL_SURFACE ( 'NONE', #103612, 3.309500000000001663, 0.9599310885968770357 ) ;
#43327 = CARTESIAN_POINT ( 'NONE',  ( -64.89877610984821388, -56.86748303091376044, 95.13561503513990658 ) ) ;
#43328 = ORIENTED_EDGE ( 'NONE', *, *, #59216, .T. ) ;
#43329 = CARTESIAN_POINT ( 'NONE',  ( 74.83543306973328413, -14.21045842199438347, 137.5190812362815791 ) ) ;
#43330 = CARTESIAN_POINT ( 'NONE',  ( -52.56483885390522914, 40.83906611473334891, -38.23529411764704378 ) ) ;
#43331 = CARTESIAN_POINT ( 'NONE',  ( 69.18913803857314804, -57.67117611319257975, -34.94735017757600559 ) ) ;
#43332 = ORIENTED_EDGE ( 'NONE', *, *, #59334, .F. ) ;
#43333 = CARTESIAN_POINT ( 'NONE',  ( 7.312789698585915765, 52.12765650109543714, -2.970840588490396783 ) ) ;
#43334 = CARTESIAN_POINT ( 'NONE',  ( -2.977408999572650039, -23.56250000204838813, -7.188101187500000933 ) ) ;
#43335 = CARTESIAN_POINT ( 'NONE',  ( -1.011124010007723006, 28.02085465524457675, -38.74700955856429374 ) ) ;
#43336 = ORIENTED_EDGE ( 'NONE', *, *, #98052, .T. ) ;
#43337 = DIRECTION ( 'NONE',  ( 0.000000000000000000, 0.000000000000000000, -1.000000000000000000 ) ) ;
#43338 = VERTEX_POINT ( 'NONE', #96755 ) ;
#43339 = CARTESIAN_POINT ( 'NONE',  ( -6.019162162301046060, 39.99999999999999289, -71.20548073448676973 ) ) ;
#43340 = CARTESIAN_POINT ( 'NONE',  ( 46.81357782755165431, 18.41089473351597761, -15.91307620878907869 ) ) ;
#43341 = CARTESIAN_POINT ( 'NONE',  ( -19.45294693897874794, -59.99999999999013767, 42.51175855280396831 ) ) ;
#43342 = CARTESIAN_POINT ( 'NONE',  ( 29.46624082845785253, 308.8359934246385592, -8.861758456725450372 ) ) ;
#43343 = CARTESIAN_POINT ( 'NONE',  ( -7.188101187500002709, -12.31250000204838635, 2.977408999572648707 ) ) ;
#43344 = CARTESIAN_POINT ( 'NONE',  ( -48.15175547875134754, 14.66334354488785507, 16.85535821593515138 ) ) ;
#43345 = DIRECTION ( 'NONE',  ( -1.000000000000000000, 0.000000000000000000, 0.000000000000000000 ) ) ;
#43346 = LINE ( 'NONE', #18559, #61617 ) ;
#43347 = CARTESIAN_POINT ( 'NONE',  ( -8.737863884121393809, 49.99999999999999289, -90.03618980231146907 ) ) ;
#43348 = DIRECTION ( 'NONE',  ( 1.000000000000000000, -0.000000000000000000, 1.224646799147353207E-16 ) ) ;
#43349 = CARTESIAN_POINT ( 'NONE',  ( 42.20041562234358423, 435.2369744135583574, 7.788607701745473122 ) ) ;
#43350 = UNCERTAINTY_MEASURE_WITH_UNIT (LENGTH_MEASURE( 1.000000000000000082E-05 ), #81759, 'distance_accuracy_value', 'NONE');
#43351 = ORIENTED_EDGE ( 'NONE', *, *, #24057, .T. ) ;
#43352 = SURFACE_STYLE_FILL_AREA ( #12034 ) ;
#43354 = CARTESIAN_POINT ( 'NONE',  ( 31.27512390054598157, -32.54638041113430802, 32.34197377954890840 ) ) ;
#43353 = CARTESIAN_POINT ( 'NONE',  ( -4.245164436743399605, -48.92819220080404108, 104.4592797835132245 ) ) ;
#43355 = CARTESIAN_POINT ( 'NONE',  ( 22.03900363279368690, -4.285714285714963268, -12.70248734011530622 ) ) ;
#43356 = EDGE_LOOP ( 'NONE', ( #94942, #10814, #15603, #98389 ) ) ;
#43357 = CARTESIAN_POINT ( 'NONE',  ( -21.99058289103490438, 25.96809656825333334, -31.66568596923509560 ) ) ;
#43358 = ORIENTED_EDGE ( 'NONE', *, *, #106628, .F. ) ;
#43360 = CARTESIAN_POINT ( 'NONE',  ( -1.098016817928066491, 43.84270387359042331, -16.88143485833182922 ) ) ;
#43359 = CARTESIAN_POINT ( 'NONE',  ( -26.10803651193542407, 35.05774228055371822, -8.035081906110033145 ) ) ;
#43361 = FACE_OUTER_BOUND ( 'NONE', #78426, .T. ) ;
#43362 = CARTESIAN_POINT ( 'NONE',  ( -21.51569398614867623, 294.9107018935607698, -9.987480606144499617 ) ) ;
#43363 = FACE_OUTER_BOUND ( 'NONE', #74968, .T. ) ;
#43364 = CARTESIAN_POINT ( 'NONE',  ( 0.000000000000000000, 17.85270131633358304, -10.00000000000000178 ) ) ;
#43365 = DIRECTION ( 'NONE',  ( 0.5735764363510440500, 0.8191520442889932418, 0.000000000000000000 ) ) ;
#43366 = EDGE_LOOP ( 'NONE', ( #51433, #72399 ) ) ;
#43367 = CARTESIAN_POINT ( 'NONE',  ( 90.09714635153191864, -59.99999999999999289, -18.66843320900434122 ) ) ;
#43368 = SURFACE_STYLE_FILL_AREA ( #84362 ) ;
#43369 = COLOUR_RGB ( '', 0.40784314, 0.44705882, 0.49803922) ;
#43370 = DIRECTION ( 'NONE',  ( -0.000000000000000000, 1.000000000000000000, -0.000000000000000000 ) ) ;
#43371 = DIRECTION ( 'NONE',  ( 0.000000000000000000, -1.000000000000000000, 0.000000000000000000 ) ) ;
#43372 = VECTOR ( 'NONE', #85865, 1000.000000000000000 ) ;
#43373 = LINE ( 'NONE', #35309, #99476 ) ;
#43374 = EDGE_LOOP ( 'NONE', ( #80450, #11968, #70529, #80420 ) ) ;
#43375 = EDGE_CURVE ( 'NONE', #5539, #57603, #17035, .T. ) ;
#43376 = EDGE_CURVE ( 'NONE', #14336, #55601, #27404, .T. ) ;
#43377 = CARTESIAN_POINT ( 'NONE',  ( -107.1906752169646353, -29.99999999999498357, 191.1798405353558792 ) ) ;
#43378 = ORIENTED_EDGE ( 'NONE', *, *, #31173, .T. ) ;
#43379 = ORIENTED_EDGE ( 'NONE', *, *, #71879, .T. ) ;
#43380 = DIRECTION ( 'NONE',  ( 0.000000000000000000, 0.000000000000000000, -1.000000000000000000 ) ) ;
#43381 = SURFACE_SIDE_STYLE ('',( #41775 ) ) ;
#43382 = CARTESIAN_POINT ( 'NONE',  ( -15.90862040200999949, 35.08000091432026579, -22.13043636769250355 ) ) ;
#43383 = CARTESIAN_POINT ( 'NONE',  ( 10.41054107240687188, 1.482358050883964840E-15, 0.000000000000000000 ) ) ;
#43384 = CARTESIAN_POINT ( 'NONE',  ( 83.75530807959195556, -45.27724494717428172, -12.71844083205649056 ) ) ;
#43386 = VECTOR ( 'NONE', #75702, 1000.000000000000000 ) ;
#43385 = CARTESIAN_POINT ( 'NONE',  ( -34.36792678279851287, 318.9604217263056398, -6.095080103624761492 ) ) ;
#43387 = CARTESIAN_POINT ( 'NONE',  ( -11.90233244705797766, 304.5915716174422982, -9.055312000094444258 ) ) ;
#43388 = DIRECTION ( 'NONE',  ( 0.000000000000000000, 0.000000000000000000, 1.000000000000000000 ) ) ;
#43389 = ORIENTED_EDGE ( 'NONE', *, *, #41015, .F. ) ;
#43391 = EDGE_CURVE ( 'NONE', #25738, #14483, #103114, .T. ) ;
#43390 = CARTESIAN_POINT ( 'NONE',  ( -42.69811214730274429, 434.9611672192513652, 18.34625614733215215 ) ) ;
#43392 = EDGE_LOOP ( 'NONE', ( #73838, #24645, #83057, #52066, #32654 ) ) ;
#43393 = FILL_AREA_STYLE_COLOUR ( '', #58814 ) ;
#43394 = DIRECTION ( 'NONE',  ( 0.2043693274454108089, 0.2793933298622084949, 0.9381751143725876041 ) ) ;
#43396 = VERTEX_POINT ( 'NONE', #8785 ) ;
#43395 = CARTESIAN_POINT ( 'NONE',  ( 5.457386620333100957, 51.31430185318657777, 8.531152949374462224 ) ) ;
#43397 = CARTESIAN_POINT ( 'NONE',  ( 75.09227317690647396, -60.31491160002002516, 137.4141434509855628 ) ) ;
#43398 = ORIENTED_EDGE ( 'NONE', *, *, #26587, .T. ) ;
#43399 = EDGE_CURVE ( 'NONE', #69704, #49330, #22216, .T. ) ;
#43400 = CARTESIAN_POINT ( 'NONE',  ( 4.881492806919405680, -52.01899411372407656, 40.12243117532113956 ) ) ;
#43401 = CARTESIAN_POINT ( 'NONE',  ( 44.46823338009918558, 1.482358050883964840E-15, 0.000000000000000000 ) ) ;
#43402 = CARTESIAN_POINT ( 'NONE',  ( -2.977408999572654480, -22.62500000204838813, 7.188101187499999156 ) ) ;
#43403 = CARTESIAN_POINT ( 'NONE',  ( -94.41147650277389403, -57.65372982601817853, -11.88746169270405773 ) ) ;
#43404 = ORIENTED_EDGE ( 'NONE', *, *, #40677, .F. ) ;
#43405 = AXIS2_PLACEMENT_3D ( 'NONE', #50088, #66274, #1521 ) ;
#43406 = SURFACE_STYLE_FILL_AREA ( #99489 ) ;
#43407 = CARTESIAN_POINT ( 'NONE',  ( 33.58349330513380693, -3.851859888774471706E-31, 4.000000000000001776 ) ) ;
#43408 = VECTOR ( 'NONE', #15355, 1000.000000000000000 ) ;
#43409 = CARTESIAN_POINT ( 'NONE',  ( 102.8682207463923532, -45.28272216667533456, 186.0846881397096695 ) ) ;
#43410 = CARTESIAN_POINT ( 'NONE',  ( -32.86086508068097345, 472.2680268995223969, 9.428505756555059847 ) ) ;
#43411 = MECHANICAL_DESIGN_GEOMETRIC_PRESENTATION_REPRESENTATION (  '', ( #95079 ), #31355 ) ;
#43412 = CARTESIAN_POINT ( 'NONE',  ( 49.26989972136220786, 12.96118195421072450, -15.76560135798010442 ) ) ;
#43413 = CARTESIAN_POINT ( 'NONE',  ( -8.000000000000000000, -14.93750000409677092, -9.797174393178825657E-16 ) ) ;
#43414 = CARTESIAN_POINT ( 'NONE',  ( 0.06682554136338086925, 6.264794173742279426, 2.149058192116893196 ) ) ;
#43415 = CARTESIAN_POINT ( 'NONE',  ( -36.59134229708980257, 25.86727557889577511, 12.99205859245150840 ) ) ;
#43416 = CARTESIAN_POINT ( 'NONE',  ( 102.9313392694734688, -2.002967142162725287E-29, 5.000000000000011546 ) ) ;
#43417 = CARTESIAN_POINT ( 'NONE',  ( 9.537927238823506570, 32.64626857118177838, -3.010735687602430044 ) ) ;
#43418 = CARTESIAN_POINT ( 'NONE',  ( 101.4868948250290259, -5.000000000000000000, 0.000000000000000000 ) ) ;
#43419 = DIRECTION ( 'NONE',  ( 5.551115123125781470E-17, -0.7916386130524933895, -0.6109896122883962111 ) ) ;
#43420 = VERTEX_POINT ( 'NONE', #98847 ) ;
#43421 = CARTESIAN_POINT ( 'NONE',  ( -5.487124250504801459, 41.99999999999998579, -59.74242263126210162 ) ) ;
#43422 = FACE_OUTER_BOUND ( 'NONE', #4519, .T. ) ;
#43423 = B_SPLINE_CURVE_WITH_KNOTS ( 'NONE', 3,
 ( #40053, #98798, #72927, #75053, #106359, #97737, #26049, #49188, #42169, #40581, #23905, #73999, #89673, #24955, #41647, #73461, #74531, #58359, #24442, #57274, #91278, #82089, #57810, #8208 ),
 .UNSPECIFIED., .F., .F.,
 ( 4, 2, 2, 2, 2, 2, 2, 2, 2, 2, 2, 4 ),
 ( 0.000000000000000000, 0.001423843649067600388, 0.002847687298135200776, 0.004271530947202801382, 0.004983452771736591493, 0.005695374596270383338, 0.007119218245337962693, 0.008543061894405543782, 0.009254983718939334761, 0.009966905543473125739, 0.01067882736800691672, 0.01139074919254070770 ),
 .UNSPECIFIED. ) ;
#43424 = CARTESIAN_POINT ( 'NONE',  ( -86.31772595132530057, -30.00000000000000355, 180.5339520493327825 ) ) ;
#43425 = EDGE_CURVE ( 'NONE', #53678, #96838, #41691, .T. ) ;
#43426 = ORIENTED_EDGE ( 'NONE', *, *, #97910, .T. ) ;
#43427 = DIRECTION ( 'NONE',  ( -1.000000000000000000, -1.224606353822377258E-16, -0.000000000000000000 ) ) ;
#43428 = CARTESIAN_POINT ( 'NONE',  ( 73.12522785550909532, -57.64690656528826906, 182.1381851100867664 ) ) ;
#43430 = DIRECTION ( 'NONE',  ( -0.000000000000000000, -1.000000000000000000, -0.000000000000000000 ) ) ;
#43429 = CARTESIAN_POINT ( 'NONE',  ( -15.51348069825386844, 2.608686647714169027, 0.4238655689775820967 ) ) ;
#43431 = EDGE_CURVE ( 'NONE', #87415, #48447, #56257, .T. ) ;
#43432 = EDGE_CURVE ( 'NONE', #2640, #56041, #93672, .T. ) ;
#43433 = CARTESIAN_POINT ( 'NONE',  ( 66.27523070486898860, -37.98760907505894124, -32.42822486897702561 ) ) ;
#43434 = CARTESIAN_POINT ( 'NONE',  ( 20.00000000000000711, 4.000000000000000888, -1.500000000000001332 ) ) ;
#43435 = CARTESIAN_POINT ( 'NONE',  ( -43.58619280597272194, 434.9882623928570524, 14.52865984557737278 ) ) ;
#43436 = CARTESIAN_POINT ( 'NONE',  ( -35.28971009319081986, -60.00000000000002132, 46.67999809849258952 ) ) ;
#43437 = CARTESIAN_POINT ( 'NONE',  ( -30.98778772510896218, 438.9961996591003413, 22.22074261274275386 ) ) ;
#43438 = CARTESIAN_POINT ( 'NONE',  ( 43.69716417794892749, 48.00000000000000000, 48.48761666242516100 ) ) ;
#43439 = CARTESIAN_POINT ( 'NONE',  ( -86.67077660397114869, -39.12965989546195544, 188.4535426357679455 ) ) ;
#43440 = COLOUR_RGB ( '', 0.31764706, 0.68627451, 0.89019608) ;
#43441 = VERTEX_POINT ( 'NONE', #32570 ) ;
#43442 = DIRECTION ( 'NONE',  ( -2.284277986162734315E-16, -0.7561819230143446147, 0.6543614439331888466 ) ) ;
#43443 = CARTESIAN_POINT ( 'NONE',  ( -5.103907831117815874, -46.43917523267403169, 31.61932201913767670 ) ) ;
#43444 = FILL_AREA_STYLE ('',( #84963 ) ) ;
#43445 = COLOUR_RGB ( '', 0.72549020, 0.75294118, 0.79215686) ;
#43446 = CARTESIAN_POINT ( 'NONE',  ( -2.714482629291888660, -49.62047324315857821, 102.8323262222670280 ) ) ;
#43448 =( NAMED_UNIT ( * ) PLANE_ANGLE_UNIT ( ) SI_UNIT ( $, .RADIAN. ) );
#43447 = CARTESIAN_POINT ( 'NONE',  ( -23.14090638779910591, 295.2019495631942050, 2.012332626436514005 ) ) ;
#43449 = ORIENTED_EDGE ( 'NONE', *, *, #20223, .T. ) ;
#43450 = EDGE_CURVE ( 'NONE', #51711, #84725, #97935, .T. ) ;
#43451 = CARTESIAN_POINT ( 'NONE',  ( 29.99397490504469133, 1.005902684993158047, 14.99698745252234033 ) ) ;
#43452 = CARTESIAN_POINT ( 'NONE',  ( -6.795578989018840943, -5.000000000000069278, -15.32583302412394310 ) ) ;
#43453 = CARTESIAN_POINT ( 'NONE',  ( -30.93151921796016524, 9.249586871975878921, -40.69907933257887578 ) ) ;
#43454 = CARTESIAN_POINT ( 'NONE',  ( 25.91107377119099198, 295.8152773742599493, -9.793025909729470513 ) ) ;
#43455 = CARTESIAN_POINT ( 'NONE',  ( 35.56416567323501710, 480.2820146177156175, -4.363888856302766683 ) ) ;
#43456 = ADVANCED_FACE ( 'NONE', ( #25002, #89192 ), #7715, .T. ) ;
#43457 = VECTOR ( 'NONE', #14879, 1000.000000000000000 ) ;
#43458 = DIRECTION ( 'NONE',  ( 0.000000000000000000, 1.000000000000000000, 0.000000000000000000 ) ) ;
#43459 = DIRECTION ( 'NONE',  ( -1.000000000000000000, 0.000000000000000000, 0.000000000000000000 ) ) ;
#43460 = CARTESIAN_POINT ( 'NONE',  ( 103.2299700508879567, -60.00000000000004974, 85.94867762990566007 ) ) ;
#43461 = CARTESIAN_POINT ( 'NONE',  ( -80.77687318190224630, -42.97080845458604870, 155.3688440231170489 ) ) ;
#43462 = ORIENTED_EDGE ( 'NONE', *, *, #95363, .F. ) ;
#43463 = DIRECTION ( 'NONE',  ( -0.5735764363510459374, -0.8191520442889919096, 0.000000000000000000 ) ) ;
#43464 = CARTESIAN_POINT ( 'NONE',  ( 5.999511540169428336, 253.9992673088543143, -0.2833228702578392544 ) ) ;
#43465 = CARTESIAN_POINT ( 'NONE',  ( 29.18545435546700162, -57.68205234359119515, 44.83568442682894784 ) ) ;
#43466 = DIRECTION ( 'NONE',  ( 0.5735764363510491570, -0.8191520442889895781, 1.003171929053522035E-16 ) ) ;
#43467 = CARTESIAN_POINT ( 'NONE',  ( 45.43264684998295877, 375.4384345595471473, 6.660155552370398802 ) ) ;
#43468 = DIRECTION ( 'NONE',  ( 0.000000000000000000, -1.000000000000000000, 0.000000000000000000 ) ) ;
#43469 = EDGE_LOOP ( 'NONE', ( #29750, #61514, #31567, #59942, #60183, #73799 ) ) ;
#43470 = FACE_OUTER_BOUND ( 'NONE', #59660, .T. ) ;
#43471 = VERTEX_POINT ( 'NONE', #81593 ) ;
#43472 = CARTESIAN_POINT ( 'NONE',  ( 0.7060372491588029487, 15.23416508904654521, 9.999999999999998224 ) ) ;
#43473 = CARTESIAN_POINT ( 'NONE',  ( 5.977870854928313271, 41.99823411354464753, -69.20734001019310710 ) ) ;
#43475 = CARTESIAN_POINT ( 'NONE',  ( -63.25915952246064222, 50.00000000000000000, 0.7870165385200997843 ) ) ;
#43474 = ADVANCED_BREP_SHAPE_REPRESENTATION ( '', ( #16991, #10728 ), #103758 ) ;
#43476 = CARTESIAN_POINT ( 'NONE',  ( 5.000000000000079048, -15.32190040641887130, 13.82401333428050627 ) ) ;
#43477 = B_SPLINE_CURVE_WITH_KNOTS ( 'NONE', 3,
 ( #52985, #85906, #29802, #53515, #11979, #4427, #37898, #44909, #103132, #46997, #30317, #79896, #54020, #3906, #69705, #86963, #13030, #28749, #61632, #45958 ),
 .UNSPECIFIED., .F., .F.,
 ( 4, 2, 2, 2, 2, 2, 2, 2, 2, 4 ),
 ( 0.006976481488830035133, 0.007983724882207922369, 0.008487346578896867721, 0.008990968275585811340, 0.009242779123930287485, 0.009494589972274761897, 0.009998211668963712453, 0.01025002251730818860, 0.01050183336565266648, 0.01100545506234161530 ),
 .UNSPECIFIED. ) ;
#43478 = ORIENTED_EDGE ( 'NONE', *, *, #76419, .F. ) ;
#43479 = CARTESIAN_POINT ( 'NONE',  ( 74.96611493089018552, -59.99999999999998579, -30.51875920910361728 ) ) ;
#43480 = AXIS2_PLACEMENT_3D ( 'NONE', #45502, #4492, #77321 ) ;
#43482 = CARTESIAN_POINT ( 'NONE',  ( 18.71245558089175276, -25.55128019488360636, 28.53050335101116275 ) ) ;
#43481 = CARTESIAN_POINT ( 'NONE',  ( -105.0772696006729632, -59.99999999999994316, 202.2127603465211223 ) ) ;
#43484 = CARTESIAN_POINT ( 'NONE',  ( 16.32074838266548156, 61.49999999999999289, 8.160374191332744331 ) ) ;
#43483 = PRODUCT_DEFINITION_CONTEXT ( 'detailed design', #100339, 'design' ) ;
#43485 = CARTESIAN_POINT ( 'NONE',  ( 20.11650669486618881, 1.474610560812782335E-15, 0.000000000000000000 ) ) ;
#43486 = CARTESIAN_POINT ( 'NONE',  ( -43.31012496879380080, -49.89329425690212361, 44.39323085342611819 ) ) ;
#43487 = CARTESIAN_POINT ( 'NONE',  ( -37.46714894334873946, 18.64284798593131853, 8.551881563997355329 ) ) ;
#43488 = UNCERTAINTY_MEASURE_WITH_UNIT (LENGTH_MEASURE( 1.000000000000000082E-05 ), #78700, 'distance_accuracy_value', 'NONE');
#43489 = ORIENTED_EDGE ( 'NONE', *, *, #60833, .T. ) ;
#43490 = CARTESIAN_POINT ( 'NONE',  ( -89.99999999999997158, -60.00000000000000000, 196.0238439516549818 ) ) ;
#43491 = LINE ( 'NONE', #2480, #45668 ) ;
#43492 = DIRECTION ( 'NONE',  ( 0.000000000000000000, 0.000000000000000000, 1.000000000000000000 ) ) ;
#43493 = DIRECTION ( 'NONE',  ( -0.000000000000000000, 1.000000000000000000, -0.000000000000000000 ) ) ;
#43494 = CARTESIAN_POINT ( 'NONE',  ( 6.169949891408088583, 6.308465495020067593, 2.073417244832475692 ) ) ;
#43495 = CARTESIAN_POINT ( 'NONE',  ( 8.380151598009016212, -0.1935070982757394475, 19.49075913394571558 ) ) ;
#43496 = VERTEX_POINT ( 'NONE', #57326 ) ;
#43497 =( NAMED_UNIT ( * ) PLANE_ANGLE_UNIT ( ) SI_UNIT ( $, .RADIAN. ) );
#43498 = ORIENTED_EDGE ( 'NONE', *, *, #82682, .F. ) ;
#43499 = CARTESIAN_POINT ( 'NONE',  ( 96.26263212673806891, -30.00000000000000711, 191.2551900954179587 ) ) ;
#43500 = CARTESIAN_POINT ( 'NONE',  ( 41.43935051928187363, 39.62186541985202126, -51.04584900469333064 ) ) ;
#43501 = CARTESIAN_POINT ( 'NONE',  ( 1.400734872026642375, 15.45478884909084272, 9.907647895771706459 ) ) ;
#43502 = CARTESIAN_POINT ( 'NONE',  ( 81.76910224116089410, -30.00000000000000000, 31.60432335422153116 ) ) ;
#43503 = FILL_AREA_STYLE ('',( #93655 ) ) ;
#43504 = EDGE_LOOP ( 'NONE', ( #72405, #26133, #104169, #39089, #33953 ) ) ;
#43505 = EDGE_CURVE ( 'NONE', #16973, #11528, #88502, .T. ) ;
#43506 = ORIENTED_EDGE ( 'NONE', *, *, #99905, .T. ) ;
#43507 = ORIENTED_EDGE ( 'NONE', *, *, #48638, .F. ) ;
#43509 = ORIENTED_EDGE ( 'NONE', *, *, #67988, .F. ) ;
#43508 = CARTESIAN_POINT ( 'NONE',  ( 0.000000000000000000, 0.000000000000000000, 5.000000000000000000 ) ) ;
#43510 = DIRECTION ( 'NONE',  ( 0.000000000000000000, -1.000000000000000000, 0.000000000000000000 ) ) ;
#43511 = CARTESIAN_POINT ( 'NONE',  ( 4.898587196589412829E-16, -15.12499999999999289, -8.000000000000000000 ) ) ;
#43512 = CARTESIAN_POINT ( 'NONE',  ( 5.725989721596482340, -13.57677111256461622, 1.809923354557178898 ) ) ;
#43513 = CARTESIAN_POINT ( 'NONE',  ( 6.585468679846620432, 3.617797563910809533, -6.733790807807556789 ) ) ;
#43514 = EDGE_CURVE ( 'NONE', #93631, #32237, #16349, .T. ) ;
#43515 = DIRECTION ( 'NONE',  ( 0.000000000000000000, -1.000000000000000000, 0.000000000000000000 ) ) ;
#43516 = EDGE_LOOP ( 'NONE', ( #70628, #70032, #81149, #49585, #5645 ) ) ;
#43518 = EDGE_CURVE ( 'NONE', #37118, #32281, #41167, .T. ) ;
#43517 = CARTESIAN_POINT ( 'NONE',  ( -11.99999999999999467, 50.00000000000000000, -83.42920367502570400 ) ) ;
#43519 = VERTEX_POINT ( 'NONE', #132 ) ;
#43520 = LINE ( 'NONE', #10079, #50093 ) ;
#43521 = CARTESIAN_POINT ( 'NONE',  ( 75.64534851151876182, -38.35868239334193674, 175.4885248428145701 ) ) ;
#43522 = DIRECTION ( 'NONE',  ( -0.000000000000000000, -0.000000000000000000, 1.000000000000000000 ) ) ;
#43523 = CARTESIAN_POINT ( 'NONE',  ( 31.99770529497660831, 299.5165077758936718, 2.979034379301395141 ) ) ;
#43524 = CIRCLE ( 'NONE', #38613, 4.000000000000007105 ) ;
#43525 = ADVANCED_FACE ( 'NONE', ( #56799 ), #25551, .T. ) ;
#43526 = CARTESIAN_POINT ( 'NONE',  ( -6.499999999999999112, 3.752776749732556816, -8.000000000000000000 ) ) ;
#43527 = AXIS2_PLACEMENT_3D ( 'NONE', #34428, #16606, #8506 ) ;
#43528 = EDGE_LOOP ( 'NONE', ( #60104, #9227, #24371, #86384 ) ) ;
#43529 = ADVANCED_FACE ( 'NONE', ( #33620 ), #58410, .T. ) ;
#43530 = CARTESIAN_POINT ( 'NONE',  ( 29.68315524076959377, 13.12249633091058243, -39.60535821593525441 ) ) ;
#43531 = DIRECTION ( 'NONE',  ( -1.000000000000000000, -1.224606353822377258E-16, -0.000000000000000000 ) ) ;
#43532 = CARTESIAN_POINT ( 'NONE',  ( 0.000000000000000000, 0.000000000000000000, -8.000000000000000000 ) ) ;
#43533 = DIRECTION ( 'NONE',  ( 0.000000000000000000, -0.8660254037844380415, 0.5000000000000009992 ) ) ;
#43534 = VERTEX_POINT ( 'NONE', #60032 ) ;
#43535 = CARTESIAN_POINT ( 'NONE',  ( -13.00000000000003730, -10.00000000000000888, -4.000000000000000000 ) ) ;
#43536 = LINE ( 'NONE', #33871, #17833 ) ;
#43537 = B_SPLINE_CURVE_WITH_KNOTS ( 'NONE', 3,
 ( #42616, #26481, #85208, #58823, #10249, #67964 ),
 .UNSPECIFIED., .F., .F.,
 ( 4, 2, 4 ),
 ( 0.008690415895085790154, 0.01102883710845593661, 0.01336725832182608306 ),
 .UNSPECIFIED. ) ;
#43538 = CARTESIAN_POINT ( 'NONE',  ( 42.74850648157743649, 465.8913842144178830, 12.61550125132738209 ) ) ;
#43539 = CARTESIAN_POINT ( 'NONE',  ( 33.32781438368718341, 490.0012478077239280, 11.19551906499331828 ) ) ;
#43540 = FACE_OUTER_BOUND ( 'NONE', #30381, .T. ) ;
#43541 = DIRECTION ( 'NONE',  ( 0.000000000000000000, 0.000000000000000000, 1.000000000000000000 ) ) ;
#43542 = CARTESIAN_POINT ( 'NONE',  ( 85.44540022114718170, -61.06638023725951570, 193.8744620643309418 ) ) ;
#43543 = FACE_OUTER_BOUND ( 'NONE', #95640, .T. ) ;
#43544 = CARTESIAN_POINT ( 'NONE',  ( -7.860264365974899192, 85.36576122642846087, 4.999999999997459810 ) ) ;
#43545 = ORIENTED_EDGE ( 'NONE', *, *, #10358, .T. ) ;
#43546 = CYLINDRICAL_SURFACE ( 'NONE', #37769, 4.000000000000000000 ) ;
#43547 = LINE ( 'NONE', #86159, #38383 ) ;
#43548 = CYLINDRICAL_SURFACE ( 'NONE', #4189, 4.000000000000001776 ) ;
#43549 =( LENGTH_UNIT ( ) NAMED_UNIT ( * ) SI_UNIT ( .MILLI., .METRE. ) );
#43550 = CARTESIAN_POINT ( 'NONE',  ( -83.18161732247874340, -29.99999999999999645, 44.35520410614308418 ) ) ;
#43551 = LINE ( 'NONE', #69435, #36570 ) ;
#43552 = CARTESIAN_POINT ( 'NONE',  ( -6.439685834476830628, 4.942299687813059172, -7.659344964963183955 ) ) ;
#43554 = CARTESIAN_POINT ( 'NONE',  ( 0.000000000000000000, 6.123233995736767268E-16, -5.000000000000000888 ) ) ;
#43553 = DIRECTION ( 'NONE',  ( 1.000000000000000000, 0.000000000000000000, 0.000000000000000000 ) ) ;
#43555 = EDGE_CURVE ( 'NONE', #101359, #17114, #83728, .T. ) ;
#43556 = CARTESIAN_POINT ( 'NONE',  ( 3.252284881921470916, -53.34547930654326819, 40.61850418307594879 ) ) ;
#43557 = CARTESIAN_POINT ( 'NONE',  ( -45.06251741407306355, -36.90970505544751035, 43.04236430708314742 ) ) ;
#43558 = CARTESIAN_POINT ( 'NONE',  ( 14.81135246989093801, 41.99477691750401931, -87.54767829888531594 ) ) ;
#43559 = CARTESIAN_POINT ( 'NONE',  ( 35.98291722399694237, -23.65727476560045872, -31.11900096256992398 ) ) ;
#43560 = CARTESIAN_POINT ( 'NONE',  ( -24.64341543703087467, -32.52149348492427094, 30.48647817142265737 ) ) ;
#43561 = ORIENTED_EDGE ( 'NONE', *, *, #97217, .T. ) ;
#43562 = CARTESIAN_POINT ( 'NONE',  ( 6.750000000000016875, -11.69134295108991495, 0.000000000000000000 ) ) ;
#43563 = CARTESIAN_POINT ( 'NONE',  ( -9.483056940782027766, 107.4438779010658038, -3.177305548492606047 ) ) ;
#43564 = CARTESIAN_POINT ( 'NONE',  ( -16.89468671705794023, -46.43925381171047917, 31.87895912059618553 ) ) ;
#43565 = CARTESIAN_POINT ( 'NONE',  ( -55.56355992248217035, -28.58787366841717414, -26.41023078683522129 ) ) ;
#43566 =( BOUNDED_SURFACE ( )  B_SPLINE_SURFACE ( 3, 2, ( 
 ( #19791, #52625, #28951 ),
 ( #77980, #85556, #59684 ),
 ( #28402, #45101, #4097 ),
 ( #37025, #69893, #78500 ),
 ( #67763, #92562, #80614 ),
 ( #97332, #6194, #46153 ),
 ( #70949, #21899, #31578 ),
 ( #64460, #31061, #23486 ),
 ( #56327, #89261, #39131 ),
 ( #104364, #72009, #13757 ) ),
 .UNSPECIFIED., .F., .F., .T. ) 
 B_SPLINE_SURFACE_WITH_KNOTS ( ( 4, 2, 2, 2, 4 ),
 ( 3, 3 ),
 ( 2.960956133057912609E-15, 0.002844712610147792642, 0.003555890762684000509, 0.004267068915220208376, 0.005689425220292624111 ),
 ( 0.000000000000000000, 1.000000000000000000 ),
 .UNSPECIFIED. ) 
 GEOMETRIC_REPRESENTATION_ITEM ( )  RATIONAL_B_SPLINE_SURFACE ( (
 ( 1.000000000000000000, 0.8258027051675366215, 1.000000000000000000),
 ( 1.000000000000000000, 0.8423184768576185144, 1.000000000000000000),
 ( 1.000000000000000000, 0.8479189272866914928, 1.000000000000000000),
 ( 1.000000000000000000, 0.8482780919515218176, 1.000000000000000000),
 ( 1.000000000000000000, 0.8479712937353218738, 1.000000000000000000),
 ( 1.000000000000000000, 0.8466356411021724870, 1.000000000000000000),
 ( 1.000000000000000000, 0.8456087446167629418, 1.000000000000000000),
 ( 1.000000000000000000, 0.8414089630425088950, 1.000000000000000000),
 ( 1.000000000000000000, 0.8371477558872925107, 1.000000000000000000),
 ( 1.000000000000000000, 0.8308329163121775940, 1.000000000000000000) ) ) 
 REPRESENTATION_ITEM ( '' )  SURFACE ( )  );
#43568 = CARTESIAN_POINT ( 'NONE',  ( -38.45611865049527012, 439.3122198965025405, 23.73029221708416614 ) ) ;
#43567 = CARTESIAN_POINT ( 'NONE',  ( -32.12958771267418712, 464.7275665249413805, 11.12424126545828784 ) ) ;
#43569 = EDGE_LOOP ( 'NONE', ( #59166, #951, #46167, #48753 ) ) ;
#43570 = CARTESIAN_POINT ( 'NONE',  ( -35.47320774096329643, 436.4618599381972217, 5.062587423523073227 ) ) ;
#43571 = ORIENTED_EDGE ( 'NONE', *, *, #10371, .T. ) ;
#43572 = DIRECTION ( 'NONE',  ( 0.000000000000000000, 0.000000000000000000, 1.000000000000000000 ) ) ;
#43573 = CARTESIAN_POINT ( 'NONE',  ( 15.86692673747663918, 3.934633648118698979, 3.950574283723627733 ) ) ;
#43574 = CARTESIAN_POINT ( 'NONE',  ( -8.421684505501604079, -59.99999999999999289, -42.47678725903364949 ) ) ;
#43575 = ORIENTED_EDGE ( 'NONE', *, *, #24802, .F. ) ;
#43576 = CARTESIAN_POINT ( 'NONE',  ( 4.000000000000002665, 4.898587196589416773E-16, -7.974599999999995248 ) ) ;
#43577 = CARTESIAN_POINT ( 'NONE',  ( 99.99568154413580601, -45.27326971109869902, 192.6082355761231213 ) ) ;
#43578 = CIRCLE ( 'NONE', #50415, 5.000000000000002665 ) ;
#43580 = CARTESIAN_POINT ( 'NONE',  ( -7.551892080562054410, -6.990122974606172157, 2.647003822403975359 ) ) ;
#43579 = CARTESIAN_POINT ( 'NONE',  ( 12.58304801162219810, -21.69704017138143115, 27.55869761091397763 ) ) ;
#43581 = ADVANCED_FACE ( 'NONE', ( #59487 ), #80529, .T. ) ;
#43582 = ORIENTED_EDGE ( 'NONE', *, *, #27329, .T. ) ;
#43583 = STYLED_ITEM ( 'NONE', ( #54260 ), #83666 ) ;
#43584 = VERTEX_POINT ( 'NONE', #20122 ) ;
#43585 = CONICAL_SURFACE ( 'NONE', #3951, 5.000000000000001776, 0.9599310885968803664 ) ;
#43586 = ORIENTED_EDGE ( 'NONE', *, *, #3073, .F. ) ;
#43587 = CARTESIAN_POINT ( 'NONE',  ( 28.80551732330762604, 315.1542978612143315, 12.69625289295432857 ) ) ;
#43588 = CARTESIAN_POINT ( 'NONE',  ( 6.500000000000007105, -3.752776749732581685, -0.7999999999999977129 ) ) ;
#43589 = DIRECTION ( 'NONE',  ( 0.000000000000000000, -1.000000000000000000, 0.000000000000000000 ) ) ;
#43590 = VERTEX_POINT ( 'NONE', #51897 ) ;
#43591 = CARTESIAN_POINT ( 'NONE',  ( 0.000000000000000000, 0.000000000000000000, -6.499999999999999112 ) ) ;
#43592 = DIRECTION ( 'NONE',  ( 1.000000000000000000, 0.000000000000000000, 0.000000000000000000 ) ) ;
#43593 = CARTESIAN_POINT ( 'NONE',  ( 23.73746414932995208, 1.482358050883964840E-15, 0.000000000000000000 ) ) ;
#43594 = CARTESIAN_POINT ( 'NONE',  ( -105.0872854236518208, -59.99999999972659737, 96.83056509434175041 ) ) ;
#43595 = FACE_BOUND ( 'NONE', #17600, .T. ) ;
#43596 = CARTESIAN_POINT ( 'NONE',  ( -31.00389226249483698, 502.9289871839745842, 8.047326149841639520 ) ) ;
#43597 = DIRECTION ( 'NONE',  ( 0.000000000000000000, 0.000000000000000000, 1.000000000000000000 ) ) ;
#43598 = CARTESIAN_POINT ( 'NONE',  ( -87.24749885984873288, -14.21045842199425024, -0.3946065656837255964 ) ) ;
#43599 = SURFACE_STYLE_USAGE ( .BOTH. , #44683 ) ;
#43600 = CARTESIAN_POINT ( 'NONE',  ( -50.06693045002293019, -46.44288008262338963, 53.18188324199074657 ) ) ;
#43601 = ORIENTED_EDGE ( 'NONE', *, *, #40811, .T. ) ;
#43602 = CARTESIAN_POINT ( 'NONE',  ( -0.2701126386571010007, 21.84581818726675095, 6.996060251427160814 ) ) ;
#43603 = VERTEX_POINT ( 'NONE', #28210 ) ;
#43604 = CARTESIAN_POINT ( 'NONE',  ( 12.50000000000000000, 0.4010731690309218278, -18.19005076526336140 ) ) ;
#43605 = CARTESIAN_POINT ( 'NONE',  ( -9.766195837844021455, 294.6492712292731539, -2.152655282870724829 ) ) ;
#43606 = CARTESIAN_POINT ( 'NONE',  ( 4.472135954999582275, -9.725881490016750064, -4.000000000000000000 ) ) ;
#43607 = VERTEX_POINT ( 'NONE', #68091 ) ;
#43608 = CARTESIAN_POINT ( 'NONE',  ( 5.909155701201248334, 246.1373831981126727, 1.073778020691680490 ) ) ;
#43609 = CARTESIAN_POINT ( 'NONE',  ( 89.24963295654325179, -29.99999999997994138, 8.815628760632554517 ) ) ;
#43610 = CARTESIAN_POINT ( 'NONE',  ( 0.000000000000000000, 152.0000000000000000, 0.000000000000000000 ) ) ;
#43611 = CARTESIAN_POINT ( 'NONE',  ( 3.396360046676563993, -49.15315706213417002, 103.9790200242190821 ) ) ;
#43612 = AXIS2_PLACEMENT_3D ( 'NONE', #92605, #10094, #101244 ) ;
#43613 = CARTESIAN_POINT ( 'NONE',  ( 13.50000000000000355, 7.794228634059934713, -13.00000000000000000 ) ) ;
#43614 = CARTESIAN_POINT ( 'NONE',  ( -23.70422451879018055, 42.00000000000000000, 88.20421627933653497 ) ) ;
#43615 = CARTESIAN_POINT ( 'NONE',  ( 87.20282465662560867, -29.99999999999999645, 184.4716329640986885 ) ) ;
#43616 = AXIS2_PLACEMENT_3D ( 'NONE', #94241, #2018, #34966 ) ;
#43617 = DIRECTION ( 'NONE',  ( 1.000000000000000000, 1.224606353822377258E-16, 0.000000000000000000 ) ) ;
#43618 = DIRECTION ( 'NONE',  ( 0.000000000000000000, 0.000000000000000000, -1.000000000000000000 ) ) ;
#43619 = VERTEX_POINT ( 'NONE', #76171 ) ;
#43620 = ORIENTED_EDGE ( 'NONE', *, *, #25828, .F. ) ;
#43621 = CARTESIAN_POINT ( 'NONE',  ( 51.81251031740741553, -56.83722578688029614, 60.27040154863821897 ) ) ;
#43622 = CONICAL_SURFACE ( 'NONE', #59111, 5.000000000000001776, 0.9599310885968803664 ) ;
#43623 = CARTESIAN_POINT ( 'NONE',  ( 6.873632531530262213, 41.52280089014492148, -58.77795419705466884 ) ) ;
#43624 = CARTESIAN_POINT ( 'NONE',  ( -7.500000000000007994, 40.00000000000000000, -65.90297133633691828 ) ) ;
#43625 = EDGE_CURVE ( 'NONE', #61515, #101499, #26614, .T. ) ;
#43626 = ORIENTED_EDGE ( 'NONE', *, *, #1136, .T. ) ;
#43628 = EDGE_CURVE ( 'NONE', #96331, #17391, #100455, .T. ) ;
#43627 = CARTESIAN_POINT ( 'NONE',  ( -90.41562289390209628, -38.40191935066286533, -14.83428885377948347 ) ) ;
#43629 = VERTEX_POINT ( 'NONE', #101527 ) ;
#43630 = CARTESIAN_POINT ( 'NONE',  ( 8.000000000000000000, -29.09375000409677270, -3.313708498984761164 ) ) ;
#43631 = CARTESIAN_POINT ( 'NONE',  ( 106.6780022803428380, -38.36736985975626624, 195.3823964213139561 ) ) ;
#43632 = CARTESIAN_POINT ( 'NONE',  ( 12.69126316887715689, 23.10611922033335119, -5.365485820795227845 ) ) ;
#43633 = CARTESIAN_POINT ( 'NONE',  ( 84.22497889915220526, -45.28298033193925676, 26.08978801077915932 ) ) ;
#43634 = PLANE ( 'NONE',  #104959 ) ;
#43635 = CARTESIAN_POINT ( 'NONE',  ( -24.71530540495096417, 306.0434402448361766, -8.740882662338435694 ) ) ;
#43636 = PRESENTATION_STYLE_ASSIGNMENT (( #51718 ) ) ;
#43637 = CARTESIAN_POINT ( 'NONE',  ( 6.585304040558097149, -4.021874164301456389, 6.500000000000001776 ) ) ;
#43638 = EDGE_CURVE ( 'NONE', #82728, #71070, #43813, .T. ) ;
#43639 = CARTESIAN_POINT ( 'NONE',  ( 36.36650669486618881, -3.999999999999998224, 0.000000000000000000 ) ) ;
#43640 = CARTESIAN_POINT ( 'NONE',  ( 7.955551520407984079, 98.60650887776563422, 0.000000000000000000 ) ) ;
#43641 = ORIENTED_EDGE ( 'NONE', *, *, #49947, .T. ) ;
#43642 = DIRECTION ( 'NONE',  ( -1.000000000000000000, 0.000000000000000000, 0.000000000000000000 ) ) ;
#43643 = CARTESIAN_POINT ( 'NONE',  ( 7.445752247298699444, 40.55658335127025538, -70.17153608768727224 ) ) ;
#43644 = DIRECTION ( 'NONE',  ( -0.000000000000000000, -0.000000000000000000, -1.000000000000000000 ) ) ;
#43645 = ORIENTED_EDGE ( 'NONE', *, *, #73673, .T. ) ;
#43646 = CARTESIAN_POINT ( 'NONE',  ( -25.85485528147027168, 306.6938288622521895, -8.594803261285228757 ) ) ;
#43647 = CARTESIAN_POINT ( 'NONE',  ( -36.42407664602379214, 305.7434830039975964, 4.478253505840557480 ) ) ;
#43648 = DIRECTION ( 'NONE',  ( -0.8191520442889974607, 0.000000000000000000, -0.5735764363510379438 ) ) ;
#43649 = LINE ( 'NONE', #84113, #24935 ) ;
#43650 = CARTESIAN_POINT ( 'NONE',  ( 3.313708498984762052, -27.21874999999999645, -8.000000000000000000 ) ) ;
#43651 = FILL_AREA_STYLE_COLOUR ( '', #31311 ) ;
#43652 = CARTESIAN_POINT ( 'NONE',  ( 18.91781669292794987, 48.00000000000000000, 62.18610382930901892 ) ) ;
#43653 = TOROIDAL_SURFACE ( 'NONE', #69461, 12.00000000000001066, 3.000000000000000000 ) ;
#43654 = ORIENTED_EDGE ( 'NONE', *, *, #74327, .T. ) ;
#43655 = CARTESIAN_POINT ( 'NONE',  ( 84.35218974313944784, -35.91427077666032375, 176.6979861380962404 ) ) ;
#43656 = DIRECTION ( 'NONE',  ( 1.000000000000000000, 0.000000000000000000, 0.000000000000000000 ) ) ;
#43657 = DIRECTION ( 'NONE',  ( -0.000000000000000000, 1.000000000000000000, -0.000000000000000000 ) ) ;
#43658 = ORIENTED_EDGE ( 'NONE', *, *, #29608, .T. ) ;
#43659 = AXIS2_PLACEMENT_3D ( 'NONE', #16770, #75532, #35650 ) ;
#43660 = CARTESIAN_POINT ( 'NONE',  ( -91.82262176611270377, -60.15457395765744053, 66.54832966913770065 ) ) ;
#43661 = CARTESIAN_POINT ( 'NONE',  ( -3.828588921589437533E-15, 7.321656987762870550, -3.318518101603011861 ) ) ;
#43662 = CARTESIAN_POINT ( 'NONE',  ( -10.19007819943550786, -3.000000000000002665, -96.34610920172687543 ) ) ;
#43663 = DIRECTION ( 'NONE',  ( 0.000000000000000000, 0.000000000000000000, 1.000000000000000000 ) ) ;
#43664 = CARTESIAN_POINT ( 'NONE',  ( -14.20331398951563173, -23.82509769195230476, -38.53390941360537170 ) ) ;
#43665 = STYLED_ITEM ( 'NONE', ( #47685 ), #52984 ) ;
#43666 =( LENGTH_UNIT ( ) NAMED_UNIT ( * ) SI_UNIT ( .MILLI., .METRE. ) );
#43667 = CARTESIAN_POINT ( 'NONE',  ( 41.54751723293285437, -60.00000000000000711, 54.42831949363168320 ) ) ;
#43668 = AXIS2_PLACEMENT_3D ( 'NONE', #63828, #55170, #38499 ) ;
#43669 = CARTESIAN_POINT ( 'NONE',  ( 32.03079550275963783, -33.76634389418148174, 41.86185369695325420 ) ) ;
#43670 = CARTESIAN_POINT ( 'NONE',  ( 7.934203308536662114, 108.8670034001779783, 1.057099537198549655 ) ) ;
#43671 = CARTESIAN_POINT ( 'NONE',  ( 26.78471285382464018, -20.14333726486478682, 31.71525114976481063 ) ) ;
#43673 = CARTESIAN_POINT ( 'NONE',  ( -12.78544757660326603, 21.24685875135632784, 5.680288811016952266 ) ) ;
#43672 = CARTESIAN_POINT ( 'NONE',  ( -38.38809213244076801, -37.07590732314030646, 47.79844471891385638 ) ) ;
#43674 = ADVANCED_FACE ( 'NONE', ( #85342 ), #49578, .T. ) ;
#43675 = CARTESIAN_POINT ( 'NONE',  ( 1.249646147396492601, 294.8475419170831060, -9.939938411525382378 ) ) ;
#43676 = CARTESIAN_POINT ( 'NONE',  ( 39.24156521425334176, 307.7088117867400001, -7.003459073692002157 ) ) ;
#43677 = DIRECTION ( 'NONE',  ( 0.000000000000000000, 1.000000000000000000, 0.000000000000000000 ) ) ;
#43678 =( NAMED_UNIT ( * ) SI_UNIT ( $, .STERADIAN. ) SOLID_ANGLE_UNIT ( ) );
#43679 = ORIENTED_EDGE ( 'NONE', *, *, #3372, .F. ) ;
#43680 = LINE ( 'NONE', #84679, #72576 ) ;
#43681 = CARTESIAN_POINT ( 'NONE',  ( -17.49999999999997158, 50.67917894244530430, 63.46126552128608722 ) ) ;
#43682 = DIRECTION ( 'NONE',  ( 0.000000000000000000, 1.000000000000000000, 0.000000000000000000 ) ) ;
#43683 = CARTESIAN_POINT ( 'NONE',  ( 0.000000000000000000, 60.00000000000000000, 0.000000000000000000 ) ) ;
#43684 = CIRCLE ( 'NONE', #4047, 4.250000000000000000 ) ;
#43685 = EDGE_CURVE ( 'NONE', #73379, #87999, #75370, .T. ) ;
#43687 = CARTESIAN_POINT ( 'NONE',  ( 12.44550202702694364, -21.77031843812234868, -30.18240907129194994 ) ) ;
#43686 = SURFACE_STYLE_USAGE ( .BOTH. , #35099 ) ;
#43688 = ORIENTED_EDGE ( 'NONE', *, *, #100555, .F. ) ;
#43689 =( GEOMETRIC_REPRESENTATION_CONTEXT ( 3 ) GLOBAL_UNCERTAINTY_ASSIGNED_CONTEXT ( ( #90450 ) ) GLOBAL_UNIT_ASSIGNED_CONTEXT ( ( #54479, #95500, #21643 ) ) REPRESENTATION_CONTEXT ( 'NONE', 'WORKASPACE' ) );
#43690 = CARTESIAN_POINT ( 'NONE',  ( -44.21269619315447130, 463.3337519764560852, 6.736501381177894210 ) ) ;
#43691 = DIRECTION ( 'NONE',  ( -1.000000000000000000, -1.224606353822377258E-16, -0.000000000000000000 ) ) ;
#43692 = MECHANICAL_DESIGN_GEOMETRIC_PRESENTATION_REPRESENTATION (  '', ( #52080 ), #62659 ) ;
#43693 = ORIENTED_EDGE ( 'NONE', *, *, #42547, .F. ) ;
#43694 = DIRECTION ( 'NONE',  ( 0.000000000000000000, -1.000000000000000000, 0.000000000000000000 ) ) ;
#43695 = CARTESIAN_POINT ( 'NONE',  ( -6.690415133250795954, 41.73276121203647904, -59.04972748448755482 ) ) ;
#43696 = DIRECTION ( 'NONE',  ( 0.000000000000000000, -1.000000000000000000, 0.000000000000000000 ) ) ;
#43697 = CARTESIAN_POINT ( 'NONE',  ( -91.86617004484983795, -60.00000000000000000, 10.83445478909512261 ) ) ;
#43698 = CARTESIAN_POINT ( 'NONE',  ( 9.797174393178825657E-16, -30.00000000000000000, -8.000000000000000000 ) ) ;
#43699 = CARTESIAN_POINT ( 'NONE',  ( 2.623433461001182909, -7.604994000793868558, -7.633824513837120129 ) ) ;
#43700 = CARTESIAN_POINT ( 'NONE',  ( 39.86626972871174246, 464.8590688799406507, 17.95745982857005529 ) ) ;
#43701 = CARTESIAN_POINT ( 'NONE',  ( 40.66084078640295729, 460.3808361429892102, 2.363412739912836180 ) ) ;
#43703 = DIRECTION ( 'NONE',  ( 0.000000000000000000, 0.000000000000000000, 1.000000000000000000 ) ) ;
#43702 = CARTESIAN_POINT ( 'NONE',  ( 1.308996937483426715, -3.000000000000002665, -75.00000000000001421 ) ) ;
#43704 = EDGE_CURVE ( 'NONE', #45269, #51428, #29429, .T. ) ;
#43705 = CARTESIAN_POINT ( 'NONE',  ( -84.69258335735655407, -28.96439599382944508, 169.4305326073071853 ) ) ;
#43706 = ORIENTED_EDGE ( 'NONE', *, *, #78011, .T. ) ;
#43707 = ORIENTED_EDGE ( 'NONE', *, *, #21015, .T. ) ;
#43708 = ORIENTED_EDGE ( 'NONE', *, *, #3797, .F. ) ;
#43709 = CARTESIAN_POINT ( 'NONE',  ( 21.08349330513380693, 4.000000000000002665, 0.000000000000000000 ) ) ;
#43710 = CARTESIAN_POINT ( 'NONE',  ( 18.16578424162143079, -4.332661967058973218, -1.112710490967694810 ) ) ;
#43711 = EDGE_CURVE ( 'NONE', #74596, #52893, #58127, .T. ) ;
#43712 = LINE ( 'NONE', #35663, #11218 ) ;
#43713 = EDGE_LOOP ( 'NONE', ( #50516, #105508, #81098, #41452, #66727 ) ) ;
#43714 = CIRCLE ( 'NONE', #90299, 4.000000000000001776 ) ;
#43715 = FACE_OUTER_BOUND ( 'NONE', #44048, .T. ) ;
#43716 = CARTESIAN_POINT ( 'NONE',  ( -113.3221076330293471, -57.67118219814813784, 155.4948299128208191 ) ) ;
#43717 = CARTESIAN_POINT ( 'NONE',  ( 7.986711519608431509, -13.97361903623434820, -0.5300249774147621773 ) ) ;
#43718 = CARTESIAN_POINT ( 'NONE',  ( 0.3173508448886554478, 8.480771745766404024, 1.310872448937997259 ) ) ;
#43719 = CARTESIAN_POINT ( 'NONE',  ( 23.21751746555303342, 27.38103382803677377, 33.20617127781017075 ) ) ;
#43720 = CYLINDRICAL_SURFACE ( 'NONE', #2831, 4.000000000000000000 ) ;
#43721 = CARTESIAN_POINT ( 'NONE',  ( -5.000000000000000000, -13.86898977591626192, 11.25489781251236820 ) ) ;
#43722 = CARTESIAN_POINT ( 'NONE',  ( 103.2299700508879567, -60.00000000000004974, 85.94867762990566007 ) ) ;
#43723 = CARTESIAN_POINT ( 'NONE',  ( -86.32002947858198638, -29.99999999999988987, 198.0868106477030892 ) ) ;
#43724 = CARTESIAN_POINT ( 'NONE',  ( -57.41802865368278930, -39.49559850351909773, 65.76057902791269782 ) ) ;
#43725 = B_SPLINE_CURVE_WITH_KNOTS ( 'NONE', 3,
 ( #7196, #63344, #72984, #39599 ),
 .UNSPECIFIED., .F., .F.,
 ( 4, 4 ),
 ( 4.336808689942017736E-18, 0.001738772145493835486 ),
 .UNSPECIFIED. ) ;
#43726 = ORIENTED_EDGE ( 'NONE', *, *, #82873, .F. ) ;
#43727 = DIRECTION ( 'NONE',  ( -0.000000000000000000, 1.000000000000000000, -0.000000000000000000 ) ) ;
#43728 = ORIENTED_EDGE ( 'NONE', *, *, #43222, .T. ) ;
#43729 = CARTESIAN_POINT ( 'NONE',  ( -104.0809943399287505, -60.15808651304565302, 190.6463388486238557 ) ) ;
#43730 = CARTESIAN_POINT ( 'NONE',  ( -2.977408999572650039, -10.06250000204838457, -7.188101187500000933 ) ) ;
#43731 =( GEOMETRIC_REPRESENTATION_CONTEXT ( 3 ) GLOBAL_UNCERTAINTY_ASSIGNED_CONTEXT ( ( #20135 ) ) GLOBAL_UNIT_ASSIGNED_CONTEXT ( ( #62164, #55084, #21189 ) ) REPRESENTATION_CONTEXT ( 'NONE', 'WORKASPACE' ) );
#43732 = DIRECTION ( 'NONE',  ( 0.000000000000000000, 0.000000000000000000, -1.000000000000000000 ) ) ;
#43733 = ORIENTED_EDGE ( 'NONE', *, *, #48632, .T. ) ;
#43734 = DIRECTION ( 'NONE',  ( 0.8191520442889924647, 1.003171929053525486E-16, -0.5735764363510451602 ) ) ;
#43735 = AXIS2_PLACEMENT_3D ( 'NONE', #93855, #4844, #28623 ) ;
#43736 = ADVANCED_FACE ( 'NONE', ( #94516 ), #92623, .T. ) ;
#43737 = CARTESIAN_POINT ( 'NONE',  ( -81.74462499157380080, -60.00000000000002132, 197.8260547546231010 ) ) ;
#43738 = CARTESIAN_POINT ( 'NONE',  ( -2.514200967265426634, -0.2912192546974278762, 102.6057089534373574 ) ) ;
#43739 = CARTESIAN_POINT ( 'NONE',  ( -5.082755093536325042, -15.96875000204838635, -5.082755093536325930 ) ) ;
#43740 = LINE ( 'NONE', #2200, #29337 ) ;
#43741 = FACE_OUTER_BOUND ( 'NONE', #47458, .T. ) ;
#43742 = AXIS2_PLACEMENT_3D ( 'NONE', #22671, #21614, #103560 ) ;
#43743 = CARTESIAN_POINT ( 'NONE',  ( 15.29468310206912740, -0.000000000000000000, -7.540179673762702706 ) ) ;
#43744 = CARTESIAN_POINT ( 'NONE',  ( -11.36244727931663689, -4.957670368922723725, -12.57265801651846893 ) ) ;
#43745 = CARTESIAN_POINT ( 'NONE',  ( 19.70764564238371719, 304.7954121406193622, 9.925013215726785631 ) ) ;
#43746 = SURFACE_STYLE_FILL_AREA ( #17898 ) ;
#43747 = UNCERTAINTY_MEASURE_WITH_UNIT (LENGTH_MEASURE( 1.000000000000000082E-05 ), #67761, 'distance_accuracy_value', 'NONE');
#43748 = CARTESIAN_POINT ( 'NONE',  ( -30.40563286230810647, -39.48936947416332544, 33.27199808670961545 ) ) ;
#43749 = UNCERTAINTY_MEASURE_WITH_UNIT (LENGTH_MEASURE( 1.000000000000000082E-05 ), #50172, 'distance_accuracy_value', 'NONE');
#43750 = CARTESIAN_POINT ( 'NONE',  ( 43.03101095780436935, -39.52523172002285889, 41.51020378114284881 ) ) ;
#43751 = DIRECTION ( 'NONE',  ( 1.000000000000000000, 1.224606353822377258E-16, 0.000000000000000000 ) ) ;
#43752 = CARTESIAN_POINT ( 'NONE',  ( -5.887588022526042408, 14.31049540200681669, 3.788193301707003524 ) ) ;
#43753 = CARTESIAN_POINT ( 'NONE',  ( -89.68772280753135817, -38.52026044421657502, 200.4884354424789308 ) ) ;
#43754 = ORIENTED_EDGE ( 'NONE', *, *, #87637, .F. ) ;
#43756 = FACE_OUTER_BOUND ( 'NONE', #20028, .T. ) ;
#43755 = CARTESIAN_POINT ( 'NONE',  ( 84.57469743677759766, -38.35847120622327822, -23.21952487094015538 ) ) ;
#43757 = CARTESIAN_POINT ( 'NONE',  ( 75.38526191690708345, -59.99999999999995737, 138.7226225906020431 ) ) ;
#43758 = CARTESIAN_POINT ( 'NONE',  ( -19.12563387234284562, 49.70270881371637017, 61.69659611208896877 ) ) ;
#43759 = CARTESIAN_POINT ( 'NONE',  ( -7.311443696993588759, 40.96481804360126233, -58.73188616880665336 ) ) ;
#43760 = CARTESIAN_POINT ( 'NONE',  ( 5.207236450897640090, 40.28819309316081387, -70.92786837021314739 ) ) ;
#43761 = DIRECTION ( 'NONE',  ( 0.000000000000000000, -1.000000000000000000, 0.000000000000000000 ) ) ;
#43762 = CARTESIAN_POINT ( 'NONE',  ( 42.31186848673542045, 465.8659795009741629, 14.28293630011768656 ) ) ;
#43763 = CARTESIAN_POINT ( 'NONE',  ( 7.500000000000000000, -6.938893903907228378E-15, -6.991905250253755533 ) ) ;
#43764 = CARTESIAN_POINT ( 'NONE',  ( 111.3354282251981573, -60.00000000000002132, 155.4017638814755173 ) ) ;
#43765 = CARTESIAN_POINT ( 'NONE',  ( 6.692588830498424457, -3.932766476276026157, 6.892929031562514908 ) ) ;
#43766 = COLOUR_RGB ( '', 0.72549020, 0.75294118, 0.79215686) ;
#43767 = ADVANCED_FACE ( 'NONE', ( #46988 ), #12493, .T. ) ;
#43768 = CARTESIAN_POINT ( 'NONE',  ( -7.934914944860276265, -68.86845647200111387, -1.051261972695694213 ) ) ;
#43769 = EDGE_LOOP ( 'NONE', ( #15075, #21746, #14890, #12310, #12939 ) ) ;
#43770 = EDGE_CURVE ( 'NONE', #56015, #68447, #8239, .T. ) ;
#43771 = CARTESIAN_POINT ( 'NONE',  ( 2.068673967786704981, -49.86383299198053720, 102.1191603898000011 ) ) ;
#43772 =( GEOMETRIC_REPRESENTATION_CONTEXT ( 3 ) GLOBAL_UNCERTAINTY_ASSIGNED_CONTEXT ( ( #58605 ) ) GLOBAL_UNIT_ASSIGNED_CONTEXT ( ( #86808, #18905, #85748 ) ) REPRESENTATION_CONTEXT ( 'NONE', 'WORKASPACE' ) );
#43773 = AXIS2_PLACEMENT_3D ( 'NONE', #106240, #97620, #56082 ) ;
#43774 = CARTESIAN_POINT ( 'NONE',  ( 0.000000000000000000, 0.000000000000000000, 6.499999999999999112 ) ) ;
#43775 = ORIENTED_EDGE ( 'NONE', *, *, #77534, .T. ) ;
#43777 = CARTESIAN_POINT ( 'NONE',  ( 0.000000000000000000, 0.000000000000000000, 0.000000000000000000 ) ) ;
#43776 = CARTESIAN_POINT ( 'NONE',  ( -68.45687734878008257, -38.33354253709327963, 127.1540152885862796 ) ) ;
#43778 = SURFACE_STYLE_USAGE ( .BOTH. , #42178 ) ;
#43779 = DIRECTION ( 'NONE',  ( 0.000000000000000000, -1.000000000000000000, 0.000000000000000000 ) ) ;
#43780 = CARTESIAN_POINT ( 'NONE',  ( 7.188101187499999156, -19.62500000204838457, 2.977408999572654924 ) ) ;
#43782 = EDGE_CURVE ( 'NONE', #91474, #74273, #23752, .T. ) ;
#43781 = CARTESIAN_POINT ( 'NONE',  ( -6.288404560131954923, -5.029641972278941608, -0.4504974108211988182 ) ) ;
#43783 = CARTESIAN_POINT ( 'NONE',  ( 30.63784394300822100, 16.09242744237242917, -40.03992687782061921 ) ) ;
#43785 = ORIENTED_EDGE ( 'NONE', *, *, #4671, .T. ) ;
#43784 =( NAMED_UNIT ( * ) SI_UNIT ( $, .STERADIAN. ) SOLID_ANGLE_UNIT ( ) );
#43786 = CARTESIAN_POINT ( 'NONE',  ( 82.78941698165385787, -32.55276419480425432, 157.1437384287463317 ) ) ;
#43787 = CARTESIAN_POINT ( 'NONE',  ( 43.88846153846154152, -4.171999999999999709, 0.000000000000000000 ) ) ;
#43788 = FACE_OUTER_BOUND ( 'NONE', #65736, .T. ) ;
#43789 = EDGE_LOOP ( 'NONE', ( #71367, #53276, #39063 ) ) ;
#43790 = CARTESIAN_POINT ( 'NONE',  ( -21.98328659339751212, 303.0786568297054373, -9.951468641084936451 ) ) ;
#43791 = CARTESIAN_POINT ( 'NONE',  ( 38.77519395269280267, 27.37135291505367718, -11.84730558812103141 ) ) ;
#43792 = DIRECTION ( 'NONE',  ( 1.000000000000000000, 0.000000000000000000, 0.000000000000000000 ) ) ;
#43793 = CARTESIAN_POINT ( 'NONE',  ( -5.858824175751776941, 253.7857906087234028, -1.318356988357146431 ) ) ;
#43794 = CARTESIAN_POINT ( 'NONE',  ( 17.76981297930376158, 43.17870619678550526, 5.956428682172403732 ) ) ;
#43795 = PRODUCT ( '16. Toe', '16. Toe', '', ( #4405 ) ) ;
#43796 = ORIENTED_EDGE ( 'NONE', *, *, #44441, .F. ) ;
#43797 = B_SPLINE_CURVE_WITH_KNOTS ( 'NONE', 3,
 ( #88602, #30928, #64338, #41112, #57268, #40575 ),
 .UNSPECIFIED., .F., .F.,
 ( 4, 2, 4 ),
 ( 0.003990927807053583701, 0.005983070073873398773, 0.007975212340693213844 ),
 .UNSPECIFIED. ) ;
#43798 = PLANE ( 'NONE',  #44059 ) ;
#43799 = CARTESIAN_POINT ( 'NONE',  ( 21.23076943213705903, 18.64284798592824899, 32.03398753740996341 ) ) ;
#43800 = CARTESIAN_POINT ( 'NONE',  ( 87.47287999732215269, -39.05335706277111285, 189.8424516346250073 ) ) ;
#43801 = DIRECTION ( 'NONE',  ( 0.5735764363510470476, -0.8191520442889911324, 1.003171929053524007E-16 ) ) ;
#43802 = EDGE_CURVE ( 'NONE', #73449, #104380, #62670, .T. ) ;
#43803 = CARTESIAN_POINT ( 'NONE',  ( -7.188101187500000044, -22.90625000204838457, -8.802885111219163269E-16 ) ) ;
#43804 = CARTESIAN_POINT ( 'NONE',  ( -41.86369521826392059, 487.3376196552076181, 9.525433426952293559 ) ) ;
#43805 = MECHANICAL_DESIGN_GEOMETRIC_PRESENTATION_REPRESENTATION (  '', ( #90312 ), #55791 ) ;
#43806 = APPLICATION_CONTEXT ( 'automotive_design' ) ;
#43807 = CARTESIAN_POINT ( 'NONE',  ( 0.000000000000000000, 27.68727484027578356, 0.000000000000000000 ) ) ;
#43808 = B_SPLINE_CURVE_WITH_KNOTS ( 'NONE', 3,
 ( #62501, #88369, #21017, #71108, #102953, #30144, #53858, #79729, #86787, #95925, #12332, #45258, #37186, #95389, #22598, #21529, #54909, #14444, #87836, #71626, #70048, #45776, #29117, #47357, #80245, #6351, #54361, #39292, #72171, #64103, #31219, #90480, #57030, #65672, #64619, #89427, #74807, #66738, #40859, #48933, #57554, #98556, #48410, #106648 ),
 .UNSPECIFIED., .F., .F.,
 ( 4, 2, 2, 2, 2, 2, 2, 2, 2, 2, 2, 2, 2, 2, 2, 2, 2, 2, 2, 2, 2, 4 ),
 ( 0.000000000000000000, 0.002182755796778808495, 0.004365511593557616990, 0.008731023187115233980, 0.01746204637423055470, 0.02619306956134582684, 0.03492409274846109551, 0.05238613912269164674, 0.06984818549692217715, 0.08731023187115276307, 0.1047722782453833629, 0.1135033014324986628, 0.1222343246196139349, 0.1265998362131715849, 0.1309653478067292209, 0.1331481036035080667, 0.1353308594002868848, 0.1364222372986763077, 0.1375136151970657306, 0.1386049930954551257, 0.1391506820446498371, 0.1396963709938445486 ),
 .UNSPECIFIED. ) ;
#43809 = CARTESIAN_POINT ( 'NONE',  ( -7.500000000000000000, -4.330127018922200755, -7.564335161054497547 ) ) ;
#43810 = CIRCLE ( 'NONE', #79907, 66.50000000000000000 ) ;
#43811 = ORIENTED_EDGE ( 'NONE', *, *, #84778, .T. ) ;
#43812 = CARTESIAN_POINT ( 'NONE',  ( -35.88302647429859604, 490.8296403864111994, 12.39892816713287083 ) ) ;
#43813 = LINE ( 'NONE', #92352, #87482 ) ;
#43814 = CARTESIAN_POINT ( 'NONE',  ( -10.54230344465946168, 6.725510416460146246, -5.000000000000000888 ) ) ;
#43815 = EDGE_CURVE ( 'NONE', #10104, #2153, #58205, .T. ) ;
#43816 = DIRECTION ( 'NONE',  ( -1.000000000000000000, -1.224606353822377258E-16, -0.000000000000000000 ) ) ;
#43817 = EDGE_LOOP ( 'NONE', ( #48145, #47709, #30189, #8805 ) ) ;
#43818 = CARTESIAN_POINT ( 'NONE',  ( -7.923942441289230310, 51.78500681803757288, -3.904538598597388166 ) ) ;
#43819 = ORIENTED_EDGE ( 'NONE', *, *, #21411, .F. ) ;
#43820 = CARTESIAN_POINT ( 'NONE',  ( 43.00000000000000000, 488.0336798547363628, -0.8984331811833908832 ) ) ;
#43821 = CARTESIAN_POINT ( 'NONE',  ( -0.9432308977042356268, 12.66755915628530538, -49.67613533980958351 ) ) ;
#43822 = CARTESIAN_POINT ( 'NONE',  ( 9.918579450955565591, 101.2069608703131252, 1.297207292923863164 ) ) ;
#43823 = FILL_AREA_STYLE_COLOUR ( '', #16865 ) ;
#43824 = CARTESIAN_POINT ( 'NONE',  ( -107.2784424374574570, -59.99999999999998579, 196.7685047584830045 ) ) ;
#43825 = CARTESIAN_POINT ( 'NONE',  ( 17.50000000000003553, 49.99999999999769074, 59.56761335716116434 ) ) ;
#43826 = CARTESIAN_POINT ( 'NONE',  ( 19.00000000000001421, -4.999999999999999112, 25.00000000000000000 ) ) ;
#43827 =( NAMED_UNIT ( * ) SI_UNIT ( $, .STERADIAN. ) SOLID_ANGLE_UNIT ( ) );
#43828 = PRESENTATION_STYLE_ASSIGNMENT (( #61094 ) ) ;
#43829 = EDGE_CURVE ( 'NONE', #38464, #92662, #3088, .T. ) ;
#43830 = CARTESIAN_POINT ( 'NONE',  ( -85.62023293286473802, -28.60697929939942696, 178.8582336157557791 ) ) ;
#43831 = AXIS2_PLACEMENT_3D ( 'NONE', #32150, #39710, #97924 ) ;
#43832 = FILL_AREA_STYLE ('',( #77272 ) ) ;
#43833 = ORIENTED_EDGE ( 'NONE', *, *, #93261, .F. ) ;
#43834 = CARTESIAN_POINT ( 'NONE',  ( -9.040043340647605064, 46.05340506531722866, -14.03079106125278841 ) ) ;
#43835 = EDGE_CURVE ( 'NONE', #72660, #84500, #51257, .T. ) ;
#43836 = CARTESIAN_POINT ( 'NONE',  ( 3.841398122528158598, -1.072224703192209416, 104.5835869663332005 ) ) ;
#43837 = AXIS2_PLACEMENT_3D ( 'NONE', #25127, #49897, #57987 ) ;
#43838 = MECHANICAL_DESIGN_GEOMETRIC_PRESENTATION_REPRESENTATION (  '', ( #21473 ), #104124 ) ;
#43839 = CARTESIAN_POINT ( 'NONE',  ( -84.22133707121940915, -45.27027536912773797, -0.5858364418087087522 ) ) ;
#43840 = CARTESIAN_POINT ( 'NONE',  ( -5.136066607407661522, -12.96798121126441039, -7.569033233150490148 ) ) ;
#43841 = CARTESIAN_POINT ( 'NONE',  ( -15.39708646668728420, 44.03708262471037216, 5.599658763118309679 ) ) ;
#43842 = CARTESIAN_POINT ( 'NONE',  ( -15.46327711221947609, -5.286601841950839820, 14.04103132160307688 ) ) ;
#43843 = CARTESIAN_POINT ( 'NONE',  ( 27.42641407226152594, 36.49996279467831073, -10.02585437320845863 ) ) ;
#43844 = SURFACE_SIDE_STYLE ('',( #100483 ) ) ;
#43845 = EDGE_CURVE ( 'NONE', #64182, #57394, #79885, .T. ) ;
#43846 = CARTESIAN_POINT ( 'NONE',  ( 74.93436731647082638, -29.99999999999996803, 156.1785850212263824 ) ) ;
#43847 = FILL_AREA_STYLE_COLOUR ( '', #58341 ) ;
#43848 = CARTESIAN_POINT ( 'NONE',  ( -88.04114847129865495, -29.99999999999995026, -17.07571352811936194 ) ) ;
#43849 = CARTESIAN_POINT ( 'NONE',  ( -66.61405105253464853, -49.91421082191510550, 96.76620431498515984 ) ) ;
#43850 = VERTEX_POINT ( 'NONE', #13556 ) ;
#43851 = CARTESIAN_POINT ( 'NONE',  ( 92.04793376076307254, -60.00000000000014211, 204.8851669578057795 ) ) ;
#43852 = CARTESIAN_POINT ( 'NONE',  ( 20.52986868762305406, 40.83832388658744605, 61.74416104812828365 ) ) ;
#43853 = CARTESIAN_POINT ( 'NONE',  ( 79.00424233902616322, -57.67119432125786460, -30.74184640794639023 ) ) ;
#43854 = EDGE_CURVE ( 'NONE', #55070, #7738, #4419, .T. ) ;
#43855 = ORIENTED_EDGE ( 'NONE', *, *, #71469, .T. ) ;
#43856 = CARTESIAN_POINT ( 'NONE',  ( 8.239673527368280403, 51.94776582111974506, -1.561980839535718202 ) ) ;
#43857 = CARTESIAN_POINT ( 'NONE',  ( 2.977408999572650927, -28.25000000204838813, -7.188101187500000933 ) ) ;
#43858 = CARTESIAN_POINT ( 'NONE',  ( -4.466912950640278268E-14, -7.505553499465147382, -0.7999999999999977129 ) ) ;
#43859 = ORIENTED_EDGE ( 'NONE', *, *, #52159, .F. ) ;
#43860 =( LENGTH_UNIT ( ) NAMED_UNIT ( * ) SI_UNIT ( .MILLI., .METRE. ) );
#43861 = ORIENTED_EDGE ( 'NONE', *, *, #57990, .F. ) ;
#43862 = CARTESIAN_POINT ( 'NONE',  ( 9.258863595255466095, 41.99999999999999289, -70.74260034492780846 ) ) ;
#43863 = DIRECTION ( 'NONE',  ( -0.000000000000000000, -1.000000000000000000, -0.000000000000000000 ) ) ;
#43864 = CARTESIAN_POINT ( 'NONE',  ( -72.62418736021129462, -60.00000000002444978, 181.5552947579788849 ) ) ;
#43865 = FACE_OUTER_BOUND ( 'NONE', #44253, .T. ) ;
#43866 = CARTESIAN_POINT ( 'NONE',  ( -2.977408999572650039, -11.18750000204838457, -7.188101187500001821 ) ) ;
#43867 = CARTESIAN_POINT ( 'NONE',  ( -48.49405853457024307, 15.66070211563346959, 14.43943585503378202 ) ) ;
#43868 = FACE_OUTER_BOUND ( 'NONE', #38807, .T. ) ;
#43869 = CARTESIAN_POINT ( 'NONE',  ( 0.000000000000000000, -1.200000000000000030E-05, 9.000000000000000000 ) ) ;
#43870 = VECTOR ( 'NONE', #48375, 1000.000000000000000 ) ;
#43871 = DIRECTION ( 'NONE',  ( 0.000000000000000000, -1.000000000000000000, 0.000000000000000000 ) ) ;
#43872 = FILL_AREA_STYLE ('',( #10952 ) ) ;
#43873 = ORIENTED_EDGE ( 'NONE', *, *, #33139, .T. ) ;
#43874 = CARTESIAN_POINT ( 'NONE',  ( 4.999999999999993783, -4.000000000000003553, 103.2791840072761858 ) ) ;
#43876 = CARTESIAN_POINT ( 'NONE',  ( 32.98111995772554650, -53.36881808543628836, 36.89039439871834247 ) ) ;
#43875 = CARTESIAN_POINT ( 'NONE',  ( 23.86650669486618881, -3.999999999999998224, 0.000000000000000000 ) ) ;
#43877 = ORIENTED_EDGE ( 'NONE', *, *, #105401, .F. ) ;
#43878 = DIRECTION ( 'NONE',  ( -0.000000000000000000, -1.000000000000000000, -0.000000000000000000 ) ) ;
#43879 = ORIENTED_EDGE ( 'NONE', *, *, #2132, .F. ) ;
#43881 =( NAMED_UNIT ( * ) SI_UNIT ( $, .STERADIAN. ) SOLID_ANGLE_UNIT ( ) );
#43880 = DIRECTION ( 'NONE',  ( -1.000000000000000000, 0.000000000000000000, 0.000000000000000000 ) ) ;
#43882 = CYLINDRICAL_SURFACE ( 'NONE', #104309, 10.00000000000000178 ) ;
#43883 = CARTESIAN_POINT ( 'NONE',  ( -1.469576158976823947E-15, -23.56250000409677270, 8.000000000000000000 ) ) ;
#43884 = AXIS2_PLACEMENT_3D ( 'NONE', #33028, #6582, #31955 ) ;
#43885 = STYLED_ITEM ( 'NONE', ( #87106 ), #55887 ) ;
#43886 = DIRECTION ( 'NONE',  ( 0.5735764363510490460, 0.8191520442889896891, 0.000000000000000000 ) ) ;
#43887 = CIRCLE ( 'NONE', #52503, 5.000000000000002665 ) ;
#43888 = DIRECTION ( 'NONE',  ( -1.000000000000000000, -1.224606353822377258E-16, -0.000000000000000000 ) ) ;
#43889 =( NAMED_UNIT ( * ) PLANE_ANGLE_UNIT ( ) SI_UNIT ( $, .RADIAN. ) );
#43890 = EDGE_LOOP ( 'NONE', ( #1304, #14528 ) ) ;
#43891 = CARTESIAN_POINT ( 'NONE',  ( 92.57516331644632146, -60.00000000000002132, -2.390279356456004756 ) ) ;
#43892 = DIRECTION ( 'NONE',  ( 1.000000000000000000, 0.000000000000000000, 0.000000000000000000 ) ) ;
#43893 = AXIS2_PLACEMENT_3D ( 'NONE', #17178, #106689, #84024 ) ;
#43894 = SURFACE_SIDE_STYLE ('',( #61707 ) ) ;
#43895 = CARTESIAN_POINT ( 'NONE',  ( 32.62734573162120455, 485.2399387473994352, 2.793905986278862663 ) ) ;
#43896 = CONICAL_SURFACE ( 'NONE', #47351, 3.309500000000007880, 0.9599310885968770357 ) ;
#43897 =( BOUNDED_SURFACE ( )  B_SPLINE_SURFACE ( 3, 2, ( 
 ( #58913, #17928, #19020 ),
 ( #91807, #8745, #41653 ),
 ( #10858, #25509, #67536 ),
 ( #50781, #75610, #74008 ) ),
 .UNSPECIFIED., .F., .F., .T. ) 
 B_SPLINE_SURFACE_WITH_KNOTS ( ( 4, 4 ),
 ( 3, 3 ),
 ( 3.469446951953614189E-18, 0.001998086366859867617 ),
 ( 0.000000000000000000, 1.000000000000000000 ),
 .UNSPECIFIED. ) 
 GEOMETRIC_REPRESENTATION_ITEM ( )  RATIONAL_B_SPLINE_SURFACE ( (
 ( 1.000000000000000000, 0.8258027051679468489, 1.000000000000000000),
 ( 1.000000000000000000, 0.8176579674346097226, 1.000000000000000000),
 ( 1.000000000000000000, 0.8085378326700221052, 1.000000000000000000),
 ( 1.000000000000000000, 0.7996726260853451729, 1.000000000000000000) ) ) 
 REPRESENTATION_ITEM ( '' )  SURFACE ( )  );
#43898 = CARTESIAN_POINT ( 'NONE',  ( -6.200186772461218965, 41.06054036581593891, -71.07396401990634160 ) ) ;
#43899 = CARTESIAN_POINT ( 'NONE',  ( 5.523799489093671039E-15, 23.58303312036771615, 45.10524579772351217 ) ) ;
#43900 = VERTEX_POINT ( 'NONE', #13019 ) ;
#43901 = EDGE_CURVE ( 'NONE', #3104, #58075, #67851, .T. ) ;
#43902 = CARTESIAN_POINT ( 'NONE',  ( -109.0742547107064269, -29.99999999999665334, 182.6719831179964331 ) ) ;
#43903 = ORIENTED_EDGE ( 'NONE', *, *, #863, .F. ) ;
#43904 = DIRECTION ( 'NONE',  ( -1.000000000000000000, -0.000000000000000000, -0.000000000000000000 ) ) ;
#43905 = CARTESIAN_POINT ( 'NONE',  ( 5.819846122303833802, -4.937269551422769354, -4.448398286272978730 ) ) ;
#43906 = CARTESIAN_POINT ( 'NONE',  ( -16.66923479943752540, 34.27251685716380791, -24.30698433968595396 ) ) ;
#43907 = CARTESIAN_POINT ( 'NONE',  ( 17.50000000000000711, 2.500000000000000444, 0.000000000000000000 ) ) ;
#43908 = CARTESIAN_POINT ( 'NONE',  ( 85.58715377439223460, -52.75714875827612360, -10.05349147758953698 ) ) ;
#43909 = CARTESIAN_POINT ( 'NONE',  ( -31.79966957013667539, 310.8780264347615230, -8.126197538413364896 ) ) ;
#43910 = FACE_OUTER_BOUND ( 'NONE', #6763, .T. ) ;
#43912 = ADVANCED_FACE ( 'NONE', ( #71270 ), #24704, .F. ) ;
#43911 = CARTESIAN_POINT ( 'NONE',  ( -17.97116198174659729, 34.27731494407649393, 23.34421261274562909 ) ) ;
#43913 = DIRECTION ( 'NONE',  ( 0.000000000000000000, 0.000000000000000000, -1.000000000000000000 ) ) ;
#43914 = ORIENTED_EDGE ( 'NONE', *, *, #48765, .T. ) ;
#43915 = CARTESIAN_POINT ( 'NONE',  ( -6.499999999999999112, 2.759383090079003065, -5.880088986489996117 ) ) ;
#43916 = VERTEX_POINT ( 'NONE', #6522 ) ;
#43917 = CARTESIAN_POINT ( 'NONE',  ( 48.98802391561655867, 7.953645742799005269, -16.40821160912129173 ) ) ;
#43918 = DIRECTION ( 'NONE',  ( 0.000000000000000000, 1.224646799147353207E-16, 1.000000000000000000 ) ) ;
#43920 = EDGE_LOOP ( 'NONE', ( #6352, #20955, #91857, #28227 ) ) ;
#43919 = CARTESIAN_POINT ( 'NONE',  ( 5.689392408559237779, 51.96560585840138202, 6.093956388208072283 ) ) ;
#43921 = CARTESIAN_POINT ( 'NONE',  ( 77.26947396445019933, -25.60795510370099137, 119.8375088053420257 ) ) ;
#43922 = ORIENTED_EDGE ( 'NONE', *, *, #27844, .F. ) ;
#43923 = CARTESIAN_POINT ( 'NONE',  ( 1.601898381236912305, -53.94709533814469182, 40.91400580830796230 ) ) ;
#43924 = FACE_OUTER_BOUND ( 'NONE', #26985, .T. ) ;
#43925 = CARTESIAN_POINT ( 'NONE',  ( -7.188101187500000933, -27.50000000204838457, -2.977408999572651371 ) ) ;
#43926 = CIRCLE ( 'NONE', #104185, 14.00000000000000178 ) ;
#43927 = CARTESIAN_POINT ( 'NONE',  ( -86.45135651325685444, -57.58031178088597812, 202.9040356603995008 ) ) ;
#43928 = EDGE_CURVE ( 'NONE', #40703, #77091, #32367, .T. ) ;
#43929 = PRODUCT_DEFINITION_FORMATION_WITH_SPECIFIED_SOURCE ( 'ANY', '', #104487, .NOT_KNOWN. ) ;
#43930 = ORIENTED_EDGE ( 'NONE', *, *, #50420, .F. ) ;
#43931 =( LENGTH_UNIT ( ) NAMED_UNIT ( * ) SI_UNIT ( .MILLI., .METRE. ) );
#43932 = CARTESIAN_POINT ( 'NONE',  ( -34.54697356181507217, 42.66571874608613513, -63.00576358640330454 ) ) ;
#43933 = CARTESIAN_POINT ( 'NONE',  ( 102.7636524767473674, -37.84830847812925469, 174.7740013299970485 ) ) ;
#43934 = DIRECTION ( 'NONE',  ( 0.000000000000000000, -1.000000000000000000, 0.000000000000000000 ) ) ;
#43935 = CARTESIAN_POINT ( 'NONE',  ( 13.58349330513380160, 4.898587196589405926E-16, -4.000000000000001776 ) ) ;
#43936 = EDGE_CURVE ( 'NONE', #13329, #7841, #41031, .T. ) ;
#43937 = CARTESIAN_POINT ( 'NONE',  ( -3.313708498984760720, -16.71875000409677270, -8.000000000000000000 ) ) ;
#43938 = CARTESIAN_POINT ( 'NONE',  ( -51.38767806049178688, -29.89936270055883938, 48.97532232888291759 ) ) ;
#43939 = DIRECTION ( 'NONE',  ( 0.5735764363510466035, -0.8191520442889914655, 1.003171929053524500E-16 ) ) ;
#43940 = FACE_OUTER_BOUND ( 'NONE', #101336, .T. ) ;
#43941 =( NAMED_UNIT ( * ) PLANE_ANGLE_UNIT ( ) SI_UNIT ( $, .RADIAN. ) );
#43942 = LINE ( 'NONE', #68772, #84397 ) ;
#43943 = DIRECTION ( 'NONE',  ( 0.000000000000000000, 0.000000000000000000, 1.000000000000000000 ) ) ;
#43944 = DIRECTION ( 'NONE',  ( -0.1957247465660222063, 0.4045265792283474493, 0.8933364821160492131 ) ) ;
#43945 = VERTEX_POINT ( 'NONE', #31896 ) ;
#43946 = CARTESIAN_POINT ( 'NONE',  ( 0.000000000000000000, -30.00000000000000000, 0.000000000000000000 ) ) ;
#43947 = CARTESIAN_POINT ( 'NONE',  ( 11.66900197424181940, -4.900341487329494150, -12.56042530111529310 ) ) ;
#43948 = CARTESIAN_POINT ( 'NONE',  ( 19.83349330513380693, 1.593028355512270962E-15, 0.000000000000000000 ) ) ;
#43949 = CARTESIAN_POINT ( 'NONE',  ( -84.88742408119121308, -30.00000000000000000, 169.2579586347718532 ) ) ;
#43950 = EDGE_CURVE ( 'NONE', #23997, #93551, #84005, .T. ) ;
#43951 = EDGE_CURVE ( 'NONE', #79477, #76499, #65058, .T. ) ;
#43952 = CIRCLE ( 'NONE', #45718, 4.000000000000000888 ) ;
#43953 = ORIENTED_EDGE ( 'NONE', *, *, #87105, .F. ) ;
#43954 = PLANE ( 'NONE',  #75397 ) ;
#43955 = CARTESIAN_POINT ( 'NONE',  ( 75.55219586201926063, -57.55829115879463131, 192.1307904649139005 ) ) ;
#43956 = AXIS2_PLACEMENT_3D ( 'NONE', #77193, #60504, #88347 ) ;
#43958 = DIRECTION ( 'NONE',  ( -0.000000000000000000, -1.000000000000000000, -0.000000000000000000 ) ) ;
#43957 = CARTESIAN_POINT ( 'NONE',  ( -15.50569080112025588, 2.636008032210750862, -0.8338155181678262862 ) ) ;
#43959 = CARTESIAN_POINT ( 'NONE',  ( 48.67663294687506692, -35.26610979276345148, -36.36738862548124729 ) ) ;
#43960 = DIRECTION ( 'NONE',  ( -1.000000000000000000, -1.224606353822377258E-16, -0.000000000000000000 ) ) ;
#43961 = CARTESIAN_POINT ( 'NONE',  ( -43.45804985508113560, -60.00000000000002132, 57.68673898691244517 ) ) ;
#43962 = CIRCLE ( 'NONE', #76673, 4.000000000000000888 ) ;
#43963 = CIRCLE ( 'NONE', #28522, 3.400000000000000355 ) ;
#43964 = CIRCLE ( 'NONE', #104242, 4.000000000000001776 ) ;
#43965 = CARTESIAN_POINT ( 'NONE',  ( 5.957442974701732119, 48.00000000000000000, 65.00000000000000000 ) ) ;
#43966 = VECTOR ( 'NONE', #101847, 1000.000000000000114 ) ;
#43967 = CARTESIAN_POINT ( 'NONE',  ( -86.85197155073301190, -31.73829086694582458, 186.9893845558580381 ) ) ;
#43968 = ORIENTED_EDGE ( 'NONE', *, *, #59880, .T. ) ;
#43969 = LINE ( 'NONE', #85501, #503 ) ;
#43970 = CARTESIAN_POINT ( 'NONE',  ( -2.000864354225422748, -32.51271004180395607, 29.30614571473786256 ) ) ;
#43971 = VECTOR ( 'NONE', #44336, 1000.000000000000000 ) ;
#43972 = CARTESIAN_POINT ( 'NONE',  ( 0.000000000000000000, 0.000000000000000000, 0.000000000000000000 ) ) ;
#43973 = CARTESIAN_POINT ( 'NONE',  ( -41.61991840646690832, 463.6613340606643305, 18.05819007330882187 ) ) ;
#43974 = CARTESIAN_POINT ( 'NONE',  ( -42.62871025531358526, 365.8542140222418766, 17.21379826104702104 ) ) ;
#43975 = EDGE_CURVE ( 'NONE', #106075, #44079, #20477, .T. ) ;
#43976 = ORIENTED_EDGE ( 'NONE', *, *, #4983, .T. ) ;
#43977 = CARTESIAN_POINT ( 'NONE',  ( -36.69279669379599795, 378.7816022980671846, 4.949611917198358135 ) ) ;
#43978 = CARTESIAN_POINT ( 'NONE',  ( -1.469576158976823947E-15, -29.37499999999999645, 8.000000000000000000 ) ) ;
#43979 = CARTESIAN_POINT ( 'NONE',  ( -9.572623054141676135, -4.999999999999671374, -20.18584606598301434 ) ) ;
#43980 = CARTESIAN_POINT ( 'NONE',  ( -30.55414771718603717, 11.21328959333581388, -39.95065846502016882 ) ) ;
#43981 = CARTESIAN_POINT ( 'NONE',  ( 17.51664081523980698, 50.00000000000000000, 63.26386782005719311 ) ) ;
#43982 = FACE_OUTER_BOUND ( 'NONE', #30645, .T. ) ;
#43983 = ADVANCED_FACE ( 'NONE', ( #81999 ), #18592, .T. ) ;
#43984 = SURFACE_STYLE_USAGE ( .BOTH. , #94684 ) ;
#43985 = CARTESIAN_POINT ( 'NONE',  ( 89.06755727843562909, -14.21045842199420939, 44.45805076957166335 ) ) ;
#43986 = CARTESIAN_POINT ( 'NONE',  ( -83.77364050599970824, -22.14433376563224343, 150.6908921694812591 ) ) ;
#43987 = ORIENTED_EDGE ( 'NONE', *, *, #55688, .T. ) ;
#43988 = DIRECTION ( 'NONE',  ( 4.738110706560371839E-17, -0.9221233147934838614, 0.3868961001538753219 ) ) ;
#43989 = CARTESIAN_POINT ( 'NONE',  ( 5.982126593009819970, 253.9733422789293229, 0.5333292889181895369 ) ) ;
#43990 = CARTESIAN_POINT ( 'NONE',  ( 28.89319199617951739, -57.68130367911507506, 44.69050114560476317 ) ) ;
#43991 = CARTESIAN_POINT ( 'NONE',  ( 26.08349330513380693, -4.000000000000000000, 4.898587196589415787E-16 ) ) ;
#43992 = CARTESIAN_POINT ( 'NONE',  ( 44.78819990628695535, 344.4780858062635502, 1.774547970702379684 ) ) ;
#43993 = DIRECTION ( 'NONE',  ( -0.000000000000000000, -0.000000000000000000, -1.000000000000000000 ) ) ;
#43994 = ORIENTED_EDGE ( 'NONE', *, *, #37360, .T. ) ;
#43995 = UNCERTAINTY_MEASURE_WITH_UNIT (LENGTH_MEASURE( 1.000000000000000082E-05 ), #79333, 'distance_accuracy_value', 'NONE');
#43996 = CARTESIAN_POINT ( 'NONE',  ( 4.959124542865535723, 54.27782660535947912, -6.063864958317412679 ) ) ;
#43997 = EDGE_CURVE ( 'NONE', #92662, #38464, #40966, .T. ) ;
#43998 = CARTESIAN_POINT ( 'NONE',  ( 31.32096926659178138, 438.4574200499464496, 22.73263893176079975 ) ) ;
#43999 = CARTESIAN_POINT ( 'NONE',  ( -2.977408999572650039, -30.68750000204839168, -7.188101187500001821 ) ) ;
#44000 = ORIENTED_EDGE ( 'NONE', *, *, #74454, .T. ) ;
#44001 = LINE ( 'NONE', #10030, #63812 ) ;
#44002 = AXIS2_PLACEMENT_3D ( 'NONE', #51359, #102039, #4412 ) ;
#44003 = DIRECTION ( 'NONE',  ( 1.000000000000000000, 0.000000000000000000, -0.000000000000000000 ) ) ;
#44004 = CARTESIAN_POINT ( 'NONE',  ( 6.762666758904207320, 41.72338998057573178, -70.10115389619511461 ) ) ;
#44005 = CARTESIAN_POINT ( 'NONE',  ( 22.66220480930525127, 50.00000000000000000, 59.06576954297840842 ) ) ;
#44006 = CARTESIAN_POINT ( 'NONE',  ( -3.313708498984760276, -18.03124999999999645, -8.000000000000000000 ) ) ;
#44007 = B_SPLINE_CURVE_WITH_KNOTS ( 'NONE', 3,
 ( #16552, #31180, #64065, #106615, #6857, #32765 ),
 .UNSPECIFIED., .F., .F.,
 ( 4, 2, 4 ),
 ( 0.4253311071485821881, 0.4347571321485946827, 0.4441831571486071217 ),
 .UNSPECIFIED. ) ;
#44008 = DIRECTION ( 'NONE',  ( -0.000000000000000000, 1.000000000000000000, -0.000000000000000000 ) ) ;
#44009 = ORIENTED_EDGE ( 'NONE', *, *, #62678, .F. ) ;
#44010 = CARTESIAN_POINT ( 'NONE',  ( 79.93009750732559837, -59.99999999999998579, -27.98265100805786787 ) ) ;
#44012 = CARTESIAN_POINT ( 'NONE',  ( 20.41555138587536788, -49.91487051538342001, 32.77847263903716879 ) ) ;
#44011 = CARTESIAN_POINT ( 'NONE',  ( -100.0713701506240767, -14.21045842199444209, 196.7486061734171585 ) ) ;
#44013 = CARTESIAN_POINT ( 'NONE',  ( 98.18081844100633759, 27.55047179872464724, 49.09040922050319722 ) ) ;
#44014 = CARTESIAN_POINT ( 'NONE',  ( -34.21665458544683247, -53.36932329917436846, 37.55107279959798205 ) ) ;
#44015 = UNCERTAINTY_MEASURE_WITH_UNIT (LENGTH_MEASURE( 1.000000000000000082E-05 ), #104759, 'distance_accuracy_value', 'NONE');
#44016 = ORIENTED_EDGE ( 'NONE', *, *, #88667, .F. ) ;
#44017 = DIRECTION ( 'NONE',  ( 0.000000000000000000, 1.000000000000000000, 0.000000000000000000 ) ) ;
#44018 = CARTESIAN_POINT ( 'NONE',  ( -43.61075255792442107, 434.4875743724463746, 10.88293886035986446 ) ) ;
#44019 = CARTESIAN_POINT ( 'NONE',  ( -13.90371668366488400, -57.59451832461709841, 25.34313603510888413 ) ) ;
#44020 = DIRECTION ( 'NONE',  ( -1.000000000000000000, -1.224606353822377258E-16, -0.000000000000000000 ) ) ;
#44021 = CARTESIAN_POINT ( 'NONE',  ( 7.743982712349851916, -61.53786985239262464, 2.020119794285911041 ) ) ;
#44022 = CARTESIAN_POINT ( 'NONE',  ( 12.37144696128342147, -4.000000000000003553, 20.44658103856077602 ) ) ;
#44023 = VERTEX_POINT ( 'NONE', #80409 ) ;
#44024 = CARTESIAN_POINT ( 'NONE',  ( -16.66949223230251675, 36.40081923159284827, -24.30698433968597172 ) ) ;
#44025 = ORIENTED_EDGE ( 'NONE', *, *, #40082, .F. ) ;
#44026 = AXIS2_PLACEMENT_3D ( 'NONE', #87606, #46598, #5607 ) ;
#44027 = CARTESIAN_POINT ( 'NONE',  ( 93.61383638276589636, -29.99999999999993960, 191.2346839720568710 ) ) ;
#44028 = CARTESIAN_POINT ( 'NONE',  ( -14.11595029532502643, 2.410436752314748521, -5.024000119269296682 ) ) ;
#44029 = UNCERTAINTY_MEASURE_WITH_UNIT (LENGTH_MEASURE( 1.000000000000000082E-05 ), #72237, 'distance_accuracy_value', 'NONE');
#44030 = DIRECTION ( 'NONE',  ( -1.000000000000000000, -0.000000000000000000, -0.000000000000000000 ) ) ;
#44031 = CARTESIAN_POINT ( 'NONE',  ( 80.76937127641447489, -30.00000000000000000, 10.56350537290334657 ) ) ;
#44032 = CARTESIAN_POINT ( 'NONE',  ( -30.47150538518798513, 326.6480560234095947, 15.53807219869773704 ) ) ;
#44033 = ORIENTED_EDGE ( 'NONE', *, *, #27606, .T. ) ;
#44034 = EDGE_CURVE ( 'NONE', #17532, #9879, #80947, .T. ) ;
#44035 = CONICAL_SURFACE ( 'NONE', #57785, 4.172000000000009479, 0.9599310885968813656 ) ;
#44036 = ORIENTED_EDGE ( 'NONE', *, *, #68691, .T. ) ;
#44037 = EDGE_LOOP ( 'NONE', ( #79241, #78522, #97662, #13434 ) ) ;
#44038 = CARTESIAN_POINT ( 'NONE',  ( -47.77500202626900005, 12.17856325595019307, -14.37326074422667332 ) ) ;
#44039 = CARTESIAN_POINT ( 'NONE',  ( -11.57605499558394513, 303.6016347804044244, 9.883825704079463037 ) ) ;
#44040 = VECTOR ( 'NONE', #3965, 1000.000000000000114 ) ;
#44041 = CARTESIAN_POINT ( 'NONE',  ( 39.33363774397094659, 438.9614164243666323, 23.36187085933288543 ) ) ;
#44042 = CARTESIAN_POINT ( 'NONE',  ( -17.39035180332607666, 43.47171372390574362, -4.392436222999140938 ) ) ;
#44043 = DIRECTION ( 'NONE',  ( -1.000000000000000000, -0.000000000000000000, -0.000000000000000000 ) ) ;
#44045 = EDGE_CURVE ( 'NONE', #60134, #1766, #54729, .T. ) ;
#44044 = SURFACE_STYLE_USAGE ( .BOTH. , #35998 ) ;
#44046 = ORIENTED_EDGE ( 'NONE', *, *, #11777, .T. ) ;
#44047 = CARTESIAN_POINT ( 'NONE',  ( -7.374560640988130800, 50.00000000000000000, -94.59600210748763516 ) ) ;
#44048 = EDGE_LOOP ( 'NONE', ( #97972, #96168, #23152, #92062, #5308 ) ) ;
#44049 = CARTESIAN_POINT ( 'NONE',  ( 71.09600594220485448, -38.32840958359373218, 140.6164948842156548 ) ) ;
#44050 = DIRECTION ( 'NONE',  ( 1.224646799147349509E-16, 0.000000000000000000, -1.000000000000000000 ) ) ;
#44051 = AXIS2_PLACEMENT_3D ( 'NONE', #42274, #100514, #41748 ) ;
#44052 = CARTESIAN_POINT ( 'NONE',  ( 25.48181057333568944, 295.7987491915667420, 2.140656098138366659 ) ) ;
#44053 = VECTOR ( 'NONE', #9080, 1000.000000000000114 ) ;
#44054 = CIRCLE ( 'NONE', #14761, 12.00000000000001066 ) ;
#44055 = CARTESIAN_POINT ( 'NONE',  ( -5.982126593009819082, 246.0266577210706203, 0.5333292889181968643 ) ) ;
#44056 = B_SPLINE_CURVE_WITH_KNOTS ( 'NONE', 3,
 ( #78374, #102660, #4494, #28818 ),
 .UNSPECIFIED., .F., .F.,
 ( 4, 4 ),
 ( 0.000000000000000000, 1.000000000000000000 ),
 .UNSPECIFIED. ) ;
#44057 = VERTEX_POINT ( 'NONE', #66908 ) ;
#44058 = DIRECTION ( 'NONE',  ( -1.000000000000000000, -0.000000000000000000, -0.000000000000000000 ) ) ;
#44059 = AXIS2_PLACEMENT_3D ( 'NONE', #76693, #90767, #82667 ) ;
#44060 = DIRECTION ( 'NONE',  ( -1.000000000000000000, 0.000000000000000000, 0.000000000000000000 ) ) ;
#44061 = CARTESIAN_POINT ( 'NONE',  ( 39.63516261196253510, 316.6154150605056543, 7.211374874840607241 ) ) ;
#44062 = CARTESIAN_POINT ( 'NONE',  ( 0.000000000000000000, -46.00000000000000000, 123.0000000000000142 ) ) ;
#44063 = EDGE_CURVE ( 'NONE', #105730, #23524, #59893, .T. ) ;
#44064 = ORIENTED_EDGE ( 'NONE', *, *, #63460, .F. ) ;
#44065 = B_SPLINE_CURVE_WITH_KNOTS ( 'NONE', 3,
 ( #38358, #88483, #29230, #21132, #21646, #87952 ),
 .UNSPECIFIED., .F., .F.,
 ( 4, 2, 4 ),
 ( 2.380733003144885302E-07, 0.001898835937927388943, 0.003797433802554463656 ),
 .UNSPECIFIED. ) ;
#44067 = CARTESIAN_POINT ( 'NONE',  ( 30.00000000000000000, 0.000000000000000000, 0.000000000000000000 ) ) ;
#44066 =( NAMED_UNIT ( * ) SI_UNIT ( $, .STERADIAN. ) SOLID_ANGLE_UNIT ( ) );
#44068 = DIRECTION ( 'NONE',  ( 0.000000000000000000, 0.000000000000000000, 1.000000000000000000 ) ) ;
#44069 = DIRECTION ( 'NONE',  ( -0.1270361284032274773, -0.9918980905719693153, 0.000000000000000000 ) ) ;
#44070 = PLANE ( 'NONE',  #78302 ) ;
#44071 = CARTESIAN_POINT ( 'NONE',  ( 4.024410228089478458, 294.8082131651069631, 1.927919447182780077 ) ) ;
#44072 = SHAPE_REPRESENTATION ( 'hex screw gradec_din_DIN EN 24018 - M10 x 40-WS', ( #10728 ), #54068 ) ;
#44073 = EDGE_CURVE ( 'NONE', #23116, #33590, #43537, .T. ) ;
#44074 = CARTESIAN_POINT ( 'NONE',  ( 42.74851244753489254, 465.8913837062017365, 12.61547527226834653 ) ) ;
#44075 = CARTESIAN_POINT ( 'NONE',  ( 9.907626560209529032, 15.45483377860037244, 1.400881274228120477 ) ) ;
#44076 = CARTESIAN_POINT ( 'NONE',  ( 85.80726315722955633, -39.24464598724059528, 186.3863758982486729 ) ) ;
#44077 = CARTESIAN_POINT ( 'NONE',  ( 0.000000000000000000, -30.00000000000000000, 8.000000000000000000 ) ) ;
#44078 = CARTESIAN_POINT ( 'NONE',  ( -4.072633637071363388, 138.0955724161418061, 4.999999999999997335 ) ) ;
#44079 = VERTEX_POINT ( 'NONE', #34572 ) ;
#44080 = CARTESIAN_POINT ( 'NONE',  ( 74.80548469941292922, -57.67118132480599968, -32.73163803306931641 ) ) ;
#44081 = CARTESIAN_POINT ( 'NONE',  ( 42.20625837426413085, -25.53023488050030210, -29.84183546610569593 ) ) ;
#44082 = DIRECTION ( 'NONE',  ( 0.000000000000000000, 1.000000000000000000, 0.000000000000000000 ) ) ;
#44083 = CARTESIAN_POINT ( 'NONE',  ( -7.500000000000000000, -4.330127018922201643, -7.422398894150036064 ) ) ;
#44084 = CARTESIAN_POINT ( 'NONE',  ( 5.000000000000000000, -13.99270448171187375, 11.59586337663402489 ) ) ;
#44085 = STYLED_ITEM ( 'NONE', ( #91191 ), #99636 ) ;
#44086 = CARTESIAN_POINT ( 'NONE',  ( -86.45485542442474980, -30.00000000000000000, 67.08978895544929344 ) ) ;
#44087 = B_SPLINE_CURVE_WITH_KNOTS ( 'NONE', 3,
 ( #46814, #79711, #102934, #29100, #71091, #105577, #8476, #50000, #82369, #9003, #16037, #91016, #106637, #16576, #48918, #41380, #7403, #32786, #74271, #48396, #65660, #40316, #40843, #73737, #74795, #32243, #81812, #98542, #33314, #24693, #83431, #57541, #65123, #66186 ),
 .UNSPECIFIED., .F., .F.,
 ( 4, 2, 2, 2, 2, 2, 2, 2, 2, 2, 2, 2, 2, 2, 2, 2, 4 ),
 ( 0.01263889472610568374, 0.01342810546992895954, 0.01421731621375223534, 0.01500652695757551114, 0.01579573770139878694, 0.01658494844522206274, 0.01737415918904533854, 0.01816336993286861434, 0.01895258067669189361, 0.01974179142051516594, 0.02053100216433844522, 0.02132021290816171755, 0.02210942365198499682, 0.02289863439580827262, 0.02368784513963154842, 0.02447705588345482769, 0.02526626662727810002 ),
 .UNSPECIFIED. ) ;
#44088 = SURFACE_SIDE_STYLE ('',( #67304 ) ) ;
#44089 = CARTESIAN_POINT ( 'NONE',  ( 20.50185113829394012, -57.67216918497611999, 42.27920450415231102 ) ) ;
#44091 = FACE_OUTER_BOUND ( 'NONE', #76512, .T. ) ;
#44090 = DIRECTION ( 'NONE',  ( -0.000000000000000000, -1.000000000000000000, -0.000000000000000000 ) ) ;
#44092 = CARTESIAN_POINT ( 'NONE',  ( 1.723082057455612048, -53.92950373265724551, 40.90106102219755257 ) ) ;
#44093 = CARTESIAN_POINT ( 'NONE',  ( -33.08593021725691585, -32.09165124679379488, 32.96944937447516111 ) ) ;
#44094 = CARTESIAN_POINT ( 'NONE',  ( 40.43320803012314713, 490.2964122661032320, 11.44029694117896234 ) ) ;
#44095 = CARTESIAN_POINT ( 'NONE',  ( 7.468836275491999466, -3.123212597914878152, -19.53079664952245409 ) ) ;
#44096 = CARTESIAN_POINT ( 'NONE',  ( 0.000000000000000000, 49.50000000000000000, 60.50000000000000000 ) ) ;
#44097 = CARTESIAN_POINT ( 'NONE',  ( 21.54459453844334149, -19.00312104139907277, -33.51129274704846495 ) ) ;
#44098 =( GEOMETRIC_REPRESENTATION_CONTEXT ( 3 ) GLOBAL_UNCERTAINTY_ASSIGNED_CONTEXT ( ( #56966 ) ) GLOBAL_UNIT_ASSIGNED_CONTEXT ( ( #69042, #87747, #2141 ) ) REPRESENTATION_CONTEXT ( 'NONE', 'WORKASPACE' ) );
#44099 = CARTESIAN_POINT ( 'NONE',  ( -23.79206963583671097, -42.95898574611043585, 32.10571046793408811 ) ) ;
#44100 = ORIENTED_EDGE ( 'NONE', *, *, #67597, .F. ) ;
#44101 = CARTESIAN_POINT ( 'NONE',  ( 41.66301127302162399, 485.3863426732068547, -3.409513628943111385 ) ) ;
#44102 = CARTESIAN_POINT ( 'NONE',  ( -9.798380800342661345, 108.4680065431550275, -2.010350564680323249 ) ) ;
#44103 = CARTESIAN_POINT ( 'NONE',  ( -17.88331992309682761, -39.47666801934411041, 30.78506762338722069 ) ) ;
#44105 = CARTESIAN_POINT ( 'NONE',  ( 39.80046283020458731, 485.2148097320063584, -4.378247030186141586 ) ) ;
#44104 = DIRECTION ( 'NONE',  ( -1.000000000000000000, -0.000000000000000000, -0.000000000000000000 ) ) ;
#44106 = ADVANCED_FACE ( 'NONE', ( #18924 ), #75516, .T. ) ;
#44107 = ORIENTED_EDGE ( 'NONE', *, *, #67988, .T. ) ;
#44108 = CARTESIAN_POINT ( 'NONE',  ( 6.443810749341193578, -2.669419465171496419, -6.839891222013547711 ) ) ;
#44109 = ORIENTED_EDGE ( 'NONE', *, *, #28438, .T. ) ;
#44111 = AXIS2_PLACEMENT_3D ( 'NONE', #67676, #48935, #100559 ) ;
#44110 =( LENGTH_UNIT ( ) NAMED_UNIT ( * ) SI_UNIT ( .MILLI., .METRE. ) );
#44112 = EDGE_CURVE ( 'NONE', #2708, #23052, #35854, .T. ) ;
#44113 = CARTESIAN_POINT ( 'NONE',  ( 15.85122647056153333, 4.114663126756291867, 4.288211754877272242 ) ) ;
#44114 = AXIS2_PLACEMENT_3D ( 'NONE', #76935, #101742, #20889 ) ;
#44115 = DIRECTION ( 'NONE',  ( -1.000000000000000000, -1.224606353822377258E-16, -0.000000000000000000 ) ) ;
#44116 = ORIENTED_EDGE ( 'NONE', *, *, #39021, .F. ) ;
#44117 = DIRECTION ( 'NONE',  ( 0.000000000000000000, 0.000000000000000000, 1.000000000000000000 ) ) ;
#44118 = CONICAL_SURFACE ( 'NONE', #2763, 4.172000000000001485, 0.9599310885968750373 ) ;
#44119 = CARTESIAN_POINT ( 'NONE',  ( 1.469576158976823356E-15, 50.00000000000000000, -73.00000000000001421 ) ) ;
#44120 = MECHANICAL_DESIGN_GEOMETRIC_PRESENTATION_REPRESENTATION (  '', ( #57873 ), #94165 ) ;
#44121 = CARTESIAN_POINT ( 'NONE',  ( 101.0742260107603698, -37.84808717716843063, 188.0777966372289995 ) ) ;
#44122 = CIRCLE ( 'NONE', #1032, 3.309500000000007880 ) ;
#44123 = CARTESIAN_POINT ( 'NONE',  ( -6.928203230275508773, -10.00000000000000711, -4.000000000000000000 ) ) ;
#44124 = ORIENTED_EDGE ( 'NONE', *, *, #42810, .F. ) ;
#44125 = VECTOR ( 'NONE', #65293, 1000.000000000000000 ) ;
#44126 = ADVANCED_FACE ( 'NONE', ( #92764 ), #77150, .T. ) ;
#44127 = ORIENTED_EDGE ( 'NONE', *, *, #68360, .F. ) ;
#44128 = AXIS2_PLACEMENT_3D ( 'NONE', #70091, #62025, #102994 ) ;
#44129 = ORIENTED_EDGE ( 'NONE', *, *, #64251, .T. ) ;
#44130 = CARTESIAN_POINT ( 'NONE',  ( 24.36322103432850739, 306.6249039800414948, 9.333189539698471648 ) ) ;
#44131 = CARTESIAN_POINT ( 'NONE',  ( 25.11650669486618881, 1.474610560812782335E-15, 0.000000000000000000 ) ) ;
#44132 = SURFACE_SIDE_STYLE ('',( #93206 ) ) ;
#44133 = ORIENTED_EDGE ( 'NONE', *, *, #29269, .T. ) ;
#44134 = B_SPLINE_CURVE_WITH_KNOTS ( 'NONE', 3,
 ( #76634, #11355, #100382, #44285, #28135, #2204 ),
 .UNSPECIFIED., .F., .F.,
 ( 4, 2, 4 ),
 ( -4.604908131561810387E-06, 0.0003318387708518404111, 0.0006682824498352427003 ),
 .UNSPECIFIED. ) ;
#44135 = DIRECTION ( 'NONE',  ( 0.000000000000000000, -1.000000000000000000, 0.000000000000000000 ) ) ;
#44136 = CARTESIAN_POINT ( 'NONE',  ( -5.465597153059336577, 41.93635067907730019, -70.00903446595771129 ) ) ;
#44137 = CARTESIAN_POINT ( 'NONE',  ( -94.99329613063325439, -60.00000000000000000, -3.093086405557472496 ) ) ;
#44138 = CARTESIAN_POINT ( 'NONE',  ( 7.213352437320218691, -67.01836473007682571, -3.463014597543476736 ) ) ;
#44139 = CARTESIAN_POINT ( 'NONE',  ( -30.87955015324946828, 351.7733141111877444, 20.67482462247657082 ) ) ;
#44140 = CARTESIAN_POINT ( 'NONE',  ( 24.05868969682389036, -5.000000000000000000, 0.000000000000000000 ) ) ;
#44141 = CARTESIAN_POINT ( 'NONE',  ( -80.19882167783929106, -30.00000000000005684, -24.77908391697505053 ) ) ;
#44142 = CARTESIAN_POINT ( 'NONE',  ( -48.40568706220404493, -60.28780075344402434, 54.82589591225594461 ) ) ;
#44143 = ORIENTED_EDGE ( 'NONE', *, *, #51641, .F. ) ;
#44144 = CARTESIAN_POINT ( 'NONE',  ( 9.833493305133801599, 1.593028355512270567E-15, 0.000000000000000000 ) ) ;
#44145 = EDGE_LOOP ( 'NONE', ( #28301, #69668 ) ) ;
#44146 = FACE_OUTER_BOUND ( 'NONE', #98193, .T. ) ;
#44147 = DIRECTION ( 'NONE',  ( 0.000000000000000000, -1.000000000000000000, 0.000000000000000000 ) ) ;
#44148 = CARTESIAN_POINT ( 'NONE',  ( 5.647817967127100047, -6.548735934712071050, -2.038183545141170061 ) ) ;
#44150 = EDGE_LOOP ( 'NONE', ( #105427, #9113 ) ) ;
#44149 = AXIS2_PLACEMENT_3D ( 'NONE', #41858, #10025, #49410 ) ;
#44151 = CARTESIAN_POINT ( 'NONE',  ( 4.472135954999577834, 249.7267009648735439, -4.000000000000003553 ) ) ;
#44152 = CARTESIAN_POINT ( 'NONE',  ( 64.82975887493691403, -38.33849854337827878, 111.7912813277601032 ) ) ;
#44153 = CARTESIAN_POINT ( 'NONE',  ( 49.19747204248938743, 12.91412732281176545, 16.05397513442666479 ) ) ;
#44154 = CARTESIAN_POINT ( 'NONE',  ( 3.460324465709686326, -48.83451908470932779, 104.5902739980971461 ) ) ;
#44155 = CARTESIAN_POINT ( 'NONE',  ( -1.000000000000000222, -5.000000000000000000, -14.14213562373095101 ) ) ;
#44156 = CIRCLE ( 'NONE', #14876, 5.000000000000011546 ) ;
#44157 = CARTESIAN_POINT ( 'NONE',  ( 30.67950393665801556, 18.64316884713159794, -23.57730434125293328 ) ) ;
#44158 = CARTESIAN_POINT ( 'NONE',  ( 88.54308360411496892, -30.00000000000001066, 187.9651850611236341 ) ) ;
#44159 = CARTESIAN_POINT ( 'NONE',  ( 43.81051912592808151, 434.3294622498374906, 12.62549197245584764 ) ) ;
#44160 = DIRECTION ( 'NONE',  ( 0.000000000000000000, -1.000000000000000000, 0.000000000000000000 ) ) ;
#44161 = EDGE_CURVE ( 'NONE', #57904, #102866, #16882, .T. ) ;
#44162 = ORIENTED_EDGE ( 'NONE', *, *, #22955, .T. ) ;
#44163 = ORIENTED_EDGE ( 'NONE', *, *, #101544, .T. ) ;
#44164 = CARTESIAN_POINT ( 'NONE',  ( 53.91603561383729470, -49.90521162105653730, 62.12114408794506204 ) ) ;
#44165 = CARTESIAN_POINT ( 'NONE',  ( 71.63333333333333997, 6.915964383211875250E-15, 0.000000000000000000 ) ) ;
#44166 = CARTESIAN_POINT ( 'NONE',  ( -7.500000000000007105, 40.00000000000000000, -62.89165061483231511 ) ) ;
#44167 = EDGE_CURVE ( 'NONE', #91513, #12793, #58275, .T. ) ;
#44168 = EDGE_CURVE ( 'NONE', #8963, #88625, #35931, .T. ) ;
#44169 = EDGE_LOOP ( 'NONE', ( #36120, #75096, #43861, #96894 ) ) ;
#44170 = CARTESIAN_POINT ( 'NONE',  ( -84.49786633764185240, -38.35845268396171548, -23.28952271651921890 ) ) ;
#44171 = ORIENTED_EDGE ( 'NONE', *, *, #21996, .F. ) ;
#44172 = FACE_OUTER_BOUND ( 'NONE', #9910, .T. ) ;
#44173 = CARTESIAN_POINT ( 'NONE',  ( 110.3737722850151073, -38.35605049689843327, 158.9517897806462656 ) ) ;
#44174 = CARTESIAN_POINT ( 'NONE',  ( 11.41053004416664862, 18.22558145230713578, 8.550477479386900725 ) ) ;
#44175 = CARTESIAN_POINT ( 'NONE',  ( 82.46918239245667337, -37.86090144012435843, 8.727031703878875391 ) ) ;
#44176 = CARTESIAN_POINT ( 'NONE',  ( 32.18156226254668439, 336.4576599714083613, 18.02643260092943933 ) ) ;
#44177 = CARTESIAN_POINT ( 'NONE',  ( -23.74341347023494109, 305.6141507394339669, -8.835825535111036189 ) ) ;
#44178 = CARTESIAN_POINT ( 'NONE',  ( 3.964214964212477099, -12.08915882607781001, -10.21564873357027281 ) ) ;
#44179 = DIRECTION ( 'NONE',  ( 1.000000000000000000, 0.000000000000000000, 0.000000000000000000 ) ) ;
#44180 = CIRCLE ( 'NONE', #28734, 4.000000000000000888 ) ;
#44181 = DIRECTION ( 'NONE',  ( 0.3420201433256622736, 1.150791560227853228E-16, 0.9396926207859106484 ) ) ;
#44182 = CARTESIAN_POINT ( 'NONE',  ( 2.849086893377218654, 70.33581626579710644, 5.000000000000000000 ) ) ;
#44183 = VERTEX_POINT ( 'NONE', #51768 ) ;
#44184 = CARTESIAN_POINT ( 'NONE',  ( 1.220343922963510463, 36.63129049403877957, 28.81469345036448004 ) ) ;
#44185 = CONICAL_SURFACE ( 'NONE', #20126, 4.250000000000000000, 0.9599310885968754814 ) ;
#44186 = ADVANCED_FACE ( 'NONE', ( #91715 ), #50178, .F. ) ;
#44187 = CARTESIAN_POINT ( 'NONE',  ( 7.499935202740302564, 40.55407105531765666, -69.64903775193384661 ) ) ;
#44188 = DIRECTION ( 'NONE',  ( 0.000000000000000000, -1.000000000000000000, 0.000000000000000000 ) ) ;
#44189 = VERTEX_POINT ( 'NONE', #97525 ) ;
#44190 = CARTESIAN_POINT ( 'NONE',  ( -35.18278326935743650, 355.7732856895711961, 2.568028608958709658 ) ) ;
#44191 = CARTESIAN_POINT ( 'NONE',  ( -40.67306599853077387, 323.5699801759080287, 8.940364875572813119 ) ) ;
#44192 = DIRECTION ( 'NONE',  ( 0.000000000000000000, -1.000000000000000000, 0.000000000000000000 ) ) ;
#44193 = CARTESIAN_POINT ( 'NONE',  ( 105.5353273971932140, 1.030564683017419500E-14, 0.000000000000000000 ) ) ;
#44194 = CARTESIAN_POINT ( 'NONE',  ( 4.898587196589412829E-16, -18.12499999999999645, -8.000000000000000000 ) ) ;
#44195 = STYLED_ITEM ( 'NONE', ( #80956 ), #25413 ) ;
#44196 = SURFACE_STYLE_USAGE ( .BOTH. , #10737 ) ;
#44197 = CIRCLE ( 'NONE', #23517, 8.542937654374686218 ) ;
#44198 = FACE_OUTER_BOUND ( 'NONE', #59668, .T. ) ;
#44199 = AXIS2_PLACEMENT_3D ( 'NONE', #60587, #27171, #92386 ) ;
#44200 = EDGE_LOOP ( 'NONE', ( #98757, #58971, #75188, #58165, #80006, #3166 ) ) ;
#44201 = CARTESIAN_POINT ( 'NONE',  ( 82.83931105584079546, -57.25424869743982725, 188.0379144665223521 ) ) ;
#44202 = EDGE_CURVE ( 'NONE', #4022, #84731, #29020, .T. ) ;
#44203 = DIRECTION ( 'NONE',  ( 8.673617379884035472E-17, 0.000000000000000000, 1.000000000000000000 ) ) ;
#44204 = CARTESIAN_POINT ( 'NONE',  ( -15.89370886130902427, 45.88935169965961336, 6.420701231162380118 ) ) ;
#44205 = ORIENTED_EDGE ( 'NONE', *, *, #64471, .T. ) ;
#44206 = CARTESIAN_POINT ( 'NONE',  ( -92.71327091926096386, -45.26532570964787539, 87.13247471504898556 ) ) ;
#44207 = VECTOR ( 'NONE', #37347, 1000.000000000000000 ) ;
#44208 = CARTESIAN_POINT ( 'NONE',  ( 8.831401106173728977, -5.000000000000002665, -94.83329464149440469 ) ) ;
#44209 = DIRECTION ( 'NONE',  ( 0.000000000000000000, -1.000000000000000000, 0.000000000000000000 ) ) ;
#44210 = CONICAL_SURFACE ( 'NONE', #101007, 8.000000000000007105, 0.7853981633974509435 ) ;
#44211 = CARTESIAN_POINT ( 'NONE',  ( -35.95030584110901373, -31.65002092866515326, -37.80030597103479550 ) ) ;
#44212 = PRESENTATION_STYLE_ASSIGNMENT (( #27534 ) ) ;
#44213 = CARTESIAN_POINT ( 'NONE',  ( 36.43960955224464016, -60.00000000000000000, 47.79037295421704812 ) ) ;
#44214 = CARTESIAN_POINT ( 'NONE',  ( 31.26640680753876111, -33.27990713294830272, 41.34742143513260970 ) ) ;
#44215 = CARTESIAN_POINT ( 'NONE',  ( 29.62811787866498037, -21.49980114393428821, 32.08485897227100736 ) ) ;
#44217 = CARTESIAN_POINT ( 'NONE',  ( -11.40730658230364192, 14.19993524424377007, 9.944788788907292343 ) ) ;
#44216 = CARTESIAN_POINT ( 'NONE',  ( 34.36770714279217032, 436.8600252229026069, 5.946269065013446209 ) ) ;
#44218 = CARTESIAN_POINT ( 'NONE',  ( 8.233767125201939763, 295.9462895464749863, -10.03054565981218715 ) ) ;
#44219 = CARTESIAN_POINT ( 'NONE',  ( 32.16694665535142406, 298.7751107022914425, -9.134474995491629556 ) ) ;
#44220 = CARTESIAN_POINT ( 'NONE',  ( 41.10204028993562986, 320.7705685081051001, 4.305717556370822763 ) ) ;
#44221 = CARTESIAN_POINT ( 'NONE',  ( 6.445370176742730273, 7.262437273741188193, -1.101027156350174341 ) ) ;
#44222 = ORIENTED_EDGE ( 'NONE', *, *, #102203, .F. ) ;
#44223 = DIRECTION ( 'NONE',  ( -1.000000000000000000, -0.000000000000000000, -0.000000000000000000 ) ) ;
#44224 = AXIS2_PLACEMENT_3D ( 'NONE', #38447, #105281, #86995 ) ;
#44225 = CARTESIAN_POINT ( 'NONE',  ( -17.49999999999991473, 51.99987222567126111, 59.97465830877287374 ) ) ;
#44226 = ORIENTED_EDGE ( 'NONE', *, *, #82861, .T. ) ;
#44227 = SURFACE_STYLE_FILL_AREA ( #84681 ) ;
#44228 = DIRECTION ( 'NONE',  ( 0.000000000000000000, -1.000000000000000000, 0.000000000000000000 ) ) ;
#44229 = AXIS2_PLACEMENT_3D ( 'NONE', #68306, #34375, #101200 ) ;
#44230 = CARTESIAN_POINT ( 'NONE',  ( 39.83349330513380693, 1.593028355512270567E-15, 0.000000000000000000 ) ) ;
#44232 = CARTESIAN_POINT ( 'NONE',  ( -15.57536127888151078, -21.77027137267931778, -29.99990132288678879 ) ) ;
#44231 = CARTESIAN_POINT ( 'NONE',  ( 10.00005432054558696, 254.0001358013791446, 0.2621623937322634657 ) ) ;
#44233 = ADVANCED_FACE ( 'NONE', ( #48970 ), #7450, .F. ) ;
#44234 = ORIENTED_EDGE ( 'NONE', *, *, #15609, .F. ) ;
#44235 = CARTESIAN_POINT ( 'NONE',  ( 9.819056950928633398, 294.6481068335447731, 1.893705519456528208 ) ) ;
#44236 = DIRECTION ( 'NONE',  ( 0.000000000000000000, -1.000000000000000000, 0.000000000000000000 ) ) ;
#44237 = ORIENTED_EDGE ( 'NONE', *, *, #47995, .T. ) ;
#44238 = ADVANCED_FACE ( 'NONE', ( #98597 ), #71994, .T. ) ;
#44239 = DIRECTION ( 'NONE',  ( 0.000000000000000000, 0.000000000000000000, -1.000000000000000000 ) ) ;
#44240 = EDGE_CURVE ( 'NONE', #66028, #63078, #14477, .T. ) ;
#44241 = CARTESIAN_POINT ( 'NONE',  ( 30.77208753046679846, 10.36816855262256887, -40.23037088889287105 ) ) ;
#44242 = SURFACE_STYLE_FILL_AREA ( #11852 ) ;
#44243 = CARTESIAN_POINT ( 'NONE',  ( -91.97819797305179179, -59.99999999999999289, 6.679364944045982355 ) ) ;
#44244 = CARTESIAN_POINT ( 'NONE',  ( -8.000000000000001776, -11.65624999999999289, 3.313708498984759387 ) ) ;
#44245 = CONICAL_SURFACE ( 'NONE', #94136, 3.309500000000001663, 0.9599310885968770357 ) ;
#44246 = CARTESIAN_POINT ( 'NONE',  ( -33.65541652956997609, 435.5971107367176955, 8.976813231754876554 ) ) ;
#44247 = CARTESIAN_POINT ( 'NONE',  ( -84.01518071232440832, -32.49904627238863952, 168.3571053931298707 ) ) ;
#44248 = ORIENTED_EDGE ( 'NONE', *, *, #33603, .T. ) ;
#44249 = CARTESIAN_POINT ( 'NONE',  ( -44.17836536378434431, 435.2619773020556408, 14.65562696767813833 ) ) ;
#44250 = EDGE_CURVE ( 'NONE', #67548, #32377, #65138, .T. ) ;
#44251 = ORIENTED_EDGE ( 'NONE', *, *, #106551, .F. ) ;
#44252 = ADVANCED_FACE ( 'NONE', ( #23688 ), #57724, .F. ) ;
#44253 = EDGE_LOOP ( 'NONE', ( #75954, #47022, #64271, #33283, #40680, #71414, #2295, #41981 ) ) ;
#44254 = DIRECTION ( 'NONE',  ( -1.000000000000000000, -0.000000000000000000, -0.000000000000000000 ) ) ;
#44255 = CARTESIAN_POINT ( 'NONE',  ( 12.76371622530481709, -5.000000000001442402, 12.10534828917873895 ) ) ;
#44256 = CARTESIAN_POINT ( 'NONE',  ( 42.51195073777421385, 462.6463319774611591, 3.762330311941330496 ) ) ;
#44257 = FACE_OUTER_BOUND ( 'NONE', #95448, .T. ) ;
#44258 = VERTEX_POINT ( 'NONE', #10128 ) ;
#44259 = FACE_OUTER_BOUND ( 'NONE', #102917, .T. ) ;
#44260 = CARTESIAN_POINT ( 'NONE',  ( -92.43439519788523739, -57.65869811958181401, -18.51275992931142156 ) ) ;
#44261 = CARTESIAN_POINT ( 'NONE',  ( -4.589357672516644726, -66.06206030977220678, -3.865585121226772447 ) ) ;
#44262 = CARTESIAN_POINT ( 'NONE',  ( 43.51084452654475143, 465.2903130129669762, 9.421687747984162087 ) ) ;
#44263 = VECTOR ( 'NONE', #38684, 1000.000000000000000 ) ;
#44264 = CARTESIAN_POINT ( 'NONE',  ( -9.381394091586566120, 102.9865039441838519, 3.465950112474256883 ) ) ;
#44265 = VECTOR ( 'NONE', #99540, 1000.000000000000000 ) ;
#44266 = CARTESIAN_POINT ( 'NONE',  ( -5.000000000000000000, -15.62228920881133298, 12.61250543006184088 ) ) ;
#44267 = CARTESIAN_POINT ( 'NONE',  ( 101.4322121444104852, -14.21045842199439235, 121.1820579999150738 ) ) ;
#44268 = CARTESIAN_POINT ( 'NONE',  ( -78.54456454054628978, -14.21045842199430709, 165.9065210845421348 ) ) ;
#44269 = CARTESIAN_POINT ( 'NONE',  ( -59.69793324311933702, -53.39077738384364125, 78.06283456996561654 ) ) ;
#44270 = ORIENTED_EDGE ( 'NONE', *, *, #15027, .F. ) ;
#44271 = DIRECTION ( 'NONE',  ( 0.000000000000000000, 0.000000000000000000, -1.000000000000000000 ) ) ;
#44273 = VERTEX_POINT ( 'NONE', #43562 ) ;
#44272 = AXIS2_PLACEMENT_3D ( 'NONE', #40899, #32832, #394 ) ;
#44274 = CARTESIAN_POINT ( 'NONE',  ( -101.9374456322503306, -37.82064644935130104, 184.3837810757028421 ) ) ;
#44275 = CIRCLE ( 'NONE', #104543, 4.000000000000007105 ) ;
#44276 = CARTESIAN_POINT ( 'NONE',  ( -6.544565951341991372, 51.40333703996573433, 7.404642427234960245 ) ) ;
#44277 = ORIENTED_EDGE ( 'NONE', *, *, #78057, .T. ) ;
#44278 = CARTESIAN_POINT ( 'NONE',  ( 19.49275996658308685, 49.99917725797203616, 60.06179185754866268 ) ) ;
#44279 = CARTESIAN_POINT ( 'NONE',  ( 77.17560814547307757, -38.35599394049779676, -28.07239321058808912 ) ) ;
#44280 = CARTESIAN_POINT ( 'NONE',  ( -3.459690225508090577, -1.108983740916333893, 104.5059395991341660 ) ) ;
#44281 = CARTESIAN_POINT ( 'NONE',  ( 2.977408999572651815, -13.81250000204838280, 7.188101187500000933 ) ) ;
#44282 = DIRECTION ( 'NONE',  ( -1.000000000000000000, -0.000000000000000000, -0.000000000000000000 ) ) ;
#44283 = CIRCLE ( 'NONE', #66677, 8.605212085995399107 ) ;
#44284 = CARTESIAN_POINT ( 'NONE',  ( -30.87955015324946828, 351.7733141111877444, 20.67482462247657082 ) ) ;
#44285 = CARTESIAN_POINT ( 'NONE',  ( -6.539196172010133701, 3.775406670193810932, -6.286444963328660762 ) ) ;
#44286 = CARTESIAN_POINT ( 'NONE',  ( -9.204916576609303291, 43.65482048207726251, -14.80499302221950764 ) ) ;
#44287 = DIRECTION ( 'NONE',  ( 0.000000000000000000, 1.000000000000000000, 0.000000000000000000 ) ) ;
#44288 = FACE_OUTER_BOUND ( 'NONE', #101234, .T. ) ;
#44289 = CARTESIAN_POINT ( 'NONE',  ( -31.63782486760322143, -39.49234467425171857, 33.75314959485503152 ) ) ;
#44290 = DIRECTION ( 'NONE',  ( 0.000000000000000000, -1.000000000000000000, 0.000000000000000000 ) ) ;
#44291 = CARTESIAN_POINT ( 'NONE',  ( 48.81385752790940558, -29.13600490472190074, 45.58993858115186271 ) ) ;
#44292 = CARTESIAN_POINT ( 'NONE',  ( 5.656854249492378806, -14.18749999999999112, 5.656854249492381470 ) ) ;
#44293 = CARTESIAN_POINT ( 'NONE',  ( -1.005743885764240231, 45.47705655343377629, 18.24665906407937754 ) ) ;
#44294 = EDGE_CURVE ( 'NONE', #80498, #7688, #20397, .T. ) ;
#44295 = CARTESIAN_POINT ( 'NONE',  ( -99.34640669332435436, -38.47270126492327336, 200.6976403403067479 ) ) ;
#44296 = EDGE_LOOP ( 'NONE', ( #7177, #55831, #71794, #7358 ) ) ;
#44298 = DIRECTION ( 'NONE',  ( 0.000000000000000000, -1.000000000000000000, 0.000000000000000000 ) ) ;
#44297 = CARTESIAN_POINT ( 'NONE',  ( 84.58503749160358609, -38.35848514516985119, -23.21063429474329354 ) ) ;
#44299 =( LENGTH_UNIT ( ) NAMED_UNIT ( * ) SI_UNIT ( .MILLI., .METRE. ) );
#44300 = CARTESIAN_POINT ( 'NONE',  ( -19.21945236286198266, 49.79349494036195267, 61.52156576933356291 ) ) ;
#44301 = CARTESIAN_POINT ( 'NONE',  ( -7.495924014863156515, 40.46140149715811418, -59.65192205970540584 ) ) ;
#44302 = CARTESIAN_POINT ( 'NONE',  ( 6.519736037359969316, 40.56016599668093647, -71.18560176916710702 ) ) ;
#44303 = CARTESIAN_POINT ( 'NONE',  ( 5.000000000000000000, -60.71953810597794643, 12.61250543007074931 ) ) ;
#44304 = CARTESIAN_POINT ( 'NONE',  ( 33.74587843296627199, 434.0087108331489958, 12.79530826050359060 ) ) ;
#44305 = TOROIDAL_SURFACE ( 'NONE', #2938, 8.499999999999992895, 0.5000000000000000000 ) ;
#44306 = CARTESIAN_POINT ( 'NONE',  ( 107.9765012271092246, -60.00000000000000711, 195.7039070726993941 ) ) ;
#44307 = CONICAL_SURFACE ( 'NONE', #106257, 3.309500000000001663, 0.9599310885968770357 ) ;
#44308 = CARTESIAN_POINT ( 'NONE',  ( 29.83349330513380693, 1.593028355512270962E-15, 0.000000000000000000 ) ) ;
#44309 = EDGE_CURVE ( 'NONE', #44023, #57615, #75926, .T. ) ;
#44310 = ORIENTED_EDGE ( 'NONE', *, *, #80846, .F. ) ;
#44311 =( LENGTH_UNIT ( ) NAMED_UNIT ( * ) SI_UNIT ( .MILLI., .METRE. ) );
#44312 = CARTESIAN_POINT ( 'NONE',  ( -80.89051708270336860, -30.00000000000003197, -12.18533877698737911 ) ) ;
#44313 = ORIENTED_EDGE ( 'NONE', *, *, #31886, .F. ) ;
#44315 = CARTESIAN_POINT ( 'NONE',  ( 5.328772475725927826, 26.78864416899411793, -45.33255757618040604 ) ) ;
#44314 = CARTESIAN_POINT ( 'NONE',  ( -50.62117180075144063, -38.33334720786235295, 69.96112571796641078 ) ) ;
#44316 = CARTESIAN_POINT ( 'NONE',  ( 45.99999999999998579, 437.8923892905293656, 12.67832064131795811 ) ) ;
#44317 = CARTESIAN_POINT ( 'NONE',  ( -7.999999999999998224, -2.999999999999999556, -1.047197551196598964 ) ) ;
#44318 = CARTESIAN_POINT ( 'NONE',  ( 9.165151389911679658, 30.00000000000000000, 4.000000000000000000 ) ) ;
#44319 = CARTESIAN_POINT ( 'NONE',  ( -5.082755093536326818, -11.09375000204838457, 5.082755093536325042 ) ) ;
#44320 = CARTESIAN_POINT ( 'NONE',  ( -7.374560640984191728, -5.000000000000002665, -75.40399789251388540 ) ) ;
#44321 = AXIS2_PLACEMENT_3D ( 'NONE', #51676, #27459, #86209 ) ;
#44322 = CARTESIAN_POINT ( 'NONE',  ( -3.313708498984803352, -11.65625000409677270, 7.999999999999960032 ) ) ;
#44323 = CIRCLE ( 'NONE', #27113, 8.000000000000000000 ) ;
#44325 = ORIENTED_EDGE ( 'NONE', *, *, #2893, .T. ) ;
#44324 = CARTESIAN_POINT ( 'NONE',  ( 3.840629472727446691E-14, -1.200000000000000030E-05, 28.50000000000000000 ) ) ;
#44326 = CARTESIAN_POINT ( 'NONE',  ( 80.67054414735359558, -60.44982962067441434, 181.0052678533708956 ) ) ;
#44327 = EDGE_CURVE ( 'NONE', #97567, #98741, #100201, .T. ) ;
#44328 = DIRECTION ( 'NONE',  ( 0.000000000000000000, -1.000000000000000000, 0.000000000000000000 ) ) ;
#44329 =( GEOMETRIC_REPRESENTATION_CONTEXT ( 3 ) GLOBAL_UNCERTAINTY_ASSIGNED_CONTEXT ( ( #101170 ) ) GLOBAL_UNIT_ASSIGNED_CONTEXT ( ( #4930, #103614, #30281 ) ) REPRESENTATION_CONTEXT ( 'NONE', 'WORKASPACE' ) );
#44330 = LINE ( 'NONE', #77224, #81550 ) ;
#44331 = ORIENTED_EDGE ( 'NONE', *, *, #22891, .F. ) ;
#44332 = CARTESIAN_POINT ( 'NONE',  ( -32.22503847990277848, 485.9064490506194147, 4.829857536089201098 ) ) ;
#44333 = CARTESIAN_POINT ( 'NONE',  ( 18.00630676350472115, 34.31621990238991060, 23.18203998712654368 ) ) ;
#44334 = CARTESIAN_POINT ( 'NONE',  ( 3.313708498984781592, -29.28124999999999645, 7.999999999999979572 ) ) ;
#44335 = DIRECTION ( 'NONE',  ( 0.000000000000000000, 0.000000000000000000, -1.000000000000000000 ) ) ;
#44336 = DIRECTION ( 'NONE',  ( -0.5735764363510494901, -0.8191520442889894671, 0.000000000000000000 ) ) ;
#44337 = CARTESIAN_POINT ( 'NONE',  ( 17.26626608613624114, 43.28465477507130288, 6.503894573084921582 ) ) ;
#44338 = SURFACE_SIDE_STYLE ('',( #76690 ) ) ;
#44339 = ORIENTED_EDGE ( 'NONE', *, *, #78201, .T. ) ;
#44340 = B_SPLINE_CURVE_WITH_KNOTS ( 'NONE', 3,
 ( #5606, #80544, #104841, #63336, #89721, #6663, #15821, #104292, #7713, #79495, #96753, #38531, #30442, #22360, #96231, #55204, #39590, #105369, #86896, #22167, #63141, #78771, #96040, #12969, #94993, #45894 ),
 .UNSPECIFIED., .F., .F.,
 ( 4, 2, 2, 2, 2, 2, 2, 2, 2, 2, 2, 2, 4 ),
 ( 0.002320533079692624519, 0.002572382410217119615, 0.002824231740741614712, 0.003076081071266110242, 0.003327930401790605338, 0.003831629062839588592, 0.004083478393364082387, 0.004335327723888575749, 0.005342725045986517970, 0.005594574376511001791, 0.005846423707035485612, 0.006098273037559968565, 0.006350122368084452386 ),
 .UNSPECIFIED. ) ;
#44341 = CARTESIAN_POINT ( 'NONE',  ( -80.83118878706208932, -29.99999999999999645, -12.37157226799604004 ) ) ;
#44342 = CARTESIAN_POINT ( 'NONE',  ( 0.000000000000000000, 0.000000000000000000, 0.000000000000000000 ) ) ;
#44343 = CARTESIAN_POINT ( 'NONE',  ( 87.46133420739155895, -42.73768625780829211, 190.5708321053066925 ) ) ;
#44344 = CARTESIAN_POINT ( 'NONE',  ( -43.00000000000000000, 436.0987441542287115, 7.567257455462727656 ) ) ;
#44345 = EDGE_CURVE ( 'NONE', #84701, #60656, #9580, .T. ) ;
#44346 = CARTESIAN_POINT ( 'NONE',  ( 2.977408999572651815, -25.43750000204838813, 7.188101187500000933 ) ) ;
#44347 = AXIS2_PLACEMENT_3D ( 'NONE', #62631, #12458, #85859 ) ;
#44348 = CIRCLE ( 'NONE', #23732, 15.00000000000000711 ) ;
#44349 = DIRECTION ( 'NONE',  ( -1.000000000000000000, -1.224606353822377258E-16, -0.000000000000000000 ) ) ;
#44350 = CIRCLE ( 'NONE', #101250, 5.000000000000001776 ) ;
#44351 = AXIS2_PLACEMENT_3D ( 'NONE', #55800, #89270, #80623 ) ;
#44352 = CYLINDRICAL_SURFACE ( 'NONE', #31050, 14.00000000000000000 ) ;
#44353 = FILL_AREA_STYLE_COLOUR ( '', #63277 ) ;
#44354 = VERTEX_POINT ( 'NONE', #34974 ) ;
#44355 = CARTESIAN_POINT ( 'NONE',  ( 42.19179521601841287, 485.4956273777429487, -3.824025998174274577 ) ) ;
#44356 = CARTESIAN_POINT ( 'NONE',  ( -5.902135779713443497, 4.635123429159628827, -5.000000000000000000 ) ) ;
#44357 = PRESENTATION_STYLE_ASSIGNMENT (( #3367 ) ) ;
#44358 = EDGE_LOOP ( 'NONE', ( #39865, #4724, #591, #94067 ) ) ;
#44359 = DIRECTION ( 'NONE',  ( -1.000000000000000000, 0.000000000000000000, 0.000000000000000000 ) ) ;
#44360 = CARTESIAN_POINT ( 'NONE',  ( -32.99999999999997868, 464.3970849722209095, 17.41240408234209269 ) ) ;
#44361 = ORIENTED_EDGE ( 'NONE', *, *, #71476, .F. ) ;
#44362 = CARTESIAN_POINT ( 'NONE',  ( 31.43208348565280374, 438.4707862388059993, 22.17802677910339781 ) ) ;
#44363 = B_SPLINE_CURVE_WITH_KNOTS ( 'NONE', 3,
 ( #85188, #103497, #102436, #35611, #19445, #28578 ),
 .UNSPECIFIED., .F., .F.,
 ( 4, 2, 4 ),
 ( 2.380733003134763523E-07, 0.001898835937927384606, 0.003797433802554455416 ),
 .UNSPECIFIED. ) ;
#44364 = FILL_AREA_STYLE_COLOUR ( '', #93177 ) ;
#44365 = AXIS2_PLACEMENT_3D ( 'NONE', #100802, #26961, #44179 ) ;
#44366 = CARTESIAN_POINT ( 'NONE',  ( -34.15310232806815094, 465.0579147271379838, 17.72315479633533997 ) ) ;
#44367 = CARTESIAN_POINT ( 'NONE',  ( 0.000000000000000000, -2.000000000000000000, 0.000000000000000000 ) ) ;
#44368 = CARTESIAN_POINT ( 'NONE',  ( -105.3254793209803779, -60.00000000000000000, 198.9436637240303298 ) ) ;
#44369 = CARTESIAN_POINT ( 'NONE',  ( 19.23735690889500916, 49.80931112121767512, 61.48632125443233321 ) ) ;
#44370 = CARTESIAN_POINT ( 'NONE',  ( 0.000000000000000000, -6.928203230275511437, -3.999999999999997335 ) ) ;
#44371 = SURFACE_STYLE_USAGE ( .BOTH. , #19073 ) ;
#44372 = DIRECTION ( 'NONE',  ( 0.000000000000000000, 0.000000000000000000, 1.000000000000000000 ) ) ;
#44373 = AXIS2_PLACEMENT_3D ( 'NONE', #76496, #18843, #44147 ) ;
#44374 = CARTESIAN_POINT ( 'NONE',  ( -82.83829789210793137, -57.26054315054904009, 188.0394631155682532 ) ) ;
#44375 = CARTESIAN_POINT ( 'NONE',  ( -4.958743871765130429, 54.27777375259184822, -6.064299819695584404 ) ) ;
#44376 = VECTOR ( 'NONE', #102230, 1000.000000000000000 ) ;
#44377 = ADVANCED_FACE ( 'NONE', ( #74844 ), #25283, .T. ) ;
#44378 = ORIENTED_EDGE ( 'NONE', *, *, #65307, .T. ) ;
#44379 = CARTESIAN_POINT ( 'NONE',  ( -10.12028333941253777, 45.42143084255511098, -15.39942097377737795 ) ) ;
#44380 = EDGE_CURVE ( 'NONE', #71627, #56853, #39294, .T. ) ;
#44381 = CARTESIAN_POINT ( 'NONE',  ( 3.355892750373846933, -0.9951980364987254024, 104.3125661743353447 ) ) ;
#44382 = CARTESIAN_POINT ( 'NONE',  ( -85.62477652849005949, -52.72148863023463150, -2.858541068345675118 ) ) ;
#44383 = CARTESIAN_POINT ( 'NONE',  ( -1.000000000000000000, -5.000000000000016875, -14.14213562373094746 ) ) ;
#44384 = SURFACE_STYLE_FILL_AREA ( #85371 ) ;
#44385 = CARTESIAN_POINT ( 'NONE',  ( 4.561000490391409201, 143.2211774994303255, -5.000000000000000888 ) ) ;
#44386 = CARTESIAN_POINT ( 'NONE',  ( -6.840078058529586613, -12.20617675668041890, 8.820020145246234122 ) ) ;
#44387 = CARTESIAN_POINT ( 'NONE',  ( -11.85444436800005263, 42.00000000000000000, 90.56128410203886858 ) ) ;
#44388 = CIRCLE ( 'NONE', #25402, 5.000000000000002665 ) ;
#44389 = CARTESIAN_POINT ( 'NONE',  ( 54.44934741818074286, -29.99999999999998224, 75.82777139632159447 ) ) ;
#44390 = CARTESIAN_POINT ( 'NONE',  ( -16.32074838266548156, 61.49999999999999289, 8.160374191332740779 ) ) ;
#44391 = CARTESIAN_POINT ( 'NONE',  ( -84.17958645690445962, -14.21045842199424314, -18.06708323581670328 ) ) ;
#44392 = CARTESIAN_POINT ( 'NONE',  ( -76.83671821405472713, -18.66161896678824661, 113.2210307655415704 ) ) ;
#44393 = EDGE_LOOP ( 'NONE', ( #62737, #40466, #72047, #62462, #56207, #50543 ) ) ;
#44394 = CARTESIAN_POINT ( 'NONE',  ( 82.63356161194110427, -60.00000000000014921, 201.7055385233423976 ) ) ;
#44395 = CARTESIAN_POINT ( 'NONE',  ( -60.44710093648797056, 40.83768557982805447, 24.08449874113471623 ) ) ;
#44396 = CARTESIAN_POINT ( 'NONE',  ( 36.45031898219243516, -60.00000000000000000, 51.27440833837025735 ) ) ;
#44397 = VERTEX_POINT ( 'NONE', #398 ) ;
#44398 = CARTESIAN_POINT ( 'NONE',  ( 13.76576316043658643, -57.17837160915925665, 29.55959131405483475 ) ) ;
#44399 = CARTESIAN_POINT ( 'NONE',  ( -7.188101187500002709, -23.18750000204838813, 2.977408999572647819 ) ) ;
#44400 = CARTESIAN_POINT ( 'NONE',  ( -6.287528586677907235E-14, 28.20649408426966431, -38.24999999999931077 ) ) ;
#44401 = ORIENTED_EDGE ( 'NONE', *, *, #71600, .T. ) ;
#44403 = CARTESIAN_POINT ( 'NONE',  ( -16.05785784214673484, 4.775831776474317891, -3.710403933782548513 ) ) ;
#44402 = MECHANICAL_DESIGN_GEOMETRIC_PRESENTATION_REPRESENTATION (  '', ( #11666 ), #32328 ) ;
#44404 = ORIENTED_EDGE ( 'NONE', *, *, #29410, .T. ) ;
#44405 = CARTESIAN_POINT ( 'NONE',  ( 0.000000000000000000, -1.500000000000000000, 0.000000000000000000 ) ) ;
#44406 = CYLINDRICAL_SURFACE ( 'NONE', #100534, 5.000000000000000888 ) ;
#44407 = CARTESIAN_POINT ( 'NONE',  ( -68.79622679644177197, -60.00000000000000000, -32.99527447484252463 ) ) ;
#44408 = CARTESIAN_POINT ( 'NONE',  ( 28.80071264762327843, 307.9646382554784054, -9.069769307751089471 ) ) ;
#44409 = CARTESIAN_POINT ( 'NONE',  ( 2.977408999572650927, -29.75000000204838813, -7.188101187500001821 ) ) ;
#44410 = CARTESIAN_POINT ( 'NONE',  ( -48.48308721883941530, 13.98293033111037964, 16.77185627386600686 ) ) ;
#44411 = CARTESIAN_POINT ( 'NONE',  ( 21.88880945939638778, -4.285714285714295357, -12.64023069600374427 ) ) ;
#44412 = DIRECTION ( 'NONE',  ( -1.000000000000000000, 0.000000000000000000, 0.000000000000000000 ) ) ;
#44413 = CARTESIAN_POINT ( 'NONE',  ( -11.99999999999999467, 50.00000000000000000, -86.57079632497432442 ) ) ;
#44414 = DIRECTION ( 'NONE',  ( -1.000000000000000000, -1.224606353822377258E-16, -0.000000000000000000 ) ) ;
#44415 = DIRECTION ( 'NONE',  ( 0.000000000000000000, 0.000000000000000000, -1.000000000000000000 ) ) ;
#44416 = VERTEX_POINT ( 'NONE', #52175 ) ;
#44417 = CARTESIAN_POINT ( 'NONE',  ( -7.439122753854266357, 41.00341855746702180, -68.91429205792265122 ) ) ;
#44418 = AXIS2_PLACEMENT_3D ( 'NONE', #35665, #20029, #68544 ) ;
#44420 = CARTESIAN_POINT ( 'NONE',  ( 31.88147913428488067, -32.54995012556515377, 32.57459458299680222 ) ) ;
#44419 = DIRECTION ( 'NONE',  ( -1.000000000000000000, -1.224606353822377258E-16, -0.000000000000000000 ) ) ;
#44421 = CARTESIAN_POINT ( 'NONE',  ( -15.50035291838927876, -4.285714285714916194, 20.16952962162167395 ) ) ;
#44422 = ORIENTED_EDGE ( 'NONE', *, *, #23994, .T. ) ;
#44423 = CARTESIAN_POINT ( 'NONE',  ( -23.21751746555235840, 25.25267828308461304, -33.20617127781177658 ) ) ;
#44424 = EDGE_CURVE ( 'NONE', #97178, #19223, #61712, .T. ) ;
#44426 = CARTESIAN_POINT ( 'NONE',  ( 7.004291983109769859, 40.56179000455576045, -71.01843131752761451 ) ) ;
#44425 = CARTESIAN_POINT ( 'NONE',  ( -26.78605409122936365, 34.59012538573716711, -10.02589350699965109 ) ) ;
#44427 = AXIS2_PLACEMENT_3D ( 'NONE', #66245, #14620, #58148 ) ;
#44428 = FACE_OUTER_BOUND ( 'NONE', #38760, .T. ) ;
#44429 = CARTESIAN_POINT ( 'NONE',  ( -34.47678062873981020, 437.1474145881089157, 5.468662283310369077 ) ) ;
#44430 = AXIS2_PLACEMENT_3D ( 'NONE', #28494, #36070, #19888 ) ;
#44431 = CARTESIAN_POINT ( 'NONE',  ( -9.500000000000000000, -5.000000000000000000, -36.97043916959987087 ) ) ;
#44432 = CARTESIAN_POINT ( 'NONE',  ( 1.592040838891563829E-15, 3.000000000000002665, 13.00000000000003730 ) ) ;
#44433 = FACE_OUTER_BOUND ( 'NONE', #69237, .T. ) ;
#44434 = ORIENTED_EDGE ( 'NONE', *, *, #76241, .F. ) ;
#44435 = CARTESIAN_POINT ( 'NONE',  ( 92.00410706449807208, -59.99999999999998579, 18.49124520143980632 ) ) ;
#44436 =( NAMED_UNIT ( * ) PLANE_ANGLE_UNIT ( ) SI_UNIT ( $, .RADIAN. ) );
#44437 = CARTESIAN_POINT ( 'NONE',  ( 33.85195725564124558, 465.2464970902059349, 17.18122764674278358 ) ) ;
#44438 = CARTESIAN_POINT ( 'NONE',  ( 13.58349330513380160, 1.593028355512270567E-15, 0.000000000000000000 ) ) ;
#44439 = CARTESIAN_POINT ( 'NONE',  ( -7.036764705882398552, 40.00000000007573675, -71.06385277390853616 ) ) ;
#44440 = CARTESIAN_POINT ( 'NONE',  ( -14.29190075645216318, 6.456385560668112866, -7.561819230143454362 ) ) ;
#44441 = EDGE_CURVE ( 'NONE', #93240, #1532, #12558, .T. ) ;
#44442 = ORIENTED_EDGE ( 'NONE', *, *, #14617, .T. ) ;
#44443 = AXIS2_PLACEMENT_3D ( 'NONE', #25964, #2686, #50176 ) ;
#44444 = CARTESIAN_POINT ( 'NONE',  ( -103.9606405686747053, -29.99999999999802824, 196.6005958887341194 ) ) ;
#44445 = VERTEX_POINT ( 'NONE', #44645 ) ;
#44446 = CARTESIAN_POINT ( 'NONE',  ( -9.215420734788352775, -54.26735268782334742, 23.11721482942554928 ) ) ;
#44447 = FACE_OUTER_BOUND ( 'NONE', #91662, .T. ) ;
#44448 = LINE ( 'NONE', #21789, #9171 ) ;
#44449 = CARTESIAN_POINT ( 'NONE',  ( 15.77996175643055565, 22.60291536983757155, 1.987376761556955307 ) ) ;
#44450 = CARTESIAN_POINT ( 'NONE',  ( 83.95844515931129592, -45.27844744688253087, -12.02577428134897808 ) ) ;
#44451 = CARTESIAN_POINT ( 'NONE',  ( 27.02022815836235026, 0.000000000000000000, 5.000000000000002665 ) ) ;
#44452 = DIRECTION ( 'NONE',  ( 0.000000000000000000, 0.000000000000000000, 1.000000000000000000 ) ) ;
#44453 = DIRECTION ( 'NONE',  ( 0.000000000000000000, 1.000000000000000000, 0.000000000000000000 ) ) ;
#44454 = ORIENTED_EDGE ( 'NONE', *, *, #78433, .F. ) ;
#44455 = CARTESIAN_POINT ( 'NONE',  ( -42.91610777303993274, 434.7038292576191338, 17.44089724611687231 ) ) ;
#44456 = EDGE_LOOP ( 'NONE', ( #31185, #64152 ) ) ;
#44457 = CARTESIAN_POINT ( 'NONE',  ( 49.07747248321130229, 8.835459238882958033, -14.91203737403161256 ) ) ;
#44458 = PRESENTATION_STYLE_ASSIGNMENT (( #68192 ) ) ;
#44460 = VERTEX_POINT ( 'NONE', #77529 ) ;
#44459 = CARTESIAN_POINT ( 'NONE',  ( 29.34999999999999787, 1.533819458162526451E-15, 0.000000000000000000 ) ) ;
#44461 = CARTESIAN_POINT ( 'NONE',  ( 75.47549834169566907, -46.43312234463159882, 127.8789400697300493 ) ) ;
#44462 = ADVANCED_FACE ( 'NONE', ( #102867 ), #17761, .F. ) ;
#44463 = VERTEX_POINT ( 'NONE', #78572 ) ;
#44464 = CARTESIAN_POINT ( 'NONE',  ( 3.010879515032809817, -49.46749084728875090, 44.29121189687241156 ) ) ;
#44465 = CARTESIAN_POINT ( 'NONE',  ( -7.188101187500002709, -18.31250000204838457, 2.977408999572647819 ) ) ;
#44466 = CARTESIAN_POINT ( 'NONE',  ( -76.22482491972903063, -57.54008153533397518, 193.6369246664269781 ) ) ;
#44467 = ADVANCED_FACE ( 'NONE', ( #37104 ), #98382, .T. ) ;
#44468 = ORIENTED_EDGE ( 'NONE', *, *, #20418, .F. ) ;
#44469 =( NAMED_UNIT ( * ) SI_UNIT ( $, .STERADIAN. ) SOLID_ANGLE_UNIT ( ) );
#44470 = CARTESIAN_POINT ( 'NONE',  ( 0.000000000000000000, -30.00000000000000000, 0.000000000000000000 ) ) ;
#44471 = AXIS2_PLACEMENT_3D ( 'NONE', #22762, #54539, #39982 ) ;
#44472 = DIRECTION ( 'NONE',  ( 0.000000000000000000, 1.000000000000000000, 0.000000000000000000 ) ) ;
#44473 = EDGE_CURVE ( 'NONE', #87774, #53571, #27311, .T. ) ;
#44474 = COLOUR_RGB ( '', 0.08235294, 0.09019608, 0.10196078) ;
#44475 = FACE_OUTER_BOUND ( 'NONE', #37685, .T. ) ;
#44477 = CARTESIAN_POINT ( 'NONE',  ( 48.15153125426022029, 16.50033784694704053, -14.35535821593549954 ) ) ;
#44476 = B_SPLINE_CURVE_WITH_KNOTS ( 'NONE', 3,
 ( #50179, #90113, #106275, #32438 ),
 .UNSPECIFIED., .F., .F.,
 ( 4, 4 ),
 ( 0.0009107969653496763478, 0.009022847091396625149 ),
 .UNSPECIFIED. ) ;
#44478 = CARTESIAN_POINT ( 'NONE',  ( -8.000000000000000000, -17.93750000409676915, -9.797174393178825657E-16 ) ) ;
#44479 = DIRECTION ( 'NONE',  ( 0.000000000000000000, 0.000000000000000000, 1.000000000000000000 ) ) ;
#44480 = DIRECTION ( 'NONE',  ( 0.000000000000000000, -0.8267102254942136907, -0.5626279437277412754 ) ) ;
#44481 = MECHANICAL_DESIGN_GEOMETRIC_PRESENTATION_REPRESENTATION (  '', ( #41002 ), #70266 ) ;
#44482 = DIRECTION ( 'NONE',  ( 0.000000000000000000, 0.000000000000000000, 1.000000000000000000 ) ) ;
#44483 = ADVANCED_FACE ( 'NONE', ( #8927 ), #19608, .T. ) ;
#44484 = CIRCLE ( 'NONE', #72043, 4.000000000000001776 ) ;
#44485 = CARTESIAN_POINT ( 'NONE',  ( 5.369174336198356379, 44.20122194677738037, -60.96850753999265748 ) ) ;
#44486 = CARTESIAN_POINT ( 'NONE',  ( 19.83349330513379982, 4.898587196589405926E-16, -4.000000000000001776 ) ) ;
#44488 = EDGE_CURVE ( 'NONE', #57881, #92046, #16955, .T. ) ;
#44487 = DIRECTION ( 'NONE',  ( 1.000000000000000000, 4.493451613005293727E-20, 6.938893903907228378E-18 ) ) ;
#44489 = DIRECTION ( 'NONE',  ( -1.000000000000000000, -1.224606353822377258E-16, -0.000000000000000000 ) ) ;
#44490 = ORIENTED_EDGE ( 'NONE', *, *, #74293, .F. ) ;
#44491 = CARTESIAN_POINT ( 'NONE',  ( -2.426529107808244490, -49.73926502898306268, 44.58451710260244738 ) ) ;
#44492 = CARTESIAN_POINT ( 'NONE',  ( 10.87128754221327931, -4.996251208102432173, -12.57223391742547314 ) ) ;
#44493 = CARTESIAN_POINT ( 'NONE',  ( 0.3602828126333169623, 7.865783509256337958, 51.69852333018035750 ) ) ;
#44494 = CARTESIAN_POINT ( 'NONE',  ( -69.26106847545361234, -30.21325109223555927, -30.03938730321735306 ) ) ;
#44495 = CARTESIAN_POINT ( 'NONE',  ( -87.75043898228696548, -30.00000000000000355, 186.1331779216796747 ) ) ;
#44496 = ORIENTED_EDGE ( 'NONE', *, *, #51112, .T. ) ;
#44497 = AXIS2_PLACEMENT_3D ( 'NONE', #7480, #74871, #40397 ) ;
#44498 = CARTESIAN_POINT ( 'NONE',  ( 17.33349330513380693, -4.000000000000000888, 4.898587196589416773E-16 ) ) ;
#44499 = CARTESIAN_POINT ( 'NONE',  ( 77.56900591926921607, -57.51690387631008861, 195.9563615345031451 ) ) ;
#44500 = CARTESIAN_POINT ( 'NONE',  ( 45.99999999995392130, 436.0345727780207881, 16.01583062800949264 ) ) ;
#44501 = COLOUR_RGB ( '', 0.40784314, 0.44705882, 0.49803922) ;
#44502 = CARTESIAN_POINT ( 'NONE',  ( 38.72114142554678295, -32.54403767304167161, -37.56696858966843422 ) ) ;
#44503 = LINE ( 'NONE', #95181, #27137 ) ;
#44504 = CARTESIAN_POINT ( 'NONE',  ( -69.23101163046497675, -60.00000000000000711, 137.2813101166285605 ) ) ;
#44505 = AXIS2_PLACEMENT_3D ( 'NONE', #42193, #67019, #33076 ) ;
#44506 = DIRECTION ( 'NONE',  ( 1.000000000000000000, -0.000000000000000000, 1.224646799147353207E-16 ) ) ;
#44507 = SURFACE_STYLE_USAGE ( .BOTH. , #84957 ) ;
#44508 = CARTESIAN_POINT ( 'NONE',  ( -85.27764252179795790, -57.47308612990543253, 192.4447815377685913 ) ) ;
#44509 = ORIENTED_EDGE ( 'NONE', *, *, #53562, .F. ) ;
#44510 = CARTESIAN_POINT ( 'NONE',  ( -42.23079339798735532, 460.7352525929354101, 2.726051457480703544 ) ) ;
#44511 = CARTESIAN_POINT ( 'NONE',  ( -4.074072711644582512, -46.43917196787263890, 31.62195155993591200 ) ) ;
#44512 = CARTESIAN_POINT ( 'NONE',  ( -7.150000055923752207, 41.64999994407625650, -59.82695526654634222 ) ) ;
#44513 = DIRECTION ( 'NONE',  ( 0.000000000000000000, -1.000000000000000000, 0.000000000000000000 ) ) ;
#44514 = CARTESIAN_POINT ( 'NONE',  ( 5.700000000000000178, 0.000000000000000000, 0.000000000000000000 ) ) ;
#44515 = ADVANCED_FACE ( 'NONE', ( #82289 ), #73753, .F. ) ;
#44516 = VERTEX_POINT ( 'NONE', #37902 ) ;
#44517 = CARTESIAN_POINT ( 'NONE',  ( -36.62035930702501929, 369.9849428499111923, 3.960109444795354872 ) ) ;
#44518 = DIRECTION ( 'NONE',  ( -0.000000000000000000, -0.000000000000000000, -1.000000000000000000 ) ) ;
#44519 = AXIS2_PLACEMENT_3D ( 'NONE', #64651, #105113, #106148 ) ;
#44520 = DIRECTION ( 'NONE',  ( 0.000000000000000000, 0.000000000000000000, 1.000000000000000000 ) ) ;
#44521 = CARTESIAN_POINT ( 'NONE',  ( -13.00000000000003730, -85.00000000000000000, 4.000000000000001776 ) ) ;
#44522 = ORIENTED_EDGE ( 'NONE', *, *, #86180, .F. ) ;
#44523 = CARTESIAN_POINT ( 'NONE',  ( 25.41720494684658149, 295.7426751966382312, -1.808613394343576930 ) ) ;
#44524 = EDGE_CURVE ( 'NONE', #27308, #56205, #2616, .T. ) ;
#44525 = CARTESIAN_POINT ( 'NONE',  ( 28.76346532419124458, 309.5219921958590135, -8.933260212751790164 ) ) ;
#44526 = DIRECTION ( 'NONE',  ( 0.000000000000000000, -1.000000000000000000, 0.000000000000000000 ) ) ;
#44527 = CARTESIAN_POINT ( 'NONE',  ( 8.099999999999999645, 3.752776749732562589, -6.500000000000000888 ) ) ;
#44528 = STYLED_ITEM ( 'NONE', ( #66838 ), #42772 ) ;
#44529 = CARTESIAN_POINT ( 'NONE',  ( 89.60175727050132366, -14.21045842199443143, 48.51353285324994147 ) ) ;
#44530 = CARTESIAN_POINT ( 'NONE',  ( -82.52651961324420427, -32.55781991263304320, 155.0962975578067642 ) ) ;
#44531 = VERTEX_POINT ( 'NONE', #86448 ) ;
#44532 = CARTESIAN_POINT ( 'NONE',  ( 42.63514723962018138, 485.0526260718772846, -1.920325882542133877 ) ) ;
#44533 = CARTESIAN_POINT ( 'NONE',  ( 5.382057749264600233, 252.9982679840394155, -2.659775980967101106 ) ) ;
#44534 = CARTESIAN_POINT ( 'NONE',  ( 4.154708322984330151E-08, -57.67120202538961138, 41.61186700422870643 ) ) ;
#44535 = CARTESIAN_POINT ( 'NONE',  ( -5.688070444779528501, -4.337726323027712994, -16.91120255684542784 ) ) ;
#44536 = CARTESIAN_POINT ( 'NONE',  ( 42.44170713277035389, 333.9443472539740014, 7.453073974849625749 ) ) ;
#44537 = CARTESIAN_POINT ( 'NONE',  ( 33.74742301870519157, 478.7271368655381707, 3.791462368787906989 ) ) ;
#44538 = ORIENTED_EDGE ( 'NONE', *, *, #39443, .F. ) ;
#44539 = LINE ( 'NONE', #45077, #51208 ) ;
#44540 = CARTESIAN_POINT ( 'NONE',  ( 0.000000000000000000, 0.000000000000000000, 0.000000000000000000 ) ) ;
#44541 = CARTESIAN_POINT ( 'NONE',  ( 2.977408999572651815, -23.93750000204838457, 7.188101187500000933 ) ) ;
#44542 = ORIENTED_EDGE ( 'NONE', *, *, #69410, .T. ) ;
#44543 = SURFACE_SIDE_STYLE ('',( #100631 ) ) ;
#44544 =( BOUNDED_SURFACE ( )  B_SPLINE_SURFACE ( 3, 2, ( 
 ( #64844, #71337, #30921 ),
 ( #47054, #63800, #96687 ),
 ( #7128, #88595, #23347 ),
 ( #40040, #14676, #31449 ) ),
 .UNSPECIFIED., .F., .F., .F. ) 
 B_SPLINE_SURFACE_WITH_KNOTS ( ( 4, 4 ),
 ( 3, 3 ),
 ( -5.212844045310305319E-16, 0.002123809863736959066 ),
 ( 0.000000000000000000, 1.000000000000000000 ),
 .UNSPECIFIED. ) 
 GEOMETRIC_REPRESENTATION_ITEM ( )  RATIONAL_B_SPLINE_SURFACE ( (
 ( 1.000000000000000000, 0.8347624811020261104, 1.000000000000000000),
 ( 1.000000000000000000, 0.8202629603800248859, 1.000000000000000000),
 ( 1.000000000000000000, 0.8052718258174417221, 1.000000000000000000),
 ( 1.000000000000000000, 0.7904469216846379265, 1.000000000000000000) ) ) 
 REPRESENTATION_ITEM ( '' )  SURFACE ( )  );
#44545 = CARTESIAN_POINT ( 'NONE',  ( 2.918503601030405736, 15.30040232763797903, 9.571198553003400278 ) ) ;
#44546 = CARTESIAN_POINT ( 'NONE',  ( 5.313748243244007519, 41.99394926078451107, -69.45901782876110531 ) ) ;
#44547 = EDGE_CURVE ( 'NONE', #79234, #39124, #30868, .T. ) ;
#44548 = CARTESIAN_POINT ( 'NONE',  ( -55.22048556080422799, 49.99999999999999289, 34.80214219305234025 ) ) ;
#44549 = DIRECTION ( 'NONE',  ( 0.5735764363510491570, -0.8191520442889895781, 1.003171929053522035E-16 ) ) ;
#44550 = B_SPLINE_CURVE_WITH_KNOTS ( 'NONE', 3,
 ( #54381, #96479, #4806, #104016, #37745, #14461, #30159, #13406, #86805, #70070, #79747, #86279, #22618, #55453, #46329, #95949, #12351, #38777 ),
 .UNSPECIFIED., .F., .F.,
 ( 4, 2, 2, 2, 2, 2, 2, 2, 4 ),
 ( 0.4999999999971661002, 0.5624999999975203169, 0.6249999999978745890, 0.6874999999982288612, 0.7499999999985831334, 0.8124999999989372945, 0.8749999999992915667, 0.9374999999996458389, 1.000000000000000000 ),
 .UNSPECIFIED. ) ;
#44552 = CYLINDRICAL_SURFACE ( 'NONE', #80479, 4.000000000000000000 ) ;
#44551 = CONICAL_SURFACE ( 'NONE', #70337, 3.309500000000001663, 0.9599310885968770357 ) ;
#44553 = VERTEX_POINT ( 'NONE', #103138 ) ;
#44554 = CARTESIAN_POINT ( 'NONE',  ( 82.32205428790078372, -60.00000000000002132, -26.51557028033280616 ) ) ;
#44556 = CARTESIAN_POINT ( 'NONE',  ( 23.46127647898429913, -32.51707366590390080, 30.27781536837194665 ) ) ;
#44555 = CARTESIAN_POINT ( 'NONE',  ( -71.62990520600911282, -30.00000000000002842, 135.6731032779996156 ) ) ;
#44557 = CARTESIAN_POINT ( 'NONE',  ( 122.4708123290697017, 1.499999999999992450, 61.23540616453489349 ) ) ;
#44558 =( GEOMETRIC_REPRESENTATION_CONTEXT ( 3 ) GLOBAL_UNCERTAINTY_ASSIGNED_CONTEXT ( ( #17901 ) ) GLOBAL_UNIT_ASSIGNED_CONTEXT ( ( #28830, #27764, #27225 ) ) REPRESENTATION_CONTEXT ( 'NONE', 'WORKASPACE' ) );
#44559 = CARTESIAN_POINT ( 'NONE',  ( -36.21398753213680521, -25.65888403626743752, 33.24715464751751171 ) ) ;
#44560 = EDGE_CURVE ( 'NONE', #37488, #84910, #18758, .T. ) ;
#44561 = UNCERTAINTY_MEASURE_WITH_UNIT (LENGTH_MEASURE( 1.000000000000000082E-05 ), #7305, 'distance_accuracy_value', 'NONE');
#44562 = ORIENTED_EDGE ( 'NONE', *, *, #29375, .F. ) ;
#44563 = CARTESIAN_POINT ( 'NONE',  ( 34.21200799993543740, 462.3300391847291166, 4.640346717380173125 ) ) ;
#44564 = CARTESIAN_POINT ( 'NONE',  ( -4.744389013293885071, -48.62707453416837211, 104.3204960233004357 ) ) ;
#44565 = CARTESIAN_POINT ( 'NONE',  ( -13.87389654945780215, -57.47116530957473657, 25.11216171227248850 ) ) ;
#44566 = COLOUR_RGB ( '', 0.09019608, 0.27058824, 0.51372549) ;
#44567 = CARTESIAN_POINT ( 'NONE',  ( 6.162888688655350222, -7.505553499465148271, 0.000000000000000000 ) ) ;
#44568 = CARTESIAN_POINT ( 'NONE',  ( 6.928203230275507885, -65.00000000000000000, 4.000000000000002665 ) ) ;
#44569 = DIRECTION ( 'NONE',  ( -1.000000000000000000, -0.000000000000000000, -0.000000000000000000 ) ) ;
#44570 = EDGE_LOOP ( 'NONE', ( #7220, #96438 ) ) ;
#44571 = ORIENTED_EDGE ( 'NONE', *, *, #17216, .T. ) ;
#44572 = CARTESIAN_POINT ( 'NONE',  ( 90.84406139033485772, -29.99999999999999289, 190.4162226198302790 ) ) ;
#44573 = CARTESIAN_POINT ( 'NONE',  ( 51.48757442383973881, 38.95383793068620548, -37.45149417477089315 ) ) ;
#44574 = CARTESIAN_POINT ( 'NONE',  ( -4.656390720430120034, -83.68353814039454619, 3.786082374785836535 ) ) ;
#44575 = CARTESIAN_POINT ( 'NONE',  ( 81.44514727150406941, -30.00000000000000711, -9.709585533065395069 ) ) ;
#44576 = CARTESIAN_POINT ( 'NONE',  ( -29.37670169769928208, 318.1281283369471566, 13.44543306026610097 ) ) ;
#44577 = ADVANCED_FACE ( 'NONE', ( #14096 ), #4973, .F. ) ;
#44578 = EDGE_LOOP ( 'NONE', ( #23510, #56690, #74718, #23056, #6265 ) ) ;
#44579 = ORIENTED_EDGE ( 'NONE', *, *, #32107, .T. ) ;
#44580 = VERTEX_POINT ( 'NONE', #103658 ) ;
#44581 = CARTESIAN_POINT ( 'NONE',  ( -46.78712017075140039, 13.65728975790554145, -15.44288672244362282 ) ) ;
#44582 =( NAMED_UNIT ( * ) SI_UNIT ( $, .STERADIAN. ) SOLID_ANGLE_UNIT ( ) );
#44583 = CARTESIAN_POINT ( 'NONE',  ( 22.33349330513380693, 1.593028355512270962E-15, 0.000000000000000000 ) ) ;
#44584 = AXIS2_PLACEMENT_3D ( 'NONE', #17998, #34736, #9875 ) ;
#44585 = CARTESIAN_POINT ( 'NONE',  ( 33.00000000000000000, 439.7597899781497972, 24.16317522621304192 ) ) ;
#44586 = CARTESIAN_POINT ( 'NONE',  ( -31.36093463545012838, 438.6317617946405676, 22.30207175520214591 ) ) ;
#44588 = CARTESIAN_POINT ( 'NONE',  ( 0.000000000000000000, 0.000000000000000000, 0.000000000000000000 ) ) ;
#44587 = AXIS2_PLACEMENT_3D ( 'NONE', #50527, #59725, #19311 ) ;
#44589 = CARTESIAN_POINT ( 'NONE',  ( 37.46929538836619855, 50.00000000000000000, -55.58823529426165067 ) ) ;
#44590 = ORIENTED_EDGE ( 'NONE', *, *, #86440, .T. ) ;
#44591 = CARTESIAN_POINT ( 'NONE',  ( 11.68767211932491712, 50.00000000000000000, -81.85902538600508649 ) ) ;
#44592 = ORIENTED_EDGE ( 'NONE', *, *, #78940, .T. ) ;
#44593 = CARTESIAN_POINT ( 'NONE',  ( -4.472135954999578722, -64.72922779932635251, 4.000000000000002665 ) ) ;
#44594 = CARTESIAN_POINT ( 'NONE',  ( 53.84901272430960972, -38.34088802725808875, 78.30668236027604223 ) ) ;
#44595 = CARTESIAN_POINT ( 'NONE',  ( 4.898587196589412829E-16, -10.81250000409677092, -8.000000000000000000 ) ) ;
#44596 = CARTESIAN_POINT ( 'NONE',  ( 28.52069848920484674, 297.0547176035682355, 2.417840208557171522 ) ) ;
#44597 = VECTOR ( 'NONE', #92209, 1000.000000000000114 ) ;
#44598 = DIRECTION ( 'NONE',  ( 0.5735764363510462704, 0.8191520442889915765, 0.000000000000000000 ) ) ;
#44599 = B_SPLINE_CURVE_WITH_KNOTS ( 'NONE', 3,
 ( #45472, #26654, #77297, #69221, #101031, #27730, #101571, #102089, #69739, #28249, #36872, #102633, #61671, #53019, #60076, #18548, #51412, #94561, #27186, #12014, #10422, #20712, #35267, #12537, #78344, #92940, #51940, #84854, #37933, #39501, #88047, #22799, #47029, #31428, #47561, #70268 ),
 .UNSPECIFIED., .F., .F.,
 ( 4, 2, 2, 2, 2, 2, 2, 2, 2, 2, 2, 2, 2, 2, 2, 2, 2, 4 ),
 ( 0.01291936762762758636, 0.01372441420841339493, 0.01452946078919920177, 0.01533450736998501034, 0.01613955395077081717, 0.01694460053155662574, 0.01774964711234243431, 0.01855469369312823941, 0.01935974027391405144, 0.02016478685469985654, 0.02096983343548566164, 0.02177488001627147368, 0.02257992659705727878, 0.02338497317784308735, 0.02419001975862889592, 0.02459254304902180194, 0.02499506633941470449, 0.02580011292020050959 ),
 .UNSPECIFIED. ) ;
#44600 = ORIENTED_EDGE ( 'NONE', *, *, #27926, .T. ) ;
#44601 = CARTESIAN_POINT ( 'NONE',  ( 29.14716730816274293, 13.65620768952807929, -39.72410719430394010 ) ) ;
#44602 = DIRECTION ( 'NONE',  ( 0.000000000000000000, -1.000000000000000000, 0.000000000000000000 ) ) ;
#44603 = FACE_OUTER_BOUND ( 'NONE', #51405, .T. ) ;
#44604 = CARTESIAN_POINT ( 'NONE',  ( -9.797611831518617365, 51.31153553680866253, 2.590295869752982316 ) ) ;
#44605 = ADVANCED_FACE ( 'NONE', ( #55088 ), #32525, .F. ) ;
#44606 = ORIENTED_EDGE ( 'NONE', *, *, #70487, .F. ) ;
#44607 = MECHANICAL_DESIGN_GEOMETRIC_PRESENTATION_REPRESENTATION (  '', ( #80673 ), #85883 ) ;
#44608 = FACE_OUTER_BOUND ( 'NONE', #79580, .T. ) ;
#44609 = CARTESIAN_POINT ( 'NONE',  ( -4.382959417677089853, -1.862050784382271784, 102.7400018439556817 ) ) ;
#44610 = CARTESIAN_POINT ( 'NONE',  ( 0.3483149870578539087, -8.861353789385034929, -7.493854785173817312 ) ) ;
#44611 = AXIS2_PLACEMENT_3D ( 'NONE', #98185, #56654, #90099 ) ;
#44612 = CARTESIAN_POINT ( 'NONE',  ( 19.96162532426519221, 302.8116070918645164, 9.928455558879853982 ) ) ;
#44613 = ADVANCED_FACE ( 'NONE', ( #38935 ), #94500, .T. ) ;
#44614 =( GEOMETRIC_REPRESENTATION_CONTEXT ( 3 ) GLOBAL_UNCERTAINTY_ASSIGNED_CONTEXT ( ( #83935 ) ) GLOBAL_UNIT_ASSIGNED_CONTEXT ( ( #104781, #78908, #62234 ) ) REPRESENTATION_CONTEXT ( 'NONE', 'WORKASPACE' ) );
#44615 = CARTESIAN_POINT ( 'NONE',  ( 43.02661387979727436, 465.7449615347604208, 11.43319743843670544 ) ) ;
#44616 = LINE ( 'NONE', #20916, #101888 ) ;
#44617 = CARTESIAN_POINT ( 'NONE',  ( 86.19842101853855354, -28.27713569860727816, 183.2257041085184710 ) ) ;
#44618 = AXIS2_PLACEMENT_3D ( 'NONE', #70410, #37009, #47169 ) ;
#44619 = DIRECTION ( 'NONE',  ( 0.000000000000000000, -1.000000000000000000, 0.000000000000000000 ) ) ;
#44620 = CARTESIAN_POINT ( 'NONE',  ( -8.340586800768058140, 120.4027948985844176, 1.270355564599584843E-12 ) ) ;
#44621 = ORIENTED_EDGE ( 'NONE', *, *, #53359, .F. ) ;
#44622 = EDGE_CURVE ( 'NONE', #96540, #15029, #105253, .T. ) ;
#44623 = EDGE_CURVE ( 'NONE', #40910, #35138, #63541, .T. ) ;
#44624 = SURFACE_STYLE_FILL_AREA ( #101258 ) ;
#44625 = CARTESIAN_POINT ( 'NONE',  ( -7.036764705882381676, 40.00000000007575807, -71.06385277390852195 ) ) ;
#44626 = CARTESIAN_POINT ( 'NONE',  ( 0.000000000000000000, 70.00000000000000000, 0.000000000000000000 ) ) ;
#44627 = CARTESIAN_POINT ( 'NONE',  ( -90.20890582660780410, -29.99999999999999289, 89.71514907472229083 ) ) ;
#44628 = AXIS2_PLACEMENT_3D ( 'NONE', #102017, #36280, #44328 ) ;
#44629 = CYLINDRICAL_SURFACE ( 'NONE', #45166, 4.000000000000000000 ) ;
#44630 = CARTESIAN_POINT ( 'NONE',  ( 17.63980495134517668, -57.67160087258927348, 41.95025224030491984 ) ) ;
#44631 = CLOSED_SHELL ( 'NONE', ( #32799, #52016, #18131, #67270, #23472, #101792, #40272, #61288, #8082, #9284, #100226, #51855, #78390, #35241, #38168, #5817, #29483, #66106, #44774, #99544, #80873, #55770, #105491, #54535, #61420, #13656, #17218, #69512, #46357, #47508, #50979, #45183, #29321, #86700, #95272, #44483, #43529, #12640, #40734, #85702, #33976, #79178, #25990, #79642, #7605, #28364, #41066, #20499, #205, #23974, #90878, #81053, #59293, #65971, #26207, #102887 ) ) ;
#44633 =( LENGTH_UNIT ( ) NAMED_UNIT ( * ) SI_UNIT ( .MILLI., .METRE. ) );
#44632 = DIRECTION ( 'NONE',  ( 0.000000000000000000, 1.000000000000000000, 0.000000000000000000 ) ) ;
#44634 = FILL_AREA_STYLE ('',( #51635 ) ) ;
#44635 = CARTESIAN_POINT ( 'NONE',  ( -43.80704950897089844, -36.52919196705796168, 41.55287977338722527 ) ) ;
#44636 = CARTESIAN_POINT ( 'NONE',  ( 41.32194754023684169, 489.6440166213181442, 10.86036015010091127 ) ) ;
#44637 = DIRECTION ( 'NONE',  ( 0.000000000000000000, -1.877893248421449036E-16, 1.000000000000000000 ) ) ;
#44638 = PRESENTATION_STYLE_ASSIGNMENT (( #52700 ) ) ;
#44640 = ADVANCED_FACE ( 'NONE', ( #87491 ), #104713, .F. ) ;
#44639 = CARTESIAN_POINT ( 'NONE',  ( 21.65227882671612747, -19.03527767991882058, -33.49607776825432381 ) ) ;
#44641 = CONICAL_SURFACE ( 'NONE', #43013, 5.000000000000000000, 0.9599310885968913576 ) ;
#44642 = SURFACE_SIDE_STYLE ('',( #46223 ) ) ;
#44643 = CARTESIAN_POINT ( 'NONE',  ( -25.57323824984261762, -25.56794925674672925, 29.49343980220939088 ) ) ;
#44644 = VERTEX_POINT ( 'NONE', #95575 ) ;
#44645 = CARTESIAN_POINT ( 'NONE',  ( 28.58349330513380337, 4.898587196589405926E-16, -4.000000000000001776 ) ) ;
#44646 = CARTESIAN_POINT ( 'NONE',  ( -9.948513602187995630, 108.8697794334385804, 1.045942665286139217 ) ) ;
#44647 = CARTESIAN_POINT ( 'NONE',  ( -19.82538544910368117, -25.55338363043042804, 28.62632469270730695 ) ) ;
#44649 = CARTESIAN_POINT ( 'NONE',  ( 39.04686241056654694, 485.1639993256666799, -4.285741954104417495 ) ) ;
#44648 = DIRECTION ( 'NONE',  ( 0.000000000000000000, -1.000000000000000000, 0.000000000000000000 ) ) ;
#44650 = EDGE_CURVE ( 'NONE', #72252, #98070, #30838, .T. ) ;
#44651 = ORIENTED_EDGE ( 'NONE', *, *, #4016, .F. ) ;
#44652 = CARTESIAN_POINT ( 'NONE',  ( 5.974109059515367193, -2.735160444454405759, -6.499999999999999112 ) ) ;
#44653 = ORIENTED_EDGE ( 'NONE', *, *, #90096, .T. ) ;
#44654 = FILL_AREA_STYLE ('',( #101288 ) ) ;
#44655 = COLOUR_RGB ( '', 0.72549020, 0.75294118, 0.79215686) ;
#44656 = ADVANCED_FACE ( 'NONE', ( #16768 ), #31910, .T. ) ;
#44657 = CARTESIAN_POINT ( 'NONE',  ( 15.90404091944966325, 3.516460376327609882, 2.884095128131958674 ) ) ;
#44658 = CARTESIAN_POINT ( 'NONE',  ( -8.528914935573171263, -60.00000000000000711, -42.47286814751166872 ) ) ;
#44659 = ORIENTED_EDGE ( 'NONE', *, *, #35012, .T. ) ;
#44660 = DIRECTION ( 'NONE',  ( -0.000000000000000000, 1.000000000000000000, 0.000000000000000000 ) ) ;
#44661 = CIRCLE ( 'NONE', #99763, 4.000000000000000888 ) ;
#44662 = CARTESIAN_POINT ( 'NONE',  ( 105.0707565437703579, -60.15135272885378015, 187.5576145010796836 ) ) ;
#44663 = CIRCLE ( 'NONE', #65352, 4.000000000000000888 ) ;
#44664 = CARTESIAN_POINT ( 'NONE',  ( -7.934203308536662114, -6.132996599822035044, 1.057099537198544326 ) ) ;
#44665 = ORIENTED_EDGE ( 'NONE', *, *, #33666, .F. ) ;
#44666 = ORIENTED_EDGE ( 'NONE', *, *, #94857, .F. ) ;
#44667 = VERTEX_POINT ( 'NONE', #25429 ) ;
#44668 = CARTESIAN_POINT ( 'NONE',  ( 24.20115299029716383, 306.5553735938593150, 10.31754309208164422 ) ) ;
#44669 = CARTESIAN_POINT ( 'NONE',  ( -39.71334445446657924, 460.7040462571920898, 2.103363390004036049 ) ) ;
#44670 = DIRECTION ( 'NONE',  ( -0.000000000000000000, 1.000000000000000000, -0.000000000000000000 ) ) ;
#44671 = ORIENTED_EDGE ( 'NONE', *, *, #33878, .F. ) ;
#44672 = EDGE_CURVE ( 'NONE', #69309, #74993, #15244, .T. ) ;
#44673 = CARTESIAN_POINT ( 'NONE',  ( 0.2595206531159274799, 2.531175536751827604, -6.499999999999999112 ) ) ;
#44674 = CARTESIAN_POINT ( 'NONE',  ( -6.639654777812401321, 41.83126063031291864, -69.93930137318731965 ) ) ;
#44675 = PRESENTATION_LAYER_ASSIGNMENT (  '', '', ( #32597 ) ) ;
#44676 = CARTESIAN_POINT ( 'NONE',  ( -94.55323015762245120, -59.99999999999268852, -13.46500496322361151 ) ) ;
#44677 = CARTESIAN_POINT ( 'NONE',  ( 7.999885325681428405, -68.99977065129940001, 0.2682325777720065973 ) ) ;
#44678 = CARTESIAN_POINT ( 'NONE',  ( 24.08356453790285201, -60.00000000000000000, 40.93464879651766353 ) ) ;
#44679 = CARTESIAN_POINT ( 'NONE',  ( 1.663454779225379987, -5.000000000000000000, 16.34235115354128709 ) ) ;
#44680 = CARTESIAN_POINT ( 'NONE',  ( -6.232496158895186156, 41.83455024993975968, -59.02481301687200244 ) ) ;
#44682 = CARTESIAN_POINT ( 'NONE',  ( 5.033794246690010965, -32.51032478759464794, 29.29834927723706883 ) ) ;
#44681 = CARTESIAN_POINT ( 'NONE',  ( -112.5893510171550105, -59.99999999999995026, 145.0943965991558002 ) ) ;
#44683 = SURFACE_SIDE_STYLE ('',( #67877 ) ) ;
#44684 = CARTESIAN_POINT ( 'NONE',  ( -48.64733360570842535, -42.98315368061135189, 49.69360454995861431 ) ) ;
#44685 = EDGE_LOOP ( 'NONE', ( #47956, #70088, #52629, #68134, #22846, #99045 ) ) ;
#44686 = CARTESIAN_POINT ( 'NONE',  ( -1.314451062625864530, 21.63968482537510241, 6.879959252342844778 ) ) ;
#44687 = ORIENTED_EDGE ( 'NONE', *, *, #80384, .F. ) ;
#44688 = CARTESIAN_POINT ( 'NONE',  ( 0.5317675288997081307, 8.007226681051733408, -51.63779123901733925 ) ) ;
#44689 = LINE ( 'NONE', #3696, #9948 ) ;
#44690 = VECTOR ( 'NONE', #93896, 1000.000000000000000 ) ;
#44691 = B_SPLINE_CURVE_WITH_KNOTS ( 'NONE', 3,
 ( #34318, #99533, #27837, #26765, #35925 ),
 .UNSPECIFIED., .F., .F.,
 ( 4, 1, 4 ),
 ( 0.000000000000000000, 0.003752776749732571800, 0.007505553499465145335 ),
 .UNSPECIFIED. ) ;
#44692 = CARTESIAN_POINT ( 'NONE',  ( 0.000000000000000000, 0.5000000000000000000, 0.000000000000000000 ) ) ;
#44693 = ORIENTED_EDGE ( 'NONE', *, *, #69198, .F. ) ;
#44694 = DIRECTION ( 'NONE',  ( 0.000000000000000000, -1.000000000000000000, 0.000000000000000000 ) ) ;
#44695 = EDGE_LOOP ( 'NONE', ( #3080, #13069, #95434, #80648, #33074 ) ) ;
#44696 = CARTESIAN_POINT ( 'NONE',  ( 106.8254625047631521, -30.00000000010051693, 139.4333767052048074 ) ) ;
#44697 = SURFACE_SIDE_STYLE ('',( #14816 ) ) ;
#44698 = CARTESIAN_POINT ( 'NONE',  ( -4.401186155046908688, -13.27308926788038690, -9.172652456351809036 ) ) ;
#44699 = CARTESIAN_POINT ( 'NONE',  ( 47.37019975563026719, 41.99999999991776178, 36.40416150969240050 ) ) ;
#44700 = CARTESIAN_POINT ( 'NONE',  ( 100.4699977146906491, -30.00000000000000000, 183.0391429837226553 ) ) ;
#44701 = CYLINDRICAL_SURFACE ( 'NONE', #38079, 10.00000000000000178 ) ;
#44702 = ORIENTED_EDGE ( 'NONE', *, *, #11082, .F. ) ;
#44703 = CIRCLE ( 'NONE', #10182, 5.999999999999998224 ) ;
#44704 = VERTEX_POINT ( 'NONE', #106287 ) ;
#44705 = EDGE_LOOP ( 'NONE', ( #70652, #69887 ) ) ;
#44706 = CARTESIAN_POINT ( 'NONE',  ( 53.92222671074195972, -25.63022886178348614, 52.72325914952270409 ) ) ;
#44707 = CARTESIAN_POINT ( 'NONE',  ( 6.798788993459229602, 41.26122520824648632, -58.42041755854287999 ) ) ;
#44708 = DIRECTION ( 'NONE',  ( 0.000000000000000000, -1.000000000000000000, 0.000000000000000000 ) ) ;
#44709 = EDGE_LOOP ( 'NONE', ( #50422, #76492, #49870, #63734 ) ) ;
#44710 = CARTESIAN_POINT ( 'NONE',  ( -90.37459492297462305, -38.40150067238776188, -14.96073006302789032 ) ) ;
#44711 = CIRCLE ( 'NONE', #27496, 3.400000000000000355 ) ;
#44712 = ORIENTED_EDGE ( 'NONE', *, *, #23275, .F. ) ;
#44713 = CARTESIAN_POINT ( 'NONE',  ( 107.1641568268869236, -38.36318885066040707, 194.5620192865105480 ) ) ;
#44714 = CARTESIAN_POINT ( 'NONE',  ( 11.43762656160894764, 13.06896439115584663, 10.01660222353511109 ) ) ;
#44715 = CARTESIAN_POINT ( 'NONE',  ( 82.50951266294359243, -37.86122216130837614, 7.438025769970757040 ) ) ;
#44716 = CARTESIAN_POINT ( 'NONE',  ( 42.74195034478192667, 379.2643428173500979, 18.73097918361189329 ) ) ;
#44717 = CARTESIAN_POINT ( 'NONE',  ( 6.547363650394499857, -12.76646305665543224, -7.895817423510056443 ) ) ;
#44718 = CIRCLE ( 'NONE', #17153, 7.499999999992679633 ) ;
#44719 = CARTESIAN_POINT ( 'NONE',  ( 6.291779652043092419, -1.386462189980837367, 6.829130021847430676 ) ) ;
#44720 = B_SPLINE_CURVE_WITH_KNOTS ( 'NONE', 3,
 ( #58628, #17642, #94037, #50503, #83415, #7926, #42970, #9514, #51037 ),
 .UNSPECIFIED., .F., .F.,
 ( 4, 2, 1, 2, 4 ),
 ( 0.000000000000000000, 0.002165063509461097931, 0.004330127018922195863, 0.006495190528383293360, 0.008660254037844391725 ),
 .UNSPECIFIED. ) ;
#44721 = CARTESIAN_POINT ( 'NONE',  ( 0.000000000000000000, 0.000000000000000000, -12.00000000000003908 ) ) ;
#44722 = CARTESIAN_POINT ( 'NONE',  ( 9.240146679119453310, 139.9709698507093947, -3.072172964960699772E-13 ) ) ;
#44723 = ORIENTED_EDGE ( 'NONE', *, *, #79195, .F. ) ;
#44724 =( LENGTH_UNIT ( ) NAMED_UNIT ( * ) SI_UNIT ( .MILLI., .METRE. ) );
#44725 = EDGE_CURVE ( 'NONE', #79044, #93975, #80758, .T. ) ;
#44726 = CARTESIAN_POINT ( 'NONE',  ( 15.54289451413696455, 36.90012926360036261, -23.41220851048994689 ) ) ;
#44727 = LINE ( 'NONE', #92183, #96988 ) ;
#44728 = ORIENTED_EDGE ( 'NONE', *, *, #42618, .T. ) ;
#44729 = ADVANCED_FACE ( 'NONE', ( #89072 ), #538, .F. ) ;
#44730 = CARTESIAN_POINT ( 'NONE',  ( -33.86200970433443302, 330.3616465235857618, -2.745656544132137000 ) ) ;
#44731 = CARTESIAN_POINT ( 'NONE',  ( -29.55140958588439659, 314.0474313513822722, 12.65717121493886133 ) ) ;
#44732 = CARTESIAN_POINT ( 'NONE',  ( 0.000000000000000000, 1.500000000000000000, 0.000000000000000000 ) ) ;
#44733 = CARTESIAN_POINT ( 'NONE',  ( -13.07034959214954384, 42.28767730836202787, -92.53124009454084842 ) ) ;
#44734 = CARTESIAN_POINT ( 'NONE',  ( 3.313708498984762496, -23.28124999999999645, 7.999999999999998224 ) ) ;
#44735 = CARTESIAN_POINT ( 'NONE',  ( 35.58102909488143695, -24.34075600965972086, 33.68644870080316167 ) ) ;
#44736 = AXIS2_PLACEMENT_3D ( 'NONE', #67691, #90903, #25676 ) ;
#44737 = ADVANCED_FACE ( 'NONE', ( #33499, #57207, #99255, #40510 ), #16226, .T. ) ;
#44738 = AXIS2_PLACEMENT_3D ( 'NONE', #42047, #92181, #67920 ) ;
#44739 = CARTESIAN_POINT ( 'NONE',  ( 37.85084083633365282, 438.0234350436313093, 4.171260309356235929 ) ) ;
#44740 = EDGE_LOOP ( 'NONE', ( #105725, #19174, #55957 ) ) ;
#44741 = CARTESIAN_POINT ( 'NONE',  ( 85.21443187028769728, -35.75854868015726140, 182.1664523584917106 ) ) ;
#44742 = CARTESIAN_POINT ( 'NONE',  ( 6.162888688655347558, 7.505553499465140277, 0.000000000000000000 ) ) ;
#44743 = EDGE_LOOP ( 'NONE', ( #29059, #14429, #67450, #19384, #5067, #8251 ) ) ;
#44744 = CARTESIAN_POINT ( 'NONE',  ( -88.35647174428689254, -37.82076271483501984, 68.44965775589997747 ) ) ;
#44745 = ADVANCED_FACE ( 'NONE', ( #98727 ), #82565, .T. ) ;
#44746 = CARTESIAN_POINT ( 'NONE',  ( 17.61650669486618881, 1.474610560812782335E-15, 0.000000000000000000 ) ) ;
#44747 = CARTESIAN_POINT ( 'NONE',  ( 9.290012601907397638, -5.000000000000002665, -75.85638632170150686 ) ) ;
#44748 = CARTESIAN_POINT ( 'NONE',  ( 13.85425718576306053, -3.000000000000003109, -90.90560122695632117 ) ) ;
#44749 = CARTESIAN_POINT ( 'NONE',  ( 10.11650669486618881, -3.851859888774471706E-31, 4.000000000000000888 ) ) ;
#44750 = EDGE_CURVE ( 'NONE', #3475, #60873, #91099, .T. ) ;
#44751 = B_SPLINE_CURVE_WITH_KNOTS ( 'NONE', 3,
 ( #95654, #37984, #21268, #55684, #37451, #45523, #38495, #30947, #78396, #21791 ),
 .UNSPECIFIED., .F., .F.,
 ( 4, 2, 2, 2, 4 ),
 ( 0.009353627468483456664, 0.01031000219096074762, 0.01126637691343803857, 0.01222275163591532779, 0.01317912635839261874 ),
 .UNSPECIFIED. ) ;
#44752 = CIRCLE ( 'NONE', #67067, 4.000000000000000888 ) ;
#44753 = CARTESIAN_POINT ( 'NONE',  ( 24.81410138265733423, -59.99999999999998579, 41.11425977102789631 ) ) ;
#44754 = CARTESIAN_POINT ( 'NONE',  ( 2.701267476147420687, -18.15621507579777827, 35.02215398985747186 ) ) ;
#44755 = CARTESIAN_POINT ( 'NONE',  ( 48.01188717829646180, -29.24194067517573004, 43.63834193384174398 ) ) ;
#44758 = CARTESIAN_POINT ( 'NONE',  ( -13.51094462923033745, 20.09129127893359268, 7.071435863031892310 ) ) ;
#44757 = PRESENTATION_LAYER_ASSIGNMENT (  '', '', ( #48185 ) ) ;
#44756 = CARTESIAN_POINT ( 'NONE',  ( 34.01847390526999959, 436.1371930933524368, 7.446563569466525756 ) ) ;
#44759 = CARTESIAN_POINT ( 'NONE',  ( -1.435124379509183671E-09, 294.8518027762758038, -10.00000000000000178 ) ) ;
#44760 = CARTESIAN_POINT ( 'NONE',  ( -5.082755093536325042, -9.593750002048384573, -5.082755093536325930 ) ) ;
#44761 = CARTESIAN_POINT ( 'NONE',  ( 43.09576643549013397, 346.8086250391238536, 10.18035955780312030 ) ) ;
#44762 = CARTESIAN_POINT ( 'NONE',  ( 5.975663821521874475, 7.000939006314125024, -0.8740179403731729302 ) ) ;
#44763 = AXIS2_PLACEMENT_3D ( 'NONE', #46917, #47965, #54996 ) ;
#44764 = ORIENTED_EDGE ( 'NONE', *, *, #59351, .T. ) ;
#44765 = CARTESIAN_POINT ( 'NONE',  ( 0.000000000000000000, 30.00000000000000000, 0.000000000000000000 ) ) ;
#44766 = CARTESIAN_POINT ( 'NONE',  ( -17.49999999999998579, 51.01864103017746999, 63.17274301512910739 ) ) ;
#44767 = ORIENTED_EDGE ( 'NONE', *, *, #61429, .F. ) ;
#44768 = CARTESIAN_POINT ( 'NONE',  ( -9.674956971852997967, -2.241286958287645348, 15.44908467815371722 ) ) ;
#44769 = CARTESIAN_POINT ( 'NONE',  ( 38.09999999999999432, 1.533819458162526451E-15, 0.000000000000000000 ) ) ;
#44770 = CARTESIAN_POINT ( 'NONE',  ( 14.34999999999999787, -3.309499999999999886, 4.475777889183790779E-16 ) ) ;
#44771 = VECTOR ( 'NONE', #83406, 1000.000000000000000 ) ;
#44773 = CARTESIAN_POINT ( 'NONE',  ( -22.10641630101648047, -34.58974403249237639, -31.65637301226508526 ) ) ;
#44772 = CARTESIAN_POINT ( 'NONE',  ( 9.699016383038332023, 253.1763817144832558, 2.444973590251036555 ) ) ;
#44774 = ADVANCED_FACE ( 'NONE', ( #9188 ), #74983, .T. ) ;
#44775 = ORIENTED_EDGE ( 'NONE', *, *, #10630, .F. ) ;
#44776 =( GEOMETRIC_REPRESENTATION_CONTEXT ( 3 ) GLOBAL_UNCERTAINTY_ASSIGNED_CONTEXT ( ( #100647 ) ) GLOBAL_UNIT_ASSIGNED_CONTEXT ( ( #64892, #47631, #97254 ) ) REPRESENTATION_CONTEXT ( 'NONE', 'WORKASPACE' ) );
#44777 = CARTESIAN_POINT ( 'NONE',  ( 9.924872551452409652, 294.6447722021068216, -1.392423705979285442 ) ) ;
#44778 = CARTESIAN_POINT ( 'NONE',  ( -43.48294191332882264, 479.1553598318504896, 6.034956245169025735 ) ) ;
#44779 = ORIENTED_EDGE ( 'NONE', *, *, #95771, .F. ) ;
#44780 = ADVANCED_FACE ( 'NONE', ( #19478 ), #54882, .T. ) ;
#44781 = EDGE_CURVE ( 'NONE', #97864, #8963, #20475, .T. ) ;
#44782 = CARTESIAN_POINT ( 'NONE',  ( 23.09999999999999432, 3.309500000000003439, 4.052968581778167743E-16 ) ) ;
#44783 = CARTESIAN_POINT ( 'NONE',  ( -91.86228806005425440, -60.00000000000000711, 11.38199961291973139 ) ) ;
#44784 = VERTEX_POINT ( 'NONE', #3250 ) ;
#44785 = CARTESIAN_POINT ( 'NONE',  ( -8.000000000000001776, -25.15624999999999289, 3.313708498984759387 ) ) ;
#44786 = CARTESIAN_POINT ( 'NONE',  ( -89.99999999999997158, -60.00000000000000000, 198.0238439516549818 ) ) ;
#44787 = CARTESIAN_POINT ( 'NONE',  ( 7.500000000000007105, 40.28750351091937176, -59.87155384411956760 ) ) ;
#44788 = CARTESIAN_POINT ( 'NONE',  ( -3.454253436624930451, -0.8414180287960395521, 103.7259032015043232 ) ) ;
#44790 = CARTESIAN_POINT ( 'NONE',  ( 0.000000000000000000, 1.500000000000000444, -61.23540616453487218 ) ) ;
#44789 = CARTESIAN_POINT ( 'NONE',  ( -46.00000000000000000, 500.0000000000002274, 0.000000000000000000 ) ) ;
#44791 = CIRCLE ( 'NONE', #37969, 3.309500000000001663 ) ;
#44792 = CARTESIAN_POINT ( 'NONE',  ( -85.01355329713241815, -22.07199797865288815, 160.8995575460550924 ) ) ;
#44793 = VERTEX_POINT ( 'NONE', #75531 ) ;
#44794 = CARTESIAN_POINT ( 'NONE',  ( -5.483261958908374645, -0.000000000000000000, 16.14668631624861916 ) ) ;
#44795 = VERTEX_POINT ( 'NONE', #10779 ) ;
#44796 = EDGE_LOOP ( 'NONE', ( #71728, #36603 ) ) ;
#44797 = CARTESIAN_POINT ( 'NONE',  ( -14.92208856358372948, -5.000000000000000000, -7.448748508017043690 ) ) ;
#44798 = DIRECTION ( 'NONE',  ( -0.000000000000000000, -1.000000000000000000, -0.000000000000000000 ) ) ;
#44799 = ORIENTED_EDGE ( 'NONE', *, *, #60166, .T. ) ;
#44800 = EDGE_CURVE ( 'NONE', #40836, #99482, #36190, .T. ) ;
#44801 = SURFACE_STYLE_FILL_AREA ( #11873 ) ;
#44802 = CARTESIAN_POINT ( 'NONE',  ( -93.88160267686131988, -57.67344353738141649, 16.36278552810739839 ) ) ;
#44803 = CARTESIAN_POINT ( 'NONE',  ( -5.093082057083964109, -67.44446206421571333, -3.176439207277722332 ) ) ;
#44804 = DIRECTION ( 'NONE',  ( 0.000000000000000000, -1.000000000000000000, 3.755786496842903988E-16 ) ) ;
#44805 = CARTESIAN_POINT ( 'NONE',  ( -9.843481099141461854, 101.4079544384661347, -1.779148000612192915 ) ) ;
#44806 = CARTESIAN_POINT ( 'NONE',  ( -13.66213079746738934, -51.55693619836885233, 23.93919572553859609 ) ) ;
#44807 = CARTESIAN_POINT ( 'NONE',  ( -27.99999999999999645, 1.347111479062088405E-15, 11.00000000000000000 ) ) ;
#44808 = AXIS2_PLACEMENT_3D ( 'NONE', #43807, #20118, #35767 ) ;
#44809 = CARTESIAN_POINT ( 'NONE',  ( 109.5930103617047422, -60.00000000000001421, 123.9179654958789456 ) ) ;
#44810 = EDGE_CURVE ( 'NONE', #13133, #11758, #99626, .T. ) ;
#44811 = CARTESIAN_POINT ( 'NONE',  ( -108.2763249159406769, -59.99999999999986500, 199.3718883026843116 ) ) ;
#44812 = CARTESIAN_POINT ( 'NONE',  ( -57.26801628779367093, -25.61114176797853048, 59.45904782552288026 ) ) ;
#44813 = EDGE_LOOP ( 'NONE', ( #78664, #50121, #38280, #76287 ) ) ;
#44814 = LINE ( 'NONE', #30764, #2222 ) ;
#44815 = VERTEX_POINT ( 'NONE', #1625 ) ;
#44816 = CARTESIAN_POINT ( 'NONE',  ( -105.7774229000524713, -60.15503266313929487, 184.0530045780120645 ) ) ;
#44817 = SURFACE_SIDE_STYLE ('',( #27062 ) ) ;
#44818 = EDGE_CURVE ( 'NONE', #52295, #86521, #60448, .T. ) ;
#44819 = CARTESIAN_POINT ( 'NONE',  ( 4.898587196589412829E-16, -18.31250000409676915, -8.000000000000000000 ) ) ;
#44820 = VERTEX_POINT ( 'NONE', #11855 ) ;
#44821 = CARTESIAN_POINT ( 'NONE',  ( 19.49162701228398831, 49.99890833186964301, 60.08453375891043891 ) ) ;
#44822 =( NAMED_UNIT ( * ) PLANE_ANGLE_UNIT ( ) SI_UNIT ( $, .RADIAN. ) );
#44823 = CARTESIAN_POINT ( 'NONE',  ( 36.32228901050014258, 26.06995930799696737, -12.06152503804560006 ) ) ;
#44824 = CARTESIAN_POINT ( 'NONE',  ( -7.188101187500002709, -17.18750000204838813, 2.977408999572648707 ) ) ;
#44825 = CARTESIAN_POINT ( 'NONE',  ( 26.69900261086841198, -5.000000000000000000, 6.123233995736768255E-16 ) ) ;
#44826 = SURFACE_STYLE_FILL_AREA ( #29208 ) ;
#44827 = CARTESIAN_POINT ( 'NONE',  ( 21.08349330513380337, 1.593028355512270567E-15, 0.000000000000000000 ) ) ;
#44828 = CARTESIAN_POINT ( 'NONE',  ( -31.02212611900126760, 360.5725590293961318, 22.12937154125974715 ) ) ;
#44829 =( NAMED_UNIT ( * ) PLANE_ANGLE_UNIT ( ) SI_UNIT ( $, .RADIAN. ) );
#44830 = CARTESIAN_POINT ( 'NONE',  ( -9.716937824887432740, 8.335377965868620009, -0.000000000000000000 ) ) ;
#44831 = CARTESIAN_POINT ( 'NONE',  ( -15.88324666189017442, 46.12968798971461837, -4.401569153915046329 ) ) ;
#44832 = CARTESIAN_POINT ( 'NONE',  ( -7.500000000000001776, -7.939616441372559841, -16.39477006944641957 ) ) ;
#44833 = ADVANCED_BREP_SHAPE_REPRESENTATION ( '', ( #17528, #10728 ), #71253 ) ;
#44834 = UNCERTAINTY_MEASURE_WITH_UNIT (LENGTH_MEASURE( 1.000000000000000082E-05 ), #25951, 'distance_accuracy_value', 'NONE');
#44835 = CARTESIAN_POINT ( 'NONE',  ( -26.89381846417044031, -29.05099145694870799, 30.38545181110030313 ) ) ;
#44836 = AXIS2_PLACEMENT_3D ( 'NONE', #24261, #57110, #90023 ) ;
#44837 = SURFACE_STYLE_FILL_AREA ( #2209 ) ;
#44838 = CARTESIAN_POINT ( 'NONE',  ( 47.00746256722314342, -49.89691352968622340, 49.27416738806363128 ) ) ;
#44839 = CARTESIAN_POINT ( 'NONE',  ( -32.68130198255966690, 486.6487900980505401, 8.407187415461715219 ) ) ;
#44840 = CARTESIAN_POINT ( 'NONE',  ( 9.601913782316094270, 10.04478976116411459, -0.2204769333330966474 ) ) ;
#44841 = CIRCLE ( 'NONE', #20779, 8.000000000000000000 ) ;
#44842 = CARTESIAN_POINT ( 'NONE',  ( -84.83356168783870999, -38.71398380538228423, 198.3796149434837730 ) ) ;
#44843 = ORIENTED_EDGE ( 'NONE', *, *, #73375, .F. ) ;
#44844 = CARTESIAN_POINT ( 'NONE',  ( -16.10103474921845645, 21.87197452378397600, -0.4486278773666070863 ) ) ;
#44845 = CARTESIAN_POINT ( 'NONE',  ( -19.35113623624150847, 49.90206012729868235, 61.17429927557744662 ) ) ;
#44846 = CARTESIAN_POINT ( 'NONE',  ( 4.881098022930994595, 41.14559726925936900, -70.72437870144329963 ) ) ;
#44847 = CARTESIAN_POINT ( 'NONE',  ( -31.43208348565049093, 438.4707862388140711, 22.17802677911227960 ) ) ;
#44848 = CARTESIAN_POINT ( 'NONE',  ( 42.38863085960136345, 465.0218298504000245, 14.26222171105679770 ) ) ;
#44849 = CARTESIAN_POINT ( 'NONE',  ( -1.152188841818234133E-13, -1.200000000000000030E-05, -50.50000000000000000 ) ) ;
#44850 = CARTESIAN_POINT ( 'NONE',  ( 111.7255001473898091, -60.00000000000002132, 159.8843962759177373 ) ) ;
#44851 = PRESENTATION_LAYER_ASSIGNMENT (  '', '', ( #31094 ) ) ;
#44852 =( BOUNDED_SURFACE ( )  B_SPLINE_SURFACE ( 3, 2, ( 
 ( #71102, #70042, #72166 ),
 ( #103990, #30139, #102949 ),
 ( #105073, #64098, #29112 ),
 ( #54903, #61980, #79722 ),
 ( #87832, #94871, #21010 ),
 ( #53851, #13912, #38753 ),
 ( #91553, #72689, #58652 ),
 ( #41918, #73208, #48928 ),
 ( #15515, #65134, #887 ),
 ( #50009, #89941, #105587 ),
 ( #41390, #106645, #82913 ),
 ( #56494, #81825, #7949 ),
 ( #98030, #73747, #7413 ),
 ( #74803, #58097, #91029 ) ),
 .UNSPECIFIED., .F., .F., .F. ) 
 B_SPLINE_SURFACE_WITH_KNOTS ( ( 4, 2, 2, 2, 2, 2, 4 ),
 ( 3, 3 ),
 ( 1.066854937725736363E-16, 0.001036839948806552976, 0.001555259923209776230, 0.002073679897612999267, 0.002592099872016222738, 0.003110519846419445775, 0.004147359795225891849 ),
 ( 0.000000000000000000, 1.000000000000000000 ),
 .UNSPECIFIED. ) 
 GEOMETRIC_REPRESENTATION_ITEM ( )  RATIONAL_B_SPLINE_SURFACE ( (
 ( 1.000000000000000000, 0.8806660624990210184, 1.000000000000000000),
 ( 1.000000000000000000, 0.8881715692663398887, 1.000000000000000000),
 ( 1.000000000000000000, 0.8928479710807692982, 1.000000000000000000),
 ( 1.000000000000000000, 0.8947313045151574773, 1.000000000000000000),
 ( 1.000000000000000000, 0.8944961860243605400, 1.000000000000000000),
 ( 1.000000000000000000, 0.8923679545987566186, 1.000000000000000000),
 ( 1.000000000000000000, 0.8904472546607578032, 1.000000000000000000),
 ( 1.000000000000000000, 0.8850746651128988951, 1.000000000000000000),
 ( 1.000000000000000000, 0.8816555630482483252, 1.000000000000000000),
 ( 1.000000000000000000, 0.8735136825612432876, 1.000000000000000000),
 ( 1.000000000000000000, 0.8687495631807600205, 1.000000000000000000),
 ( 1.000000000000000000, 0.8530568296136552542, 1.000000000000000000),
 ( 1.000000000000000000, 0.8406856949796707168, 1.000000000000000000),
 ( 1.000000000000000000, 0.8270258197359637853, 1.000000000000000000) ) ) 
 REPRESENTATION_ITEM ( '' )  SURFACE ( )  );
#44853 = CARTESIAN_POINT ( 'NONE',  ( 102.0666666666666629, -4.171999999999998820, 5.616230220889773285E-16 ) ) ;
#44854 = AXIS2_PLACEMENT_3D ( 'NONE', #96307, #22436, #88205 ) ;
#44855 = EDGE_LOOP ( 'NONE', ( #56965, #54144, #35445, #26857 ) ) ;
#44856 = EDGE_CURVE ( 'NONE', #37712, #38220, #43176, .T. ) ;
#44857 = CARTESIAN_POINT ( 'NONE',  ( -100.7109739928592660, -29.99999999999998224, 161.5959690901798069 ) ) ;
#44858 = ORIENTED_EDGE ( 'NONE', *, *, #61082, .T. ) ;
#44859 =( GEOMETRIC_REPRESENTATION_CONTEXT ( 3 ) GLOBAL_UNCERTAINTY_ASSIGNED_CONTEXT ( ( #18708 ) ) GLOBAL_UNIT_ASSIGNED_CONTEXT ( ( #90504, #73233, #33893 ) ) REPRESENTATION_CONTEXT ( 'NONE', 'WORKASPACE' ) );
#44860 = CARTESIAN_POINT ( 'NONE',  ( 5.227629274769425294, 7.725904378977054066, -28.12787702362269471 ) ) ;
#44861 = CARTESIAN_POINT ( 'NONE',  ( 12.40392177672334029, -4.188815825756464051, -12.99189655448344105 ) ) ;
#44862 = CARTESIAN_POINT ( 'NONE',  ( -5.000000000000000000, 0.000000000000000000, -0.02540000000000007530 ) ) ;
#44863 = CARTESIAN_POINT ( 'NONE',  ( -1.320432766682874540E-15, -12.40625000204838635, 7.188101187500000044 ) ) ;
#44864 = EDGE_CURVE ( 'NONE', #15128, #47515, #101405, .T. ) ;
#44865 = AXIS2_PLACEMENT_3D ( 'NONE', #29342, #62232, #96695 ) ;
#44866 = LINE ( 'NONE', #13528, #70785 ) ;
#44868 = ORIENTED_EDGE ( 'NONE', *, *, #80711, .F. ) ;
#44867 = CARTESIAN_POINT ( 'NONE',  ( 83.86866073052654258, 1.030564683017419500E-14, 0.000000000000000000 ) ) ;
#44869 = CARTESIAN_POINT ( 'NONE',  ( 83.14894204440837200, -39.48093398824585165, 171.2762584616673394 ) ) ;
#44870 = EDGE_CURVE ( 'NONE', #19669, #1420, #47943, .T. ) ;
#44871 = AXIS2_PLACEMENT_3D ( 'NONE', #91499, #50473, #83384 ) ;
#44872 = CARTESIAN_POINT ( 'NONE',  ( -46.00000000000000000, 460.3195313667367827, 7.040850765593992477 ) ) ;
#44874 = EDGE_CURVE ( 'NONE', #53794, #61442, #75699, .T. ) ;
#44873 = CARTESIAN_POINT ( 'NONE',  ( 9.221346651730840449, 86.04834020068338418, -3.869102247876031520 ) ) ;
#44875 = EDGE_LOOP ( 'NONE', ( #96114, #46809, #94375, #38329 ) ) ;
#44876 = DIRECTION ( 'NONE',  ( 0.000000000000000000, -1.000000000000000000, 0.000000000000000000 ) ) ;
#44877 = EDGE_CURVE ( 'NONE', #76301, #57315, #23909, .T. ) ;
#44878 = LINE ( 'NONE', #36284, #75355 ) ;
#44879 = DIRECTION ( 'NONE',  ( 0.000000000000000000, 0.000000000000000000, 1.000000000000000000 ) ) ;
#44880 = CARTESIAN_POINT ( 'NONE',  ( 29.99999999999999645, 486.7667864837127354, 5.222266633581397421 ) ) ;
#44881 = DIRECTION ( 'NONE',  ( 1.000000000000000000, 1.224606353822377258E-16, 0.000000000000000000 ) ) ;
#44882 = CARTESIAN_POINT ( 'NONE',  ( -42.57704743493907529, 486.1612337113410831, 7.852296464539637810 ) ) ;
#44883 = CARTESIAN_POINT ( 'NONE',  ( 0.000000000000000000, 4.898587196589412829E-16, -4.000000000000000000 ) ) ;
#44884 = VERTEX_POINT ( 'NONE', #45311 ) ;
#44885 =( LENGTH_UNIT ( ) NAMED_UNIT ( * ) SI_UNIT ( .MILLI., .METRE. ) );
#44886 = CARTESIAN_POINT ( 'NONE',  ( -3.957035243681184866, 299.4356451597976161, 9.196738408810819720 ) ) ;
#44887 = AXIS2_PLACEMENT_3D ( 'NONE', #74437, #58268, #1604 ) ;
#44888 = DIRECTION ( 'NONE',  ( 0.000000000000000000, -1.000000000000000000, 0.000000000000000000 ) ) ;
#44889 = PLANE ( 'NONE',  #92376 ) ;
#44891 = DIRECTION ( 'NONE',  ( 0.000000000000000000, 0.000000000000000000, 1.000000000000000000 ) ) ;
#44890 = CARTESIAN_POINT ( 'NONE',  ( 4.582575694955839829, 15.00000000000000000, 10.00000000000000000 ) ) ;
#44892 = CIRCLE ( 'NONE', #26064, 10.39117206796836257 ) ;
#44893 = B_SPLINE_CURVE_WITH_KNOTS ( 'NONE', 3,
 ( #97628, #58242, #89030, #23793, #24842, #106248, #8629, #65280, #81974, #8095 ),
 .UNSPECIFIED., .F., .F.,
 ( 4, 2, 2, 2, 4 ),
 ( 8.182674270850422113E-18, 0.0008022363492415295842, 0.001604472698483051145, 0.002406709047724572489, 0.003208945396966094050 ),
 .UNSPECIFIED. ) ;
#44894 = CARTESIAN_POINT ( 'NONE',  ( -7.188101187500000044, -25.90625000204838813, -8.802885111219163269E-16 ) ) ;
#44895 = CARTESIAN_POINT ( 'NONE',  ( 4.898587196589412829E-16, -28.62499999999999289, -8.000000000000000000 ) ) ;
#44896 = CARTESIAN_POINT ( 'NONE',  ( 0.000000000000000000, 36.79151656018385097, 22.55262289886175964 ) ) ;
#44897 = DIRECTION ( 'NONE',  ( 0.000000000000000000, -0.9253863139535632998, 0.3790252893243894472 ) ) ;
#44898 = ORIENTED_EDGE ( 'NONE', *, *, #95834, .T. ) ;
#44899 = DIRECTION ( 'NONE',  ( -1.000000000000000000, -0.000000000000000000, -0.000000000000000000 ) ) ;
#44900 = CARTESIAN_POINT ( 'NONE',  ( -80.00000000000000000, -38.00000000001091394, -21.09707704303352926 ) ) ;
#44901 = CARTESIAN_POINT ( 'NONE',  ( -3.067150697641109591, 44.40839135605776988, -5.000000000000000000 ) ) ;
#44902 = DIRECTION ( 'NONE',  ( -0.5735764363510461594, 0.8191520442889916875, 1.003171929053524870E-16 ) ) ;
#44903 = PRESENTATION_LAYER_ASSIGNMENT (  '', '', ( #56877 ) ) ;
#44904 = ORIENTED_EDGE ( 'NONE', *, *, #62879, .T. ) ;
#44905 = CARTESIAN_POINT ( 'NONE',  ( 37.54639040359151636, 463.7818835076658388, 19.50744869160540773 ) ) ;
#44906 = CARTESIAN_POINT ( 'NONE',  ( 8.000000000000000000, -21.59375000409677625, -3.313708498984761164 ) ) ;
#44907 = VERTEX_POINT ( 'NONE', #38296 ) ;
#44908 = EDGE_CURVE ( 'NONE', #16577, #95900, #29681, .T. ) ;
#44909 = CARTESIAN_POINT ( 'NONE',  ( -28.35646210991579963, 34.18623537382805466, 8.867673889502601270 ) ) ;
#44910 = CARTESIAN_POINT ( 'NONE',  ( 89.64643850830432825, -2.002967142162725287E-29, 5.000000000000011546 ) ) ;
#44911 = CARTESIAN_POINT ( 'NONE',  ( 9.948561005166130400, 101.1300972625180066, -1.045755304005130837 ) ) ;
#44912 = DIRECTION ( 'NONE',  ( 0.000000000000000000, 0.000000000000000000, 1.000000000000000000 ) ) ;
#44913 = UNCERTAINTY_MEASURE_WITH_UNIT (LENGTH_MEASURE( 1.000000000000000082E-05 ), #37370, 'distance_accuracy_value', 'NONE');
#44914 = CARTESIAN_POINT ( 'NONE',  ( -92.43873093052026491, -59.99999999999999289, 202.4061414662364484 ) ) ;
#44915 = DIRECTION ( 'NONE',  ( 0.000000000000000000, 0.000000000000000000, 1.000000000000000000 ) ) ;
#44916 = DIRECTION ( 'NONE',  ( 1.000000000000000000, 0.000000000000000000, 0.000000000000000000 ) ) ;
#44917 = CARTESIAN_POINT ( 'NONE',  ( 6.069741682797264559, 53.39713335310042908, -8.261810659904046616 ) ) ;
#44918 = CARTESIAN_POINT ( 'NONE',  ( 17.99632133236754328, 34.41154148830023018, -22.85738012984803547 ) ) ;
#44919 = CARTESIAN_POINT ( 'NONE',  ( -83.89707888881473252, -46.55430503609073867, 184.2034029786331359 ) ) ;
#44920 = CARTESIAN_POINT ( 'NONE',  ( 34.69770406740761359, 42.64551627458131833, -62.79854340097827503 ) ) ;
#44921 = VECTOR ( 'NONE', #71484, 1000.000000000000114 ) ;
#44922 = STYLED_ITEM ( 'NONE', ( #78521 ), #50189 ) ;
#44923 = VERTEX_POINT ( 'NONE', #13969 ) ;
#44924 = DIRECTION ( 'NONE',  ( -1.000000000000000000, 0.000000000000000000, 0.000000000000000000 ) ) ;
#44925 = CARTESIAN_POINT ( 'NONE',  ( 8.099999999999999645, 0.000000000000000000, 8.400000000000000355 ) ) ;
#44926 = CARTESIAN_POINT ( 'NONE',  ( -83.74416109486040227, -45.26689415792657911, 7.590503140103296964 ) ) ;
#44927 = CIRCLE ( 'NONE', #69029, 4.000000000000007105 ) ;
#44928 = LINE ( 'NONE', #5509, #28842 ) ;
#44929 = CARTESIAN_POINT ( 'NONE',  ( -3.006283056400744780, 103.2180882720525545, -4.999999999999999112 ) ) ;
#44930 = CARTESIAN_POINT ( 'NONE',  ( 8.830611806671452513, 133.7952729321947061, -4.999999999999385381 ) ) ;
#44931 = CARTESIAN_POINT ( 'NONE',  ( 28.35143274818196346, 36.34363242571733110, -8.614219218061366590 ) ) ;
#44932 = CARTESIAN_POINT ( 'NONE',  ( -37.36680950586716676, 18.64316884709021238, -10.04205104292877770 ) ) ;
#44933 = MECHANICAL_DESIGN_GEOMETRIC_PRESENTATION_REPRESENTATION (  '', ( #20887 ), #88036 ) ;
#44934 = CARTESIAN_POINT ( 'NONE',  ( 52.56736687853028656, -59.99999999999993605, 85.36620364727897936 ) ) ;
#44935 = SURFACE_STYLE_USAGE ( .BOTH. , #35257 ) ;
#44936 = AXIS2_PLACEMENT_3D ( 'NONE', #65277, #97624, #41001 ) ;
#44937 = CARTESIAN_POINT ( 'NONE',  ( -84.06615883987635129, -30.00000000000009592, -21.85610764691116259 ) ) ;
#44938 = CARTESIAN_POINT ( 'NONE',  ( -64.14719193146001430, -42.96209425739802157, 85.50081336499792428 ) ) ;
#44939 = VERTEX_POINT ( 'NONE', #20561 ) ;
#44940 = CARTESIAN_POINT ( 'NONE',  ( 110.6388055374740276, -59.99999999999995026, 195.8051704144367591 ) ) ;
#44941 = CARTESIAN_POINT ( 'NONE',  ( 43.67033176680568118, 40.83721295465350920, 48.51745517052664525 ) ) ;
#44942 = CARTESIAN_POINT ( 'NONE',  ( 14.10670912403736210, -60.00000000000986233, 42.10997246407520578 ) ) ;
#44943 = EDGE_LOOP ( 'NONE', ( #6564, #70588 ) ) ;
#44944 = DIRECTION ( 'NONE',  ( -1.000000000000000000, -1.224606353822377258E-16, -0.000000000000000000 ) ) ;
#44945 = CARTESIAN_POINT ( 'NONE',  ( 5.082755093536324154, -24.21875000204838813, 5.082755093536326818 ) ) ;
#44946 = EDGE_CURVE ( 'NONE', #49330, #56292, #97928, .T. ) ;
#44947 = CARTESIAN_POINT ( 'NONE',  ( 7.149395896920095848E-21, 27.29656849860388235, -40.75000000000000000 ) ) ;
#44948 = VERTEX_POINT ( 'NONE', #69586 ) ;
#44949 = FACE_OUTER_BOUND ( 'NONE', #19243, .T. ) ;
#44950 = VERTEX_POINT ( 'NONE', #103010 ) ;
#44951 = CARTESIAN_POINT ( 'NONE',  ( 6.019162162299725338, 41.99999999999999289, -71.20548073449060666 ) ) ;
#44952 = CARTESIAN_POINT ( 'NONE',  ( -60.77971423025187647, -59.99999999999997868, -35.44896578423877287 ) ) ;
#44953 = DIRECTION ( 'NONE',  ( -0.000000000000000000, 1.000000000000000000, -0.000000000000000000 ) ) ;
#44954 = CARTESIAN_POINT ( 'NONE',  ( 5.082755093536325930, -31.34375000204838457, -5.082755093536325042 ) ) ;
#44955 = CARTESIAN_POINT ( 'NONE',  ( -48.91297851735075852, 13.22767571191107194, 16.49376885358302758 ) ) ;
#44956 = CARTESIAN_POINT ( 'NONE',  ( 16.65484354297773351, 1.340359594676612611E-15, 0.000000000000000000 ) ) ;
#44957 = CARTESIAN_POINT ( 'NONE',  ( 0.000000000000000000, 152.0000000000000000, 5.000000000000000000 ) ) ;
#44958 = CARTESIAN_POINT ( 'NONE',  ( 3.140974613991526887, 50.00000000000000000, -73.31232788067644890 ) ) ;
#44959 = CARTESIAN_POINT ( 'NONE',  ( -7.618844049274130725, 108.1723589892945938, 2.450177051822847840 ) ) ;
#44960 = CYLINDRICAL_SURFACE ( 'NONE', #97779, 1.249999999999999334 ) ;
#44961 = STYLED_ITEM ( 'NONE', ( #30322 ), #105147 ) ;
#44962 = ORIENTED_EDGE ( 'NONE', *, *, #23819, .T. ) ;
#44964 = CARTESIAN_POINT ( 'NONE',  ( 33.16625095708381110, -39.49312339222125701, 34.41974150182668524 ) ) ;
#44963 = CARTESIAN_POINT ( 'NONE',  ( 4.044331601661468767, 52.01019311517404731, -7.150024461864991743 ) ) ;
#44965 = AXIS2_PLACEMENT_3D ( 'NONE', #74220, #41861, #74748 ) ;
#44966 = CARTESIAN_POINT ( 'NONE',  ( -20.16952962162825358, -4.285714285714285587, -15.50035291838207741 ) ) ;
#44967 = ORIENTED_EDGE ( 'NONE', *, *, #69469, .T. ) ;
#44968 = CARTESIAN_POINT ( 'NONE',  ( 34.42195163688486303, 484.1350747783266684, 0.1342865971131924074 ) ) ;
#44969 = CONICAL_SURFACE ( 'NONE', #105231, 3.309500000000001663, 0.9599310885968770357 ) ;
#44971 = CARTESIAN_POINT ( 'NONE',  ( 20.19615384615384457, 4.172000000000003261, 0.000000000000000000 ) ) ;
#44970 =( LENGTH_UNIT ( ) NAMED_UNIT ( * ) SI_UNIT ( .MILLI., .METRE. ) );
#44972 = DIRECTION ( 'NONE',  ( 0.000000000000000000, 0.000000000000000000, -1.000000000000000000 ) ) ;
#44973 = CARTESIAN_POINT ( 'NONE',  ( -18.69764690323647116, 302.6592417714942940, -10.04078470653332822 ) ) ;
#44974 = CARTESIAN_POINT ( 'NONE',  ( -7.500000000000000000, -4.999999999999999112, -20.99851272547259029 ) ) ;
#44975 = CARTESIAN_POINT ( 'NONE',  ( 26.69900261086841198, 6.123233995736772199E-16, -5.000000000000001776 ) ) ;
#44976 = CARTESIAN_POINT ( 'NONE',  ( -14.29190075645216851, 12.99999999999999289, 0.000000000000000000 ) ) ;
#44977 = CARTESIAN_POINT ( 'NONE',  ( -34.38464471058380667, 463.7420058809016723, 19.22113941036815277 ) ) ;
#44978 = VERTEX_POINT ( 'NONE', #21069 ) ;
#44979 = CARTESIAN_POINT ( 'NONE',  ( 92.42593725262484838, -60.00000000000000000, -0.2051320214708048373 ) ) ;
#44980 = DIRECTION ( 'NONE',  ( -1.000000000000000000, -1.224606353822377258E-16, -0.000000000000000000 ) ) ;
#44981 = CARTESIAN_POINT ( 'NONE',  ( 6.162888688655350222, -7.505553499465148271, 0.000000000000000000 ) ) ;
#44982 = CARTESIAN_POINT ( 'NONE',  ( -35.50958238476149376, 382.3993991366144201, 6.026798545227356918 ) ) ;
#44983 = CARTESIAN_POINT ( 'NONE',  ( -6.040960885908838840, 41.48433382036304096, -70.81801790822488840 ) ) ;
#44984 = DIRECTION ( 'NONE',  ( 0.000000000000000000, 0.000000000000000000, -1.000000000000000000 ) ) ;
#44985 = EDGE_LOOP ( 'NONE', ( #17275, #35483, #80714, #31581 ) ) ;
#44986 = CARTESIAN_POINT ( 'NONE',  ( -102.1093457436780625, -30.00000000000017764, 198.0925856303319108 ) ) ;
#44987 = ORIENTED_EDGE ( 'NONE', *, *, #63940, .T. ) ;
#44988 = EDGE_CURVE ( 'NONE', #96386, #24908, #86760, .T. ) ;
#44989 = CARTESIAN_POINT ( 'NONE',  ( -9.574562898131892652, -56.64787618657226176, 24.10796671758935261 ) ) ;
#44990 = FILL_AREA_STYLE_COLOUR ( '', #68376 ) ;
#44991 = CARTESIAN_POINT ( 'NONE',  ( 38.09999999999999432, 1.533819458162526451E-15, 0.000000000000000000 ) ) ;
#44992 = CARTESIAN_POINT ( 'NONE',  ( 14.77180908113486346, 22.75028154196231611, 2.587654188261260924 ) ) ;
#44993 = CARTESIAN_POINT ( 'NONE',  ( 83.19409135691178392, -45.27699134791323843, -14.11599572094245936 ) ) ;
#44994 = CARTESIAN_POINT ( 'NONE',  ( -5.082755093536325042, -32.46875000204838813, -5.082755093536325930 ) ) ;
#44995 = CARTESIAN_POINT ( 'NONE',  ( -17.59381741287697665, 45.00000000000001421, 63.12291724128729697 ) ) ;
#44996 = CARTESIAN_POINT ( 'NONE',  ( 9.443129677143925704, 46.21199370134088014, -13.23108103747124353 ) ) ;
#44997 = ORIENTED_EDGE ( 'NONE', *, *, #49160, .F. ) ;
#44998 = FILL_AREA_STYLE ('',( #55171 ) ) ;
#44999 = EDGE_CURVE ( 'NONE', #106581, #4153, #65208, .T. ) ;
#45000 = ORIENTED_EDGE ( 'NONE', *, *, #54982, .F. ) ;
#45001 = CARTESIAN_POINT ( 'NONE',  ( 48.48335035450812569, 8.813057796081539053, -16.77177117249988214 ) ) ;
#45003 = ORIENTED_EDGE ( 'NONE', *, *, #5143, .F. ) ;
#45002 = DIRECTION ( 'NONE',  ( 0.000000000000000000, 0.000000000000000000, 1.000000000000000000 ) ) ;
#45004 = CARTESIAN_POINT ( 'NONE',  ( 77.54917875449221754, -56.83930884621564417, 148.6048652908098404 ) ) ;
#45005 = VERTEX_POINT ( 'NONE', #46362 ) ;
#45006 = MECHANICAL_DESIGN_GEOMETRIC_PRESENTATION_REPRESENTATION (  '', ( #41510 ), #17431 ) ;
#45007 = CARTESIAN_POINT ( 'NONE',  ( 4.788374038886465733, -47.31025204562959630, 42.82694009917617706 ) ) ;
#45008 = EDGE_CURVE ( 'NONE', #58498, #73855, #51501, .T. ) ;
#45009 = CARTESIAN_POINT ( 'NONE',  ( -7.188101187500000044, -16.90625000204838813, -8.802885111219163269E-16 ) ) ;
#45010 = EDGE_CURVE ( 'NONE', #21775, #79502, #15316, .T. ) ;
#45011 = CARTESIAN_POINT ( 'NONE',  ( -107.9249424950986906, -57.65976581800653378, 199.0938304663491749 ) ) ;
#45012 = ORIENTED_EDGE ( 'NONE', *, *, #78405, .F. ) ;
#45014 = B_SPLINE_CURVE_WITH_KNOTS ( 'NONE', 3,
 ( #74211, #49942, #73681, #25728, #32186, #50464, #42383, #41322, #71683, #90413, #38818, #59120, #99552, #58586, #106039, #48865, #26257, #41852, #91487, #65069, #56959, #92001, #32735, #290, #83374, #65602, #821, #106583, #97965, #17602, #24641, #8421, #15988, #9471 ),
 .UNSPECIFIED., .F., .F.,
 ( 4, 2, 2, 2, 2, 2, 2, 2, 2, 2, 2, 2, 2, 2, 2, 2, 4 ),
 ( 0.01263889472610567853, 0.01342810546992895433, 0.01421731621375223013, 0.01500652695757550767, 0.01579573770139878347, 0.01658494844522205927, 0.01737415918904533507, 0.01816336993286861434, 0.01895258067669189014, 0.01974179142051516594, 0.02053100216433844522, 0.02132021290816171755, 0.02210942365198499682, 0.02289863439580826915, 0.02368784513963154842, 0.02447705588345482422, 0.02526626662727810002 ),
 .UNSPECIFIED. ) ;
#45013 = AXIS2_PLACEMENT_3D ( 'NONE', #66785, #99671, #73249 ) ;
#45015 = EDGE_CURVE ( 'NONE', #104331, #478, #13616, .T. ) ;
#45017 = CARTESIAN_POINT ( 'NONE',  ( -4.472135954999581386, -10.00000000000000888, -4.000000000000000000 ) ) ;
#45016 = STYLED_ITEM ( 'NONE', ( #29058 ), #19335 ) ;
#45018 = CARTESIAN_POINT ( 'NONE',  ( -9.918325909156568088, 81.20764768292566771, 1.298699613733151237 ) ) ;
#45019 = CONICAL_SURFACE ( 'NONE', #34708, 5.000000000000000000, 0.9599310885968913576 ) ;
#45020 = CARTESIAN_POINT ( 'NONE',  ( 17.61650669486618881, 4.000000000000003553, 4.898587196589414801E-16 ) ) ;
#45021 = CARTESIAN_POINT ( 'NONE',  ( -8.000000000000001776, -20.84375000409677270, 3.313708498984758943 ) ) ;
#45022 = CARTESIAN_POINT ( 'NONE',  ( -43.37936553595135791, -27.70851877802382290, 38.49181127301306304 ) ) ;
#45023 = CARTESIAN_POINT ( 'NONE',  ( 43.10000000000000142, -3.309499999999999886, 0.000000000000000000 ) ) ;
#45024 = CARTESIAN_POINT ( 'NONE',  ( 5.365535441410388628, 42.28877518162276772, -59.25308630239388208 ) ) ;
#45025 = CARTESIAN_POINT ( 'NONE',  ( 97.05545962818543160, -41.67787136694374084, 193.4168249765711778 ) ) ;
#45026 = SHAPE_DEFINITION_REPRESENTATION ( #60525, #7490 ) ;
#45027 = DIRECTION ( 'NONE',  ( 0.000000000000000000, -1.000000000000000000, 0.000000000000000000 ) ) ;
#45028 = VERTEX_POINT ( 'NONE', #95439 ) ;
#45029 = CARTESIAN_POINT ( 'NONE',  ( -1.269730911708409238, -50.00000000000000000, 44.94218429609317411 ) ) ;
#45030 = CARTESIAN_POINT ( 'NONE',  ( 11.62087833628057432, -4.912050167074662355, -12.56209946431235203 ) ) ;
#45031 = DIRECTION ( 'NONE',  ( -0.000000000000000000, -0.000000000000000000, -1.000000000000000000 ) ) ;
#45032 = CARTESIAN_POINT ( 'NONE',  ( -8.577179510621105507, -18.39515840085658382, -37.90072206629012896 ) ) ;
#45033 = CARTESIAN_POINT ( 'NONE',  ( -60.71702475842560176, -30.00000000000000000, 68.69174167666419351 ) ) ;
#45034 = CARTESIAN_POINT ( 'NONE',  ( 22.59067934059547156, 27.55769764751301665, -33.04957285560310254 ) ) ;
#45035 = B_SPLINE_CURVE_WITH_KNOTS ( 'NONE', 3,
 ( #60048, #26627, #83223, #1758, #18518, #50318, #34715, #100468, #9317, #51912, #58966, #99386, #2832, #68663, #17977, #92372, #76188, #1211, #25568, #27159, #51377, #10386 ),
 .UNSPECIFIED., .F., .F.,
 ( 4, 2, 2, 2, 2, 2, 2, 2, 2, 2, 4 ),
 ( 0.007115138407500913240, 0.007619047327870813284, 0.008122956248240713328, 0.008626865168610614240, 0.008878819628795569033, 0.009130774088980523825, 0.009382728549165480353, 0.009634683009350435146, 0.01013859192972034300, 0.01064250085009025085, 0.01114640977046015870 ),
 .UNSPECIFIED. ) ;
#45036 = ORIENTED_EDGE ( 'NONE', *, *, #13889, .T. ) ;
#45037 = FACE_OUTER_BOUND ( 'NONE', #34721, .T. ) ;
#45038 = CARTESIAN_POINT ( 'NONE',  ( 75.31978416560909295, -57.56542590815787719, 191.5343058687835764 ) ) ;
#45039 = VECTOR ( 'NONE', #36226, 1000.000000000000000 ) ;
#45040 = CARTESIAN_POINT ( 'NONE',  ( 0.000000000000000000, -3.035766082959412415E-15, 0.000000000000000000 ) ) ;
#45041 = EDGE_CURVE ( 'NONE', #93508, #673, #65290, .T. ) ;
#45042 = CARTESIAN_POINT ( 'NONE',  ( 27.87892343117143668, -28.78925693790030849, -38.27049670904933265 ) ) ;
#45043 = VECTOR ( 'NONE', #89726, 1000.000000000000227 ) ;
#45044 = CARTESIAN_POINT ( 'NONE',  ( 9.500000000000000000, -5.000000000000000000, -36.97043916959991350 ) ) ;
#45045 = FACE_OUTER_BOUND ( 'NONE', #21827, .T. ) ;
#45046 = CARTESIAN_POINT ( 'NONE',  ( -49.57512317434233040, -60.00000000000000711, 70.75543162407628017 ) ) ;
#45047 = DIRECTION ( 'NONE',  ( -1.000000000000000000, 0.000000000000000000, 0.000000000000000000 ) ) ;
#45048 = CARTESIAN_POINT ( 'NONE',  ( 39.04923757935661399, 48.00000000000000000, 52.30342408741256577 ) ) ;
#45049 = CARTESIAN_POINT ( 'NONE',  ( -86.36540683355931947, -20.96352888107788104, 181.2261683823607825 ) ) ;
#45050 = ORIENTED_EDGE ( 'NONE', *, *, #28962, .T. ) ;
#45051 = CARTESIAN_POINT ( 'NONE',  ( -4.060342910471293365, -42.95752896766379081, 31.04180052082970676 ) ) ;
#45052 = CARTESIAN_POINT ( 'NONE',  ( -6.814345648127551947, 41.80574614977290793, -59.39410014841684671 ) ) ;
#45053 = FACE_OUTER_BOUND ( 'NONE', #47490, .T. ) ;
#45054 = CARTESIAN_POINT ( 'NONE',  ( -7.314965114740616947, 54.29834303721024469, 2.637232812314642239 ) ) ;
#45055 = ORIENTED_EDGE ( 'NONE', *, *, #69071, .T. ) ;
#45056 = CONICAL_SURFACE ( 'NONE', #15685, 4.000000000000001776, 0.9599310885968808105 ) ;
#45057 = CARTESIAN_POINT ( 'NONE',  ( -36.68474926415177606, 425.7828876856403895, 5.530442334352566824 ) ) ;
#45058 = CARTESIAN_POINT ( 'NONE',  ( 66.00571552735603120, -4.000000000000000000, 4.898587196589421703E-16 ) ) ;
#45059 = PRESENTATION_STYLE_ASSIGNMENT (( #63365 ) ) ;
#45060 = CARTESIAN_POINT ( 'NONE',  ( -5.956988534971662475, 4.556784786910193397, -5.000000000000000000 ) ) ;
#45061 = VERTEX_POINT ( 'NONE', #71157 ) ;
#45062 = CARTESIAN_POINT ( 'NONE',  ( 17.50000000000000711, 50.00000000000000711, 63.71427545230567802 ) ) ;
#45063 = CARTESIAN_POINT ( 'NONE',  ( 11.89035689955473885, 21.46281526437144649, 7.296656512214268808 ) ) ;
#45064 = CARTESIAN_POINT ( 'NONE',  ( -22.03900363278799190, -4.285714285715346072, 12.70248734012972669 ) ) ;
#45065 =( NAMED_UNIT ( * ) PLANE_ANGLE_UNIT ( ) SI_UNIT ( $, .RADIAN. ) );
#45066 = CARTESIAN_POINT ( 'NONE',  ( 97.22633417984880566, -59.99999999999997158, 47.92222960719137603 ) ) ;
#45067 = CARTESIAN_POINT ( 'NONE',  ( -82.86146759555738583, -22.15494292095191753, 144.5965692535937421 ) ) ;
#45068 = ORIENTED_EDGE ( 'NONE', *, *, #80036, .F. ) ;
#45069 = CARTESIAN_POINT ( 'NONE',  ( 42.36162206505706251, 485.1874691988858217, -2.398526663485936350 ) ) ;
#45070 = DIRECTION ( 'NONE',  ( 0.000000000000000000, 0.000000000000000000, 1.000000000000000000 ) ) ;
#45071 = SURFACE_STYLE_USAGE ( .BOTH. , #69345 ) ;
#45072 = CARTESIAN_POINT ( 'NONE',  ( 50.94745919686198476, 50.00000000000000000, -37.05882352941176094 ) ) ;
#45073 = CARTESIAN_POINT ( 'NONE',  ( 36.57040099523793941, 337.1877129126421551, -1.689591862844450620 ) ) ;
#45074 = ADVANCED_FACE ( 'NONE', ( #79779 ), #28832, .T. ) ;
#45075 = CARTESIAN_POINT ( 'NONE',  ( 28.58349330513380337, 1.593028355512270567E-15, 0.000000000000000000 ) ) ;
#45076 = ORIENTED_EDGE ( 'NONE', *, *, #97150, .T. ) ;
#45077 = CARTESIAN_POINT ( 'NONE',  ( 3.400000000000000355, 0.000000000000000000, -1.581124522925831499 ) ) ;
#45078 = AXIS2_PLACEMENT_3D ( 'NONE', #53222, #19836, #44068 ) ;
#45079 = CARTESIAN_POINT ( 'NONE',  ( 31.50457389700596167, 439.3522922964306190, 23.21593941183056131 ) ) ;
#45080 = CARTESIAN_POINT ( 'NONE',  ( 2.977408999572650927, -26.37500000204838457, -7.188101187500001821 ) ) ;
#45081 = ORIENTED_EDGE ( 'NONE', *, *, #25237, .F. ) ;
#45082 = CONICAL_SURFACE ( 'NONE', #26170, 11.27631144943088337, 1.221730476396025722 ) ;
#45084 = ADVANCED_FACE ( 'NONE', ( #57086 ), #56006, .T. ) ;
#45083 = DIRECTION ( 'NONE',  ( -1.000000000000000000, 0.000000000000000000, 1.734723475976807094E-16 ) ) ;
#45085 = CARTESIAN_POINT ( 'NONE',  ( 5.342383757966601365, 41.79455485342771226, -70.44171435326786934 ) ) ;
#45086 = CARTESIAN_POINT ( 'NONE',  ( 0.08224679563971615259, -7.710515798486368588, -2.644994884459107354 ) ) ;
#45087 = CARTESIAN_POINT ( 'NONE',  ( 5.911949307999758041, -11.74847537023907584, -9.342369578515908657 ) ) ;
#45088 = CARTESIAN_POINT ( 'NONE',  ( -24.00351036083299761, 27.29299690957943980, -32.94270042870569881 ) ) ;
#45089 = VERTEX_POINT ( 'NONE', #88942 ) ;
#45090 = CARTESIAN_POINT ( 'NONE',  ( 13.89483002323571093, -60.00000000000000000, -42.23792084422591842 ) ) ;
#45091 =( GEOMETRIC_REPRESENTATION_CONTEXT ( 3 ) GLOBAL_UNCERTAINTY_ASSIGNED_CONTEXT ( ( #99049 ) ) GLOBAL_UNIT_ASSIGNED_CONTEXT ( ( #6295, #62969, #54850 ) ) REPRESENTATION_CONTEXT ( 'NONE', 'WORKASPACE' ) );
#45093 = CARTESIAN_POINT ( 'NONE',  ( 26.71221250542331305, -39.47873605212244996, 32.14795869538025386 ) ) ;
#45092 = CARTESIAN_POINT ( 'NONE',  ( -35.95074892501450847, -14.21045842199431242, 40.03088108345822604 ) ) ;
#45094 = CARTESIAN_POINT ( 'NONE',  ( 72.28092228780032258, 43.22324503868516388, 36.14046114390017550 ) ) ;
#45095 = CARTESIAN_POINT ( 'NONE',  ( -35.25737817069384050, -29.11316072765389151, 33.41771700477326590 ) ) ;
#45096 = AXIS2_PLACEMENT_3D ( 'NONE', #2935, #12610, #54125 ) ;
#45097 = UNCERTAINTY_MEASURE_WITH_UNIT (LENGTH_MEASURE( 1.000000000000000082E-05 ), #23073, 'distance_accuracy_value', 'NONE');
#45098 = VERTEX_POINT ( 'NONE', #106703 ) ;
#45099 = CARTESIAN_POINT ( 'NONE',  ( 35.02909328022846580, 463.2801532500066628, 4.636725553699557523 ) ) ;
#45100 = CARTESIAN_POINT ( 'NONE',  ( -5.232798140227928663, -48.02337292624943643, 104.1190344879414056 ) ) ;
#45101 = CARTESIAN_POINT ( 'NONE',  ( -43.61182701070574552, 463.4400368046242988, 6.347502766231601257 ) ) ;
#45102 = CARTESIAN_POINT ( 'NONE',  ( -1.007138393507579499, 51.97797158553648700, -8.242245250298140036 ) ) ;
#45103 = CARTESIAN_POINT ( 'NONE',  ( 7.551437640244097693, -61.99127537477090755, -2.648272645923382740 ) ) ;
#45104 = CARTESIAN_POINT ( 'NONE',  ( 0.01372220897661975345, -5.948365447239588377, -2.697128823393877273 ) ) ;
#45105 = ORIENTED_EDGE ( 'NONE', *, *, #36245, .T. ) ;
#45106 = CARTESIAN_POINT ( 'NONE',  ( -76.00296169842491167, -38.37803246168048332, 178.3767332364141680 ) ) ;
#45107 = FILL_AREA_STYLE ('',( #103329 ) ) ;
#45108 = CARTESIAN_POINT ( 'NONE',  ( 100.2372838592740720, -30.00000000000000711, 155.9018345844573901 ) ) ;
#45109 = CARTESIAN_POINT ( 'NONE',  ( 23.97042203813707673, 41.62162537289933084, -74.34607944144084968 ) ) ;
#45110 = EDGE_CURVE ( 'NONE', #32012, #76213, #102549, .T. ) ;
#45111 = CARTESIAN_POINT ( 'NONE',  ( 0.7016502453916999560, 15.23274035658503145, 9.981544566921638051 ) ) ;
#45112 = CARTESIAN_POINT ( 'NONE',  ( 80.95957609789309117, -30.00000000000000355, 4.740870403401825861 ) ) ;
#45113 = DIRECTION ( 'NONE',  ( -0.7071067811865460184, 0.000000000000000000, 0.7071067811865490160 ) ) ;
#45114 = VERTEX_POINT ( 'NONE', #56552 ) ;
#45115 = AXIS2_PLACEMENT_3D ( 'NONE', #65215, #31802, #6430 ) ;
#45116 = EDGE_LOOP ( 'NONE', ( #37567, #96736, #37896, #25600 ) ) ;
#45117 = ORIENTED_EDGE ( 'NONE', *, *, #6989, .T. ) ;
#45118 = LINE ( 'NONE', #30002, #12902 ) ;
#45119 = CARTESIAN_POINT ( 'NONE',  ( 37.55249893777119041, 42.26547227746785751, -58.87384932487446321 ) ) ;
#45120 = DIRECTION ( 'NONE',  ( -1.000000000000000000, -0.000000000000000000, -0.000000000000000000 ) ) ;
#45121 =( GEOMETRIC_REPRESENTATION_CONTEXT ( 3 ) GLOBAL_UNCERTAINTY_ASSIGNED_CONTEXT ( ( #8583 ) ) GLOBAL_UNIT_ASSIGNED_CONTEXT ( ( #97329, #61412, #12300 ) ) REPRESENTATION_CONTEXT ( 'NONE', 'WORKASPACE' ) );
#45122 = CARTESIAN_POINT ( 'NONE',  ( 21.08349330513380337, -4.000000000000000888, 4.898587196589416773E-16 ) ) ;
#45123 = CARTESIAN_POINT ( 'NONE',  ( -1.116724534379475386, -70.61792054436683941, 13.04250788268058692 ) ) ;
#45124 = CARTESIAN_POINT ( 'NONE',  ( -7.934914944860278041, -88.86845647200112808, -1.051261972695691771 ) ) ;
#45125 = DIRECTION ( 'NONE',  ( 0.000000000000000000, 0.000000000000000000, -1.000000000000000000 ) ) ;
#45126 = ORIENTED_EDGE ( 'NONE', *, *, #102686, .F. ) ;
#45127 = CARTESIAN_POINT ( 'NONE',  ( -5.036189802311180408, 48.00000000000000000, -76.26213611587843388 ) ) ;
#45128 = CIRCLE ( 'NONE', #48545, 8.000000000000000000 ) ;
#45129 = EDGE_LOOP ( 'NONE', ( #56751, #68425, #1829, #77871 ) ) ;
#45130 = DIRECTION ( 'NONE',  ( 0.000000000000000000, 0.000000000000000000, -1.000000000000000000 ) ) ;
#45131 = CARTESIAN_POINT ( 'NONE',  ( 32.87547266101556431, 465.6993878536748070, 10.91512469976365551 ) ) ;
#45132 = DIRECTION ( 'NONE',  ( 1.000000000000000000, -0.000000000000000000, 1.224646799147353207E-16 ) ) ;
#45133 = CARTESIAN_POINT ( 'NONE',  ( 27.69667248624871903, 296.8482049418585120, 10.37257860731564385 ) ) ;
#45134 = CYLINDRICAL_SURFACE ( 'NONE', #27034, 5.000000000000002665 ) ;
#45135 = CARTESIAN_POINT ( 'NONE',  ( 62.57728911496235469, -46.43500176870801965, 82.71392919577269254 ) ) ;
#45136 = ORIENTED_EDGE ( 'NONE', *, *, #25828, .T. ) ;
#45137 = CARTESIAN_POINT ( 'NONE',  ( 28.43338544108014077, 12.59781646960430201, -40.78060993930086653 ) ) ;
#45138 = ADVANCED_FACE ( 'NONE', ( #40382 ), #57608, .T. ) ;
#45139 = DIRECTION ( 'NONE',  ( 1.000000000000000000, 0.000000000000000000, 0.000000000000000000 ) ) ;
#45140 = CARTESIAN_POINT ( 'NONE',  ( -43.00000000000000000, 436.0987441542287115, 7.567257455462727656 ) ) ;
#45141 = EDGE_CURVE ( 'NONE', #39827, #41900, #81876, .T. ) ;
#45142 = DIRECTION ( 'NONE',  ( 0.8902151594054004136, 0.000000000000000000, 0.4555403055326912032 ) ) ;
#45143 = B_SPLINE_CURVE_WITH_KNOTS ( 'NONE', 3,
 ( #41432, #66236, #25839, #83481, #50049, #99121, #927, #67322, #40905, #98598, #1487, #25286, #59232, #32838, #92105, #58143, #57594, #9054, #75928, #82959, #90516, #49518, #99669, #91071, #57072, #33912, #42495, #34452, #66781, #24223, #58695, #17706, #18248, #100202 ),
 .UNSPECIFIED., .F., .F.,
 ( 4, 2, 2, 2, 2, 2, 2, 2, 2, 2, 2, 2, 2, 2, 2, 2, 4 ),
 ( 0.01272238763756221129, 0.01351613129786392864, 0.01430987495816564599, 0.01510361861846736334, 0.01589736227876908242, 0.01669110593907079804, 0.01748484959937251712, 0.01827859325967423620, 0.01907233691997595182, 0.01986608058027767090, 0.02065982424057938999, 0.02145356790088110560, 0.02224731156118282122, 0.02304105522148454030, 0.02383479888178625938, 0.02462854254208797500, 0.02542228620238969408 ),
 .UNSPECIFIED. ) ;
#45144 = ORIENTED_EDGE ( 'NONE', *, *, #80694, .T. ) ;
#45145 = CARTESIAN_POINT ( 'NONE',  ( 10.39117206796836435, 0.000000000000000000, -8.500000000000000000 ) ) ;
#45146 = CARTESIAN_POINT ( 'NONE',  ( -34.92499999999994742, 0.000000000000000000, 14.00000000000000000 ) ) ;
#45147 = EDGE_CURVE ( 'NONE', #70292, #57113, #22288, .T. ) ;
#45148 = DIRECTION ( 'NONE',  ( -0.000000000000000000, -0.000000000000000000, 1.000000000000000000 ) ) ;
#45149 = CARTESIAN_POINT ( 'NONE',  ( 17.33349330513380337, 1.593028355512270567E-15, 0.000000000000000000 ) ) ;
#45150 = CARTESIAN_POINT ( 'NONE',  ( 86.74131503813627830, -31.75820404643615902, 186.6526303525701564 ) ) ;
#45151 = CARTESIAN_POINT ( 'NONE',  ( -5.221602127173184726, 7.006837110516260125, -27.47515623844168786 ) ) ;
#45152 = CARTESIAN_POINT ( 'NONE',  ( -8.067121135810884525, 44.45135178119092956, 4.999999999994918731 ) ) ;
#45153 = EDGE_LOOP ( 'NONE', ( #20588, #98806, #41839 ) ) ;
#45154 = VECTOR ( 'NONE', #86145, 1000.000000000000000 ) ;
#45155 = DIRECTION ( 'NONE',  ( 0.000000000000000000, -1.000000000000000000, 0.000000000000000000 ) ) ;
#45156 = CARTESIAN_POINT ( 'NONE',  ( -6.701893397842001221, 41.44328394191487774, -70.59544911652842814 ) ) ;
#45157 = CARTESIAN_POINT ( 'NONE',  ( 5.000000000000000000, -14.21727251090713828, 9.320362779989000757 ) ) ;
#45158 = VECTOR ( 'NONE', #55470, 1000.000000000000000 ) ;
#45159 = CARTESIAN_POINT ( 'NONE',  ( -90.20126103059185141, -30.00000000000000000, 89.67039343529408768 ) ) ;
#45160 = B_SPLINE_CURVE_WITH_KNOTS ( 'NONE', 3,
 ( #55665, #14157, #64851, #15234, #56741, #55149, #32515, #63274, #104780, #48119, #97731, #106353, #81018, #15765, #65387, #96174, #47590, #7136, #22303, #88079 ),
 .UNSPECIFIED., .F., .F.,
 ( 4, 2, 2, 2, 2, 2, 2, 2, 2, 4 ),
 ( 0.003283110296550481328, 0.003787170202193927693, 0.004039200155015654561, 0.004291230107837381430, 0.005299349919124314925, 0.005803409824767780806, 0.006055439777589506807, 0.006307469730411232808, 0.006811529636054676137, 0.007315589541698119466 ),
 .UNSPECIFIED. ) ;
#45161 =( NAMED_UNIT ( * ) SI_UNIT ( $, .STERADIAN. ) SOLID_ANGLE_UNIT ( ) );
#45162 = AXIS2_PLACEMENT_3D ( 'NONE', #78887, #21234, #54063 ) ;
#45163 = CARTESIAN_POINT ( 'NONE',  ( 0.06508481715640716814, -57.67120202701944720, 41.61186395748749334 ) ) ;
#45165 = SURFACE_SIDE_STYLE ('',( #84551 ) ) ;
#45164 = CARTESIAN_POINT ( 'NONE',  ( 10.28624191511840458, 43.25714326066859172, 15.40779740156149202 ) ) ;
#45166 = AXIS2_PLACEMENT_3D ( 'NONE', #3630, #12231, #27950 ) ;
#45167 = EDGE_CURVE ( 'NONE', #17802, #77528, #57432, .T. ) ;
#45168 = DIRECTION ( 'NONE',  ( 0.000000000000000000, 0.000000000000000000, 1.000000000000000000 ) ) ;
#45169 = CARTESIAN_POINT ( 'NONE',  ( -32.20627895475222857, 464.6794106235103641, 10.68705400064572686 ) ) ;
#45170 = DIRECTION ( 'NONE',  ( 0.000000000000000000, -1.000000000000000000, -1.877893248421449036E-16 ) ) ;
#45171 = DIRECTION ( 'NONE',  ( 0.000000000000000000, -1.000000000000000000, 0.000000000000000000 ) ) ;
#45172 = FACE_BOUND ( 'NONE', #53081, .T. ) ;
#45173 = EDGE_CURVE ( 'NONE', #21685, #70585, #24237, .T. ) ;
#45174 = FILL_AREA_STYLE ('',( #5749 ) ) ;
#45175 = CARTESIAN_POINT ( 'NONE',  ( -87.32469796123234573, -39.06411114470611778, 189.6241748795063700 ) ) ;
#45176 = VERTEX_POINT ( 'NONE', #60321 ) ;
#45177 = CARTESIAN_POINT ( 'NONE',  ( 40.17717846856370301, 485.8445156049149887, -4.962122411038198067 ) ) ;
#45178 = CARTESIAN_POINT ( 'NONE',  ( -9.380871178326117388, 107.0111637979832580, 3.467392232194204116 ) ) ;
#45179 = CARTESIAN_POINT ( 'NONE',  ( -16.76553171890364879, -39.47645239752473856, 30.70764041000546740 ) ) ;
#45180 =( BOUNDED_SURFACE ( )  B_SPLINE_SURFACE ( 2, 3, ( 
 ( #12113, #45044, #93043, #60175 ),
 ( #93582, #27826, #61218, #11574 ),
 ( #19207, #61766, #76850, #18651 ) ),
 .UNSPECIFIED., .F., .F., .F. ) 
 B_SPLINE_SURFACE_WITH_KNOTS ( ( 3, 3 ),
 ( 4, 4 ),
 ( 0.000000000000000000, 1.000000000000000000 ),
 ( 0.02099851272547260256, 0.06891429205785459811 ),
 .UNSPECIFIED. ) 
 GEOMETRIC_REPRESENTATION_ITEM ( )  RATIONAL_B_SPLINE_SURFACE ( (
 ( 1.000000000000000000, 1.000000000000000000, 1.000000000000000000, 1.000000000000000000),
 ( 1.857142857142858317, 1.857142857142858317, 1.857142857142858317, 1.857142857142858317),
 ( 1.000000000000000000, 1.000000000000000000, 1.000000000000000000, 1.000000000000000000) ) ) 
 REPRESENTATION_ITEM ( '' )  SURFACE ( )  );
#45183 = ADVANCED_FACE ( 'NONE', ( #59243 ), #73900, .T. ) ;
#45182 = LINE ( 'NONE', #69451, #38812 ) ;
#45181 = CARTESIAN_POINT ( 'NONE',  ( 4.684273348644264514E-15, 28.20649408426940141, 38.25000000000000000 ) ) ;
#45184 = ORIENTED_EDGE ( 'NONE', *, *, #59621, .F. ) ;
#45185 = CIRCLE ( 'NONE', #24563, 5.000000000000002665 ) ;
#45186 = CARTESIAN_POINT ( 'NONE',  ( 15.05785784214675616, 3.824195276769981611, -4.604276673498455708 ) ) ;
#45187 = VERTEX_POINT ( 'NONE', #99683 ) ;
#45188 = DIRECTION ( 'NONE',  ( -0.000000000000000000, -1.000000000000000000, -0.000000000000000000 ) ) ;
#45189 = CIRCLE ( 'NONE', #43480, 4.000000000000000888 ) ;
#45190 = CIRCLE ( 'NONE', #53565, 8.000000000000000000 ) ;
#45191 = DIRECTION ( 'NONE',  ( 0.000000000000000000, 1.000000000000000000, 0.000000000000000000 ) ) ;
#45192 = CARTESIAN_POINT ( 'NONE',  ( -8.464573819226677287, -59.99999999999997868, -42.47522266335410990 ) ) ;
#45193 = ORIENTED_EDGE ( 'NONE', *, *, #26185, .T. ) ;
#45194 =( NAMED_UNIT ( * ) PLANE_ANGLE_UNIT ( ) SI_UNIT ( $, .RADIAN. ) );
#45195 = DIRECTION ( 'NONE',  ( 0.000000000000000000, -1.000000000000000000, 0.000000000000000000 ) ) ;
#45196 = CARTESIAN_POINT ( 'NONE',  ( 103.5716558477763130, -60.15916816527329303, 191.7890153051873483 ) ) ;
#45198 = CARTESIAN_POINT ( 'NONE',  ( 0.000000000000000000, 0.000000000000000000, -5.575057142857143155 ) ) ;
#45197 = CARTESIAN_POINT ( 'NONE',  ( 42.01828575296529777, -35.92164807018873773, 39.63900877982145232 ) ) ;
#45199 = EDGE_CURVE ( 'NONE', #55144, #2494, #20550, .T. ) ;
#45200 = ORIENTED_EDGE ( 'NONE', *, *, #72802, .T. ) ;
#45201 = ORIENTED_EDGE ( 'NONE', *, *, #35238, .F. ) ;
#45202 = ORIENTED_EDGE ( 'NONE', *, *, #101544, .F. ) ;
#45203 = CARTESIAN_POINT ( 'NONE',  ( 25.37047581387864170, 306.3720789167446696, 10.50697067398095719 ) ) ;
#45204 = ADVANCED_FACE ( 'NONE', ( #9594 ), #68398, .T. ) ;
#45205 = DIRECTION ( 'NONE',  ( -1.000000000000000000, -1.224606353822377258E-16, -0.000000000000000000 ) ) ;
#45206 = FILL_AREA_STYLE ('',( #3673 ) ) ;
#45207 = ORIENTED_EDGE ( 'NONE', *, *, #2275, .F. ) ;
#45208 = CARTESIAN_POINT ( 'NONE',  ( 40.34715123528543046, 1.340359594676612611E-15, 0.000000000000000000 ) ) ;
#45209 = CARTESIAN_POINT ( 'NONE',  ( -5.385153346518941397, 41.85687274187981188, -70.29203086348832130 ) ) ;
#45210 = CARTESIAN_POINT ( 'NONE',  ( -94.51847600260155957, -59.99999999997076117, 21.88820220593430577 ) ) ;
#45211 = CARTESIAN_POINT ( 'NONE',  ( 7.934203308536663890, -68.86700340017799249, 1.057099537198552097 ) ) ;
#45212 = CARTESIAN_POINT ( 'NONE',  ( 22.69281982466505809, -60.00000000000000000, 40.64002152815756830 ) ) ;
#45213 = CARTESIAN_POINT ( 'NONE',  ( 16.21548335344357028, -5.000000000000000000, -2.627579377633686430 ) ) ;
#45214 = CARTESIAN_POINT ( 'NONE',  ( -6.507454417189439511, 41.74144650497772346, -58.94379852000331965 ) ) ;
#45216 = CARTESIAN_POINT ( 'NONE',  ( 7.280253809880594673, -60.35889587898908104, 33.93986660363172092 ) ) ;
#45215 = CARTESIAN_POINT ( 'NONE',  ( -89.60210353745294753, -14.21045842199431597, 48.51666376363581890 ) ) ;
#45217 = ADVANCED_FACE ( 'NONE', ( #19361 ), #75404, .T. ) ;
#45218 = CARTESIAN_POINT ( 'NONE',  ( -48.85179756045110366, -49.90554923932949549, 52.24086561123009176 ) ) ;
#45219 = VERTEX_POINT ( 'NONE', #66796 ) ;
#45220 = CARTESIAN_POINT ( 'NONE',  ( 100.0424503805845831, -5.000000000000000000, 0.000000000000000000 ) ) ;
#45221 = ORIENTED_EDGE ( 'NONE', *, *, #106544, .F. ) ;
#45222 = CARTESIAN_POINT ( 'NONE',  ( 39.85564080103976181, 459.8412824357643558, 1.882109076563826200 ) ) ;
#45223 = CARTESIAN_POINT ( 'NONE',  ( 5.093082057083966774, -7.555537935784294667, -3.176439207277719667 ) ) ;
#45224 = ORIENTED_EDGE ( 'NONE', *, *, #101942, .F. ) ;
#45225 = CARTESIAN_POINT ( 'NONE',  ( -3.808203125592111604, -9.155674645823081548, 13.42226102569178892 ) ) ;
#45226 = ORIENTED_EDGE ( 'NONE', *, *, #46604, .T. ) ;
#45227 = CARTESIAN_POINT ( 'NONE',  ( 82.77319705486205237, -29.99999999998750866, -22.91096955354018050 ) ) ;
#45228 = CARTESIAN_POINT ( 'NONE',  ( 3.352941176470588758, -48.79941684889504927, 104.5794940929807524 ) ) ;
#45229 = ADVANCED_FACE ( 'NONE', ( #35521 ), #60840, .F. ) ;
#45230 = CARTESIAN_POINT ( 'NONE',  ( 6.847405647391515693, 41.77151288785266559, -59.31773432185592299 ) ) ;
#45231 = CARTESIAN_POINT ( 'NONE',  ( -51.76085035121451483, 41.99999999999999289, -29.83308852628634966 ) ) ;
#45232 = CARTESIAN_POINT ( 'NONE',  ( 100.4882595953770021, -29.99999999999999289, 182.9151894254146953 ) ) ;
#45233 = CARTESIAN_POINT ( 'NONE',  ( -7.000000000000000000, 8.572527594031471218E-16, -4.874849604647447876 ) ) ;
#45234 = ORIENTED_EDGE ( 'NONE', *, *, #28403, .F. ) ;
#45235 = B_SPLINE_CURVE_WITH_KNOTS ( 'NONE', 3,
 ( #93782, #37713, #21003, #86774, #36649, #101865 ),
 .UNSPECIFIED., .F., .F.,
 ( 4, 2, 4 ),
 ( 0.02294124189247799192, 0.02484059228080997411, 0.02673994266914195284 ),
 .UNSPECIFIED. ) ;
#45236 = ORIENTED_EDGE ( 'NONE', *, *, #85200, .F. ) ;
#45237 = ORIENTED_EDGE ( 'NONE', *, *, #75666, .F. ) ;
#45238 = CARTESIAN_POINT ( 'NONE',  ( 54.79840299013832094, -49.90675031112721882, 64.09447975165772959 ) ) ;
#45239 = CARTESIAN_POINT ( 'NONE',  ( -46.00000000000000711, 461.1586514445786520, 8.541706603213405913 ) ) ;
#45240 = VERTEX_POINT ( 'NONE', #101810 ) ;
#45241 = CARTESIAN_POINT ( 'NONE',  ( -90.37937951170148665, -38.40155043091493781, -14.94611653123792649 ) ) ;
#45242 = ORIENTED_EDGE ( 'NONE', *, *, #46140, .F. ) ;
#45243 = DIRECTION ( 'NONE',  ( -0.8660254037844379305, -0.5000000000000014433, 0.000000000000000000 ) ) ;
#45244 = CARTESIAN_POINT ( 'NONE',  ( 94.02768479641977706, -38.49244630022761271, 201.1932099879993530 ) ) ;
#45245 = CARTESIAN_POINT ( 'NONE',  ( 11.41582910567000830, 13.93800615581069380, 9.960141238938595265 ) ) ;
#45246 = CARTESIAN_POINT ( 'NONE',  ( 86.14658077292135374, -60.13954629211933423, 13.87186910527404748 ) ) ;
#45247 = CARTESIAN_POINT ( 'NONE',  ( 33.15578469393098260, 409.3745932105718452, 25.92517817600723617 ) ) ;
#45248 =( NAMED_UNIT ( * ) SI_UNIT ( $, .STERADIAN. ) SOLID_ANGLE_UNIT ( ) );
#45249 = APPLICATION_CONTEXT ( 'automotive_design' ) ;
#45250 = CARTESIAN_POINT ( 'NONE',  ( 1.517883041479706208E-15, -5.000000000000000888, -97.00000000000000000 ) ) ;
#45251 = CARTESIAN_POINT ( 'NONE',  ( -43.71789550058824148, 434.9437403290502289, 13.92762231526895711 ) ) ;
#45252 = SURFACE_STYLE_FILL_AREA ( #103991 ) ;
#45253 = ORIENTED_EDGE ( 'NONE', *, *, #59985, .T. ) ;
#45254 = AXIS2_PLACEMENT_3D ( 'NONE', #102432, #43657, #29131 ) ;
#45255 = EDGE_CURVE ( 'NONE', #46568, #59047, #101486, .T. ) ;
#45256 = DIRECTION ( 'NONE',  ( 0.000000000000000000, -1.000000000000000000, 0.000000000000000000 ) ) ;
#45257 = DIRECTION ( 'NONE',  ( 1.000000000000000000, 0.000000000000000000, 0.000000000000000000 ) ) ;
#45258 = CARTESIAN_POINT ( 'NONE',  ( -3.208644920884031304, 114.8591176307894415, 5.000000000000000000 ) ) ;
#45259 = ORIENTED_EDGE ( 'NONE', *, *, #80719, .T. ) ;
#45260 = CARTESIAN_POINT ( 'NONE',  ( -27.53989814665412084, 308.1507782404630120, -8.257886362634577537 ) ) ;
#45261 = CARTESIAN_POINT ( 'NONE',  ( -31.46913928081870182, 326.8580950721863019, 15.82560803904243407 ) ) ;
#45262 = DIRECTION ( 'NONE',  ( 0.000000000000000000, -1.000000000000000000, 0.000000000000000000 ) ) ;
#45263 = PRESENTATION_STYLE_ASSIGNMENT (( #4262 ) ) ;
#45264 = CARTESIAN_POINT ( 'NONE',  ( -1.469576158976823947E-15, -20.37499999999999289, 8.000000000000000000 ) ) ;
#45265 = CIRCLE ( 'NONE', #93538, 8.000000000000000000 ) ;
#45266 = CARTESIAN_POINT ( 'NONE',  ( -33.96155455825784486, -26.02205035446894854, 41.25632646196086029 ) ) ;
#45267 = EDGE_CURVE ( 'NONE', #99488, #49442, #39445, .T. ) ;
#45268 = CARTESIAN_POINT ( 'NONE',  ( 0.000000000000000000, 0.000000000000000000, -0.5505556536572887572 ) ) ;
#45269 = VERTEX_POINT ( 'NONE', #36594 ) ;
#45270 = CARTESIAN_POINT ( 'NONE',  ( 85.56702050224303946, -28.63500417004610554, 178.3742600491905534 ) ) ;
#45271 = CARTESIAN_POINT ( 'NONE',  ( -49.26574068698176490, 8.068653426789120786, 15.39376958037561849 ) ) ;
#45272 = CARTESIAN_POINT ( 'NONE',  ( -83.88445482477082749, -59.99999999999995737, 191.6821729358339610 ) ) ;
#45273 = ORIENTED_EDGE ( 'NONE', *, *, #62302, .F. ) ;
#45274 = CARTESIAN_POINT ( 'NONE',  ( -91.53872723970857805, -37.82056087769771580, 87.62393259169999737 ) ) ;
#45275 = FILL_AREA_STYLE ('',( #53872 ) ) ;
#45276 = CARTESIAN_POINT ( 'NONE',  ( 9.891797161801495264, -5.000000000000002665, -73.72381496649794030 ) ) ;
#45277 = DIRECTION ( 'NONE',  ( -1.000000000000000000, -1.224606353822377258E-16, -0.000000000000000000 ) ) ;
#45278 = CARTESIAN_POINT ( 'NONE',  ( 0.000000000000000000, -0.5000000000000000000, 0.000000000000000000 ) ) ;
#45279 = ADVANCED_FACE ( 'NONE', ( #4719 ), #61372, .F. ) ;
#45280 = SHAPE_DEFINITION_REPRESENTATION ( #11050, #533 ) ;
#45281 = CARTESIAN_POINT ( 'NONE',  ( 21.41851261898789005, -26.63141905998440961, 37.18235420823341286 ) ) ;
#45282 = CARTESIAN_POINT ( 'NONE',  ( 31.33511474313509382, -22.32021645782860730, 32.40417205478716767 ) ) ;
#45284 = CARTESIAN_POINT ( 'NONE',  ( -11.21656899573597954, 19.84217242128376668, 8.532680616503345306 ) ) ;
#45283 = DIRECTION ( 'NONE',  ( -1.000000000000000000, -1.224606353822377258E-16, -0.000000000000000000 ) ) ;
#45285 = ADVANCED_FACE ( 'NONE', ( #46761 ), #61915, .T. ) ;
#45286 = CARTESIAN_POINT ( 'NONE',  ( 7.697757149314820246, 296.0912719809091982, -10.02629731371293786 ) ) ;
#45287 = DIRECTION ( 'NONE',  ( 0.000000000000000000, 0.000000000000000000, 1.000000000000000000 ) ) ;
#45288 = ORIENTED_EDGE ( 'NONE', *, *, #605, .F. ) ;
#45289 = CARTESIAN_POINT ( 'NONE',  ( 34.73151746388065675, 302.0917208187174197, -0.3540781040331686391 ) ) ;
#45290 = DIRECTION ( 'NONE',  ( -0.6175266994148785882, 0.6213472858387578679, 0.4822741190345746221 ) ) ;
#45291 = EDGE_LOOP ( 'NONE', ( #9181, #54943, #52849, #6960, #53842 ) ) ;
#45292 = DIRECTION ( 'NONE',  ( -1.000000000000000000, 0.000000000000000000, 0.000000000000000000 ) ) ;
#45293 = VECTOR ( 'NONE', #101776, 1000.000000000000000 ) ;
#45294 = EDGE_LOOP ( 'NONE', ( #9176, #95006, #94524, #11215 ) ) ;
#45295 = CARTESIAN_POINT ( 'NONE',  ( -15.75694905239713783, -1.457936233759121514, 14.93097729572344790 ) ) ;
#45296 = DIRECTION ( 'NONE',  ( 0.5735764363510490460, 0.8191520442889896891, 0.000000000000000000 ) ) ;
#45297 = STYLED_ITEM ( 'NONE', ( #65857 ), #52510 ) ;
#45298 = DIRECTION ( 'NONE',  ( -1.000000000000000000, -1.224606353822377258E-16, -0.000000000000000000 ) ) ;
#45301 = EDGE_CURVE ( 'NONE', #55816, #72001, #69458, .T. ) ;
#45300 = CARTESIAN_POINT ( 'NONE',  ( 8.063737759921492554, -60.22818524261399631, -36.77936988234735338 ) ) ;
#45299 = DIRECTION ( 'NONE',  ( -0.000000000000000000, 0.000000000000000000, 1.000000000000000000 ) ) ;
#45302 = VERTEX_POINT ( 'NONE', #87767 ) ;
#45303 = DIRECTION ( 'NONE',  ( -1.224646799147351482E-16, 0.000000000000000000, -1.000000000000000000 ) ) ;
#45304 = SURFACE_STYLE_USAGE ( .BOTH. , #20552 ) ;
#45306 = VERTEX_POINT ( 'NONE', #28490 ) ;
#45305 = AXIS2_PLACEMENT_3D ( 'NONE', #3850, #2769, #60511 ) ;
#45307 = CARTESIAN_POINT ( 'NONE',  ( 15.11650669486618881, 0.000000000000000000, 4.000000000000000888 ) ) ;
#45308 = CARTESIAN_POINT ( 'NONE',  ( 0.000000000000000000, 1.005902684993156715, 0.000000000000000000 ) ) ;
#45309 = CARTESIAN_POINT ( 'NONE',  ( -92.03711610564900525, -60.00000000000000000, 19.24587899639053390 ) ) ;
#45310 = ORIENTED_EDGE ( 'NONE', *, *, #25097, .T. ) ;
#45311 = CARTESIAN_POINT ( 'NONE',  ( 7.500000000000000888, 0.000000000000000000, 1.734723475976807094E-15 ) ) ;
#45312 = FACE_BOUND ( 'NONE', #89096, .T. ) ;
#45313 = CARTESIAN_POINT ( 'NONE',  ( 89.99999999999997158, -52.00000000000000000, 196.0238439516549818 ) ) ;
#45314 = CARTESIAN_POINT ( 'NONE',  ( -9.333555687487613994, 28.21897303391028800, 3.591168747312690979 ) ) ;
#45315 = CARTESIAN_POINT ( 'NONE',  ( 32.61650669486618881, -3.999999999999998224, 0.000000000000000000 ) ) ;
#45316 = CARTESIAN_POINT ( 'NONE',  ( -80.86724053673806623, -56.93357778657505719, 177.6017799944823992 ) ) ;
#45317 = EDGE_LOOP ( 'NONE', ( #79161, #105696, #76365, #18540, #33908 ) ) ;
#45318 = CARTESIAN_POINT ( 'NONE',  ( -40.66415791351455056, 490.1350948120810358, 11.30186264364090221 ) ) ;
#45319 = VERTEX_POINT ( 'NONE', #69979 ) ;
#45320 = ORIENTED_EDGE ( 'NONE', *, *, #49369, .F. ) ;
#45321 = CARTESIAN_POINT ( 'NONE',  ( -9.117185603063706623, -4.332661967064742825, -15.39580070564181469 ) ) ;
#45322 = CONICAL_SURFACE ( 'NONE', #100433, 5.000000000000001776, 0.9599310885968803664 ) ;
#45323 = ADVANCED_FACE ( 'NONE', ( #102882, #13848 ), #21454, .T. ) ;
#45324 = CARTESIAN_POINT ( 'NONE',  ( 0.000000000000000000, 12.00000000000000000, 0.000000000000000000 ) ) ;
#45325 = CARTESIAN_POINT ( 'NONE',  ( 0.000000000000000000, 152.0000000000000000, 0.000000000000000000 ) ) ;
#45326 = ORIENTED_EDGE ( 'NONE', *, *, #51664, .F. ) ;
#45327 = CARTESIAN_POINT ( 'NONE',  ( -22.65267572660740569, 28.20149222899207331, 30.83791392134356713 ) ) ;
#45328 = B_SPLINE_CURVE_WITH_KNOTS ( 'NONE', 3,
 ( #5083, #104290, #87075, #105367, #30440, #15288, #89186, #22358, #88130, #96229, #13148, #14212, #104839, #63861, #46077, #29908, #22883, #88650, #38015, #70876, #82135, #33097, #17428, #57853, #15819, #81587, #48699, #74575, #83205, #99369, #98843, #105881, #56795, #75095 ),
 .UNSPECIFIED., .F., .F.,
 ( 4, 2, 2, 2, 2, 2, 2, 2, 2, 2, 2, 2, 2, 2, 2, 2, 4 ),
 ( 0.000000000000000000, 0.0007899309203816213881, 0.001579861840763242776, 0.002369792761144844974, 0.003159723681526447822, 0.003949654601908049803, 0.004739585522289651784, 0.005529516442671255499, 0.006319447363052857480, 0.007109378283434458594, 0.007899309203816059707, 0.008689240124197661688, 0.009479171044579263669, 0.01026910196496086738, 0.01105903288534246763, 0.01184896380572406961, 0.01263889472610566986 ),
 .UNSPECIFIED. ) ;
#45329 =( NAMED_UNIT ( * ) PLANE_ANGLE_UNIT ( ) SI_UNIT ( $, .RADIAN. ) );
#45330 = CARTESIAN_POINT ( 'NONE',  ( -94.77678295284667342, -57.67204358354969429, 30.25255809810320429 ) ) ;
#45331 = CARTESIAN_POINT ( 'NONE',  ( 6.944031699373470090, -10.53460654556130116, 3.972913591453822502 ) ) ;
#45332 = CARTESIAN_POINT ( 'NONE',  ( -0.5342533769375044095, 13.87968997803932503, 6.984477836909634085 ) ) ;
#45333 = AXIS2_PLACEMENT_3D ( 'NONE', #49476, #80782, #105590 ) ;
#45334 = CARTESIAN_POINT ( 'NONE',  ( -9.646032546913144046, 101.9871967152563172, 2.644051433538248119 ) ) ;
#45335 = DIRECTION ( 'NONE',  ( -1.000000000000000000, 0.000000000000000000, 0.000000000000000000 ) ) ;
#45336 = CARTESIAN_POINT ( 'NONE',  ( 4.397168787612283580, 15.00000000000000000, -9.999999999999998224 ) ) ;
#45337 = CARTESIAN_POINT ( 'NONE',  ( 80.19743504398171297, -30.00000000000002487, -24.77996380036185187 ) ) ;
#45338 = ADVANCED_FACE ( 'NONE', ( #79655 ), #13005, .F. ) ;
#45339 = CARTESIAN_POINT ( 'NONE',  ( -73.11793949506163415, -30.00000000000001776, 143.8487384131749423 ) ) ;
#45340 = CARTESIAN_POINT ( 'NONE',  ( -53.62371817297555054, -56.84947591570442427, 64.25590909039557630 ) ) ;
#45341 = ORIENTED_EDGE ( 'NONE', *, *, #85097, .T. ) ;
#45342 = CARTESIAN_POINT ( 'NONE',  ( 6.239770560962896617, 15.44424954685939255, -3.176762229947382998 ) ) ;
#45343 = ORIENTED_EDGE ( 'NONE', *, *, #33297, .F. ) ;
#45344 = CARTESIAN_POINT ( 'NONE',  ( -101.1402928026442538, -52.73124438991371932, 193.2249404277670237 ) ) ;
#45345 = CARTESIAN_POINT ( 'NONE',  ( 99.18548223479925241, -38.00000000000000711, 133.7811713353216874 ) ) ;
#45346 =( BOUNDED_SURFACE ( )  B_SPLINE_SURFACE ( 3, 2, ( 
 ( #52832, #62018, #11833 ),
 ( #44762, #11290, #44221 ),
 ( #77652, #3767, #36698 ),
 ( #67266, #42438, #58639 ),
 ( #59173, #100145, #91540 ),
 ( #51588, #43513, #92053 ) ),
 .UNSPECIFIED., .F., .F., .F. ) 
 B_SPLINE_SURFACE_WITH_KNOTS ( ( 4, 2, 4 ),
 ( 3, 3 ),
 ( 0.003199762745115996340, 0.007302762474435749336, 0.01140576220375550190 ),
 ( 0.000000000000000000, 1.000000000000000000 ),
 .UNSPECIFIED. ) 
 GEOMETRIC_REPRESENTATION_ITEM ( )  RATIONAL_B_SPLINE_SURFACE ( (
 ( 1.000000000000000000, 0.8047731410850428313, 1.000000000000000000),
 ( 1.000000000000000000, 0.8125552299151648228, 1.000000000000000000),
 ( 1.000000000000000000, 0.8191520442896039755, 1.000000000000000000),
 ( 1.000000000000000000, 0.8191520442883749586, 1.000000000000000000),
 ( 1.000000000000000000, 0.8125552299160877512, 1.000000000000000000),
 ( 1.000000000000000000, 0.8047731410850426093, 1.000000000000000000) ) ) 
 REPRESENTATION_ITEM ( '' )  SURFACE ( )  );
#45347 = CARTESIAN_POINT ( 'NONE',  ( -30.87886018709214397, 13.47971040000131993, -41.23243855231599042 ) ) ;
#45348 = ORIENTED_EDGE ( 'NONE', *, *, #29529, .F. ) ;
#45349 = FILL_AREA_STYLE_COLOUR ( '', #29228 ) ;
#45350 = PLANE ( 'NONE',  #51924 ) ;
#45351 = CARTESIAN_POINT ( 'NONE',  ( -5.082755093536326818, -14.09375000204838457, 5.082755093536325042 ) ) ;
#45352 = ADVANCED_FACE ( 'NONE', ( #38688 ), #37766, .F. ) ;
#45353 = CARTESIAN_POINT ( 'NONE',  ( 22.20318009218133071, 295.0333587257888439, 9.975590323731541531 ) ) ;
#45354 = SURFACE_STYLE_USAGE ( .BOTH. , #94973 ) ;
#45355 = CARTESIAN_POINT ( 'NONE',  ( 7.045965687440310710, -83.69607536213965204, 3.790395326974321133 ) ) ;
#45356 = CARTESIAN_POINT ( 'NONE',  ( 69.66098783280243367, -30.00000000000000000, 94.24250346725962402 ) ) ;
#45357 = FACE_OUTER_BOUND ( 'NONE', #42913, .T. ) ;
#45358 = CARTESIAN_POINT ( 'NONE',  ( -10.12015569271582649, 43.29311026828216313, -15.39938930500394498 ) ) ;
#45359 = CARTESIAN_POINT ( 'NONE',  ( -5.268008033849937100, 13.26688624804745587, -33.14867888032319598 ) ) ;
#45360 = CARTESIAN_POINT ( 'NONE',  ( -29.16980113487907289, -53.38861740668193079, 35.28666285170401551 ) ) ;
#45361 = CARTESIAN_POINT ( 'NONE',  ( 47.88527768379917404, -56.81691787927777426, 52.80198151643631377 ) ) ;
#45362 = CARTESIAN_POINT ( 'NONE',  ( 8.000000000000000000, -13.99999999999999112, 0.000000000000000000 ) ) ;
#45363 = CARTESIAN_POINT ( 'NONE',  ( -0.9554805223982675288, 45.45499091158017535, 18.31010292441292364 ) ) ;
#45364 = CARTESIAN_POINT ( 'NONE',  ( -87.28184510988498346, -38.58415483285815384, 199.6650293345611544 ) ) ;
#45365 = ORIENTED_EDGE ( 'NONE', *, *, #24868, .T. ) ;
#45366 = CARTESIAN_POINT ( 'NONE',  ( 89.55318350885924872, -38.38936930854548990, -17.00445670180018354 ) ) ;
#45367 = CARTESIAN_POINT ( 'NONE',  ( 12.44919954815503083, 7.219060511667757751, -8.177915604358730661 ) ) ;
#45368 = B_SPLINE_CURVE_WITH_KNOTS ( 'NONE', 3,
 ( #42832, #41766, #91915, #91399, #57939, #2362, #50905, #76257, #83816, #27226, #75729, #92978 ),
 .UNSPECIFIED., .F., .F.,
 ( 4, 2, 2, 2, 2, 4 ),
 ( 0.000000000000000000, 0.001748721146019791700, 0.003497442292039583400, 0.004371802865049432413, 0.005246163438059279691, 0.006994884584079062717 ),
 .UNSPECIFIED. ) ;
#45369 = CARTESIAN_POINT ( 'NONE',  ( -19.01480799866954285, 49.53976911447221454, 61.88728409518844131 ) ) ;
#45370 = DIRECTION ( 'NONE',  ( 0.000000000000000000, 0.000000000000000000, 1.000000000000000000 ) ) ;
#45371 = CARTESIAN_POINT ( 'NONE',  ( 5.569582024719362146, 40.00000000167852932, -71.04463995182341307 ) ) ;
#45372 = CARTESIAN_POINT ( 'NONE',  ( -31.80090313571708904, 436.0476724931270951, 18.01393100247755541 ) ) ;
#45374 = CARTESIAN_POINT ( 'NONE',  ( 5.000000000000000000, -15.93202192939576634, -5.930487099830193287 ) ) ;
#45373 = AXIS2_PLACEMENT_3D ( 'NONE', #63263, #103186, #21761 ) ;
#45375 = CARTESIAN_POINT ( 'NONE',  ( 0.000000000000000000, -15.00000000000000000, 0.000000000000000000 ) ) ;
#45376 = CARTESIAN_POINT ( 'NONE',  ( 111.3059636549010065, -59.99999999999999289, 185.6424028919510363 ) ) ;
#45377 = AXIS2_PLACEMENT_3D ( 'NONE', #1626, #99806, #41573 ) ;
#45378 = CONICAL_SURFACE ( 'NONE', #102264, 3.309500000000001663, 0.9599310885968770357 ) ;
#45379 = LINE ( 'NONE', #92846, #52562 ) ;
#45380 = VERTEX_POINT ( 'NONE', #105526 ) ;
#45381 = EDGE_CURVE ( 'NONE', #86580, #22652, #94578, .T. ) ;
#45382 = CARTESIAN_POINT ( 'NONE',  ( 3.871024465589345542, -48.78517836376548189, 104.2728733527511906 ) ) ;
#45383 = CARTESIAN_POINT ( 'NONE',  ( -77.11398825348869934, -30.00000000000000000, -16.56961864290801500 ) ) ;
#45384 = VERTEX_POINT ( 'NONE', #49401 ) ;
#45386 = CARTESIAN_POINT ( 'NONE',  ( 5.134970455931373579, -1.158234108193381795, -20.02603949707692266 ) ) ;
#45385 = CARTESIAN_POINT ( 'NONE',  ( -77.95742533360386517, -38.56940929884702740, 188.1909952854809092 ) ) ;
#45387 = CARTESIAN_POINT ( 'NONE',  ( 26.84999999999999787, 1.533819458162526451E-15, 0.000000000000000000 ) ) ;
#45388 = CARTESIAN_POINT ( 'NONE',  ( 0.000000000000000000, 6.123233995736770227E-16, -5.000000000000002665 ) ) ;
#45389 = CARTESIAN_POINT ( 'NONE',  ( 38.11055680731727335, 437.2326489915187153, 4.664335030333705667 ) ) ;
#45390 = CIRCLE ( 'NONE', #72911, 8.000000000000000000 ) ;
#45391 = CARTESIAN_POINT ( 'NONE',  ( -7.188101187500001821, -12.87500000204838813, -2.977408999572651371 ) ) ;
#45392 = CARTESIAN_POINT ( 'NONE',  ( -5.036189802309414709, -5.000000000000015099, -93.73786388411730286 ) ) ;
#45393 = EDGE_CURVE ( 'NONE', #21224, #30181, #58439, .T. ) ;
#45394 = EDGE_CURVE ( 'NONE', #22140, #57238, #41321, .T. ) ;
#45395 = CARTESIAN_POINT ( 'NONE',  ( -42.61140200160144786, 465.9030374194822457, 13.21253569360411895 ) ) ;
#45397 = EDGE_LOOP ( 'NONE', ( #95330, #33704, #96627, #5518, #15328, #59928 ) ) ;
#45396 = DIRECTION ( 'NONE',  ( 0.000000000000000000, -1.000000000000000000, 0.000000000000000000 ) ) ;
#45398 = CARTESIAN_POINT ( 'NONE',  ( 84.01537763452704155, -32.49674573478225170, 168.3552522700273073 ) ) ;
#45399 = CARTESIAN_POINT ( 'NONE',  ( 8.160631864331239882, 112.3644544865306898, -0.000000000000000000 ) ) ;
#45400 = B_SPLINE_CURVE_WITH_KNOTS ( 'NONE', 3,
 ( #59954, #100377, #84205, #50744, #18977, #85266, #27071, #92821, #26540, #59412, #92276, #3288, #18430, #10819, #10301, #51285, #99846, #58878, #93367, #36228 ),
 .UNSPECIFIED., .F., .F.,
 ( 4, 2, 2, 2, 2, 2, 2, 2, 2, 4 ),
 ( 0.007276925029303864083, 0.007780880140201501885, 0.008284835251099140555, 0.008788790361996777489, 0.009292745472894416159, 0.009796700583792054828, 0.01030065569468969176, 0.01080461080558733043, 0.01105658836103614803, 0.01130856591648496563 ),
 .UNSPECIFIED. ) ;
#45401 = CARTESIAN_POINT ( 'NONE',  ( 9.165151389911681434, 85.00000000000001421, -4.000000000000000000 ) ) ;
#45402 = ORIENTED_EDGE ( 'NONE', *, *, #88714, .F. ) ;
#45403 = CARTESIAN_POINT ( 'NONE',  ( -37.34223837122399203, 354.2692148566569585, 1.818772290766931032 ) ) ;
#45404 = AXIS2_PLACEMENT_3D ( 'NONE', #6357, #39298, #80789 ) ;
#45405 = SURFACE_SIDE_STYLE ('',( #77763 ) ) ;
#45406 = DIRECTION ( 'NONE',  ( 0.000000000000000000, -0.8802307401757925032, 0.4745459346044136328 ) ) ;
#45407 = DIRECTION ( 'NONE',  ( -1.000000000000000000, -1.224606353822377258E-16, -0.000000000000000000 ) ) ;
#45408 = DIRECTION ( 'NONE',  ( -0.000000000000000000, -1.000000000000000000, -0.000000000000000000 ) ) ;
#45409 = CARTESIAN_POINT ( 'NONE',  ( -19.96162532426521352, 302.8116070918646301, 9.928455558879880627 ) ) ;
#45410 = EDGE_CURVE ( 'NONE', #105140, #12817, #90412, .T. ) ;
#45411 = ORIENTED_EDGE ( 'NONE', *, *, #21263, .F. ) ;
#45412 = PRESENTATION_LAYER_ASSIGNMENT (  '', '', ( #2341 ) ) ;
#45413 = AXIS2_PLACEMENT_3D ( 'NONE', #30253, #55016, #28681 ) ;
#45414 = B_SPLINE_CURVE_WITH_KNOTS ( 'NONE', 3,
 ( #97740, #6615, #75470, #56747, #81540, #74923, #83555, #9130 ),
 .UNSPECIFIED., .F., .F.,
 ( 4, 2, 2, 4 ),
 ( 0.4104551234109616309, 0.4139675962486015215, 0.4174800690862414121, 0.4245050147615211378 ),
 .UNSPECIFIED. ) ;
#45415 = VECTOR ( 'NONE', #42591, 1000.000000000000114 ) ;
#45416 = CARTESIAN_POINT ( 'NONE',  ( -80.33428810687757959, -29.99999999999999645, -13.32063309743382895 ) ) ;
#45417 = DIRECTION ( 'NONE',  ( -1.000000000000000000, -1.224606353822377258E-16, -0.000000000000000000 ) ) ;
#45419 = EDGE_CURVE ( 'NONE', #2695, #62559, #63980, .T. ) ;
#45418 = CARTESIAN_POINT ( 'NONE',  ( 0.7145311798163216377, 4.618802153517004960, 7.999999999999998224 ) ) ;
#45420 = CARTESIAN_POINT ( 'NONE',  ( 0.000000000000000000, 47.77514352166374323, -11.96035173608223090 ) ) ;
#45421 = CARTESIAN_POINT ( 'NONE',  ( -7.188101187500001821, -27.50000000204838813, -2.977408999572651371 ) ) ;
#45422 = DIRECTION ( 'NONE',  ( -1.000000000000000000, -0.000000000000000000, -0.000000000000000000 ) ) ;
#45423 = CARTESIAN_POINT ( 'NONE',  ( 10.00012749751951802, -5.000000000000000000, -1.308371270547806553 ) ) ;
#45424 = DIRECTION ( 'NONE',  ( -1.000000000000000000, 0.000000000000000000, 0.000000000000000000 ) ) ;
#45425 = VERTEX_POINT ( 'NONE', #23043 ) ;
#45426 = LINE ( 'NONE', #19594, #31945 ) ;
#45427 = CARTESIAN_POINT ( 'NONE',  ( 1.000000000000002887, -70.58759490697437400, 11.03128057732868150 ) ) ;
#45428 = CARTESIAN_POINT ( 'NONE',  ( -9.686785446062245342, 8.472505610524187603, 0.000000000000000000 ) ) ;
#45429 = CARTESIAN_POINT ( 'NONE',  ( 70.41111111111112564, 6.915964383211875250E-15, 0.000000000000000000 ) ) ;
#45430 =( GEOMETRIC_REPRESENTATION_CONTEXT ( 3 ) GLOBAL_UNCERTAINTY_ASSIGNED_CONTEXT ( ( #104177 ) ) GLOBAL_UNIT_ASSIGNED_CONTEXT ( ( #102638, #61678, #37410 ) ) REPRESENTATION_CONTEXT ( 'NONE', 'WORKASPACE' ) );
#45431 = ORIENTED_EDGE ( 'NONE', *, *, #61906, .F. ) ;
#45432 = DIRECTION ( 'NONE',  ( -1.000000000000000000, -0.000000000000000000, -0.000000000000000000 ) ) ;
#45433 = CARTESIAN_POINT ( 'NONE',  ( -34.88900972249398080, 464.6206820655985439, 18.69027339340991034 ) ) ;
#45434 = VERTEX_POINT ( 'NONE', #65068 ) ;
#45435 = CARTESIAN_POINT ( 'NONE',  ( 7.000000000000000000, 0.000000000000000000, -13.00000000000000000 ) ) ;
#45436 = CARTESIAN_POINT ( 'NONE',  ( 0.000000000000000000, 0.000000000000000000, 5.000000000000000888 ) ) ;
#45437 = DIRECTION ( 'NONE',  ( -1.000000000000000000, 0.000000000000000000, 0.000000000000000000 ) ) ;
#45438 = CARTESIAN_POINT ( 'NONE',  ( -98.77838488027474284, -60.00000000000001421, 202.1921766562477103 ) ) ;
#45439 = DIRECTION ( 'NONE',  ( 0.000000000000000000, 1.000000000000000000, 0.000000000000000000 ) ) ;
#45440 = PRESENTATION_LAYER_ASSIGNMENT (  '', '', ( #93712 ) ) ;
#45441 = CARTESIAN_POINT ( 'NONE',  ( -37.83989825151947173, 491.6297408768480750, 12.44743998624971049 ) ) ;
#45442 = CARTESIAN_POINT ( 'NONE',  ( 5.934563312262005397, 54.01391609258696036, -6.164477179060972034 ) ) ;
#45443 = CARTESIAN_POINT ( 'NONE',  ( 43.00000000000000000, 464.8825480873695710, 15.07585856869435936 ) ) ;
#45444 = CARTESIAN_POINT ( 'NONE',  ( -83.72764112179662277, -42.98392764094067786, 180.3475611446869777 ) ) ;
#45445 = AXIS2_PLACEMENT_3D ( 'NONE', #15575, #105643, #48467 ) ;
#45446 = CARTESIAN_POINT ( 'NONE',  ( 39.15195563986023330, 42.02328961493514470, -56.67495990243617143 ) ) ;
#45447 = MECHANICAL_DESIGN_GEOMETRIC_PRESENTATION_REPRESENTATION (  '', ( #71067 ), #95408 ) ;
#45448 = ORIENTED_EDGE ( 'NONE', *, *, #101853, .F. ) ;
#45449 = DIRECTION ( 'NONE',  ( 0.000000000000000000, 1.000000000000000000, 0.000000000000000000 ) ) ;
#45450 = EDGE_CURVE ( 'NONE', #38500, #85705, #103878, .T. ) ;
#45451 = CARTESIAN_POINT ( 'NONE',  ( -13.45079846400083312, -54.00000000000000711, 23.11721482942554928 ) ) ;
#45452 = CARTESIAN_POINT ( 'NONE',  ( -85.37616942211955973, -52.71083131077448058, 0.7312150782069049004 ) ) ;
#45453 = CARTESIAN_POINT ( 'NONE',  ( 23.09999999999999432, 3.309500000000003439, 0.000000000000000000 ) ) ;
#45454 = FACE_OUTER_BOUND ( 'NONE', #36343, .T. ) ;
#45455 = CARTESIAN_POINT ( 'NONE',  ( 9.075061004355355010, 137.9460510617185491, 0.000000000000000000 ) ) ;
#45456 = CARTESIAN_POINT ( 'NONE',  ( -1.127757440534757460, -7.231345287187126658, -6.344532336093720026 ) ) ;
#45457 = CARTESIAN_POINT ( 'NONE',  ( 23.57730434126663255, 18.64316884711714906, 30.67950393662606245 ) ) ;
#45458 = EDGE_CURVE ( 'NONE', #43396, #77668, #47803, .T. ) ;
#45459 = CARTESIAN_POINT ( 'NONE',  ( 100.5651899622199039, -60.00000000000009948, 204.3456409986242477 ) ) ;
#45460 = FACE_OUTER_BOUND ( 'NONE', #62415, .T. ) ;
#45461 = ADVANCED_FACE ( 'NONE', ( #14909 ), #101552, .F. ) ;
#45462 = CARTESIAN_POINT ( 'NONE',  ( -86.99605493950913626, -14.21045842199422005, 24.11595694609475160 ) ) ;
#45463 = CARTESIAN_POINT ( 'NONE',  ( -63.59289893964069051, -46.43872110597177993, 85.67305972463248054 ) ) ;
#45464 = VERTEX_POINT ( 'NONE', #39743 ) ;
#45465 = CARTESIAN_POINT ( 'NONE',  ( 88.35660587733796945, -14.21045842199459486, 197.0604887900697122 ) ) ;
#45466 = CARTESIAN_POINT ( 'NONE',  ( 62.84406313655870946, 39.42568531683917143, -16.86755852376854037 ) ) ;
#45467 = CARTESIAN_POINT ( 'NONE',  ( 80.96048728771400249, -60.00000000000738254, 200.5225259978467136 ) ) ;
#45468 = VERTEX_POINT ( 'NONE', #89357 ) ;
#45469 = DIRECTION ( 'NONE',  ( -1.000000000000000000, -0.000000000000000000, -0.000000000000000000 ) ) ;
#45470 = EDGE_CURVE ( 'NONE', #62602, #32259, #21573, .T. ) ;
#45471 = CARTESIAN_POINT ( 'NONE',  ( 2.977408999572650927, -19.25000000204838457, -7.188101187500000933 ) ) ;
#45472 = CARTESIAN_POINT ( 'NONE',  ( -4.472135954999580498, -10.00000000000000888, 4.000000000000000000 ) ) ;
#45473 = VERTEX_POINT ( 'NONE', #57487 ) ;
#45474 = CARTESIAN_POINT ( 'NONE',  ( 60.63333333333333286, 6.915964383211875250E-15, 0.000000000000000000 ) ) ;
#45475 = ORIENTED_EDGE ( 'NONE', *, *, #42547, .T. ) ;
#45476 = CARTESIAN_POINT ( 'NONE',  ( 8.087340429040205336, 41.99999999999999289, -69.98180430517568595 ) ) ;
#45477 = AXIS2_PLACEMENT_3D ( 'NONE', #17548, #100033, #26727 ) ;
#45478 = CARTESIAN_POINT ( 'NONE',  ( 47.36344235967300875, 18.16811379743735344, -14.54383657267871577 ) ) ;
#45479 = CARTESIAN_POINT ( 'NONE',  ( -92.28351384443637073, -60.00000000000002842, -12.64941138170132540 ) ) ;
#45480 = CARTESIAN_POINT ( 'NONE',  ( 34.62633797947415104, 326.3522410840145653, -4.484366321573728165 ) ) ;
#45481 = CARTESIAN_POINT ( 'NONE',  ( -7.188101187500002709, -9.312500002048384573, 2.977408999572648707 ) ) ;
#45482 = ADVANCED_FACE ( 'NONE', ( #80178 ), #39222, .T. ) ;
#45483 = DIRECTION ( 'NONE',  ( 0.000000000000000000, -1.000000000000000000, 0.000000000000000000 ) ) ;
#45484 =( BOUNDED_SURFACE ( )  B_SPLINE_SURFACE ( 3, 2, ( 
 ( #63348, #96248, #89736 ),
 ( #39602, #65972, #8262 ),
 ( #41703, #23968, #57332 ),
 ( #73518, #49786, #23423 ),
 ( #105892, #105380, #56264 ),
 ( #106419, #25563, #57866 ),
 ( #90794, #33109, #72987 ),
 ( #98852, #90255, #32577 ),
 ( #65452, #33628, #89201 ),
 ( #15300, #48187, #25013 ),
 ( #81090, #74586, #48712 ),
 ( #15829, #97275, #7202 ),
 ( #662, #74054, #16907 ),
 ( #6674, #40111, #82148 ),
 ( #41175, #98345, #32039 ),
 ( #82691, #24498, #31520 ) ),
 .UNSPECIFIED., .F., .F., .F. ) 
 B_SPLINE_SURFACE_WITH_KNOTS ( ( 4, 2, 2, 2, 2, 2, 2, 4 ),
 ( 3, 3 ),
 ( 4.542807102714263578E-16, 0.0005221599045761193174, 0.001044319809151784354, 0.001566479713727449499, 0.002088639618303114644, 0.002610799522878779790, 0.003132959427454444501, 0.004177279236605774791 ),
 ( 0.000000000000000000, 1.000000000000000000 ),
 .UNSPECIFIED. ) 
 GEOMETRIC_REPRESENTATION_ITEM ( )  RATIONAL_B_SPLINE_SURFACE ( (
 ( 1.000000000000000000, 0.8909749942925634381, 1.000000000000000000),
 ( 1.000000000000000000, 0.8947619310225533029, 1.000000000000000000),
 ( 1.000000000000000000, 0.8978044232700120864, 1.000000000000000000),
 ( 1.000000000000000000, 0.9023043032701206778, 1.000000000000000000),
 ( 1.000000000000000000, 0.9037672509123999554, 1.000000000000000000),
 ( 1.000000000000000000, 0.9049062503973974714, 1.000000000000000000),
 ( 1.000000000000000000, 0.9045936109753576204, 1.000000000000000000),
 ( 1.000000000000000000, 0.9022616022696634541, 1.000000000000000000),
 ( 1.000000000000000000, 0.9002067130753756974, 1.000000000000000000),
 ( 1.000000000000000000, 0.8945795303837162926, 1.000000000000000000),
 ( 1.000000000000000000, 0.8910211780061220166, 1.000000000000000000),
 ( 1.000000000000000000, 0.8825640046873736155, 1.000000000000000000),
 ( 1.000000000000000000, 0.8776492255282648536, 1.000000000000000000),
 ( 1.000000000000000000, 0.8615337984056086196, 1.000000000000000000),
 ( 1.000000000000000000, 0.8487841387201691123, 1.000000000000000000),
 ( 1.000000000000000000, 0.8347624811018451441, 1.000000000000000000) ) ) 
 REPRESENTATION_ITEM ( '' )  SURFACE ( )  );
#45485 = AXIS2_PLACEMENT_3D ( 'NONE', #85052, #52668, #66736 ) ;
#45486 = CARTESIAN_POINT ( 'NONE',  ( 6.539732759932823214, -4.285714285714295357, 24.41571844174603356 ) ) ;
#45487 = CARTESIAN_POINT ( 'NONE',  ( 1.000000000000000000, -68.69132998577646276, 12.24443901500763765 ) ) ;
#45488 = CARTESIAN_POINT ( 'NONE',  ( 6.043427762770655853, 50.00000000000000000, -74.51456333905269958 ) ) ;
#45489 = CARTESIAN_POINT ( 'NONE',  ( -46.00000000000000000, 437.9690125970932968, 14.09127711025707796 ) ) ;
#45490 = CARTESIAN_POINT ( 'NONE',  ( 39.86396139244071435, 437.4902212974453164, 4.924226175448357168 ) ) ;
#45491 = CARTESIAN_POINT ( 'NONE',  ( 43.00000000000000000, 500.0000000000002274, 0.000000000000000000 ) ) ;
#45492 = MECHANICAL_DESIGN_GEOMETRIC_PRESENTATION_REPRESENTATION (  '', ( #23089 ), #16201 ) ;
#45493 = AXIS2_PLACEMENT_3D ( 'NONE', #49069, #7026, #16721 ) ;
#45494 = ORIENTED_EDGE ( 'NONE', *, *, #9834, .F. ) ;
#45495 = CARTESIAN_POINT ( 'NONE',  ( -8.717040642419030760, 53.90705534479965166, -1.531152949374502192 ) ) ;
#45496 = CARTESIAN_POINT ( 'NONE',  ( 4.869065774733602581, -2.951204850257813206, 102.3543991519893979 ) ) ;
#45498 = CARTESIAN_POINT ( 'NONE',  ( 35.80305322736619189, -60.28683605755409758, 39.79195959564579255 ) ) ;
#45497 = CARTESIAN_POINT ( 'NONE',  ( 4.181903434330047631, 51.73312897152540302, -7.942462034357892442 ) ) ;
#45499 = CARTESIAN_POINT ( 'NONE',  ( 38.86650669486618881, 1.474610560812782335E-15, 0.000000000000000000 ) ) ;
#45500 = ORIENTED_EDGE ( 'NONE', *, *, #5611, .T. ) ;
#45501 = CARTESIAN_POINT ( 'NONE',  ( -22.88609270656953143, 26.05164082683736737, -30.73907939488839602 ) ) ;
#45503 = CARTESIAN_POINT ( 'NONE',  ( -28.21644434148578640, 308.7733337496239301, -9.112255642778062992 ) ) ;
#45502 = CARTESIAN_POINT ( 'NONE',  ( 25.11650669486618881, 1.474610560812782335E-15, 0.000000000000000000 ) ) ;
#45504 = DIRECTION ( 'NONE',  ( -1.000000000000000000, -1.224606353822377258E-16, -0.000000000000000000 ) ) ;
#45505 = DIRECTION ( 'NONE',  ( 0.5735764363510491570, -0.8191520442889895781, 1.003171929053522035E-16 ) ) ;
#45506 = DIRECTION ( 'NONE',  ( 0.000000000000000000, 0.000000000000000000, -1.000000000000000000 ) ) ;
#45507 = CARTESIAN_POINT ( 'NONE',  ( 2.500000000000025757, -22.55587004235349369, 27.64561374872702260 ) ) ;
#45508 = CARTESIAN_POINT ( 'NONE',  ( -48.02835407290534420, 14.94086294439724227, -16.85535821593460426 ) ) ;
#45509 = SURFACE_STYLE_FILL_AREA ( #62236 ) ;
#45510 = VERTEX_POINT ( 'NONE', #74737 ) ;
#45511 = CARTESIAN_POINT ( 'NONE',  ( 92.00241997389161952, -59.99999999999999289, 6.158180974754545289 ) ) ;
#45512 = CARTESIAN_POINT ( 'NONE',  ( 32.99999999999999289, 464.3970849722209095, 17.41240408234209980 ) ) ;
#45513 = CARTESIAN_POINT ( 'NONE',  ( -6.035608738543801088, 41.34018720349636311, -70.92167698604198733 ) ) ;
#45514 = CARTESIAN_POINT ( 'NONE',  ( -11.42555267934544005, 13.51116504447436206, -9.988710933107451950 ) ) ;
#45515 = ORIENTED_EDGE ( 'NONE', *, *, #44874, .F. ) ;
#45516 = EDGE_CURVE ( 'NONE', #33537, #64587, #18906, .T. ) ;
#45517 = CARTESIAN_POINT ( 'NONE',  ( -101.8367267568395391, -29.99999999999178968, 198.2562598845839545 ) ) ;
#45518 = ORIENTED_EDGE ( 'NONE', *, *, #68620, .F. ) ;
#45519 = DIRECTION ( 'NONE',  ( 0.000000000000000000, -1.000000000000000000, 0.000000000000000000 ) ) ;
#45520 = FILL_AREA_STYLE_COLOUR ( '', #4628 ) ;
#45521 = DIRECTION ( 'NONE',  ( 0.000000000000000000, -1.000000000000000000, 0.000000000000000000 ) ) ;
#45522 = CARTESIAN_POINT ( 'NONE',  ( 15.74121454705160517, 22.21713694096877134, -3.427215416333057707 ) ) ;
#45523 = CARTESIAN_POINT ( 'NONE',  ( -6.499999999999999112, 2.227636940139120725, -0.2900584647821155548 ) ) ;
#45524 = CARTESIAN_POINT ( 'NONE',  ( -2.977408999572650039, -31.06250000204838813, -7.188101187500001821 ) ) ;
#45525 = CARTESIAN_POINT ( 'NONE',  ( -17.98225906059938239, 44.99999999999999289, 62.57939804496447067 ) ) ;
#45526 = FILL_AREA_STYLE_COLOUR ( '', #16099 ) ;
#45528 = ADVANCED_FACE ( 'NONE', ( #33790 ), #67212, .T. ) ;
#45527 = CARTESIAN_POINT ( 'NONE',  ( 34.88692455808023141, 481.7028197735354524, 14.61755684903771879 ) ) ;
#45529 = ORIENTED_EDGE ( 'NONE', *, *, #69423, .F. ) ;
#45530 = COLOUR_RGB ( '', 0.08235294, 0.09019608, 0.10196078) ;
#45532 = VERTEX_POINT ( 'NONE', #9470 ) ;
#45531 = DIRECTION ( 'NONE',  ( 0.000000000000000000, -1.000000000000000000, 0.000000000000000000 ) ) ;
#45533 = CARTESIAN_POINT ( 'NONE',  ( 79.92391610595905149, -42.96574981224191703, 149.1602879951772138 ) ) ;
#45534 = B_SPLINE_CURVE_WITH_KNOTS ( 'NONE', 3,
 ( #92703, #77054, #3170, #35572 ),
 .UNSPECIFIED., .F., .F.,
 ( 4, 4 ),
 ( 2.442512830937285646E-17, 0.001829834443479524389 ),
 .UNSPECIFIED. ) ;
#45535 = CONICAL_SURFACE ( 'NONE', #76527, 6.500000000000000888, 0.8987552595851637793 ) ;
#45536 = ORIENTED_EDGE ( 'NONE', *, *, #84689, .F. ) ;
#45537 = DIRECTION ( 'NONE',  ( -0.8191520442889881348, 1.003171929053520186E-16, 0.5735764363510513775 ) ) ;
#45538 = CARTESIAN_POINT ( 'NONE',  ( 5.082755093536324154, -19.34375000204838457, 5.082755093536326818 ) ) ;
#45539 = EDGE_CURVE ( 'NONE', #81756, #83791, #41851, .T. ) ;
#45540 = CARTESIAN_POINT ( 'NONE',  ( -88.64096389254642361, -57.60155557764662149, 203.6424623121221487 ) ) ;
#45541 = ORIENTED_EDGE ( 'NONE', *, *, #75261, .F. ) ;
#45542 = CARTESIAN_POINT ( 'NONE',  ( -4.905194654929171172, -12.02394395019843465, 3.459476078998854565 ) ) ;
#45543 = CARTESIAN_POINT ( 'NONE',  ( -9.843481099141461854, 81.40795443846614887, -1.779148000612192915 ) ) ;
#45544 = EDGE_CURVE ( 'NONE', #106169, #41106, #27535, .T. ) ;
#45545 = CARTESIAN_POINT ( 'NONE',  ( 48.49405853457110283, 15.66070211563104131, -14.43943585503448723 ) ) ;
#45546 = CARTESIAN_POINT ( 'NONE',  ( 4.898587196589412829E-16, -15.31250000409677092, -8.000000000000000000 ) ) ;
#45547 = CARTESIAN_POINT ( 'NONE',  ( -48.78551423464154624, -29.44057650021229477, 44.71846274219842599 ) ) ;
#45548 = SURFACE_SIDE_STYLE ('',( #5598 ) ) ;
#45549 = CARTESIAN_POINT ( 'NONE',  ( 42.75139825103809699, 485.3314578938637283, -3.157348782698981893 ) ) ;
#45550 = EDGE_CURVE ( 'NONE', #63169, #6761, #100620, .T. ) ;
#45551 = CARTESIAN_POINT ( 'NONE',  ( 0.000000000000000000, 0.000000000000000000, 0.000000000000000000 ) ) ;
#45552 = CARTESIAN_POINT ( 'NONE',  ( 4.506530263362012789, 52.18350610267697220, 6.292767562283435367 ) ) ;
#45554 = AXIS2_PLACEMENT_3D ( 'NONE', #47894, #106669, #80801 ) ;
#45553 = DIRECTION ( 'NONE',  ( 1.000000000000000000, 6.989781874810890086E-17, -5.620325286447034103E-17 ) ) ;
#45555 = FACE_OUTER_BOUND ( 'NONE', #63426, .T. ) ;
#45556 = ORIENTED_EDGE ( 'NONE', *, *, #77436, .F. ) ;
#45557 = CARTESIAN_POINT ( 'NONE',  ( -1.626968941750977393, -50.01525831937068034, 40.95668304117249647 ) ) ;
#45558 = CARTESIAN_POINT ( 'NONE',  ( 11.71448656990683723, -4.888164313292308272, -12.55940474970822329 ) ) ;
#45559 = CARTESIAN_POINT ( 'NONE',  ( 0.000000000000000000, 0.000000000000000000, -10.00000000000000000 ) ) ;
#45560 = AXIS2_PLACEMENT_3D ( 'NONE', #7560, #63716, #23256 ) ;
#45561 = CARTESIAN_POINT ( 'NONE',  ( -6.831292435471142177, -18.15074247170165833, -37.92091795732829951 ) ) ;
#45562 = CARTESIAN_POINT ( 'NONE',  ( -63.62542678175617539, -29.99999999999999645, 76.38903665440084012 ) ) ;
#45563 = FACE_OUTER_BOUND ( 'NONE', #104163, .T. ) ;
#45564 = EDGE_LOOP ( 'NONE', ( #27785, #73910, #12256, #100774 ) ) ;
#45565 = FACE_OUTER_BOUND ( 'NONE', #97844, .T. ) ;
#45566 = CARTESIAN_POINT ( 'NONE',  ( 83.65515381790297056, -57.54282162997657224, 201.5564494504526181 ) ) ;
#45567 = CARTESIAN_POINT ( 'NONE',  ( 59.17222854736898796, -60.22833427386899530, -29.94836549083426291 ) ) ;
#45568 = CARTESIAN_POINT ( 'NONE',  ( 102.9313392694734688, 1.016364837396684119E-14, 0.000000000000000000 ) ) ;
#45569 = DIRECTION ( 'NONE',  ( 0.000000000000000000, -0.8660254037844381525, 0.5000000000000008882 ) ) ;
#45570 = DIRECTION ( 'NONE',  ( 0.000000000000000000, -1.000000000000000000, 0.000000000000000000 ) ) ;
#45571 = CARTESIAN_POINT ( 'NONE',  ( -53.40412661496910829, -59.99999999999999289, 80.76610350128422056 ) ) ;
#45572 = LINE ( 'NONE', #30460, #28767 ) ;
#45573 = CARTESIAN_POINT ( 'NONE',  ( -5.774137037018697960, 50.00000000000000000, 63.00000000000000000 ) ) ;
#45574 = CARTESIAN_POINT ( 'NONE',  ( -86.32981076077537352, -24.59913943680475867, 182.4586318646072414 ) ) ;
#45575 = VERTEX_POINT ( 'NONE', #10545 ) ;
#45576 = CARTESIAN_POINT ( 'NONE',  ( 36.40625082012290648, 355.8303869323650588, 1.860620477795003502 ) ) ;
#45577 = CARTESIAN_POINT ( 'NONE',  ( -20.24579557674103469, 304.8297271373346575, -10.00469232190998703 ) ) ;
#45578 = CARTESIAN_POINT ( 'NONE',  ( -6.359250320826728142, 41.88719959362819623, -59.22188769180981893 ) ) ;
#45579 = DIRECTION ( 'NONE',  ( -0.000000000000000000, 1.000000000000000000, -0.000000000000000000 ) ) ;
#45580 = FACE_OUTER_BOUND ( 'NONE', #83168, .T. ) ;
#45581 = EDGE_CURVE ( 'NONE', #41052, #8974, #59651, .T. ) ;
#45583 = SURFACE_STYLE_USAGE ( .BOTH. , #96262 ) ;
#45582 = AXIS2_PLACEMENT_3D ( 'NONE', #87417, #5422, #55533 ) ;
#45584 = DIRECTION ( 'NONE',  ( 0.000000000000000000, -1.000000000000000000, 0.000000000000000000 ) ) ;
#45585 = FACE_OUTER_BOUND ( 'NONE', #26302, .T. ) ;
#45586 = DIRECTION ( 'NONE',  ( -0.000000000000000000, -1.000000000000000000, -0.000000000000000000 ) ) ;
#45587 = ORIENTED_EDGE ( 'NONE', *, *, #67541, .T. ) ;
#45588 = CARTESIAN_POINT ( 'NONE',  ( 19.06777080879943398, 50.00000000000000000, 60.49338507843820878 ) ) ;
#45589 = CARTESIAN_POINT ( 'NONE',  ( 39.83349330513380693, -4.000000000000000000, 4.898587196589415787E-16 ) ) ;
#45590 = EDGE_CURVE ( 'NONE', #90268, #712, #25398, .T. ) ;
#45591 = CARTESIAN_POINT ( 'NONE',  ( 24.56594385547636605, -4.285714285715934047, 6.601913983210457637 ) ) ;
#45592 = ADVANCED_FACE ( 'NONE', ( #51538 ), #42975, .T. ) ;
#45593 = CARTESIAN_POINT ( 'NONE',  ( 95.23263947746859515, -60.00000000000000000, 30.92889862699057701 ) ) ;
#45594 = CARTESIAN_POINT ( 'NONE',  ( -78.59425758961695863, -46.43800249855129181, 144.3747020998414996 ) ) ;
#45595 = AXIS2_PLACEMENT_3D ( 'NONE', #53209, #27919, #60782 ) ;
#45596 = EDGE_LOOP ( 'NONE', ( #77039, #11297, #91784, #86115 ) ) ;
#45597 = SURFACE_STYLE_USAGE ( .BOTH. , #31027 ) ;
#45598 = CARTESIAN_POINT ( 'NONE',  ( 44.43430165216474137, -57.68372671355613335, 63.93072606185115347 ) ) ;
#45599 = CIRCLE ( 'NONE', #43884, 11.27631144943088515 ) ;
#45600 = CARTESIAN_POINT ( 'NONE',  ( 62.81518281356948563, 50.00000000000000711, -4.977348761394969401 ) ) ;
#45601 = AXIS2_PLACEMENT_3D ( 'NONE', #23058, #22540, #89374 ) ;
#45602 = CARTESIAN_POINT ( 'NONE',  ( 42.27457937377090502, 331.6756111660436659, 6.933568496604577192 ) ) ;
#45603 = CARTESIAN_POINT ( 'NONE',  ( 38.89974058468706630, 460.7404207148335900, 2.234280701989461715 ) ) ;
#45604 = ORIENTED_EDGE ( 'NONE', *, *, #15815, .T. ) ;
#45605 = CONICAL_SURFACE ( 'NONE', #74823, 8.000000000000000000, 1.047197551196600296 ) ;
#45606 = CARTESIAN_POINT ( 'NONE',  ( 4.180739497430161933, 54.25981830507254955, -6.682218162442597809 ) ) ;
#45607 = CARTESIAN_POINT ( 'NONE',  ( 0.000000000000000000, 0.000000000000000000, 0.000000000000000000 ) ) ;
#45608 = CARTESIAN_POINT ( 'NONE',  ( 2.977408999572650927, -27.87500000204838457, -7.188101187500001821 ) ) ;
#45609 = EDGE_CURVE ( 'NONE', #17654, #104748, #44752, .T. ) ;
#45610 = CARTESIAN_POINT ( 'NONE',  ( 43.71297783477875498, 485.1278128289774259, -1.116606130291244892 ) ) ;
#45611 = CIRCLE ( 'NONE', #66293, 5.000000000000010658 ) ;
#45612 = DIRECTION ( 'NONE',  ( 0.000000000000000000, 0.000000000000000000, 1.000000000000000000 ) ) ;
#45613 = CARTESIAN_POINT ( 'NONE',  ( 6.214520401345230205, 41.72339003054456441, -70.49303489710376880 ) ) ;
#45614 = CARTESIAN_POINT ( 'NONE',  ( -2.500000000000011990, -30.00000000000000000, -31.87333704504306908 ) ) ;
#45615 = FACE_OUTER_BOUND ( 'NONE', #38605, .T. ) ;
#45616 = DIRECTION ( 'NONE',  ( -0.8191520442889881348, 1.003171929053520186E-16, 0.5735764363510513775 ) ) ;
#45617 = ORIENTED_EDGE ( 'NONE', *, *, #23551, .F. ) ;
#45618 = CARTESIAN_POINT ( 'NONE',  ( 78.70688208539898767, -59.99999999999998579, -28.66616797828253027 ) ) ;
#45620 = CARTESIAN_POINT ( 'NONE',  ( 28.38568808205318916, -49.90851060535624839, 34.42946133055457381 ) ) ;
#45619 = CARTESIAN_POINT ( 'NONE',  ( -69.27297328317253289, -60.00000000000002132, 151.6304908672517513 ) ) ;
#45621 = CARTESIAN_POINT ( 'NONE',  ( 88.26372640434641426, 34.25047185182970111, 44.13186320217322844 ) ) ;
#45622 = ORIENTED_EDGE ( 'NONE', *, *, #38929, .F. ) ;
#45623 = VERTEX_POINT ( 'NONE', #75818 ) ;
#45624 = CARTESIAN_POINT ( 'NONE',  ( -3.301565691951511727, -4.285714285714296246, -25.05982991920904368 ) ) ;
#45625 = CARTESIAN_POINT ( 'NONE',  ( -8.572527594031464315E-16, 60.00000000000000000, 6.999999999999992895 ) ) ;
#45626 = FACE_OUTER_BOUND ( 'NONE', #71623, .T. ) ;
#45627 = CYLINDRICAL_SURFACE ( 'NONE', #93166, 8.000000000000000000 ) ;
#45628 = FILL_AREA_STYLE_COLOUR ( '', #79238 ) ;
#45629 = ORIENTED_EDGE ( 'NONE', *, *, #69466, .T. ) ;
#45630 = CARTESIAN_POINT ( 'NONE',  ( 18.91791044776121211, 47.99999999999999289, 62.18611311450882795 ) ) ;
#45631 = CARTESIAN_POINT ( 'NONE',  ( 97.94761177215855241, -29.99999999999992184, 190.5827337369310897 ) ) ;
#45632 = CARTESIAN_POINT ( 'NONE',  ( -11.69124344503904389, 21.01850713022480477, -7.685374053051364562 ) ) ;
#45633 = CARTESIAN_POINT ( 'NONE',  ( -4.472135954999579610, -85.00000000000000000, 4.000000000000001776 ) ) ;
#45634 = CARTESIAN_POINT ( 'NONE',  ( 81.07608397363662789, -29.99999999999999645, 2.777871215026683771 ) ) ;
#45635 = DIRECTION ( 'NONE',  ( 0.000000000000000000, 0.000000000000000000, 1.000000000000000000 ) ) ;
#45636 = ORIENTED_EDGE ( 'NONE', *, *, #51349, .T. ) ;
#45637 = VERTEX_POINT ( 'NONE', #1371 ) ;
#45638 = EDGE_LOOP ( 'NONE', ( #102307, #6751, #104406, #20131, #76047, #39374 ) ) ;
#45639 = CARTESIAN_POINT ( 'NONE',  ( -12.39578842395470915, 8.431745484731985485, -0.8377008405913517475 ) ) ;
#45640 = CARTESIAN_POINT ( 'NONE',  ( 46.36650669486618881, 1.474610560812782335E-15, 0.000000000000000000 ) ) ;
#45641 = DIRECTION ( 'NONE',  ( -1.000000000000000000, -0.000000000000000000, -0.000000000000000000 ) ) ;
#45642 = CARTESIAN_POINT ( 'NONE',  ( -45.44494901784073448, 426.7272893100207511, 7.514821686672757295 ) ) ;
#45643 = CARTESIAN_POINT ( 'NONE',  ( -1.832167802012315994, -70.57974515660504267, 13.11834054208777189 ) ) ;
#45644 = CARTESIAN_POINT ( 'NONE',  ( -7.618844049274129837, -88.17235898929459381, 2.450177051822847840 ) ) ;
#45645 = CARTESIAN_POINT ( 'NONE',  ( -28.99999999999998934, 0.000000000000000000, 0.000000000000000000 ) ) ;
#45646 = EDGE_LOOP ( 'NONE', ( #105055, #7886, #7430, #32938, #91842 ) ) ;
#45648 = ADVANCED_FACE ( 'NONE', ( #8948 ), #1913, .T. ) ;
#45647 = CARTESIAN_POINT ( 'NONE',  ( 35.90484354297773706, -5.000000000000000000, 0.000000000000000000 ) ) ;
#45649 = EDGE_LOOP ( 'NONE', ( #30665, #9479, #106120, #22966, #80289 ) ) ;
#45650 = CARTESIAN_POINT ( 'NONE',  ( -0.7016502453916991788, 15.23274035658503145, -9.981544566921638051 ) ) ;
#45651 = CARTESIAN_POINT ( 'NONE',  ( 59.06997099859516709, -38.34368760562352918, 93.42682326698202644 ) ) ;
#45652 = FACE_OUTER_BOUND ( 'NONE', #101747, .T. ) ;
#45653 = CARTESIAN_POINT ( 'NONE',  ( 25.14920469222126798, 295.6996425374044293, 2.119131604868921492 ) ) ;
#45654 = CARTESIAN_POINT ( 'NONE',  ( 6.683837171061809634, -7.911893696991943337, -3.558927330633863411E-17 ) ) ;
#45655 = CARTESIAN_POINT ( 'NONE',  ( 63.92674818503888901, -46.43411801997230270, 86.65795160353560789 ) ) ;
#45656 = ORIENTED_EDGE ( 'NONE', *, *, #102133, .F. ) ;
#45657 = LINE ( 'NONE', #19308, #42724 ) ;
#45658 = CARTESIAN_POINT ( 'NONE',  ( -55.98517882506007481, -36.72792837143562394, -35.06346615357033869 ) ) ;
#45659 = CARTESIAN_POINT ( 'NONE',  ( -10.00000000000000355, 0.000000000000000000, -10.00000000000000000 ) ) ;
#45660 = EDGE_CURVE ( 'NONE', #8148, #86629, #51581, .T. ) ;
#45661 = CARTESIAN_POINT ( 'NONE',  ( -8.559508646656370345, 51.55638410492942114, 4.031152949374564365 ) ) ;
#45662 = ORIENTED_EDGE ( 'NONE', *, *, #105830, .T. ) ;
#45663 = SURFACE_STYLE_FILL_AREA ( #69413 ) ;
#45664 = CARTESIAN_POINT ( 'NONE',  ( -1.282512619719470059, -8.391164935524027868, -7.795653906408888112 ) ) ;
#45665 = FACE_OUTER_BOUND ( 'NONE', #33378, .T. ) ;
#45666 = CIRCLE ( 'NONE', #102472, 4.000000000000001776 ) ;
#45667 = CARTESIAN_POINT ( 'NONE',  ( 1.102182119232618897E-15, -20.00000000000001776, 9.000000000000007105 ) ) ;
#45668 = VECTOR ( 'NONE', #92030, 1000.000000000000000 ) ;
#45669 = DIRECTION ( 'NONE',  ( -1.000000000000000000, -1.224606353822377258E-16, -0.000000000000000000 ) ) ;
#45670 = VECTOR ( 'NONE', #35534, 1000.000000000000000 ) ;
#45671 = CARTESIAN_POINT ( 'NONE',  ( 86.71155056234793790, -28.07589402024821723, 185.8220023598428270 ) ) ;
#45672 = VECTOR ( 'NONE', #46621, 1000.000000000000000 ) ;
#45673 = CARTESIAN_POINT ( 'NONE',  ( 43.98364154369441792, 462.7566471324786335, 5.557736785945600388 ) ) ;
#45674 = EDGE_CURVE ( 'NONE', #101774, #40136, #65372, .T. ) ;
#45675 = CARTESIAN_POINT ( 'NONE',  ( -9.252395038874292155, 11.88928468661912596, 5.000000000000317080 ) ) ;
#45676 = CARTESIAN_POINT ( 'NONE',  ( 7.801339272325197527, -6.412685280403009891, -1.788609912539670832 ) ) ;
#45677 = CARTESIAN_POINT ( 'NONE',  ( 1.406919699518766720, -15.40373694258998682, -35.22331805215249290 ) ) ;
#45678 = SURFACE_STYLE_USAGE ( .BOTH. , #76427 ) ;
#45679 = CARTESIAN_POINT ( 'NONE',  ( -6.924711584187146940, 40.92328497002484511, -70.90711766174086961 ) ) ;
#45680 = CARTESIAN_POINT ( 'NONE',  ( 0.000000000000000000, 79.50000000000000000, 0.000000000000000000 ) ) ;
#45681 = CARTESIAN_POINT ( 'NONE',  ( -100.2369334069439617, -30.00000000000000000, 156.2071045385363846 ) ) ;
#45682 = CARTESIAN_POINT ( 'NONE',  ( 7.000000000000000000, -60.71953810598073886, 12.61250543006184088 ) ) ;
#45683 = CARTESIAN_POINT ( 'NONE',  ( 32.39832671728185431, -57.69015538478544158, 46.85044192637200666 ) ) ;
#45685 = CARTESIAN_POINT ( 'NONE',  ( 0.000000000000000000, 304.8518027762758038, -10.00000000000000178 ) ) ;
#45684 = CARTESIAN_POINT ( 'NONE',  ( 9.185096382416778837, 44.03884783307326956, 13.56034858340154337 ) ) ;
#45686 = CARTESIAN_POINT ( 'NONE',  ( -31.48004745648652758, 41.29390966982543176, -67.22208989512388655 ) ) ;
#45687 = LINE ( 'NONE', #78048, #101393 ) ;
#45688 = CARTESIAN_POINT ( 'NONE',  ( 0.000000000000000000, 0.000000000000000000, 0.000000000000000000 ) ) ;
#45689 =( NAMED_UNIT ( * ) SI_UNIT ( $, .STERADIAN. ) SOLID_ANGLE_UNIT ( ) );
#45690 = PLANE ( 'NONE',  #9704 ) ;
#45691 = ORIENTED_EDGE ( 'NONE', *, *, #76195, .F. ) ;
#45692 = CARTESIAN_POINT ( 'NONE',  ( 39.14057804814122221, 485.8491723118621053, -4.975388520153434690 ) ) ;
#45693 =( NAMED_UNIT ( * ) PLANE_ANGLE_UNIT ( ) SI_UNIT ( $, .RADIAN. ) );
#45694 = CARTESIAN_POINT ( 'NONE',  ( -20.66668522848859624, -60.36289094223184293, 34.55967790951763163 ) ) ;
#45695 = CIRCLE ( 'NONE', #105961, 4.000000000000000888 ) ;
#45697 = CARTESIAN_POINT ( 'NONE',  ( 38.81358894280276672, 485.1131561813238591, -4.191378885298274959 ) ) ;
#45696 = CARTESIAN_POINT ( 'NONE',  ( -92.99974329923009009, -60.00000000000000000, 74.19676606278758868 ) ) ;
#45698 = ORIENTED_EDGE ( 'NONE', *, *, #39704, .F. ) ;
#45699 = VERTEX_POINT ( 'NONE', #50991 ) ;
#45700 = CARTESIAN_POINT ( 'NONE',  ( 43.75401118688390767, 486.3173572309543715, 5.908089951475124835 ) ) ;
#45701 = DIRECTION ( 'NONE',  ( -0.7663137714221263108, 0.000000000000000000, 0.6424665000829203887 ) ) ;
#45702 = CARTESIAN_POINT ( 'NONE',  ( 15.17407431220850533, 1.340359594676612611E-15, 0.000000000000000000 ) ) ;
#45703 = VERTEX_POINT ( 'NONE', #35399 ) ;
#45704 = CARTESIAN_POINT ( 'NONE',  ( 32.63942548537020372, 439.6774874792970422, 24.06980402992034485 ) ) ;
#45705 = DIRECTION ( 'NONE',  ( 0.000000000000000000, 0.000000000000000000, 1.000000000000000000 ) ) ;
#45706 = CARTESIAN_POINT ( 'NONE',  ( 103.4866592801870553, -52.71721449814598515, 188.6654185098675214 ) ) ;
#45708 = FACE_OUTER_BOUND ( 'NONE', #35536, .T. ) ;
#45707 = PRESENTATION_STYLE_ASSIGNMENT (( #61920 ) ) ;
#45709 = VERTEX_POINT ( 'NONE', #100086 ) ;
#45710 = COLOUR_RGB ( '', 0.40784314, 0.44705882, 0.49803922) ;
#45711 = EDGE_LOOP ( 'NONE', ( #57276, #75933, #30122, #63553 ) ) ;
#45712 = ADVANCED_FACE ( 'NONE', ( #10019 ), #67735, .T. ) ;
#45713 = EDGE_LOOP ( 'NONE', ( #69287, #97415 ) ) ;
#45714 = CARTESIAN_POINT ( 'NONE',  ( 52.81650669486619165, -4.000000000000000000, 0.000000000000000000 ) ) ;
#45715 = EDGE_CURVE ( 'NONE', #46319, #32781, #26782, .T. ) ;
#45716 = DIRECTION ( 'NONE',  ( 0.000000000000000000, -0.000000000000000000, -1.000000000000000000 ) ) ;
#45717 = ORIENTED_EDGE ( 'NONE', *, *, #30453, .F. ) ;
#45718 = AXIS2_PLACEMENT_3D ( 'NONE', #69127, #95000, #51314 ) ;
#45719 = DIRECTION ( 'NONE',  ( -0.5735764363510497121, 0.8191520442889892450, 1.003171929053521665E-16 ) ) ;
#45720 = CARTESIAN_POINT ( 'NONE',  ( -6.746993971545061974, 41.86978750136238858, -69.53909815634938241 ) ) ;
#45721 = CARTESIAN_POINT ( 'NONE',  ( -72.27154473826411163, -59.99999999998056666, -34.24698835184248225 ) ) ;
#45722 = CARTESIAN_POINT ( 'NONE',  ( 6.944371705245972137, -65.53899691424550156, -3.972324460300565185 ) ) ;
#45723 = CARTESIAN_POINT ( 'NONE',  ( 5.625240605873267796, -59.99999999996141753, -44.94030595675567241 ) ) ;
#45724 = CARTESIAN_POINT ( 'NONE',  ( -8.012318136523624901, -5.000000000000000000, 14.34023295164496403 ) ) ;
#45725 = CARTESIAN_POINT ( 'NONE',  ( -6.315604073028507237, 41.49696650568338896, -58.51869299239607614 ) ) ;
#45726 = CIRCLE ( 'NONE', #7747, 15.43455230191221261 ) ;
#45728 = CARTESIAN_POINT ( 'NONE',  ( 11.28666612630582833, -35.99164038003812038, 29.91485281499912219 ) ) ;
#45727 = CARTESIAN_POINT ( 'NONE',  ( -96.66672766003948425, -59.99999999999999289, 43.67975107286704883 ) ) ;
#45729 = SURFACE_STYLE_FILL_AREA ( #103953 ) ;
#45730 = CARTESIAN_POINT ( 'NONE',  ( -48.77537313921662587, -32.59926516119964646, 46.61647805872783579 ) ) ;
#45731 = CARTESIAN_POINT ( 'NONE',  ( -13.00000000000003730, 249.9999999999999432, 0.000000000000000000 ) ) ;
#45732 = COLOUR_RGB ( '', 0.09019608, 0.27058824, 0.51372549) ;
#45733 = ORIENTED_EDGE ( 'NONE', *, *, #102924, .F. ) ;
#45734 = VECTOR ( 'NONE', #53051, 1000.000000000000000 ) ;
#45735 = CARTESIAN_POINT ( 'NONE',  ( 42.23079339798727716, 460.7352525929352964, 2.726051457480584972 ) ) ;
#45736 = CIRCLE ( 'NONE', #4387, 4.000000000000000888 ) ;
#45737 = AXIS2_PLACEMENT_3D ( 'NONE', #70244, #38943, #88026 ) ;
#45738 = CARTESIAN_POINT ( 'NONE',  ( 0.000000000000000000, 45.00000000000000711, -56.99999999999999289 ) ) ;
#45739 = ORIENTED_EDGE ( 'NONE', *, *, #40900, .T. ) ;
#45740 = CARTESIAN_POINT ( 'NONE',  ( -7.577538872965776662, -12.42143731976112875, 8.412936539037117356 ) ) ;
#45741 = CIRCLE ( 'NONE', #2683, 5.000000000000011546 ) ;
#45742 = EDGE_LOOP ( 'NONE', ( #57353, #98718, #21187, #43819 ) ) ;
#45743 = CARTESIAN_POINT ( 'NONE',  ( 87.88634981426525883, -29.99999999999498002, -17.24999379162776592 ) ) ;
#45744 = CARTESIAN_POINT ( 'NONE',  ( 4.195612334303191915, -48.94124001270402857, 104.4881327927250112 ) ) ;
#45745 = CARTESIAN_POINT ( 'NONE',  ( 6.566498343660657433, 41.80386961834008730, -59.12741152495549102 ) ) ;
#45746 = AXIS2_PLACEMENT_3D ( 'NONE', #49222, #97776, #32554 ) ;
#45747 = CARTESIAN_POINT ( 'NONE',  ( 15.50526908265481296, 41.99999999991779731, -57.69562748401063601 ) ) ;
#45748 = CARTESIAN_POINT ( 'NONE',  ( 96.00844566870836161, -30.00000000000000000, 191.2852847503578460 ) ) ;
#45749 = CARTESIAN_POINT ( 'NONE',  ( 6.849999999999999645, -4.618802153517012954, -8.000000000000001776 ) ) ;
#45750 = VERTEX_POINT ( 'NONE', #76875 ) ;
#45751 = VERTEX_POINT ( 'NONE', #33255 ) ;
#45752 = ORIENTED_EDGE ( 'NONE', *, *, #61667, .F. ) ;
#45753 = CARTESIAN_POINT ( 'NONE',  ( 53.18860290234052712, -56.84141687534781795, 63.26041922679137741 ) ) ;
#45754 = CARTESIAN_POINT ( 'NONE',  ( 43.27530345109022392, 461.7562057072080393, 3.870800370044423566 ) ) ;
#45755 = FACE_OUTER_BOUND ( 'NONE', #14718, .T. ) ;
#45756 = ORIENTED_EDGE ( 'NONE', *, *, #51266, .F. ) ;
#45758 = EDGE_CURVE ( 'NONE', #48079, #72287, #49941, .T. ) ;
#45757 = CARTESIAN_POINT ( 'NONE',  ( -77.86225395006566430, -38.35593842581449309, -27.73772653773013630 ) ) ;
#45759 = ORIENTED_EDGE ( 'NONE', *, *, #42711, .T. ) ;
#45760 = DIRECTION ( 'NONE',  ( 0.5735764363510470476, -0.8191520442889911324, 1.003171929053524007E-16 ) ) ;
#45761 = CARTESIAN_POINT ( 'NONE',  ( 88.88549997972674532, -38.53645272322479087, 200.2533030273275472 ) ) ;
#45762 = CARTESIAN_POINT ( 'NONE',  ( 11.42431500150486023, 20.37266984104267209, 8.170926251056844336 ) ) ;
#45763 = CARTESIAN_POINT ( 'NONE',  ( 82.45637196367515287, -37.86046039678901565, 9.370868085246026880 ) ) ;
#45764 = CARTESIAN_POINT ( 'NONE',  ( 0.000000000000000000, 0.000000000000000000, 0.000000000000000000 ) ) ;
#45765 = CARTESIAN_POINT ( 'NONE',  ( 40.85802308819273776, 440.2752458712913608, 25.57190656468647560 ) ) ;
#45766 = DIRECTION ( 'NONE',  ( -1.000000000000000000, -1.224606353822377258E-16, -0.000000000000000000 ) ) ;
#45767 = DIRECTION ( 'NONE',  ( 0.000000000000000000, -1.000000000000000000, 0.000000000000000000 ) ) ;
#45768 =( BOUNDED_SURFACE ( )  B_SPLINE_SURFACE ( 3, 2, ( 
 ( #34398, #879, #25235 ),
 ( #26843, #24697, #99070 ),
 ( #59180, #91021, #67793 ),
 ( #74799, #83435, #17127 ),
 ( #16580, #18196, #33858 ),
 ( #16042, #9007, #99614 ) ),
 .UNSPECIFIED., .F., .F., .F. ) 
 B_SPLINE_SURFACE_WITH_KNOTS ( ( 4, 2, 4 ),
 ( 3, 3 ),
 ( 0.003199762745115997641, 0.007302762474435750203, 0.01140576220375550190 ),
 ( 0.000000000000000000, 1.000000000000000000 ),
 .UNSPECIFIED. ) 
 GEOMETRIC_REPRESENTATION_ITEM ( )  RATIONAL_B_SPLINE_SURFACE ( (
 ( 1.000000000000000000, 0.8047731410850428313, 1.000000000000000000),
 ( 1.000000000000000000, 0.8125552299159717329, 1.000000000000000000),
 ( 1.000000000000000000, 0.8191520442885290576, 1.000000000000000000),
 ( 1.000000000000000000, 0.8191520442894507648, 1.000000000000000000),
 ( 1.000000000000000000, 0.8125552299152797309, 1.000000000000000000),
 ( 1.000000000000000000, 0.8047731410850426093, 1.000000000000000000) ) ) 
 REPRESENTATION_ITEM ( '' )  SURFACE ( )  );
#45769 = VECTOR ( 'NONE', #64139, 1000.000000000000000 ) ;
#45770 =( NAMED_UNIT ( * ) PLANE_ANGLE_UNIT ( ) SI_UNIT ( $, .RADIAN. ) );
#45771 = ORIENTED_EDGE ( 'NONE', *, *, #68542, .F. ) ;
#45772 = ADVANCED_FACE ( 'NONE', ( #62314 ), #5466, .F. ) ;
#45773 = EDGE_CURVE ( 'NONE', #12690, #36732, #10230, .T. ) ;
#45774 = CARTESIAN_POINT ( 'NONE',  ( -8.000000000000000000, -10.43750000409677092, -9.797174393178825657E-16 ) ) ;
#45775 = CARTESIAN_POINT ( 'NONE',  ( -36.71055512278706345, 461.9588081675148601, 3.153288429120979508 ) ) ;
#45776 = CARTESIAN_POINT ( 'NONE',  ( -3.227781575335565645, 36.26785195737000578, 5.000000000000000888 ) ) ;
#45777 = ORIENTED_EDGE ( 'NONE', *, *, #11777, .F. ) ;
#45778 = FACE_OUTER_BOUND ( 'NONE', #1066, .T. ) ;
#45779 = CARTESIAN_POINT ( 'NONE',  ( -36.51296643074312698, 309.5443268485549311, 13.44797477174485856 ) ) ;
#45780 = CARTESIAN_POINT ( 'NONE',  ( 4.154708322984369194E-08, -57.67120202538961138, 41.61186700422869933 ) ) ;
#45781 = CARTESIAN_POINT ( 'NONE',  ( 0.06682554136337581774, -4.993536075455411449, 4.350941807883112133 ) ) ;
#45782 = CARTESIAN_POINT ( 'NONE',  ( -5.656854249492381470, -19.06249999999999289, 5.656854249492379694 ) ) ;
#45783 = CARTESIAN_POINT ( 'NONE',  ( 1.046656298439633925, -14.82702095649888641, 34.47215281706392886 ) ) ;
#45784 = DIRECTION ( 'NONE',  ( 0.000000000000000000, 0.000000000000000000, 1.000000000000000000 ) ) ;
#45785 = VERTEX_POINT ( 'NONE', #38061 ) ;
#45786 = CARTESIAN_POINT ( 'NONE',  ( 85.21129371257987373, -32.24359312048367343, 179.1469130256770086 ) ) ;
#45787 = CARTESIAN_POINT ( 'NONE',  ( -49.27997219161970577, 7.868281554635428776, 15.62830927991589647 ) ) ;
#45788 = ADVANCED_FACE ( 'NONE', ( #70917 ), #60247, .T. ) ;
#45789 = AXIS2_PLACEMENT_3D ( 'NONE', #53786, #21452, #22522 ) ;
#45790 = ORIENTED_EDGE ( 'NONE', *, *, #61001, .F. ) ;
#45791 = CARTESIAN_POINT ( 'NONE',  ( -98.39902859776117339, -60.15518905392604410, 105.6211524846448526 ) ) ;
#45792 = EDGE_CURVE ( 'NONE', #79214, #47612, #13693, .T. ) ;
#45793 = DIRECTION ( 'NONE',  ( 0.000000000000000000, -1.000000000000000000, 0.000000000000000000 ) ) ;
#45794 = CARTESIAN_POINT ( 'NONE',  ( -42.88690168185247842, 465.8389250139255751, 12.02233836084348262 ) ) ;
#45795 = CARTESIAN_POINT ( 'NONE',  ( -30.80770627799311967, 8.073552547385885347, 41.40953488888247591 ) ) ;
#45796 = DIRECTION ( 'NONE',  ( -1.000000000000000000, -0.000000000000000000, -0.000000000000000000 ) ) ;
#45797 =( BOUNDED_SURFACE ( )  B_SPLINE_SURFACE ( 3, 2, ( 
 ( #50976, #43973, #58572 ),
 ( #42910, #82832, #84438 ),
 ( #17586, #1896, #1357 ),
 ( #101678, #101143, #76861 ),
 ( #100604, #26240, #10528 ),
 ( #2968, #93054, #34851 ) ),
 .UNSPECIFIED., .F., .F., .F. ) 
 B_SPLINE_SURFACE_WITH_KNOTS ( ( 4, 2, 4 ),
 ( 3, 3 ),
 ( 0.1175780374352882046, 0.1311840582298423041, 0.1447900790243964175 ),
 ( 0.3700809061630451202, 1.000000000000000000 ),
 .UNSPECIFIED. ) 
 GEOMETRIC_REPRESENTATION_ITEM ( )  RATIONAL_B_SPLINE_SURFACE ( (
 ( 0.8634406101731282313, 0.8155006276293699230, 1.000000000000000000),
 ( 0.8634404976690126521, 0.8155004756300181512, 1.000000000000000000),
 ( 0.8634404321542359373, 0.8155003871158911233, 1.000000000000000000),
 ( 0.8634404611618202718, 0.8155004263067597847, 1.000000000000000000),
 ( 0.8634405542443903681, 0.8155005520665173924, 1.000000000000000000),
 ( 0.8634406634513454026, 0.8155006996112208473, 1.000000000000000000) ) ) 
 REPRESENTATION_ITEM ( '' )  SURFACE ( )  );
#45798 = ADVANCED_FACE ( 'NONE', ( #5128 ), #70533, .T. ) ;
#45799 = AXIS2_PLACEMENT_3D ( 'NONE', #84523, #44060, #68882 ) ;
#45800 =( NAMED_UNIT ( * ) SI_UNIT ( $, .STERADIAN. ) SOLID_ANGLE_UNIT ( ) );
#45801 = AXIS2_PLACEMENT_3D ( 'NONE', #31696, #97453, #32220 ) ;
#45802 = LINE ( 'NONE', #78679, #5493 ) ;
#45803 = CARTESIAN_POINT ( 'NONE',  ( 1.238781280732904611, -2.150544339304492541E-15, 101.3451024322571641 ) ) ;
#45804 = CARTESIAN_POINT ( 'NONE',  ( 33.82190865419818948, -23.50910416088391841, 33.09154993403522838 ) ) ;
#45805 = ADVANCED_FACE ( 'NONE', ( #4597 ), #62838, .T. ) ;
#45807 = CARTESIAN_POINT ( 'NONE',  ( -11.40270841904595933, 18.20400957074633297, 8.563861102918378876 ) ) ;
#45806 = DIRECTION ( 'NONE',  ( -1.000000000000000000, -0.000000000000000000, -0.000000000000000000 ) ) ;
#45808 = EDGE_CURVE ( 'NONE', #90586, #53794, #54177, .T. ) ;
#45809 = CARTESIAN_POINT ( 'NONE',  ( 0.9108375753702777633, 296.5938209094946956, -10.00058097679032265 ) ) ;
#45810 =( GEOMETRIC_REPRESENTATION_CONTEXT ( 3 ) GLOBAL_UNCERTAINTY_ASSIGNED_CONTEXT ( ( #85407 ) ) GLOBAL_UNIT_ASSIGNED_CONTEXT ( ( #54293, #62958, #36598 ) ) REPRESENTATION_CONTEXT ( 'NONE', 'WORKASPACE' ) );
#45811 = SURFACE_STYLE_FILL_AREA ( #46340 ) ;
#45812 = EDGE_CURVE ( 'NONE', #25325, #53932, #93611, .T. ) ;
#45813 = CARTESIAN_POINT ( 'NONE',  ( 9.090909090909086387, 15.00000000000000000, -4.165977904505313134 ) ) ;
#45814 = CARTESIAN_POINT ( 'NONE',  ( -14.29190075644363489, 21.26710225492988116, -5.626279437295411689 ) ) ;
#45815 = AXIS2_PLACEMENT_3D ( 'NONE', #69741, #53551, #19104 ) ;
#45816 = CIRCLE ( 'NONE', #95795, 9.500000000000000000 ) ;
#45817 = CARTESIAN_POINT ( 'NONE',  ( -89.12526225705758520, -38.00000000000000000, 73.22758371480502149 ) ) ;
#45818 = PRODUCT_DEFINITION_SHAPE ( 'NONE', 'NONE',  #106793 ) ;
#45819 = EDGE_CURVE ( 'NONE', #26769, #57292, #102222, .T. ) ;
#45820 = ORIENTED_EDGE ( 'NONE', *, *, #105012, .T. ) ;
#45821 = CARTESIAN_POINT ( 'NONE',  ( -9.918585201507950089, -2.743081709124135070, 15.35584857294453442 ) ) ;
#45822 = DIRECTION ( 'NONE',  ( 0.000000000000000000, -1.000000000000000000, 0.000000000000000000 ) ) ;
#45823 = CIRCLE ( 'NONE', #73358, 11.00000000000000000 ) ;
#45824 = CARTESIAN_POINT ( 'NONE',  ( -42.50585811106670064, 460.9576338508424556, 2.953927975892561619 ) ) ;
#45825 = CARTESIAN_POINT ( 'NONE',  ( 6.360191607006829173, -47.40891213495661560, -34.69802138687305160 ) ) ;
#45826 = ORIENTED_EDGE ( 'NONE', *, *, #106145, .F. ) ;
#45827 = CARTESIAN_POINT ( 'NONE',  ( -43.96303167068774087, 462.7533654737459301, 5.566168170703541307 ) ) ;
#45828 = CARTESIAN_POINT ( 'NONE',  ( 0.000000000000000000, -5.629165124598853431, -3.249999999999994227 ) ) ;
#45829 = AXIS2_PLACEMENT_3D ( 'NONE', #49066, #80912, #64741 ) ;
#45830 = ORIENTED_EDGE ( 'NONE', *, *, #65176, .F. ) ;
#45831 = CARTESIAN_POINT ( 'NONE',  ( 30.23165830866633996, 7.786015354292205259, -41.98067155130507189 ) ) ;
#45832 = DIRECTION ( 'NONE',  ( 0.000000000000000000, 0.000000000000000000, 1.000000000000000000 ) ) ;
#45833 = CARTESIAN_POINT ( 'NONE',  ( -94.40663350262447295, -60.00000000000000711, 44.56717037654195224 ) ) ;
#45834 = ORIENTED_EDGE ( 'NONE', *, *, #89046, .T. ) ;
#45835 = CARTESIAN_POINT ( 'NONE',  ( -7.305752995881348966, 41.99999999999663913, -58.79284008965307606 ) ) ;
#45836 = FACE_OUTER_BOUND ( 'NONE', #44875, .T. ) ;
#45837 = CARTESIAN_POINT ( 'NONE',  ( -9.537927238823508347, 27.35373142881821096, -3.010735687602430488 ) ) ;
#45839 = CARTESIAN_POINT ( 'NONE',  ( 0.000000000000000000, 0.000000000000000000, 0.000000000000000000 ) ) ;
#45838 = CARTESIAN_POINT ( 'NONE',  ( -5.656854249492381470, -26.56249999999999645, 5.656854249492379694 ) ) ;
#45840 = CARTESIAN_POINT ( 'NONE',  ( -81.62634306135213080, -49.94837975070949909, 173.6806837566333286 ) ) ;
#45841 = ORIENTED_EDGE ( 'NONE', *, *, #74446, .F. ) ;
#45842 = CARTESIAN_POINT ( 'NONE',  ( -4.418451808487692922, 0.000000000000000000, 16.46925340495486267 ) ) ;
#45843 = ORIENTED_EDGE ( 'NONE', *, *, #80846, .T. ) ;
#45844 = AXIS2_PLACEMENT_3D ( 'NONE', #80461, #63780, #13070 ) ;
#45845 = EDGE_LOOP ( 'NONE', ( #57116, #87497, #2714, #43507 ) ) ;
#45846 = CARTESIAN_POINT ( 'NONE',  ( -16.28378713909053843, -4.332661967060385422, -8.128475758626676040 ) ) ;
#45847 = EDGE_CURVE ( 'NONE', #83001, #98221, #87118, .T. ) ;
#45848 = ORIENTED_EDGE ( 'NONE', *, *, #36180, .F. ) ;
#45849 = CARTESIAN_POINT ( 'NONE',  ( -32.86204548368812084, 471.3237325390174419, 9.718390497932560379 ) ) ;
#45850 = CARTESIAN_POINT ( 'NONE',  ( -101.8692865417259696, -57.67122770170253432, 80.25822756173465677 ) ) ;
#45851 = CARTESIAN_POINT ( 'NONE',  ( 44.46823338009918558, 6.123233995736772199E-16, -5.000000000000001776 ) ) ;
#45852 = CARTESIAN_POINT ( 'NONE',  ( 43.52576059139532560, 465.2718218682666702, 9.360783428388922189 ) ) ;
#45853 = CARTESIAN_POINT ( 'NONE',  ( -9.381593208289373820, 102.9856136188049334, -3.465401811657803588 ) ) ;
#45854 = CARTESIAN_POINT ( 'NONE',  ( -13.90377727273328645, -50.40522912573743497, 25.34355585267129740 ) ) ;
#45855 = DIRECTION ( 'NONE',  ( 0.000000000000000000, 0.3548932414479700759, 0.9349068334195407282 ) ) ;
#45856 = EDGE_CURVE ( 'NONE', #36720, #53278, #53667, .T. ) ;
#45857 = CARTESIAN_POINT ( 'NONE',  ( 56.79302105626919683, -14.21045842199427867, -31.02814365720875500 ) ) ;
#45858 = CARTESIAN_POINT ( 'NONE',  ( -64.82027869498183748, -30.00000000000004619, 107.4038593739741430 ) ) ;
#45859 = CARTESIAN_POINT ( 'NONE',  ( -55.06067097896985274, -53.38329654548371650, 66.16146764719466944 ) ) ;
#45860 = ORIENTED_EDGE ( 'NONE', *, *, #7287, .F. ) ;
#45861 = FACE_OUTER_BOUND ( 'NONE', #82699, .T. ) ;
#45862 = ORIENTED_EDGE ( 'NONE', *, *, #99777, .T. ) ;
#45863 = CARTESIAN_POINT ( 'NONE',  ( -100.0726282877276958, -45.25679602138151125, 192.5320261463655811 ) ) ;
#45864 = CARTESIAN_POINT ( 'NONE',  ( 32.86086508068095213, 472.2680268995274560, 9.428505756553761330 ) ) ;
#45865 = ORIENTED_EDGE ( 'NONE', *, *, #94792, .T. ) ;
#45866 = CARTESIAN_POINT ( 'NONE',  ( 19.36342679109174370, 49.91170501117324676, 61.12863474974990652 ) ) ;
#45867 = COLOUR_RGB ( '', 0.66274510, 0.83137255, 0.94901961) ;
#45868 = CARTESIAN_POINT ( 'NONE',  ( -7.188101187500002709, -12.68750000204838635, 2.977408999572648707 ) ) ;
#45869 = CARTESIAN_POINT ( 'NONE',  ( -4.545178794966575619E-15, 5.948846446048900560, -2.696295709017757503 ) ) ;
#45870 = DIRECTION ( 'NONE',  ( -1.000000000000000000, -1.224606353822377258E-16, -0.000000000000000000 ) ) ;
#45871 = CARTESIAN_POINT ( 'NONE',  ( 7.343637806710343163, -82.55636878099383580, 3.177475076494674866 ) ) ;
#45872 = CARTESIAN_POINT ( 'NONE',  ( 69.74927355208504309, -30.00000000000000355, 94.52352744978905719 ) ) ;
#45873 = CARTESIAN_POINT ( 'NONE',  ( -10.28624191511816832, 43.25714326066847804, -15.40779740156204980 ) ) ;
#45874 = CARTESIAN_POINT ( 'NONE',  ( 0.000000000000000000, 0.000000000000000000, 0.000000000000000000 ) ) ;
#45875 = ADVANCED_FACE ( 'NONE', ( #53151 ), #38511, .T. ) ;
#45876 = CARTESIAN_POINT ( 'NONE',  ( -33.74271564777244237, 484.1802673187709729, 2.058285076122319701 ) ) ;
#45877 = UNCERTAINTY_MEASURE_WITH_UNIT (LENGTH_MEASURE( 1.000000000000000082E-05 ), #60632, 'distance_accuracy_value', 'NONE');
#45878 = B_SPLINE_CURVE_WITH_KNOTS ( 'NONE', 3,
 ( #42053, #5839, #13924, #45781, #70592, #38250, #71113, #4793 ),
 .UNSPECIFIED., .F., .F.,
 ( 4, 2, 2, 4 ),
 ( 0.003797433802554455416, 0.004743183970586251769, 0.005688934138618045519, 0.007580434474681635622 ),
 .UNSPECIFIED. ) ;
#45879 = CARTESIAN_POINT ( 'NONE',  ( -29.64972134613275045, -49.91194892834956676, 34.84693478522385846 ) ) ;
#45880 = ORIENTED_EDGE ( 'NONE', *, *, #81625, .F. ) ;
#45881 = VERTEX_POINT ( 'NONE', #82465 ) ;
#45882 = CARTESIAN_POINT ( 'NONE',  ( 48.64717611995057212, -42.97917151878713327, 49.69220790373555730 ) ) ;
#45883 = MECHANICAL_DESIGN_GEOMETRIC_PRESENTATION_REPRESENTATION (  '', ( #101162 ), #97754 ) ;
#45884 = DIRECTION ( 'NONE',  ( -1.000000000000000000, -1.224606353822377258E-16, -0.000000000000000000 ) ) ;
#45885 = PLANE ( 'NONE',  #65149 ) ;
#45887 = EDGE_CURVE ( 'NONE', #81895, #56180, #65218, .T. ) ;
#45886 = CARTESIAN_POINT ( 'NONE',  ( -104.5817897493230788, -38.40156824060414209, 197.8926955786276949 ) ) ;
#45888 = VECTOR ( 'NONE', #28013, 1000.000000000000000 ) ;
#45889 = VERTEX_POINT ( 'NONE', #91108 ) ;
#45890 = CARTESIAN_POINT ( 'NONE',  ( 91.31362265674661671, -38.40000453515457224, -10.25727057701513623 ) ) ;
#45891 =( NAMED_UNIT ( * ) PLANE_ANGLE_UNIT ( ) SI_UNIT ( $, .RADIAN. ) );
#45892 = CARTESIAN_POINT ( 'NONE',  ( -18.93028278895031136, 49.10155414044731970, 62.09492669842853729 ) ) ;
#45894 = CARTESIAN_POINT ( 'NONE',  ( 10.28624191511840458, 43.99263840937192782, 12.90779740156148847 ) ) ;
#45893 = CIRCLE ( 'NONE', #90691, 4.000000000000003553 ) ;
#45895 = AXIS2_PLACEMENT_3D ( 'NONE', #106135, #83472, #48961 ) ;
#45896 = CARTESIAN_POINT ( 'NONE',  ( 6.060122754898491948, 40.55658532241655223, -71.16215414250133620 ) ) ;
#45897 = CARTESIAN_POINT ( 'NONE',  ( -32.85046847605558185, 435.2650770123868256, 16.49042918348624553 ) ) ;
#45898 = SURFACE_SIDE_STYLE ('',( #14558 ) ) ;
#45899 = FILL_AREA_STYLE_COLOUR ( '', #53836 ) ;
#45900 = CARTESIAN_POINT ( 'NONE',  ( 108.8408623652823337, -60.00000000000000711, 194.0362837791606978 ) ) ;
#45901 = VECTOR ( 'NONE', #70792, 1000.000000000000114 ) ;
#45902 = CONICAL_SURFACE ( 'NONE', #106150, 8.000000000000000000, 1.047197551196600296 ) ;
#45903 = CARTESIAN_POINT ( 'NONE',  ( -15.50566716382173738, 34.92505762992946927, 22.93027035652926315 ) ) ;
#45904 = VERTEX_POINT ( 'NONE', #17217 ) ;
#45905 = CARTESIAN_POINT ( 'NONE',  ( -26.62232737841250696, 304.7806955871358809, -9.577114476195255577 ) ) ;
#45906 = ADVANCED_FACE ( 'NONE', ( #16666 ), #86114, .T. ) ;
#45907 = DIRECTION ( 'NONE',  ( 1.000000000000000000, -0.000000000000000000, -0.000000000000000000 ) ) ;
#45908 = CARTESIAN_POINT ( 'NONE',  ( -7.986711519608433285, 26.02638096376566068, -0.5300249774147565152 ) ) ;
#45909 = EDGE_LOOP ( 'NONE', ( #4301, #1153, #19297, #100147, #98476 ) ) ;
#45911 = CARTESIAN_POINT ( 'NONE',  ( 5.223130590452879751, 7.187516661514774974, -27.63920076787009350 ) ) ;
#45910 = CARTESIAN_POINT ( 'NONE',  ( -91.43450980527380523, -38.37461378256361400, -4.864083082636263100 ) ) ;
#45912 = CARTESIAN_POINT ( 'NONE',  ( 12.34835181856063002, -4.332967528434596538, -12.86601580078908214 ) ) ;
#45913 = CARTESIAN_POINT ( 'NONE',  ( -4.028951842967194885, -3.000000000000000444, -6.990291106834064294 ) ) ;
#45914 = CARTESIAN_POINT ( 'NONE',  ( -5.082755093536326818, -12.59375000204838635, 5.082755093536325042 ) ) ;
#45915 = CARTESIAN_POINT ( 'NONE',  ( 0.000000000000000000, -5.000000000000002665, -75.00000000000001421 ) ) ;
#45916 = PRODUCT_DEFINITION_SHAPE ( 'NONE', 'NONE',  #103634 ) ;
#45917 = DIRECTION ( 'NONE',  ( 0.000000000000000000, -1.000000000000000000, 0.000000000000000000 ) ) ;
#45919 = ORIENTED_EDGE ( 'NONE', *, *, #68885, .F. ) ;
#45918 = FILL_AREA_STYLE_COLOUR ( '', #97736 ) ;
#45920 = CARTESIAN_POINT ( 'NONE',  ( 82.17288844096735545, -46.46110024266576488, 173.2037556483296896 ) ) ;
#45922 = CIRCLE ( 'NONE', #87269, 3.309500000000001663 ) ;
#45921 = CARTESIAN_POINT ( 'NONE',  ( 7.953361656945785008, 53.62094058914818362, 1.444447458290428860E-31 ) ) ;
#45923 = B_SPLINE_CURVE_WITH_KNOTS ( 'NONE', 3,
 ( #28805, #87009, #88061, #14141 ),
 .UNSPECIFIED., .F., .F.,
 ( 4, 4 ),
 ( 0.000000000000000000, 0.0001235227585958290715 ),
 .UNSPECIFIED. ) ;
#45924 = CARTESIAN_POINT ( 'NONE',  ( 37.56673239365870387, 27.60449318992555945, 13.45617127780999134 ) ) ;
#45925 = ORIENTED_EDGE ( 'NONE', *, *, #40958, .F. ) ;
#45926 = DIRECTION ( 'NONE',  ( -1.000000000000000000, -1.224606353822377258E-16, -0.000000000000000000 ) ) ;
#45927 = CARTESIAN_POINT ( 'NONE',  ( -47.57308385268305528, 17.76309546253597560, 14.43907613026821757 ) ) ;
#45928 = CARTESIAN_POINT ( 'NONE',  ( 5.656854249492380582, -28.81249999999999289, -5.656854249492379694 ) ) ;
#45929 = DIRECTION ( 'NONE',  ( 0.000000000000000000, -1.000000000000000000, 0.000000000000000000 ) ) ;
#45930 = DIRECTION ( 'NONE',  ( -1.000000000000000000, -1.224606353822377258E-16, -0.000000000000000000 ) ) ;
#45931 = DIRECTION ( 'NONE',  ( 0.000000000000000000, 0.000000000000000000, 1.000000000000000000 ) ) ;
#45932 = EDGE_CURVE ( 'NONE', #74451, #64739, #31804, .T. ) ;
#45933 = VERTEX_POINT ( 'NONE', #15597 ) ;
#45934 = CARTESIAN_POINT ( 'NONE',  ( -9.756537947068297356, 294.6499343785214933, 2.217872953681543802 ) ) ;
#45935 = CARTESIAN_POINT ( 'NONE',  ( -5.000000000000000888, -43.09265016210607513, 0.3552338647229656421 ) ) ;
#45936 = DIRECTION ( 'NONE',  ( -0.000000000000000000, 1.000000000000000000, -1.224646799147353207E-16 ) ) ;
#45937 = ADVANCED_FACE ( 'NONE', ( #82997 ), #53286, .T. ) ;
#45939 = CARTESIAN_POINT ( 'NONE',  ( -13.72104688144364992, 3.071979568406547401, -6.016404424592845857 ) ) ;
#45938 = CARTESIAN_POINT ( 'NONE',  ( 0.000000000000000000, 0.000000000000000000, 0.000000000000000000 ) ) ;
#45940 = CARTESIAN_POINT ( 'NONE',  ( -1.320432766682874540E-15, -21.03125000204838457, 7.188101187500000044 ) ) ;
#45941 = DIRECTION ( 'NONE',  ( 0.000000000000000000, -1.000000000000000000, 0.000000000000000000 ) ) ;
#45942 = CARTESIAN_POINT ( 'NONE',  ( 5.062179317057940331, -5.000000000000000000, -8.716351559230457013 ) ) ;
#45943 = AXIS2_PLACEMENT_3D ( 'NONE', #12595, #87573, #54638 ) ;
#45944 = ORIENTED_EDGE ( 'NONE', *, *, #20913, .F. ) ;
#45945 = EDGE_CURVE ( 'NONE', #104544, #101499, #6840, .T. ) ;
#45946 = DIRECTION ( 'NONE',  ( -0.8139476909583208686, 0.000000000000000000, 0.5809381691571124939 ) ) ;
#45947 = DIRECTION ( 'NONE',  ( -0.000000000000000000, 0.5000000000000009992, 0.8660254037844380415 ) ) ;
#45948 = CARTESIAN_POINT ( 'NONE',  ( -8.570032633590477289, 24.09669418279240816, -1.270257828436642457E-12 ) ) ;
#45949 = LINE ( 'NONE', #55074, #29202 ) ;
#45950 = B_SPLINE_CURVE_WITH_KNOTS ( 'NONE', 3,
 ( #556, #66947, #87910, #29191, #52879, #36213, #54439, #12935, #46385, #79274, #85806, #3273, #53420, #104073, #4330, #11880, #29704, #95462 ),
 .UNSPECIFIED., .F., .F.,
 ( 4, 2, 2, 2, 2, 2, 2, 2, 4 ),
 ( 0.007125849503216023610, 0.007630052828287927844, 0.008134256153359832944, 0.008638459478431736310, 0.009142662803503641411, 0.009646866128575546512, 0.01015106945364745161, 0.01065527277871935498, 0.01115947610379126008 ),
 .UNSPECIFIED. ) ;
#45951 = DIRECTION ( 'NONE',  ( 0.000000000000000000, -0.000000000000000000, -1.000000000000000000 ) ) ;
#45952 = EDGE_LOOP ( 'NONE', ( #68848, #95264, #10613, #88956, #93136 ) ) ;
#45953 = DIRECTION ( 'NONE',  ( 1.000000000000000000, 1.224606353822377258E-16, 0.000000000000000000 ) ) ;
#45954 = AXIS2_PLACEMENT_3D ( 'NONE', #82011, #24878, #16764 ) ;
#45955 = COLOUR_RGB ( '', 0.66274510, 0.83137255, 0.94901961) ;
#45956 = ORIENTED_EDGE ( 'NONE', *, *, #16808, .F. ) ;
#45957 =( BOUNDED_SURFACE ( )  B_SPLINE_SURFACE ( 3, 2, ( 
 ( #51726, #104528, #47356 ),
 ( #103475, #22596, #80244 ),
 ( #95387, #6350, #5321 ),
 ( #79199, #88888, #95924 ),
 ( #4787, #105078, #22050 ),
 ( #30143, #78649, #14442 ),
 ( #63027, #31217, #13916 ),
 ( #71625, #39291, #72170 ),
 ( #45775, #71106, #64102 ),
 ( #38244, #14979, #54908 ),
 ( #37725, #96979, #87835 ),
 ( #23112, #63569, #30682 ) ),
 .UNSPECIFIED., .F., .F., .T. ) 
 B_SPLINE_SURFACE_WITH_KNOTS ( ( 4, 2, 2, 2, 2, 4 ),
 ( 3, 3 ),
 ( 0.0007440794992175734507, 0.002885623262178780343, 0.003956395143659383572, 0.005027167025139987235, 0.007168710788101193693, 0.009310254551062401018 ),
 ( 0.000000000000000000, 1.000000000000000000 ),
 .UNSPECIFIED. ) 
 GEOMETRIC_REPRESENTATION_ITEM ( )  RATIONAL_B_SPLINE_SURFACE ( (
 ( 1.000000000000000000, 0.7301269460246678777, 1.000000000000000000),
 ( 1.000000000000000000, 0.7402241639605217083, 1.000000000000000000),
 ( 1.000000000000000000, 0.7526921830315997930, 1.000000000000000000),
 ( 1.000000000000000000, 0.7732044076585372627, 1.000000000000000000),
 ( 1.000000000000000000, 0.7803010015268321276, 1.000000000000000000),
 ( 1.000000000000000000, 0.7944988828236099199, 1.000000000000000000),
 ( 1.000000000000000000, 0.8016356104975063124, 1.000000000000000000),
 ( 1.000000000000000000, 0.8228127629107910845, 1.000000000000000000),
 ( 1.000000000000000000, 0.8367252785235839152, 1.000000000000000000),
 ( 1.000000000000000000, 0.8612815991380949887, 1.000000000000000000),
 ( 1.000000000000000000, 0.8720645852075524784, 1.000000000000000000),
 ( 1.000000000000000000, 0.8806660624990084729, 1.000000000000000000) ) ) 
 REPRESENTATION_ITEM ( '' )  SURFACE ( )  );
#45958 = CARTESIAN_POINT ( 'NONE',  ( -27.10511071441183262, 34.47735702144344572, 10.05698433968616001 ) ) ;
#45959 = CARTESIAN_POINT ( 'NONE',  ( -42.34743190980356076, 39.51742533357018772, -49.83185399579645036 ) ) ;
#45960 = CARTESIAN_POINT ( 'NONE',  ( -17.15361759915034412, 37.01177862285504006, 21.87054431129721621 ) ) ;
#45961 = UNCERTAINTY_MEASURE_WITH_UNIT (LENGTH_MEASURE( 1.000000000000000082E-05 ), #67594, 'distance_accuracy_value', 'NONE');
#45962 = CARTESIAN_POINT ( 'NONE',  ( -108.5389370269662805, -59.99999999999999289, 194.6443121377485852 ) ) ;
#45963 =( GEOMETRIC_REPRESENTATION_CONTEXT ( 3 ) GLOBAL_UNCERTAINTY_ASSIGNED_CONTEXT ( ( #34365 ) ) GLOBAL_UNIT_ASSIGNED_CONTEXT ( ( #86523, #40060, #88092 ) ) REPRESENTATION_CONTEXT ( 'NONE', 'WORKASPACE' ) );
#45964 = CONICAL_SURFACE ( 'NONE', #9830, 5.000000000000001776, 0.9599310885968803664 ) ;
#45965 = CARTESIAN_POINT ( 'NONE',  ( 33.09999999999999432, 3.309500000000003439, 4.052968581778167743E-16 ) ) ;
#45966 = TOROIDAL_SURFACE ( 'NONE', #51175, 3.500000000000000000, 0.5000000000000000000 ) ;
#45967 = VECTOR ( 'NONE', #67354, 1000.000000000000000 ) ;
#45968 = CARTESIAN_POINT ( 'NONE',  ( 13.48661044872033266, 304.5494699462643666, -9.064266023533495087 ) ) ;
#45969 = CARTESIAN_POINT ( 'NONE',  ( 5.618297568691034805, 54.12964757744262556, -6.031152949374448013 ) ) ;
#45970 = CARTESIAN_POINT ( 'NONE',  ( -82.78613966356304843, -50.04786190543876501, 182.2101918582118572 ) ) ;
#45971 = CARTESIAN_POINT ( 'NONE',  ( 34.62244506083275297, 42.65563576728210649, -62.90200742928525557 ) ) ;
#45972 = AXIS2_PLACEMENT_3D ( 'NONE', #75821, #35945, #52598 ) ;
#45973 = VERTEX_POINT ( 'NONE', #16129 ) ;
#45974 = CARTESIAN_POINT ( 'NONE',  ( 44.53215874387051088, 465.2814620064199858, 9.437388644045839214 ) ) ;
#45975 = EDGE_CURVE ( 'NONE', #37591, #72871, #20265, .T. ) ;
#45976 = CARTESIAN_POINT ( 'NONE',  ( 4.595881407952571607, -66.06625433201323006, -3.857520671226067233 ) ) ;
#45977 = CARTESIAN_POINT ( 'NONE',  ( -83.71838643811501868, -45.26559428471287561, 15.97475021176123278 ) ) ;
#45978 = DIRECTION ( 'NONE',  ( -1.000000000000000000, 0.000000000000000000, 0.000000000000000000 ) ) ;
#45979 = CARTESIAN_POINT ( 'NONE',  ( -3.794165308086080213, 18.81398966773962300, -5.000000000000000000 ) ) ;
#45980 = CARTESIAN_POINT ( 'NONE',  ( 8.642223818515795131, 129.6034357518201148, -4.999999999999999112 ) ) ;
#45981 = PRESENTATION_STYLE_ASSIGNMENT (( #55104 ) ) ;
#45982 = CARTESIAN_POINT ( 'NONE',  ( 36.40416150948652785, 42.00000000008225953, 47.37019975542485639 ) ) ;
#45983 = EDGE_CURVE ( 'NONE', #32846, #3555, #18988, .T. ) ;
#45984 = CARTESIAN_POINT ( 'NONE',  ( 104.0082629745172653, -14.21045842199441012, 192.0643512960946282 ) ) ;
#45985 = CARTESIAN_POINT ( 'NONE',  ( -55.68167212273443312, 51.11204936430952017, -27.84083606136722011 ) ) ;
#45986 = CARTESIAN_POINT ( 'NONE',  ( -102.6949714452557885, -14.21045842199446518, 129.2658233771313974 ) ) ;
#45987 = CARTESIAN_POINT ( 'NONE',  ( -63.59055291699712598, -56.86855241622866686, 91.13439659791259828 ) ) ;
#45988 = ORIENTED_EDGE ( 'NONE', *, *, #12477, .T. ) ;
#45989 = CARTESIAN_POINT ( 'NONE',  ( 61.99214259692967488, 39.42505830967482439, -19.76944376150414939 ) ) ;
#45990 = CARTESIAN_POINT ( 'NONE',  ( 55.94905262869426110, -59.99999999988309440, 95.40321447124708243 ) ) ;
#45991 = VERTEX_POINT ( 'NONE', #93219 ) ;
#45992 = CARTESIAN_POINT ( 'NONE',  ( -10.00000000000000355, 85.00000000000000000, 4.000000000000000000 ) ) ;
#45993 = CARTESIAN_POINT ( 'NONE',  ( 5.082755093536324154, -21.21875000204838813, 5.082755093536326818 ) ) ;
#45994 = CARTESIAN_POINT ( 'NONE',  ( 32.22503847990208925, 485.9064490506207221, 4.829857536092688974 ) ) ;
#45995 = ORIENTED_EDGE ( 'NONE', *, *, #69819, .T. ) ;
#45996 = VECTOR ( 'NONE', #91881, 1000.000000000000000 ) ;
#45997 = CARTESIAN_POINT ( 'NONE',  ( 0.000000000000000000, 0.000000000000000000, 0.000000000000000000 ) ) ;
#45998 = VERTEX_POINT ( 'NONE', #85125 ) ;
#45999 = CARTESIAN_POINT ( 'NONE',  ( 11.49412716574625115, 45.59192006558699006, -13.79863126508847948 ) ) ;
#46000 = DIRECTION ( 'NONE',  ( 0.000000000000000000, -1.000000000000000000, 0.000000000000000000 ) ) ;
#46001 = CARTESIAN_POINT ( 'NONE',  ( -85.96599883021772825, -60.00000000000000000, -23.70204626803236891 ) ) ;
#46002 = CARTESIAN_POINT ( 'NONE',  ( 5.601730134768061475, -12.35429686688396522, -0.02849990174191881914 ) ) ;
#46003 = CARTESIAN_POINT ( 'NONE',  ( 2.977408999572650927, -34.25000000204838813, -7.188101187500001821 ) ) ;
#46004 = DIRECTION ( 'NONE',  ( -1.000000000000000000, 0.000000000000000000, 0.000000000000000000 ) ) ;
#46005 = AXIS2_PLACEMENT_3D ( 'NONE', #103220, #54632, #46567 ) ;
#46006 = CYLINDRICAL_SURFACE ( 'NONE', #36171, 5.000000000000000888 ) ;
#46007 = CARTESIAN_POINT ( 'NONE',  ( 1.000000000000000000, -43.08885284239458713, 0.3536648519171542993 ) ) ;
#46008 = CARTESIAN_POINT ( 'NONE',  ( 2.617478844992369158, 49.99999999999999289, -75.26027323389158141 ) ) ;
#46009 = DIRECTION ( 'NONE',  ( 1.000000000000000000, -0.000000000000000000, -0.000000000000000000 ) ) ;
#46010 = CARTESIAN_POINT ( 'NONE',  ( -42.49506089581998936, 334.4681969747575749, 7.580802331008121620 ) ) ;
#46011 = ADVANCED_FACE ( 'NONE', ( #25878 ), #9620, .T. ) ;
#46012 = CARTESIAN_POINT ( 'NONE',  ( 24.16352152586478752, 303.6474178691188968, -9.828590987157472370 ) ) ;
#46013 = EDGE_LOOP ( 'NONE', ( #102454, #97610, #90971, #24102 ) ) ;
#46014 = CARTESIAN_POINT ( 'NONE',  ( 96.86866073052655679, -5.000000000000000888, 6.123233995736779101E-16 ) ) ;
#46015 = DIRECTION ( 'NONE',  ( -1.000000000000000000, -1.224606353822377258E-16, -0.000000000000000000 ) ) ;
#46016 = CARTESIAN_POINT ( 'NONE',  ( 33.84593435154630470, -46.42942808596986026, 36.05400579749584011 ) ) ;
#46017 = CARTESIAN_POINT ( 'NONE',  ( -21.65942590379792776, -9.659702761776270386E-13, -5.820808985972203864 ) ) ;
#46018 = ORIENTED_EDGE ( 'NONE', *, *, #19938, .T. ) ;
#46019 = CARTESIAN_POINT ( 'NONE',  ( 6.445370176742772017, -7.262437273741305432, 1.101027156350034231 ) ) ;
#46021 = CARTESIAN_POINT ( 'NONE',  ( -34.72474116627837759, 338.3618661353910966, -1.881472242819908436 ) ) ;
#46020 = CARTESIAN_POINT ( 'NONE',  ( 9.455047728417365960, -5.000000000000000000, -19.27141366270301504 ) ) ;
#46022 = CARTESIAN_POINT ( 'NONE',  ( -80.00000000000000000, -52.00000000000000000, -21.09707704303352926 ) ) ;
#46023 = LINE ( 'NONE', #79438, #6943 ) ;
#46024 = FILL_AREA_STYLE ('',( #5033 ) ) ;
#46025 = DIRECTION ( 'NONE',  ( -0.000000000000000000, -1.000000000000000000, -0.000000000000000000 ) ) ;
#46027 = COLOUR_RGB ( '', 0.40784314, 0.44705882, 0.49803922) ;
#46026 = CARTESIAN_POINT ( 'NONE',  ( 0.000000000000000000, 0.000000000000000000, -1.581124522925831499 ) ) ;
#46028 = CARTESIAN_POINT ( 'NONE',  ( -1.284384921555213888, -49.99999999999999289, 44.94055355497947346 ) ) ;
#46029 = ORIENTED_EDGE ( 'NONE', *, *, #72290, .T. ) ;
#46030 = CARTESIAN_POINT ( 'NONE',  ( 92.26607695852590041, -60.00000000000001421, 1.976148175831901721 ) ) ;
#46031 = COLOUR_RGB ( '', 0.31764706, 0.68627451, 0.89019608) ;
#46032 = CARTESIAN_POINT ( 'NONE',  ( 27.42642194216384866, 34.37160210622304390, -10.02587544220627080 ) ) ;
#46033 = CARTESIAN_POINT ( 'NONE',  ( -32.99999999999986500, 488.9035777786946255, 11.52689957822637901 ) ) ;
#46034 = CARTESIAN_POINT ( 'NONE',  ( -6.654387163495472990, 41.27136526523243987, -70.82047234851677331 ) ) ;
#46035 = CARTESIAN_POINT ( 'NONE',  ( -11.41837999597691322, 13.88778927716229461, -9.962302244322264855 ) ) ;
#46036 = EDGE_LOOP ( 'NONE', ( #63669, #1899, #51152, #54767, #94873, #4355 ) ) ;
#46037 = CARTESIAN_POINT ( 'NONE',  ( -82.71132764841163976, -30.00000000000251532, -22.95911469658347315 ) ) ;
#46038 = EDGE_LOOP ( 'NONE', ( #89998, #81554 ) ) ;
#46039 = DIRECTION ( 'NONE',  ( 0.5735764363510490460, 0.8191520442889896891, 0.000000000000000000 ) ) ;
#46040 = CARTESIAN_POINT ( 'NONE',  ( 15.79067987436806852, 22.71383723441031677, 1.248691266792864019 ) ) ;
#46041 =( NAMED_UNIT ( * ) SI_UNIT ( $, .STERADIAN. ) SOLID_ANGLE_UNIT ( ) );
#46042 = STYLED_ITEM ( 'NONE', ( #76198 ), #59831 ) ;
#46043 = CARTESIAN_POINT ( 'NONE',  ( 5.082755093536325930, -29.84375000204838813, -5.082755093536325042 ) ) ;
#46044 = CARTESIAN_POINT ( 'NONE',  ( -44.26592756129811335, 485.3087896057427884, 1.848518878038618807 ) ) ;
#46045 = CARTESIAN_POINT ( 'NONE',  ( -6.582107400625343274, 304.7470122113059574, 8.914715104312284311 ) ) ;
#46046 = CARTESIAN_POINT ( 'NONE',  ( 31.86300348751240108, 472.3516342516534223, 13.84838610500362144 ) ) ;
#46047 = ORIENTED_EDGE ( 'NONE', *, *, #51210, .F. ) ;
#46048 = AXIS2_PLACEMENT_3D ( 'NONE', #93931, #69658, #102550 ) ;
#46049 = VECTOR ( 'NONE', #77394, 1000.000000000000000 ) ;
#46050 = CIRCLE ( 'NONE', #49491, 4.000000000000001776 ) ;
#46051 = ORIENTED_EDGE ( 'NONE', *, *, #100847, .F. ) ;
#46052 = CARTESIAN_POINT ( 'NONE',  ( 78.10417343428038350, -36.02394493292788979, 131.9787684300717387 ) ) ;
#46053 = CARTESIAN_POINT ( 'NONE',  ( 15.51348069825422016, 2.608686647713930107, -0.4238655689582255803 ) ) ;
#46054 = VERTEX_POINT ( 'NONE', #35547 ) ;
#46055 = B_SPLINE_CURVE_WITH_KNOTS ( 'NONE', 3,
 ( #83160, #77197, #26564, #26045, #59436, #9256 ),
 .UNSPECIFIED., .F., .F.,
 ( 4, 2, 4 ),
 ( 0.01913986446880882805, 0.02104055318064340999, 0.02294124189247799192 ),
 .UNSPECIFIED. ) ;
#46056 = CARTESIAN_POINT ( 'NONE',  ( -12.50000000000000533, 27.18014154145715011, -44.71980230305747028 ) ) ;
#46057 = TOROIDAL_SURFACE ( 'NONE', #8147, 66.00000000000000000, 0.5000000000000000000 ) ;
#46058 = CARTESIAN_POINT ( 'NONE',  ( 4.401442555609581635E-16, -20.28125000204838813, -7.188101187500000044 ) ) ;
#46059 = AXIS2_PLACEMENT_3D ( 'NONE', #57082, #91081, #82438 ) ;
#46060 = CARTESIAN_POINT ( 'NONE',  ( -112.7923893646043183, -57.67119337860199124, 188.3631819635289446 ) ) ;
#46061 = EDGE_CURVE ( 'NONE', #86885, #98395, #58736, .T. ) ;
#46062 = ORIENTED_EDGE ( 'NONE', *, *, #6606, .T. ) ;
#46063 = SURFACE_STYLE_FILL_AREA ( #52540 ) ;
#46064 = DIRECTION ( 'NONE',  ( -1.000000000000000000, -0.000000000000000000, -0.000000000000000000 ) ) ;
#46065 = CARTESIAN_POINT ( 'NONE',  ( -5.647817967127100935, -13.45126406528794938, -2.038183545141171393 ) ) ;
#46066 = CARTESIAN_POINT ( 'NONE',  ( 7.302671812080789415, 41.33023047990123899, -59.14964464841043679 ) ) ;
#46067 = DIRECTION ( 'NONE',  ( -0.000000000000000000, 1.000000000000000000, 0.000000000000000000 ) ) ;
#46068 = CIRCLE ( 'NONE', #13313, 8.750000000000033751 ) ;
#46069 = CARTESIAN_POINT ( 'NONE',  ( 7.999999999999998224, -14.28125000409677092, 3.313708498984766493 ) ) ;
#46070 = CARTESIAN_POINT ( 'NONE',  ( -40.60913831900013804, -26.58592182782365398, 36.35858900883707889 ) ) ;
#46071 = CARTESIAN_POINT ( 'NONE',  ( 9.373884331925060209, 15.95332971149351842, 3.487646406148156242 ) ) ;
#46072 = CARTESIAN_POINT ( 'NONE',  ( 0.000000000000000000, 0.000000000000000000, 33.82893434829263413 ) ) ;
#46073 = CIRCLE ( 'NONE', #63245, 8.000000000000005329 ) ;
#46074 = CARTESIAN_POINT ( 'NONE',  ( 5.168696396656956793, 1.295298111819218168, -22.28139744604624184 ) ) ;
#46075 = CARTESIAN_POINT ( 'NONE',  ( -34.47678062873982441, 436.2905755606494722, 4.953078263947475968 ) ) ;
#46076 = DIRECTION ( 'NONE',  ( 0.9183650514339934956, 0.000000000000000000, -0.3957342950827467121 ) ) ;
#46077 = CARTESIAN_POINT ( 'NONE',  ( -9.948561005166130400, 33.86990273748199343, -1.045755304005141273 ) ) ;
#46078 = ORIENTED_EDGE ( 'NONE', *, *, #10917, .F. ) ;
#46079 = EDGE_CURVE ( 'NONE', #10915, #36785, #48180, .T. ) ;
#46080 = LINE ( 'NONE', #28329, #42318 ) ;
#46081 =( GEOMETRIC_REPRESENTATION_CONTEXT ( 3 ) GLOBAL_UNCERTAINTY_ASSIGNED_CONTEXT ( ( #13196 ) ) GLOBAL_UNIT_ASSIGNED_CONTEXT ( ( #58303, #34069, #76075 ) ) REPRESENTATION_CONTEXT ( 'NONE', 'WORKASPACE' ) );
#46082 = CARTESIAN_POINT ( 'NONE',  ( -38.56577463025283947, 437.0885780681463757, 4.837144025084506360 ) ) ;
#46083 = CARTESIAN_POINT ( 'NONE',  ( -50.89201122668178101, -28.75060113657595906, -34.85379606938838037 ) ) ;
#46084 = CARTESIAN_POINT ( 'NONE',  ( -67.48283298184769308, -30.00000000000000000, 87.50264991667094705 ) ) ;
#46085 = CARTESIAN_POINT ( 'NONE',  ( 5.500000000000007105, 42.00000000000000000, -65.90297133634214788 ) ) ;
#46086 = ORIENTED_EDGE ( 'NONE', *, *, #1355, .T. ) ;
#46087 = VECTOR ( 'NONE', #56615, 1000.000000000000000 ) ;
#46088 = CARTESIAN_POINT ( 'NONE',  ( -17.59386865947600143, -4.333298119783918878, 3.400962272289256294 ) ) ;
#46089 = CARTESIAN_POINT ( 'NONE',  ( 101.8486387914506253, -57.63170129011940901, 203.3287309220910970 ) ) ;
#46090 = CARTESIAN_POINT ( 'NONE',  ( 62.72655763203226087, -21.76998695923418481, -22.22484975073092883 ) ) ;
#46091 = FACE_OUTER_BOUND ( 'NONE', #21922, .T. ) ;
#46092 = CARTESIAN_POINT ( 'NONE',  ( -15.77973964953674724, 22.60063761605398369, -1.998938598361739150 ) ) ;
#46093 = PLANE ( 'NONE',  #40874 ) ;
#46094 = CARTESIAN_POINT ( 'NONE',  ( -53.50820603565255595, -59.99999999999999289, 81.05475964807466482 ) ) ;
#46095 = AXIS2_PLACEMENT_3D ( 'NONE', #73104, #29538, #21432 ) ;
#46096 = DIRECTION ( 'NONE',  ( 0.000000000000000000, 0.000000000000000000, 1.000000000000000000 ) ) ;
#46097 = DIRECTION ( 'NONE',  ( 0.000000000000000000, 1.000000000000000000, 0.000000000000000000 ) ) ;
#46098 = CARTESIAN_POINT ( 'NONE',  ( -52.56483885390515809, 48.00000000000000000, -38.23529411764715036 ) ) ;
#46099 = VECTOR ( 'NONE', #95283, 1000.000000000000000 ) ;
#46100 = CARTESIAN_POINT ( 'NONE',  ( -86.39008134157819541, -17.29286641282893555, 180.4476020658233892 ) ) ;
#46101 = ORIENTED_EDGE ( 'NONE', *, *, #32408, .T. ) ;
#46102 = CARTESIAN_POINT ( 'NONE',  ( 32.24532331159723952, 318.5265593782120845, -6.687297269301426539 ) ) ;
#46103 = DIRECTION ( 'NONE',  ( 1.000000000000000000, 0.000000000000000000, -1.224646799147353207E-16 ) ) ;
#46104 = CARTESIAN_POINT ( 'NONE',  ( -6.777274421432666784, 41.87254869799794932, -59.70743268153353256 ) ) ;
#46105 =( NAMED_UNIT ( * ) SI_UNIT ( $, .STERADIAN. ) SOLID_ANGLE_UNIT ( ) );
#46106 =( BOUNDED_CURVE ( )  B_SPLINE_CURVE ( 2, ( #48484, #82461, #33403 ),
 .UNSPECIFIED., .F., .F. ) 
 B_SPLINE_CURVE_WITH_KNOTS ( ( 3, 3 ),
 ( 0.000000000000000000, 1.000000000000000000 ),
 .UNSPECIFIED. ) 
 CURVE ( )  GEOMETRIC_REPRESENTATION_ITEM ( )  RATIONAL_B_SPLINE_CURVE ( ( 1.000000000000000000, 1.857142857142858317, 1.000000000000000000 ) ) 
 REPRESENTATION_ITEM ( '' )  );
#46107 = CARTESIAN_POINT ( 'NONE',  ( -7.046289519167718396, -11.30591819944378074, -3.789821819998817176 ) ) ;
#46108 = ADVANCED_FACE ( 'NONE', ( #19381 ), #68797, .F. ) ;
#46109 = CARTESIAN_POINT ( 'NONE',  ( -26.47418998143891500, 305.8622656725908087, -9.557889300953828382 ) ) ;
#46110 = CARTESIAN_POINT ( 'NONE',  ( -85.71891674152472262, -60.21565766106578366, -14.78162960339309251 ) ) ;
#46111 = CARTESIAN_POINT ( 'NONE',  ( 9.833493305133805151, 1.593028355512270962E-15, 0.000000000000000000 ) ) ;
#46112 = CARTESIAN_POINT ( 'NONE',  ( 0.000000000000000000, -1.200583151104953394, 112.0000000000000000 ) ) ;
#46113 = AXIS2_PLACEMENT_3D ( 'NONE', #18676, #2447, #1366 ) ;
#46114 = VERTEX_POINT ( 'NONE', #52750 ) ;
#46115 = STYLED_ITEM ( 'NONE', ( #94414 ), #60434 ) ;
#46116 = CARTESIAN_POINT ( 'NONE',  ( -1.908195823574487804E-14, -8.660254037844390851, -0.9999999999999974465 ) ) ;
#46117 = ADVANCED_FACE ( 'NONE', ( #68961 ), #67357, .F. ) ;
#46118 = CARTESIAN_POINT ( 'NONE',  ( 3.301606509414339641, -4.285714285714286476, -25.22241582816893413 ) ) ;
#46119 = CARTESIAN_POINT ( 'NONE',  ( 0.05533025579362134405, 6.264553569211843254, -2.149474931388135612 ) ) ;
#46120 = CARTESIAN_POINT ( 'NONE',  ( 94.98342851799053221, -59.99999999999993605, -11.07591208537989580 ) ) ;
#46121 = CARTESIAN_POINT ( 'NONE',  ( -76.52857891266238255, -60.31752180720845047, 145.8076901902507814 ) ) ;
#46122 = ORIENTED_EDGE ( 'NONE', *, *, #27480, .T. ) ;
#46123 =( NAMED_UNIT ( * ) SI_UNIT ( $, .STERADIAN. ) SOLID_ANGLE_UNIT ( ) );
#46124 = CARTESIAN_POINT ( 'NONE',  ( 72.70482823910218428, -57.66012140098748517, 178.8402823191526636 ) ) ;
#46125 = AXIS2_PLACEMENT_3D ( 'NONE', #24560, #47725, #32104 ) ;
#46126 = CARTESIAN_POINT ( 'NONE',  ( 42.45506592911483068, 319.4331922859328756, -4.049034721733997699 ) ) ;
#46127 = CARTESIAN_POINT ( 'NONE',  ( 18.00000000000000355, 12.99999999999999289, 0.000000000000000000 ) ) ;
#46128 = ORIENTED_EDGE ( 'NONE', *, *, #95834, .F. ) ;
#46129 = CARTESIAN_POINT ( 'NONE',  ( 1.625879232102889042E-15, 0.000000000000000000, -13.27631144943088515 ) ) ;
#46130 = DIRECTION ( 'NONE',  ( -1.000000000000000000, -1.224606353822377258E-16, -0.000000000000000000 ) ) ;
#46131 = DIRECTION ( 'NONE',  ( -1.000000000000000000, 0.000000000000000000, 0.000000000000000000 ) ) ;
#46132 = CARTESIAN_POINT ( 'NONE',  ( -7.188101187500000044, -27.40625000204838813, -8.802885111219163269E-16 ) ) ;
#46133 = ORIENTED_EDGE ( 'NONE', *, *, #28770, .F. ) ;
#46134 = CARTESIAN_POINT ( 'NONE',  ( 4.898587196589412829E-16, -19.81250000409677270, -8.000000000000000000 ) ) ;
#46135 = AXIS2_PLACEMENT_3D ( 'NONE', #24665, #80738, #82342 ) ;
#46136 = CARTESIAN_POINT ( 'NONE',  ( 75.30000000000001137, 0.000000000000000000, 0.000000000000000000 ) ) ;
#46137 = CARTESIAN_POINT ( 'NONE',  ( -44.36567622869332439, 435.2186464882956329, 12.63794204390610254 ) ) ;
#46138 = CARTESIAN_POINT ( 'NONE',  ( -17.40604945778709478, 45.37707562542235706, -6.412274061844375872 ) ) ;
#46139 = PLANE ( 'NONE',  #61151 ) ;
#46140 = EDGE_CURVE ( 'NONE', #44950, #30745, #68927, .T. ) ;
#46141 = VECTOR ( 'NONE', #21698, 999.9999999999998863 ) ;
#46142 = FACE_OUTER_BOUND ( 'NONE', #302, .T. ) ;
#46143 = ORIENTED_EDGE ( 'NONE', *, *, #68349, .F. ) ;
#46144 = CARTESIAN_POINT ( 'NONE',  ( 43.47770857297108904, 484.8227827122623808, 4.253339224814284059 ) ) ;
#46146 = CARTESIAN_POINT ( 'NONE',  ( 26.62717767826400816, -53.38857218945616978, 34.52190694528636783 ) ) ;
#46145 = CARTESIAN_POINT ( 'NONE',  ( -68.01705929348101165, -29.99999999999997158, 119.4519777144086703 ) ) ;
#46147 = CARTESIAN_POINT ( 'NONE',  ( 23.38277283915452642, 28.07830159701457617, -30.71447743823567933 ) ) ;
#46148 = EDGE_LOOP ( 'NONE', ( #62562, #40879, #53015, #51867 ) ) ;
#46149 = AXIS2_PLACEMENT_3D ( 'NONE', #74099, #67632, #8309 ) ;
#46150 = UNCERTAINTY_MEASURE_WITH_UNIT (LENGTH_MEASURE( 1.000000000000000082E-05 ), #17074, 'distance_accuracy_value', 'NONE');
#46151 = EDGE_LOOP ( 'NONE', ( #73936, #44325, #72372, #41899, #5300 ) ) ;
#46152 = CARTESIAN_POINT ( 'NONE',  ( 33.21794938082042847, 463.2572442978370759, 6.155096106961184255 ) ) ;
#46153 = CARTESIAN_POINT ( 'NONE',  ( -44.29460294111019891, 463.8401613562648436, 7.966579552388332708 ) ) ;
#46154 = EDGE_CURVE ( 'NONE', #32665, #92392, #48455, .T. ) ;
#46155 = CARTESIAN_POINT ( 'NONE',  ( -14.83882035797137888, 4.620392632316137949, 5.701545570406011620 ) ) ;
#46157 = ORIENTED_EDGE ( 'NONE', *, *, #96453, .T. ) ;
#46156 = AXIS2_PLACEMENT_3D ( 'NONE', #59274, #84068, #77577 ) ;
#46158 =( NAMED_UNIT ( * ) PLANE_ANGLE_UNIT ( ) SI_UNIT ( $, .RADIAN. ) );
#46159 = CARTESIAN_POINT ( 'NONE',  ( 83.61123812565043067, -29.99999999999987566, 157.5619696514056614 ) ) ;
#46160 = CARTESIAN_POINT ( 'NONE',  ( -10.52583372651181115, 10.24894645679494509, -10.32074519161062476 ) ) ;
#46161 = CARTESIAN_POINT ( 'NONE',  ( 0.000000000000000000, 27.55047179872464724, -49.09040922050319011 ) ) ;
#46162 = CARTESIAN_POINT ( 'NONE',  ( 81.13473597870090259, -30.00000000000000355, 1.891638132046062015 ) ) ;
#46163 = CARTESIAN_POINT ( 'NONE',  ( 86.75754961941542831, 5.000000000000021316, 0.000000000000000000 ) ) ;
#46164 = ORIENTED_EDGE ( 'NONE', *, *, #94277, .F. ) ;
#46165 = ORIENTED_EDGE ( 'NONE', *, *, #35218, .F. ) ;
#46166 = TOROIDAL_SURFACE ( 'NONE', #16903, 8.400000000000000355, 0.5999999999999978684 ) ;
#46167 = ORIENTED_EDGE ( 'NONE', *, *, #10199, .T. ) ;
#46168 = CARTESIAN_POINT ( 'NONE',  ( -14.54015256618497176, 142.2617268803927573, 5.000000000000000000 ) ) ;
#46169 = CARTESIAN_POINT ( 'NONE',  ( 12.21253585067004543, 1.340359594676612611E-15, 0.000000000000000000 ) ) ;
#46170 = LINE ( 'NONE', #20356, #19256 ) ;
#46171 = LINE ( 'NONE', #102813, #10100 ) ;
#46172 = CARTESIAN_POINT ( 'NONE',  ( -7.412906595240168706, -87.64188272852256034, 3.014362223629233561 ) ) ;
#46173 = CARTESIAN_POINT ( 'NONE',  ( -33.00540147334746166, 487.4196752801198613, 9.523982417603901851 ) ) ;
#46174 = CIRCLE ( 'NONE', #35886, 5.000000000000000000 ) ;
#46175 = ORIENTED_EDGE ( 'NONE', *, *, #102523, .F. ) ;
#46176 = CARTESIAN_POINT ( 'NONE',  ( 1.224646799147352665E-15, 48.00000000000000000, -75.00000000000001421 ) ) ;
#46177 = EDGE_LOOP ( 'NONE', ( #77859, #50252, #47802, #55474 ) ) ;
#46178 = CARTESIAN_POINT ( 'NONE',  ( -38.79307744976971861, 485.8212363931074265, -4.896981067614003535 ) ) ;
#46179 = CIRCLE ( 'NONE', #97811, 5.000000000000010658 ) ;
#46180 = CARTESIAN_POINT ( 'NONE',  ( -83.34567396899497282, -60.00000000000000711, 190.8012197679059057 ) ) ;
#46181 = CARTESIAN_POINT ( 'NONE',  ( 62.91851151839247791, -46.43458783406691026, 83.69961423548066648 ) ) ;
#46182 = VECTOR ( 'NONE', #85885, 1000.000000000000000 ) ;
#46183 = VERTEX_POINT ( 'NONE', #36617 ) ;
#46184 = CARTESIAN_POINT ( 'NONE',  ( 40.05582037023106778, 464.2476455834488434, 17.93522255631042484 ) ) ;
#46185 = CARTESIAN_POINT ( 'NONE',  ( -69.28496039471292534, -38.19304130032977440, -31.44853639721581473 ) ) ;
#46186 = CARTESIAN_POINT ( 'NONE',  ( -6.770001855160698412, 9.416670812148407066, -1.796682604554742602 ) ) ;
#46187 = DIRECTION ( 'NONE',  ( -0.4157805170469000555, 0.4085867419963847835, 0.8125167296179151011 ) ) ;
#46188 = ADVANCED_FACE ( 'NONE', ( #3687 ), #27614, .T. ) ;
#46189 = ORIENTED_EDGE ( 'NONE', *, *, #10896, .F. ) ;
#46190 = CARTESIAN_POINT ( 'NONE',  ( 0.05613245601036537941, 1.278525034529256699, 6.499999999999999112 ) ) ;
#46191 = CARTESIAN_POINT ( 'NONE',  ( -73.50473004590615744, -60.00000000000000000, -24.84693947030580574 ) ) ;
#46192 = AXIS2_PLACEMENT_3D ( 'NONE', #8559, #34483, #41993 ) ;
#46193 = AXIS2_PLACEMENT_3D ( 'NONE', #41847, #67731, #41316 ) ;
#46194 = EDGE_CURVE ( 'NONE', #35657, #37979, #12814, .T. ) ;
#46195 = CARTESIAN_POINT ( 'NONE',  ( 33.58349330513379982, -7.703719777548943412E-31, 4.000000000000001776 ) ) ;
#46196 = EDGE_CURVE ( 'NONE', #79592, #18742, #67228, .T. ) ;
#46197 = CARTESIAN_POINT ( 'NONE',  ( 4.898587196589412829E-16, -33.31250000409677625, -8.000000000000000000 ) ) ;
#46198 = AXIS2_PLACEMENT_3D ( 'NONE', #32059, #23446, #7218 ) ;
#46199 = CARTESIAN_POINT ( 'NONE',  ( -29.68315524076956180, 8.302504244945341227, 42.10535821593508388 ) ) ;
#46200 = PRESENTATION_LAYER_ASSIGNMENT (  '', '', ( #101322 ) ) ;
#46201 = CARTESIAN_POINT ( 'NONE',  ( 86.63474249928231075, -20.69447793298352423, 184.5529616228748750 ) ) ;
#46202 = EDGE_CURVE ( 'NONE', #63953, #51686, #25925, .T. ) ;
#46203 = CARTESIAN_POINT ( 'NONE',  ( 44.22243490918458519, 464.2587958754115220, 9.201099836299508894 ) ) ;
#46204 = CARTESIAN_POINT ( 'NONE',  ( -4.604390456819611011, 8.535337771752283587, 5.000000000000000000 ) ) ;
#46205 = CARTESIAN_POINT ( 'NONE',  ( 7.046289519167717508, -8.694081800556235251, -3.789821819998816288 ) ) ;
#46206 = CARTESIAN_POINT ( 'NONE',  ( 16.53875398580865053, 304.5679815164853608, 8.876634110831217228 ) ) ;
#46207 = CARTESIAN_POINT ( 'NONE',  ( 13.83891950279925354, -50.53292902901529970, 29.12888379965242081 ) ) ;
#46208 = ADVANCED_FACE ( 'NONE', ( #28515 ), #54317, .T. ) ;
#46209 = CARTESIAN_POINT ( 'NONE',  ( 35.34153741681340222, 436.0142057970623455, 5.687792605519862654 ) ) ;
#46210 = EDGE_CURVE ( 'NONE', #14419, #55315, #69482, .T. ) ;
#46211 = CARTESIAN_POINT ( 'NONE',  ( -100.3611959579476292, -30.00000000000000000, 157.5875141194946707 ) ) ;
#46212 = CARTESIAN_POINT ( 'NONE',  ( 0.000000000000000000, 0.000000000000000000, -5.703399999999999359 ) ) ;
#46213 = CARTESIAN_POINT ( 'NONE',  ( 27.93397395458839938, -57.67923204457687802, 44.25413198997598840 ) ) ;
#46215 = LINE ( 'NONE', #71530, #82690 ) ;
#46214 = CARTESIAN_POINT ( 'NONE',  ( 13.99175139092173481, 6.893215643474297494, -7.923894012196674552 ) ) ;
#46216 = CIRCLE ( 'NONE', #84090, 1.000000000000004885 ) ;
#46217 = DIRECTION ( 'NONE',  ( -0.000000000000000000, -0.000000000000000000, -1.000000000000000000 ) ) ;
#46218 = CARTESIAN_POINT ( 'NONE',  ( 80.00000000000000000, -52.00000000000000000, -21.09707704303352926 ) ) ;
#46219 = CARTESIAN_POINT ( 'NONE',  ( -10.00000000000000000, 15.00000000000000000, 2.701558353794764056 ) ) ;
#46220 = CARTESIAN_POINT ( 'NONE',  ( -6.750000000000018652, 11.69134295108991317, 0.000000000000000000 ) ) ;
#46221 = CARTESIAN_POINT ( 'NONE',  ( 4.750478166817060810, -15.57755379964487297, -35.13231593693921440 ) ) ;
#46222 = CIRCLE ( 'NONE', #68644, 7.999999999999973355 ) ;
#46223 = SURFACE_STYLE_FILL_AREA ( #45174 ) ;
#46224 = CARTESIAN_POINT ( 'NONE',  ( -87.35314139720050264, -35.37591848484672141, 188.8839025493173267 ) ) ;
#46225 = ORIENTED_EDGE ( 'NONE', *, *, #26249, .T. ) ;
#46226 = CARTESIAN_POINT ( 'NONE',  ( -3.202918473694307266, -48.99785005461730947, 104.2983563224298109 ) ) ;
#46227 = CARTESIAN_POINT ( 'NONE',  ( -14.45088570581510190, -32.51316581980542963, 29.42462076004476756 ) ) ;
#46229 = CARTESIAN_POINT ( 'NONE',  ( 20.11650669486618881, 1.474610560812782335E-15, 0.000000000000000000 ) ) ;
#46228 = CARTESIAN_POINT ( 'NONE',  ( -87.00764824667378150, -60.00000000000000711, -8.040170719849857761 ) ) ;
#46230 = ORIENTED_EDGE ( 'NONE', *, *, #44112, .F. ) ;
#46231 = CARTESIAN_POINT ( 'NONE',  ( 0.000000000000000000, 4.898587196589412829E-16, -4.000000000000000000 ) ) ;
#46232 = COLOUR_RGB ( '', 0.08235294, 0.09019608, 0.10196078) ;
#46233 = CARTESIAN_POINT ( 'NONE',  ( 14.58597127887092526, 5.499146323182380058, -6.679532531461099154 ) ) ;
#46234 = CARTESIAN_POINT ( 'NONE',  ( 43.03185303983489263, 485.3613526602387083, 6.073233449168520259 ) ) ;
#46235 = AXIS2_PLACEMENT_3D ( 'NONE', #32103, #75728, #15899 ) ;
#46236 = ADVANCED_FACE ( 'NONE', ( #86215 ), #79220, .T. ) ;
#46237 = CARTESIAN_POINT ( 'NONE',  ( 15.85122647056135392, 4.114663126756306077, -4.288211754877241155 ) ) ;
#46238 = CARTESIAN_POINT ( 'NONE',  ( 8.572527594031457413E-16, 273.9999999999999432, 6.999999999999982236 ) ) ;
#46239 = ORIENTED_EDGE ( 'NONE', *, *, #3671, .T. ) ;
#46240 = CARTESIAN_POINT ( 'NONE',  ( 32.39561178865213975, 439.6665705367017836, 24.00535790829840721 ) ) ;
#46241 = CARTESIAN_POINT ( 'NONE',  ( -35.23236120362036417, 435.7070508914230231, 6.197761447607906149 ) ) ;
#46243 = SURFACE_STYLE_FILL_AREA ( #71557 ) ;
#46242 = CARTESIAN_POINT ( 'NONE',  ( -13.50000000000000178, 1.319989657865592303, -0.02800283339254916112 ) ) ;
#46244 = CARTESIAN_POINT ( 'NONE',  ( 0.000000000000000000, 303.8518027762758038, -10.00000000000000355 ) ) ;
#46245 = ORIENTED_EDGE ( 'NONE', *, *, #24121, .T. ) ;
#46246 = ORIENTED_EDGE ( 'NONE', *, *, #1841, .T. ) ;
#46247 = CARTESIAN_POINT ( 'NONE',  ( -27.18383540787484520, 309.6430342986412256, 11.30725836788668204 ) ) ;
#46248 = ORIENTED_EDGE ( 'NONE', *, *, #6415, .F. ) ;
#46249 = CARTESIAN_POINT ( 'NONE',  ( 21.85903006778882229, 305.2263394331082509, 10.01755384245877423 ) ) ;
#46250 = ADVANCED_FACE ( 'NONE', ( #94288 ), #82684, .T. ) ;
#46251 = CARTESIAN_POINT ( 'NONE',  ( 8.000000000000000000, -14.09375000409676915, -3.313708498984761164 ) ) ;
#46252 = DIRECTION ( 'NONE',  ( 0.000000000000000000, 0.000000000000000000, -1.000000000000000000 ) ) ;
#46253 = ORIENTED_EDGE ( 'NONE', *, *, #69880, .T. ) ;
#46254 = CARTESIAN_POINT ( 'NONE',  ( 1.724765290415787300, -3.000000000000002665, -69.73714729959421277 ) ) ;
#46255 = CARTESIAN_POINT ( 'NONE',  ( -5.308064226573042887, 41.67430808342687243, -70.56675994572434263 ) ) ;
#46256 = CARTESIAN_POINT ( 'NONE',  ( -102.5752670435136054, -60.00000000001715250, 203.5310177018276363 ) ) ;
#46257 = CARTESIAN_POINT ( 'NONE',  ( 46.00000000000000000, 485.9062929993805255, 0.4531997891273246704 ) ) ;
#46258 = CIRCLE ( 'NONE', #25581, 1.000000000000000888 ) ;
#46259 = CARTESIAN_POINT ( 'NONE',  ( 93.40270045618473205, -59.99999999999997868, -17.32733600390682227 ) ) ;
#46260 = CARTESIAN_POINT ( 'NONE',  ( -32.04737116498198901, 465.7264234052246934, 15.44069434688416464 ) ) ;
#46261 = CARTESIAN_POINT ( 'NONE',  ( -5.896196268914855487, 41.78011476317043815, -58.83937604779054453 ) ) ;
#46262 = VECTOR ( 'NONE', #87641, 1000.000000000000000 ) ;
#46264 = CARTESIAN_POINT ( 'NONE',  ( 10.30248428635618296, -42.95372659178649144, 31.06077762009211440 ) ) ;
#46263 = CARTESIAN_POINT ( 'NONE',  ( -92.59939171350268339, -30.00000000000003908, 50.96567362325610873 ) ) ;
#46265 = VECTOR ( 'NONE', #62384, 1000.000000000000000 ) ;
#46266 = CARTESIAN_POINT ( 'NONE',  ( 69.18888888888888289, 6.915964383211875250E-15, 0.000000000000000000 ) ) ;
#46267 = CARTESIAN_POINT ( 'NONE',  ( -49.64579935860110282, -18.74248632113715374, 43.46943838681040972 ) ) ;
#46268 = CARTESIAN_POINT ( 'NONE',  ( -2.026245759303455518, 21.31123701474006182, 6.704152251160012455 ) ) ;
#46269 = EDGE_LOOP ( 'NONE', ( #2522, #25555, #45105, #80481 ) ) ;
#46270 = CARTESIAN_POINT ( 'NONE',  ( 36.28638774858024618, 437.5816761911047479, 4.254147741574738184 ) ) ;
#46271 = AXIS2_PLACEMENT_3D ( 'NONE', #23796, #98692, #89564 ) ;
#46272 = CYLINDRICAL_SURFACE ( 'NONE', #11637, 3.400000000000000355 ) ;
#46273 = EDGE_CURVE ( 'NONE', #69218, #50155, #96481, .T. ) ;
#46274 = DIRECTION ( 'NONE',  ( 0.000000000000000000, -1.000000000000000000, 0.000000000000000000 ) ) ;
#46275 = ORIENTED_EDGE ( 'NONE', *, *, #56545, .T. ) ;
#46276 = CARTESIAN_POINT ( 'NONE',  ( -15.82282301484858067, -3.734535164757628589, 14.53964175053558883 ) ) ;
#46277 = ORIENTED_EDGE ( 'NONE', *, *, #13896, .F. ) ;
#46278 = CARTESIAN_POINT ( 'NONE',  ( 86.44521950301134439, -30.00000000000693490, 197.9828864136313484 ) ) ;
#46279 = CARTESIAN_POINT ( 'NONE',  ( 0.000000000000000000, 67.05096163904791240, 0.000000000000000000 ) ) ;
#46280 = CARTESIAN_POINT ( 'NONE',  ( 5.767822811355441281, 42.00032026584280231, -59.73203674101891636 ) ) ;
#46281 = CARTESIAN_POINT ( 'NONE',  ( -37.36680950586716676, 18.64316884709021238, -10.04205104292877770 ) ) ;
#46282 = CARTESIAN_POINT ( 'NONE',  ( 94.54221292022157286, -30.00000000000000000, 191.3208119123549409 ) ) ;
#46283 = CARTESIAN_POINT ( 'NONE',  ( 0.000000000000000000, 0.9999999999999970024, 0.000000000000000000 ) ) ;
#46284 = ORIENTED_EDGE ( 'NONE', *, *, #93988, .T. ) ;
#46285 = ORIENTED_EDGE ( 'NONE', *, *, #44380, .F. ) ;
#46286 = EDGE_LOOP ( 'NONE', ( #7014, #53317, #78646, #13603 ) ) ;
#46287 = CARTESIAN_POINT ( 'NONE',  ( -43.50377727019363761, 435.9167426301696651, 18.24083946424746117 ) ) ;
#46288 = LINE ( 'NONE', #71085, #5979 ) ;
#46289 = DIRECTION ( 'NONE',  ( -0.000000000000000000, 1.000000000000000000, 0.000000000000000000 ) ) ;
#46291 = VERTEX_POINT ( 'NONE', #81260 ) ;
#46290 = MECHANICAL_DESIGN_GEOMETRIC_PRESENTATION_REPRESENTATION (  '', ( #97933 ), #99875 ) ;
#46292 = DIRECTION ( 'NONE',  ( 0.000000000000000000, 0.000000000000000000, 1.000000000000000000 ) ) ;
#46293 = VECTOR ( 'NONE', #74047, 1000.000000000000000 ) ;
#46294 = ORIENTED_EDGE ( 'NONE', *, *, #7874, .F. ) ;
#46295 = PLANE ( 'NONE',  #81043 ) ;
#46296 = CARTESIAN_POINT ( 'NONE',  ( 88.56009130522666339, -38.54379311642402683, 200.1470422519182648 ) ) ;
#46297 = CARTESIAN_POINT ( 'NONE',  ( 15.55524313394574776, 4.752315816073751975, 5.679728908060340586 ) ) ;
#46298 = PRODUCT_RELATED_PRODUCT_CATEGORY ( 'part', '', ( #84520 ) ) ;
#46299 = CARTESIAN_POINT ( 'NONE',  ( 83.67125305368273303, -45.28243862851755352, 10.83020272535897277 ) ) ;
#46300 = CARTESIAN_POINT ( 'NONE',  ( -5.000000000000000888, 0.000000000000000000, 5.000000000000000000 ) ) ;
#46301 = CARTESIAN_POINT ( 'NONE',  ( 33.06938392854667086, 440.0271615209351239, 23.76204839300703853 ) ) ;
#46302 = CARTESIAN_POINT ( 'NONE',  ( -43.64531880384350160, 464.9151967207102416, 12.30391130302176350 ) ) ;
#46303 = AXIS2_PLACEMENT_3D ( 'NONE', #41594, #65868, #9737 ) ;
#46304 = CARTESIAN_POINT ( 'NONE',  ( 7.549006887134069643, 4.358421158401191597, -7.700127545397313256 ) ) ;
#46305 = LINE ( 'NONE', #62492, #21655 ) ;
#46306 = ORIENTED_EDGE ( 'NONE', *, *, #77541, .T. ) ;
#46307 = B_SPLINE_CURVE_WITH_KNOTS ( 'NONE', 3,
 ( #51139, #10158, #2058, #35006, #67873, #16124, #49008, #81909, #8025, #65749, #57628, #93213, #94824, #52208, #45211, #69476, #44677, #85666, #12281, #102361, #19901, #11205, #12808, #27992, #76484, #59798, #10679, #44138, #35542, #78085, #28508, #45722, #77564, #61391 ),
 .UNSPECIFIED., .F., .F.,
 ( 4, 2, 2, 2, 2, 2, 2, 2, 2, 2, 2, 2, 2, 2, 2, 2, 4 ),
 ( 0.01272238763756222690, 0.01351613129786394599, 0.01430987495816566507, 0.01510361861846738415, 0.01589736227876910324, 0.01669110593907082232, 0.01748484959937254141, 0.01827859325967426049, 0.01907233691997597957, 0.01986608058027769866, 0.02065982424057941774, 0.02145356790088113683, 0.02224731156118285591, 0.02304105522148457846, 0.02383479888178629408, 0.02462854254208801663, 0.02542228620238973225 ),
 .UNSPECIFIED. ) ;
#46308 = CARTESIAN_POINT ( 'NONE',  ( 14.75116209840774495, 43.55504285524111907, -90.22050492864485705 ) ) ;
#46309 = CARTESIAN_POINT ( 'NONE',  ( -26.94613670386046778, 36.94238681296033633, 7.556984339686012575 ) ) ;
#46310 = ORIENTED_EDGE ( 'NONE', *, *, #90182, .F. ) ;
#46311 = DIRECTION ( 'NONE',  ( -1.000000000000000000, -0.000000000000000000, -0.000000000000000000 ) ) ;
#46312 = CARTESIAN_POINT ( 'NONE',  ( -30.36635531035291535, 298.1745412196082157, 2.670034220700619354 ) ) ;
#46313 = CARTESIAN_POINT ( 'NONE',  ( 7.808002908774420270, 53.96896602587193570, -3.792909619549702516 ) ) ;
#46314 = CARTESIAN_POINT ( 'NONE',  ( 5.656854249492378806, -18.68749999999999289, 5.656854249492381470 ) ) ;
#46315 = CARTESIAN_POINT ( 'NONE',  ( -27.02137051350053198, -22.88282787297301368, 37.55591774060851407 ) ) ;
#46316 = CLOSED_SHELL ( 'NONE', ( #39853, #26428, #36583, #87638, #19117, #95259, #102828, #41370, #54694, #90576, #93079, #56902, #90864, #44577, #72138, #31256, #14716, #11922, #97466, #9496, #85004, #93400, #79708, #17821, #14500, #32445, #43674, #96183 ) ) ;
#46317 = EDGE_CURVE ( 'NONE', #71702, #22401, #37914, .T. ) ;
#46318 = DIRECTION ( 'NONE',  ( -0.000000000000000000, 0.3049629831706211491, 0.9523642049634560847 ) ) ;
#46319 = VERTEX_POINT ( 'NONE', #14935 ) ;
#46320 = CARTESIAN_POINT ( 'NONE',  ( 86.40316107272373358, -17.81776296206304977, 175.1963145870509209 ) ) ;
#46321 = CARTESIAN_POINT ( 'NONE',  ( -38.19034542652883601, 27.40923537312541214, 13.30185581998165389 ) ) ;
#46322 = CIRCLE ( 'NONE', #29130, 8.000000000000000000 ) ;
#46323 = B_SPLINE_CURVE_WITH_KNOTS ( 'NONE', 3,
 ( #76184, #68098, #27156, #15167, #39987, #38932 ),
 .UNSPECIFIED., .F., .F.,
 ( 4, 2, 4 ),
 ( 0.000000000000000000, 0.001916782365109756352, 0.003833564730219512703 ),
 .UNSPECIFIED. ) ;
#46324 = CARTESIAN_POINT ( 'NONE',  ( 4.284822031654965890, -1.092833614412281662, 104.4267991316945086 ) ) ;
#46325 = ORIENTED_EDGE ( 'NONE', *, *, #106511, .F. ) ;
#46326 = CARTESIAN_POINT ( 'NONE',  ( 95.57097302797416205, -57.67170133996449977, 37.79358618412610582 ) ) ;
#46327 = CARTESIAN_POINT ( 'NONE',  ( 9.165151389911699198, 249.9999999999999432, 4.000000000000002665 ) ) ;
#46328 = CARTESIAN_POINT ( 'NONE',  ( 2.384812152908761806, -5.000000000000002665, -98.00000000000000000 ) ) ;
#46329 = CARTESIAN_POINT ( 'NONE',  ( 16.50306599534081187, -4.333298119783718150, -6.982805420311324340 ) ) ;
#46330 = EDGE_CURVE ( 'NONE', #73621, #8869, #53445, .T. ) ;
#46331 = CARTESIAN_POINT ( 'NONE',  ( 5.691929483231186637, -5.637851296924623057E-15, -6.499999999999999112 ) ) ;
#46332 = EDGE_CURVE ( 'NONE', #77482, #50441, #87858, .T. ) ;
#46333 = CARTESIAN_POINT ( 'NONE',  ( 51.88291765283137380, 277.1183258647170646, 267.1969486012846460 ) ) ;
#46334 = CARTESIAN_POINT ( 'NONE',  ( 5.451874645059660018, -18.69079845380849747, 35.10559483537603143 ) ) ;
#46335 = CARTESIAN_POINT ( 'NONE',  ( 51.87563516386928342, -29.94825904151492324, 49.86669112565530781 ) ) ;
#46336 = VECTOR ( 'NONE', #902, 1000.000000000000000 ) ;
#46338 = CARTESIAN_POINT ( 'NONE',  ( -11.09991137466503197, 10.54797039668288150, 9.715157720006006414 ) ) ;
#46337 = CARTESIAN_POINT ( 'NONE',  ( 41.60913933150737876, 468.1839071376891184, 17.09486578100470311 ) ) ;
#46339 = CARTESIAN_POINT ( 'NONE',  ( 7.742691193538925987, 302.4167829614624452, -10.02995440365113744 ) ) ;
#46340 = FILL_AREA_STYLE ('',( #87866 ) ) ;
#46341 = FILL_AREA_STYLE_COLOUR ( '', #73302 ) ;
#46342 = CARTESIAN_POINT ( 'NONE',  ( -11.71696977824031194, 294.5934938086913917, 1.882064959436767548 ) ) ;
#46343 = AXIS2_PLACEMENT_3D ( 'NONE', #63057, #6388, #45287 ) ;
#46344 = CARTESIAN_POINT ( 'NONE',  ( -99.18585800602104996, -38.00000000000002132, 133.7838027881280425 ) ) ;
#46345 = ORIENTED_EDGE ( 'NONE', *, *, #36831, .T. ) ;
#46346 = CARTESIAN_POINT ( 'NONE',  ( -9.354938227918532689, -1.847069743908760664, 15.48488176184545040 ) ) ;
#46347 = CARTESIAN_POINT ( 'NONE',  ( -20.49977525862259142, 302.8459220885798686, -10.00124997875687427 ) ) ;
#46348 = CARTESIAN_POINT ( 'NONE',  ( 5.855777637195783036, -61.21893503241554413, -1.331220292256679372 ) ) ;
#46350 = CARTESIAN_POINT ( 'NONE',  ( -3.173625681713546420, -47.40886789814266677, -34.77114549613931871 ) ) ;
#46349 = DIRECTION ( 'NONE',  ( 0.000000000000000000, -1.000000000000000000, 0.000000000000000000 ) ) ;
#46351 = ORIENTED_EDGE ( 'NONE', *, *, #80293, .T. ) ;
#46352 = VECTOR ( 'NONE', #97539, 1000.000000000000114 ) ;
#46353 = CARTESIAN_POINT ( 'NONE',  ( 2.499999999999999556, -8.000000000000000000, 17.89626171146327138 ) ) ;
#46354 = DIRECTION ( 'NONE',  ( -0.3048027540940019264, 0.4519649026942499925, -0.8383453988835919413 ) ) ;
#46355 = EDGE_LOOP ( 'NONE', ( #96919, #59698 ) ) ;
#46356 = CIRCLE ( 'NONE', #29161, 8.000000000000007105 ) ;
#46357 = ADVANCED_FACE ( 'NONE', ( #17088 ), #49955, .T. ) ;
#46358 = DIRECTION ( 'NONE',  ( -0.000000000000000000, -1.000000000000000000, -0.000000000000000000 ) ) ;
#46359 = FACE_OUTER_BOUND ( 'NONE', #71863, .T. ) ;
#46360 = CARTESIAN_POINT ( 'NONE',  ( -92.40188694392391255, -60.00000000000001421, -12.05163403178383241 ) ) ;
#46361 = EDGE_LOOP ( 'NONE', ( #9520, #44665, #5831, #46078 ) ) ;
#46362 = CARTESIAN_POINT ( 'NONE',  ( -27.99999999999999645, 0.000000000000000000, 15.00000000000000000 ) ) ;
#46363 = DIRECTION ( 'NONE',  ( 0.5735764363510470476, -0.8191520442889911324, 1.003171929053524007E-16 ) ) ;
#46364 = CARTESIAN_POINT ( 'NONE',  ( -9.221216839714866609, 28.95240251831025446, 3.869414262756994294 ) ) ;
#46366 = DIRECTION ( 'NONE',  ( -1.000000000000000000, -1.224606353822377258E-16, -0.000000000000000000 ) ) ;
#46365 = DIRECTION ( 'NONE',  ( 0.8191520442889974607, 1.003171929053531649E-16, -0.5735764363510380548 ) ) ;
#46367 = AXIS2_PLACEMENT_3D ( 'NONE', #42939, #101706, #35955 ) ;
#46368 = CARTESIAN_POINT ( 'NONE',  ( -81.18994567851672173, -53.43462853400483681, 175.1505282733661204 ) ) ;
#46369 = VERTEX_POINT ( 'NONE', #31172 ) ;
#46370 = CARTESIAN_POINT ( 'NONE',  ( 6.746887896523637629, 3.895317543247282188, -6.526184258131186411 ) ) ;
#46371 = ORIENTED_EDGE ( 'NONE', *, *, #15941, .T. ) ;
#46372 = ORIENTED_EDGE ( 'NONE', *, *, #56286, .F. ) ;
#46373 = LINE ( 'NONE', #72748, #84518 ) ;
#46374 = ADVANCED_FACE ( 'NONE', ( #48367 ), #19060, .T. ) ;
#46375 = CARTESIAN_POINT ( 'NONE',  ( -4.420167282472111658, -68.81245422675547729, 13.71330708048197700 ) ) ;
#46376 = ORIENTED_EDGE ( 'NONE', *, *, #50377, .T. ) ;
#46377 = DIRECTION ( 'NONE',  ( 0.000000000000000000, -1.000000000000000000, 0.000000000000000000 ) ) ;
#46378 = CARTESIAN_POINT ( 'NONE',  ( -10.00000000000000000, 15.00000000000000000, -1.544939622599426743 ) ) ;
#46379 = CARTESIAN_POINT ( 'NONE',  ( -86.45135651325685444, -57.58031178088597812, 202.9040356603995008 ) ) ;
#46380 = CARTESIAN_POINT ( 'NONE',  ( -9.928372500597216543, 294.6449087092673835, 1.240117573296916298 ) ) ;
#46381 = AXIS2_PLACEMENT_3D ( 'NONE', #92194, #67937, #58796 ) ;
#46382 = CARTESIAN_POINT ( 'NONE',  ( -19.38977043078304519, 294.6924723843361562, -2.033472732115015891 ) ) ;
#46383 = CARTESIAN_POINT ( 'NONE',  ( 28.99999999999999645, 0.000000000000000000, 0.000000000000000000 ) ) ;
#46384 = CARTESIAN_POINT ( 'NONE',  ( -13.56235479181388115, -52.22051512849589017, 23.52533112101723844 ) ) ;
#46385 = CARTESIAN_POINT ( 'NONE',  ( -18.00631980831517609, 36.44533851663729962, -23.17937010874027237 ) ) ;
#46386 = CARTESIAN_POINT ( 'NONE',  ( 86.84200744108139247, -14.21045842199445630, 3.673032677714961558 ) ) ;
#46387 = CARTESIAN_POINT ( 'NONE',  ( -58.28906562901213562, -14.21045842199421294, 78.48115787639689245 ) ) ;
#46388 = CARTESIAN_POINT ( 'NONE',  ( -55.72770594965891178, -56.85688678655485262, 69.22944270131350208 ) ) ;
#46389 = AXIS2_PLACEMENT_3D ( 'NONE', #55775, #104345, #55258 ) ;
#46390 = ORIENTED_EDGE ( 'NONE', *, *, #51954, .T. ) ;
#46391 = CARTESIAN_POINT ( 'NONE',  ( 43.99225961071574176, 464.6045839418123364, 10.45666854317311589 ) ) ;
#46392 = EDGE_LOOP ( 'NONE', ( #79910, #30116, #74025, #77682 ) ) ;
#46393 = CARTESIAN_POINT ( 'NONE',  ( -99.16296381929923598, -37.78500836856461831, 191.7250047312669210 ) ) ;
#46394 = CARTESIAN_POINT ( 'NONE',  ( -30.42269336643015620, 12.90989212739755665, -41.86604079465153916 ) ) ;
#46395 = ADVANCED_FACE ( 'NONE', ( #41345 ), #105550, .F. ) ;
#46396 = AXIS2_PLACEMENT_3D ( 'NONE', #2818, #92354, #67043 ) ;
#46397 = ORIENTED_EDGE ( 'NONE', *, *, #16456, .F. ) ;
#46398 = CARTESIAN_POINT ( 'NONE',  ( 0.000000000000000000, 0.5000000000000000000, 0.000000000000000000 ) ) ;
#46399 =( LENGTH_UNIT ( ) NAMED_UNIT ( * ) SI_UNIT ( .MILLI., .METRE. ) );
#46400 = CARTESIAN_POINT ( 'NONE',  ( 37.33349330513379982, 1.593028355512270567E-15, 0.000000000000000000 ) ) ;
#46401 = LINE ( 'NONE', #38846, #69776 ) ;
#46402 = CARTESIAN_POINT ( 'NONE',  ( 6.162888688655344005, -3.752776749732561257, 6.500000000000000000 ) ) ;
#46403 =( BOUNDED_SURFACE ( )  B_SPLINE_SURFACE ( 3, 2, ( 
 ( #14553, #5431, #97598 ),
 ( #104108, #31329, #22166 ),
 ( #79834, #55541, #80355 ),
 ( #64211, #23765, #40441 ) ),
 .UNSPECIFIED., .F., .F., .F. ) 
 B_SPLINE_SURFACE_WITH_KNOTS ( ( 4, 4 ),
 ( 3, 3 ),
 ( 0.01401837328402455105, 0.01447126798403660167 ),
 ( 0.1702042094205807321, 1.000000000000000000 ),
 .UNSPECIFIED. ) 
 GEOMETRIC_REPRESENTATION_ITEM ( )  RATIONAL_B_SPLINE_SURFACE ( (
 ( 0.9213079014936687017, 0.7688303398187987803, 1.000000000000000000),
 ( 0.9199763408694713318, 0.7649186838476262906, 1.000000000000000000),
 ( 0.9186293857494203241, 0.7609618042715087238, 1.000000000000000000),
 ( 0.9172666068268391371, 0.7569584399386861673, 1.000000000000000000) ) ) 
 REPRESENTATION_ITEM ( '' )  SURFACE ( )  );
#46404 =( NAMED_UNIT ( * ) SI_UNIT ( $, .STERADIAN. ) SOLID_ANGLE_UNIT ( ) );
#46406 = CARTESIAN_POINT ( 'NONE',  ( 62.03678553237772775, -30.00000000000000000, 72.12393787702889369 ) ) ;
#46405 = UNCERTAINTY_MEASURE_WITH_UNIT (LENGTH_MEASURE( 1.000000000000000082E-05 ), #3078, 'distance_accuracy_value', 'NONE');
#46407 = EDGE_CURVE ( 'NONE', #8098, #50266, #4532, .T. ) ;
#46408 = CARTESIAN_POINT ( 'NONE',  ( -7.847409547159631238, 80.92320383547315998, 4.333342374871287676E-31 ) ) ;
#46409 = DIRECTION ( 'NONE',  ( -0.2284631855477322060, 0.3307511317731628431, 0.9156463627843199893 ) ) ;
#46410 = CARTESIAN_POINT ( 'NONE',  ( 3.313708498984722972, -24.21874999999998934, -8.000000000000040856 ) ) ;
#46411 = CARTESIAN_POINT ( 'NONE',  ( -28.67889886441531289, -56.86647899729697997, 35.73133030458858173 ) ) ;
#46412 = ORIENTED_EDGE ( 'NONE', *, *, #69720, .T. ) ;
#46413 = ORIENTED_EDGE ( 'NONE', *, *, #29080, .F. ) ;
#46414 = CARTESIAN_POINT ( 'NONE',  ( 48.33509361711793417, -42.98009849617663036, 49.20160666384766301 ) ) ;
#46415 = CARTESIAN_POINT ( 'NONE',  ( -1.250939209597460522, 10.43205495851956499, 50.60755518596315028 ) ) ;
#46416 = AXIS2_PLACEMENT_3D ( 'NONE', #42339, #25124, #101112 ) ;
#46417 = DIRECTION ( 'NONE',  ( 0.000000000000000000, -1.000000000000000000, 0.000000000000000000 ) ) ;
#46418 = CARTESIAN_POINT ( 'NONE',  ( -110.5695627141435011, -38.35612508034719781, 181.7239276426034280 ) ) ;
#46419 = ORIENTED_EDGE ( 'NONE', *, *, #85769, .T. ) ;
#46420 = CARTESIAN_POINT ( 'NONE',  ( 88.64318705069558746, -38.37819253202206227, -18.64980564892555748 ) ) ;
#46421 = FILL_AREA_STYLE ('',( #62099 ) ) ;
#46422 = CARTESIAN_POINT ( 'NONE',  ( -19.50010530980351220, 50.00000000000000000, 59.90637122617393828 ) ) ;
#46423 = DIRECTION ( 'NONE',  ( 0.000000000000000000, 0.000000000000000000, 1.000000000000000000 ) ) ;
#46424 = AXIS2_PLACEMENT_3D ( 'NONE', #84283, #36834, #28744 ) ;
#46425 = VECTOR ( 'NONE', #59564, 1000.000000000000000 ) ;
#46426 = CARTESIAN_POINT ( 'NONE',  ( -32.70906958965466060, 434.6718458994130287, 17.16895555686161501 ) ) ;
#46427 = CARTESIAN_POINT ( 'NONE',  ( 3.313708498984762496, -17.46875000409676915, 7.999999999999998224 ) ) ;
#46428 = CARTESIAN_POINT ( 'NONE',  ( 12.50000000000000000, -3.000000000000000000, -8.595933841506987250 ) ) ;
#46429 = CARTESIAN_POINT ( 'NONE',  ( 99.55086857495790298, -59.99999999999998579, 202.0088339642364019 ) ) ;
#46430 = EDGE_CURVE ( 'NONE', #83401, #22025, #105170, .T. ) ;
#46431 = VERTEX_POINT ( 'NONE', #34361 ) ;
#46432 = CARTESIAN_POINT ( 'NONE',  ( -29.84307261967341063, 307.6666711317456020, -8.906761001086930918 ) ) ;
#46433 = CARTESIAN_POINT ( 'NONE',  ( 7.934203308536660337, 33.86700340017797117, 1.057099537198553652 ) ) ;
#46434 = FILL_AREA_STYLE ('',( #4917 ) ) ;
#46435 = ORIENTED_EDGE ( 'NONE', *, *, #85508, .F. ) ;
#46437 = CARTESIAN_POINT ( 'NONE',  ( 5.293610867670049736, 18.51054415109676654, -37.87873510570408087 ) ) ;
#46436 = CARTESIAN_POINT ( 'NONE',  ( -91.36008717904577736, -38.39848663321568267, -9.799652820967615696 ) ) ;
#46438 = DIRECTION ( 'NONE',  ( 0.000000000000000000, -1.000000000000000000, 0.000000000000000000 ) ) ;
#46439 = CARTESIAN_POINT ( 'NONE',  ( -50.94745919686192082, 50.00000000000000000, -37.05882352941185331 ) ) ;
#46440 = FILL_AREA_STYLE_COLOUR ( '', #90271 ) ;
#46441 = CARTESIAN_POINT ( 'NONE',  ( 2.977408999572650927, -13.25000000204838280, -7.188101187500001821 ) ) ;
#46442 = CARTESIAN_POINT ( 'NONE',  ( 2.617478844990903664, -3.000000000000002665, -94.73972676610405586 ) ) ;
#46443 = AXIS2_PLACEMENT_3D ( 'NONE', #94867, #5314, #85712 ) ;
#46444 = CARTESIAN_POINT ( 'NONE',  ( 0.000000000000000000, 0.000000000000000000, 5.000000000000002665 ) ) ;
#46445 = CONICAL_SURFACE ( 'NONE', #11939, 5.000000000000001776, 0.9599310885968803664 ) ;
#46447 = VERTEX_POINT ( 'NONE', #78360 ) ;
#46446 = FACE_OUTER_BOUND ( 'NONE', #13108, .T. ) ;
#46448 = CARTESIAN_POINT ( 'NONE',  ( 85.40742040225673293, -21.99728074668004396, 165.0038221370978988 ) ) ;
#46449 = CARTESIAN_POINT ( 'NONE',  ( 0.000000000000000000, 1.005902684993156715, -14.99698745252234566 ) ) ;
#46450 = DIRECTION ( 'NONE',  ( 0.5735764363510462704, 0.8191520442889915765, 0.000000000000000000 ) ) ;
#46451 = EDGE_LOOP ( 'NONE', ( #35557, #34904 ) ) ;
#46452 = CARTESIAN_POINT ( 'NONE',  ( -37.64086492829254382, 431.4026006243604456, 5.263644812418108110 ) ) ;
#46453 = CARTESIAN_POINT ( 'NONE',  ( 17.39415106586603343, 34.16989912227196413, 24.14244565807133469 ) ) ;
#46454 = CARTESIAN_POINT ( 'NONE',  ( 1.347111479062088996E-15, -46.00000000000000000, 100.9999999999999858 ) ) ;
#46455 = DIRECTION ( 'NONE',  ( 0.000000000000000000, -1.000000000000000000, 0.000000000000000000 ) ) ;
#46456 = CARTESIAN_POINT ( 'NONE',  ( -34.37606913705030820, 42.68840706779676708, -63.24071832532951731 ) ) ;
#46457 = DIRECTION ( 'NONE',  ( 0.000000000000000000, 0.000000000000000000, 1.000000000000000000 ) ) ;
#46458 = B_SPLINE_SURFACE_WITH_KNOTS ( 'NONE', 1, 3, ( 
 ( #57208, #48057, #90127, #62299, #82014, #89604, #21322, #15698 ),
 ( #73388, #54158, #32451, #73929, #32979, #12646, #13176, #45577 ) ),
 .UNSPECIFIED., .F., .F., .F.,
 ( 2, 2 ),
 ( 4, 2, 2, 4 ),
 ( 0.000000000000000000, 1.000000000000000000 ),
 ( 0.000000000000000000, 0.04450745600790868145, 0.06676118401186306728, 0.08901491201581737678 ),
 .UNSPECIFIED. ) ;
#46459 = EDGE_CURVE ( 'NONE', #37408, #22823, #86257, .T. ) ;
#46460 = ORIENTED_EDGE ( 'NONE', *, *, #7251, .T. ) ;
#46461 = CARTESIAN_POINT ( 'NONE',  ( -9.145685108131942798, 294.9588331864474640, 4.056731813190911140 ) ) ;
#46462 = ADVANCED_FACE ( 'NONE', ( #68293 ), #100113, .T. ) ;
#46463 = CARTESIAN_POINT ( 'NONE',  ( -1.000000000000000000, -48.53184174326406009, 2.645245988156326611 ) ) ;
#46464 = DIRECTION ( 'NONE',  ( 1.000000000000000000, 0.000000000000000000, -0.000000000000000000 ) ) ;
#46466 = CARTESIAN_POINT ( 'NONE',  ( -14.77855167844241535, 5.771020710681859178, -6.929713172033096669 ) ) ;
#46465 = CARTESIAN_POINT ( 'NONE',  ( -20.97754405179121662, 294.8763868968453608, 9.942224931492262385 ) ) ;
#46467 = AXIS2_PLACEMENT_3D ( 'NONE', #2739, #44282, #91770 ) ;
#46468 = CARTESIAN_POINT ( 'NONE',  ( 2.977408999572650927, -20.37500000204838457, -7.188101187500001821 ) ) ;
#46469 = CARTESIAN_POINT ( 'NONE',  ( 15.43345822995523342, 294.5569497680363042, -10.06267294328710271 ) ) ;
#46470 = DIRECTION ( 'NONE',  ( -1.000000000000000000, 0.000000000000000000, 0.000000000000000000 ) ) ;
#46471 = CONICAL_SURFACE ( 'NONE', #99811, 5.000000000000000000, 0.9599310885968913576 ) ;
#46472 = ORIENTED_EDGE ( 'NONE', *, *, #43026, .T. ) ;
#46473 = DIRECTION ( 'NONE',  ( 0.000000000000000000, 0.000000000000000000, 1.000000000000000000 ) ) ;
#46474 = CARTESIAN_POINT ( 'NONE',  ( 0.000000000000000000, -100.0000000000000000, 0.000000000000000000 ) ) ;
#46475 = CARTESIAN_POINT ( 'NONE',  ( -9.076657995136841350, 14.02231722287513804, 6.347424771477776860E-13 ) ) ;
#46476 = CARTESIAN_POINT ( 'NONE',  ( -7.230783165911326194, -2.999999999999882760, -70.90935356276069967 ) ) ;
#46477 = ADVANCED_FACE ( 'NONE', ( #9494 ), #58676, .T. ) ;
#46478 = CARTESIAN_POINT ( 'NONE',  ( 6.575925811255156184, 3.850887307289501571, 6.669932470447524686 ) ) ;
#46479 = ORIENTED_EDGE ( 'NONE', *, *, #66582, .T. ) ;
#46480 = FACE_OUTER_BOUND ( 'NONE', #48913, .T. ) ;
#46481 = VERTEX_POINT ( 'NONE', #67236 ) ;
#46482 = AXIS2_PLACEMENT_3D ( 'NONE', #9418, #1322, #67159 ) ;
#46483 = CARTESIAN_POINT ( 'NONE',  ( 32.04230769230768772, 4.172000000000003261, 0.000000000000000000 ) ) ;
#46484 = EDGE_CURVE ( 'NONE', #81058, #82447, #82872, .T. ) ;
#46485 = CARTESIAN_POINT ( 'NONE',  ( -45.44351312664282716, 39.21094759328430257, -45.67963897325379463 ) ) ;
#46486 = SURFACE_STYLE_FILL_AREA ( #935 ) ;
#46487 = CARTESIAN_POINT ( 'NONE',  ( -109.0225424287328480, -59.99999999999999289, 136.1364017776934077 ) ) ;
#46488 = DIRECTION ( 'NONE',  ( 1.000000000000000000, 0.000000000000000000, 0.000000000000000000 ) ) ;
#46489 = CARTESIAN_POINT ( 'NONE',  ( 0.000000000000000000, 0.000000000000000000, 0.000000000000000000 ) ) ;
#46490 = CARTESIAN_POINT ( 'NONE',  ( 1.489880555935390203E-15, 34.19642918197134662, 12.16579798332631945 ) ) ;
#46491 = EDGE_CURVE ( 'NONE', #27869, #55349, #96558, .T. ) ;
#46492 = CARTESIAN_POINT ( 'NONE',  ( -84.60744667541021613, -35.87728133031075828, 178.5872408570687924 ) ) ;
#46493 = CARTESIAN_POINT ( 'NONE',  ( 46.38169941325361378, 41.13208785335375239, -46.73570547342293935 ) ) ;
#46494 = ORIENTED_EDGE ( 'NONE', *, *, #19163, .T. ) ;
#46495 = EDGE_CURVE ( 'NONE', #35442, #93186, #62218, .T. ) ;
#46496 = CARTESIAN_POINT ( 'NONE',  ( -6.928203230275510549, 85.00000000000000000, -4.000000000000000000 ) ) ;
#46497 = CARTESIAN_POINT ( 'NONE',  ( -87.44129366413766036, -60.15208811969213087, 34.29055148929769814 ) ) ;
#46498 = FACE_OUTER_BOUND ( 'NONE', #7780, .T. ) ;
#46499 = CARTESIAN_POINT ( 'NONE',  ( 0.000000000000000000, -4.000000000000003553, 112.0000000000000000 ) ) ;
#46500 = CARTESIAN_POINT ( 'NONE',  ( 8.167402502808952747, 112.7203465494860097, 0.000000000000000000 ) ) ;
#46501 = FACE_OUTER_BOUND ( 'NONE', #60168, .T. ) ;
#46502 = CARTESIAN_POINT ( 'NONE',  ( -1.233923992984923027E-14, 18.64316884711714195, -38.36535705883633085 ) ) ;
#46503 = CARTESIAN_POINT ( 'NONE',  ( 75.52921836606891759, -59.99999999999984368, 193.8580410961210134 ) ) ;
#46504 = CARTESIAN_POINT ( 'NONE',  ( -112.0516705497441876, -59.99999999999997868, 140.8505598867089645 ) ) ;
#46505 = CARTESIAN_POINT ( 'NONE',  ( -63.26349711878434334, -56.86881976255739346, 90.13409198860577476 ) ) ;
#46506 = ORIENTED_EDGE ( 'NONE', *, *, #99922, .T. ) ;
#46507 = CARTESIAN_POINT ( 'NONE',  ( -14.79725422420208858, 39.42585232341617996, 63.36302458054748854 ) ) ;
#46508 = CARTESIAN_POINT ( 'NONE',  ( 83.38104608230275971, -59.99999999998523492, 202.0684823824225589 ) ) ;
#46509 = EDGE_LOOP ( 'NONE', ( #47358, #93658, #102968 ) ) ;
#46510 = CARTESIAN_POINT ( 'NONE',  ( -33.82585650164656954, 464.6969192971417328, 6.993179704485911863 ) ) ;
#46511 = CARTESIAN_POINT ( 'NONE',  ( 2.977408999572652260, -16.81250000204838813, 7.188101187500000044 ) ) ;
#46512 = EDGE_CURVE ( 'NONE', #99443, #98362, #83931, .T. ) ;
#46513 = CARTESIAN_POINT ( 'NONE',  ( 32.95646543402837381, 485.7809766657144905, 5.067016726498170698 ) ) ;
#46514 = EDGE_LOOP ( 'NONE', ( #30888, #61735, #7909, #30124, #64167, #44016 ) ) ;
#46515 = CARTESIAN_POINT ( 'NONE',  ( -11.48443175375259706, 45.38933445805909628, 14.52341122396179784 ) ) ;
#46516 = VERTEX_POINT ( 'NONE', #1394 ) ;
#46517 = CARTESIAN_POINT ( 'NONE',  ( 18.86650669486618881, 1.474610560812782335E-15, 0.000000000000000000 ) ) ;
#46518 = SURFACE_STYLE_USAGE ( .BOTH. , #55122 ) ;
#46519 = CARTESIAN_POINT ( 'NONE',  ( -91.91800064235249579, -60.00000000000000000, 8.006063584207543826 ) ) ;
#46520 = CARTESIAN_POINT ( 'NONE',  ( 36.74063307289657132, 396.2865697957464590, 6.153410032987091327 ) ) ;
#46521 = CARTESIAN_POINT ( 'NONE',  ( 5.082755093536325930, -34.34375000204838813, -5.082755093536325042 ) ) ;
#46522 = TOROIDAL_SURFACE ( 'NONE', #67251, 62.00000000000000000, 0.5000000000000000000 ) ;
#46523 = CARTESIAN_POINT ( 'NONE',  ( 46.84999999999999432, 1.533819458162526451E-15, 0.000000000000000000 ) ) ;
#46524 = CARTESIAN_POINT ( 'NONE',  ( 5.000000000000000000, -49.63763114970241475, 7.479721976420974805 ) ) ;
#46525 = AXIS2_PLACEMENT_3D ( 'NONE', #13231, #97334, #6195 ) ;
#46526 = CARTESIAN_POINT ( 'NONE',  ( -6.145467200824003662, 48.00000000000000000, -77.00333157709306420 ) ) ;
#46527 = EDGE_CURVE ( 'NONE', #3051, #95088, #52094, .T. ) ;
#46528 = CARTESIAN_POINT ( 'NONE',  ( -7.212408192734267587, 107.0151708932036883, -3.465038817813882233 ) ) ;
#46529 = PLANE ( 'NONE',  #40974 ) ;
#46530 = CARTESIAN_POINT ( 'NONE',  ( 21.98474283332737045, 303.0789298805325416, -9.951410097099058660 ) ) ;
#46531 = VECTOR ( 'NONE', #29656, 1000.000000000000000 ) ;
#46532 = ORIENTED_EDGE ( 'NONE', *, *, #24131, .F. ) ;
#46533 = CARTESIAN_POINT ( 'NONE',  ( -9.325077861619707420, 53.46604456964644214, -3.783146714563820012 ) ) ;
#46534 = FILL_AREA_STYLE_COLOUR ( '', #5917 ) ;
#46535 = CARTESIAN_POINT ( 'NONE',  ( 32.49827954884306536, -22.15127066472643591, 30.86793192670277719 ) ) ;
#46536 = CARTESIAN_POINT ( 'NONE',  ( 19.43146043914768129, -2.896176105056903703E-12, 11.19959342721819695 ) ) ;
#46537 = ORIENTED_EDGE ( 'NONE', *, *, #26774, .F. ) ;
#46538 = ADVANCED_FACE ( 'NONE', ( #92023 ), #87935, .T. ) ;
#46539 = CARTESIAN_POINT ( 'NONE',  ( -43.18793366350591612, 465.6364658675350370, 10.75294125769769416 ) ) ;
#46540 = CONICAL_SURFACE ( 'NONE', #1779, 8.500000000000000000, 0.7853981633974504994 ) ;
#46541 = EDGE_LOOP ( 'NONE', ( #13847, #36602, #39293, #76143, #4559, #89395 ) ) ;
#46543 = CARTESIAN_POINT ( 'NONE',  ( 45.48126212248870814, 413.7349014071057240, 8.309231847991947362 ) ) ;
#46542 = CARTESIAN_POINT ( 'NONE',  ( 8.743816783185534902, -5.000000000000000888, -16.78777973705476612 ) ) ;
#46544 = CARTESIAN_POINT ( 'NONE',  ( 6.123233995736766282E-16, 70.00000000000000000, -5.000000000000000000 ) ) ;
#46545 = CARTESIAN_POINT ( 'NONE',  ( 32.62207953394533178, 1.482358050883964840E-15, 0.000000000000000000 ) ) ;
#46546 = CARTESIAN_POINT ( 'NONE',  ( 6.400000000000000355, 4.618802153517003184, -8.000000000000000000 ) ) ;
#46547 = CYLINDRICAL_SURFACE ( 'NONE', #8638, 6.999999999999993783 ) ;
#46548 = CARTESIAN_POINT ( 'NONE',  ( -4.764086639414292002, -47.35998716217660132, 42.85178489487338283 ) ) ;
#46549 = ORIENTED_EDGE ( 'NONE', *, *, #100457, .F. ) ;
#46550 = VECTOR ( 'NONE', #22392, 999.9999999999998863 ) ;
#46551 = CARTESIAN_POINT ( 'NONE',  ( 95.81779620297204758, -60.00000000000000711, 54.82891626782047467 ) ) ;
#46552 = CARTESIAN_POINT ( 'NONE',  ( 27.26512758450284579, 34.42275309689889440, -10.05698433968635719 ) ) ;
#46553 = CARTESIAN_POINT ( 'NONE',  ( 6.162888688655344005, 3.752776749732565253, 6.499999999999997335 ) ) ;
#46554 = CYLINDRICAL_SURFACE ( 'NONE', #7741, 4.000000000000000000 ) ;
#46555 = DIRECTION ( 'NONE',  ( 0.000000000000000000, 1.000000000000000000, -0.000000000000000000 ) ) ;
#46556 = ORIENTED_EDGE ( 'NONE', *, *, #69560, .F. ) ;
#46557 = CARTESIAN_POINT ( 'NONE',  ( -88.16932760057679275, -29.99999999999833022, -16.71407748645461666 ) ) ;
#46558 = ORIENTED_EDGE ( 'NONE', *, *, #43901, .F. ) ;
#46559 = FILL_AREA_STYLE ('',( #13647 ) ) ;
#46560 = FILL_AREA_STYLE ('',( #45520 ) ) ;
#46561 = CARTESIAN_POINT ( 'NONE',  ( 42.98746414932995208, 5.000000000000003553, 0.000000000000000000 ) ) ;
#46562 = CARTESIAN_POINT ( 'NONE',  ( 16.14595037822608603, 20.23371447308070259, -4.922994507608427384 ) ) ;
#46563 = CARTESIAN_POINT ( 'NONE',  ( -5.082755093536326818, -30.59375000204838813, 5.082755093536325042 ) ) ;
#46564 = AXIS2_PLACEMENT_3D ( 'NONE', #26211, #34286, #37483 ) ;
#46565 = CARTESIAN_POINT ( 'NONE',  ( -43.71297783477830734, 485.1278128289774259, -1.116606130290624721 ) ) ;
#46566 = CARTESIAN_POINT ( 'NONE',  ( 39.44615384615384812, 4.172000000000003261, 0.000000000000000000 ) ) ;
#46567 = DIRECTION ( 'NONE',  ( -1.000000000000000000, 0.000000000000000000, 0.000000000000000000 ) ) ;
#46568 = VERTEX_POINT ( 'NONE', #70285 ) ;
#46570 = VERTEX_POINT ( 'NONE', #51560 ) ;
#46569 = CARTESIAN_POINT ( 'NONE',  ( 75.30000000000001137, 0.000000000000000000, 0.000000000000000000 ) ) ;
#46571 = CARTESIAN_POINT ( 'NONE',  ( 78.75440294992556289, -29.08478707705966215, 129.2257095857447666 ) ) ;
#46572 = CARTESIAN_POINT ( 'NONE',  ( 14.71845092680647760, 2.464670597979462308, -2.845879451958821527 ) ) ;
#46573 = ORIENTED_EDGE ( 'NONE', *, *, #42229, .F. ) ;
#46574 = DIRECTION ( 'NONE',  ( 0.000000000000000000, 0.000000000000000000, -1.000000000000000000 ) ) ;
#46575 = CARTESIAN_POINT ( 'NONE',  ( 6.944031699373470090, -85.53460654556131715, 3.972913591453824278 ) ) ;
#46576 = CARTESIAN_POINT ( 'NONE',  ( -1.320432766682874540E-15, -18.03125000204838457, 7.188101187500000044 ) ) ;
#46577 = CARTESIAN_POINT ( 'NONE',  ( -22.17556693859086536, -57.67274538812966256, 42.55074624272938877 ) ) ;
#46578 = CARTESIAN_POINT ( 'NONE',  ( 19.99629473115066958, 294.7507145989418404, 9.915512459802851453 ) ) ;
#46579 = EDGE_CURVE ( 'NONE', #84500, #72783, #81059, .T. ) ;
#46580 = ORIENTED_EDGE ( 'NONE', *, *, #95812, .F. ) ;
#46581 = COLOUR_RGB ( '', 0.31764706, 0.68627451, 0.89019608) ;
#46582 = CARTESIAN_POINT ( 'NONE',  ( 2.869469963220363962, 64.67082520353208963, 5.000000000000000000 ) ) ;
#46583 = ADVANCED_FACE ( 'NONE', ( #37420 ), #17332, .T. ) ;
#46584 = CARTESIAN_POINT ( 'NONE',  ( 7.217786572945549040, 41.17942765912351177, -58.69595075570492071 ) ) ;
#46585 = CARTESIAN_POINT ( 'NONE',  ( 55.26095113931063452, 6.856755485862130937E-15, 0.000000000000000000 ) ) ;
#46586 = CARTESIAN_POINT ( 'NONE',  ( 3.313708498984762052, -9.406250004096769146, -8.000000000000000000 ) ) ;
#46587 = VECTOR ( 'NONE', #14488, 999.9999999999998863 ) ;
#46588 = CARTESIAN_POINT ( 'NONE',  ( -6.501439726548199793, -13.08475520213678678, 32.05172811864072457 ) ) ;
#46589 = CARTESIAN_POINT ( 'NONE',  ( 10.00000000000003730, 14.99999999999998934, 4.210530276628143831 ) ) ;
#46590 = CARTESIAN_POINT ( 'NONE',  ( 28.09999999999999787, 1.533819458162526451E-15, 0.000000000000000000 ) ) ;
#46591 = CARTESIAN_POINT ( 'NONE',  ( 7.500000000000001776, 9.462792962020666110, -29.31754814678773968 ) ) ;
#46592 = DIRECTION ( 'NONE',  ( 0.000000000000000000, -1.000000000000000000, 0.000000000000000000 ) ) ;
#46593 = DIRECTION ( 'NONE',  ( 4.382630684334561370E-17, 4.930380657631323784E-32, -0.9999999999999997780 ) ) ;
#46594 = CARTESIAN_POINT ( 'NONE',  ( -9.089383533625918332, -13.56607094171270056, 16.34888743995582061 ) ) ;
#46595 = ORIENTED_EDGE ( 'NONE', *, *, #84212, .T. ) ;
#46596 = CARTESIAN_POINT ( 'NONE',  ( -2.273600070709648424, -49.89527936504848782, 40.92025501607385252 ) ) ;
#46597 = MECHANICAL_DESIGN_GEOMETRIC_PRESENTATION_REPRESENTATION (  '', ( #24219 ), #49 ) ;
#46598 = DIRECTION ( 'NONE',  ( -1.000000000000000000, -1.224606353822377258E-16, -0.000000000000000000 ) ) ;
#46599 = CARTESIAN_POINT ( 'NONE',  ( -3.222962768498216414E-17, 13.85270131633358304, -7.000000000000011546 ) ) ;
#46600 = VECTOR ( 'NONE', #58488, 1000.000000000000000 ) ;
#46601 = CARTESIAN_POINT ( 'NONE',  ( -66.59044967886386246, -29.86133635736485559, -22.39369228100312981 ) ) ;
#46602 = CARTESIAN_POINT ( 'NONE',  ( -66.46769023514099217, -30.00000000000000711, 84.48792742084529550 ) ) ;
#46603 = DIRECTION ( 'NONE',  ( 1.000000000000000000, 1.224606353822377258E-16, 0.000000000000000000 ) ) ;
#46604 = EDGE_CURVE ( 'NONE', #66185, #81976, #54758, .T. ) ;
#46605 = ORIENTED_EDGE ( 'NONE', *, *, #65444, .T. ) ;
#46606 = AXIS2_PLACEMENT_3D ( 'NONE', #104168, #30310, #96093 ) ;
#46607 = CARTESIAN_POINT ( 'NONE',  ( 13.37207953394533355, -5.000000000000000888, 6.123233995736769241E-16 ) ) ;
#46608 = CARTESIAN_POINT ( 'NONE',  ( 97.17653136007717762, -57.62292585091598340, 204.4293388724284171 ) ) ;
#46609 = DIRECTION ( 'NONE',  ( 0.000000000000000000, -1.000000000000000000, 0.000000000000000000 ) ) ;
#46611 = CARTESIAN_POINT ( 'NONE',  ( 7.500000000000001776, 1.028703311283776783E-15, -8.400000000000000355 ) ) ;
#46610 = AXIS2_PLACEMENT_3D ( 'NONE', #12463, #4929, #29245 ) ;
#46612 = CARTESIAN_POINT ( 'NONE',  ( -16.11696382278816841, 21.57140452653678153, 2.149593460082904972 ) ) ;
#46613 = LINE ( 'NONE', #53122, #54635 ) ;
#46614 = CARTESIAN_POINT ( 'NONE',  ( -73.91699298931344231, -60.00000000000000000, 171.3787799675980352 ) ) ;
#46615 = SURFACE_STYLE_USAGE ( .BOTH. , #13704 ) ;
#46616 = CARTESIAN_POINT ( 'NONE',  ( -9.165151389911681434, 30.00000000000000000, -4.000000000000000000 ) ) ;
#46617 = CARTESIAN_POINT ( 'NONE',  ( -65.26738680893376454, 49.99999999999999289, 0.8120011905356555593 ) ) ;
#46618 = CARTESIAN_POINT ( 'NONE',  ( -85.16857999255211098, -46.56716161443675617, 187.9269890765743583 ) ) ;
#46619 = VERTEX_POINT ( 'NONE', #47047 ) ;
#46620 = CARTESIAN_POINT ( 'NONE',  ( 32.84463799220507241, 316.8457873297845708, -6.870995899933766360 ) ) ;
#46621 = DIRECTION ( 'NONE',  ( -0.000000000000000000, 1.000000000000000000, -0.000000000000000000 ) ) ;
#46622 = EDGE_CURVE ( 'NONE', #6703, #37867, #21384, .T. ) ;
#46623 = CARTESIAN_POINT ( 'NONE',  ( -29.42328174557860265, 308.7510679269275897, -8.882624838725998728 ) ) ;
#46624 = CARTESIAN_POINT ( 'NONE',  ( -83.11894961437765517, -45.25969856680515591, -14.26080704251342368 ) ) ;
#46625 = DIRECTION ( 'NONE',  ( 0.000000000000000000, 1.000000000000000000, -0.000000000000000000 ) ) ;
#46626 = DIRECTION ( 'NONE',  ( 0.000000000000000000, 0.000000000000000000, 1.000000000000000000 ) ) ;
#46627 = ORIENTED_EDGE ( 'NONE', *, *, #51259, .F. ) ;
#46628 = PRESENTATION_LAYER_ASSIGNMENT (  '', '', ( #31119 ) ) ;
#46629 = CARTESIAN_POINT ( 'NONE',  ( 18.47404693474707571, 50.00000000000000711, 61.29115758976740835 ) ) ;
#46630 = CARTESIAN_POINT ( 'NONE',  ( 13.58261091780133789, 24.75325252249499997, 0.6700394777244487177 ) ) ;
#46631 = CARTESIAN_POINT ( 'NONE',  ( 25.22241582816893413, -4.285714285714286476, -3.301606509414618973 ) ) ;
#46632 = CARTESIAN_POINT ( 'NONE',  ( -36.93845425212112588, 463.9889438915046753, 19.60668832162587094 ) ) ;
#46633 = CARTESIAN_POINT ( 'NONE',  ( 93.93995408072316877, -60.00000000000007816, -15.95669063232190155 ) ) ;
#46634 = CARTESIAN_POINT ( 'NONE',  ( -81.45673704895914113, -25.62446345033223238, 139.9564592401801804 ) ) ;
#46635 = ORIENTED_EDGE ( 'NONE', *, *, #53034, .F. ) ;
#46636 = CARTESIAN_POINT ( 'NONE',  ( 42.40769230769231513, -4.171999999999999709, 0.000000000000000000 ) ) ;
#46637 = CARTESIAN_POINT ( 'NONE',  ( 1.899844911462918340, 42.00000000000000000, -68.00818075325166490 ) ) ;
#46638 = CARTESIAN_POINT ( 'NONE',  ( 100.2630844185923564, -57.62774964585633342, 203.8563738720838785 ) ) ;
#46639 = CARTESIAN_POINT ( 'NONE',  ( 58.66297648405128484, 49.99999999999999289, -23.00451178233782557 ) ) ;
#46640 = CARTESIAN_POINT ( 'NONE',  ( 37.19305974667213377, 304.2850609022308959, -7.836023120251422114 ) ) ;
#46641 = CARTESIAN_POINT ( 'NONE',  ( -11.52959627970376033, 12.35318608925452111, 9.999999999999845457 ) ) ;
#46642 = ORIENTED_EDGE ( 'NONE', *, *, #2642, .F. ) ;
#46643 = FACE_BOUND ( 'NONE', #69781, .T. ) ;
#46645 = CARTESIAN_POINT ( 'NONE',  ( -106.4266840043012081, -60.15521262700561778, 168.2409215529943083 ) ) ;
#46644 = CARTESIAN_POINT ( 'NONE',  ( -16.75187969033532553, 37.11970326878314808, 21.80698433968612093 ) ) ;
#46646 = CARTESIAN_POINT ( 'NONE',  ( 7.188101187500000044, -25.15625000204838813, 0.000000000000000000 ) ) ;
#46647 = CARTESIAN_POINT ( 'NONE',  ( 3.313708498984800688, -20.46875000409677270, 7.999999999999960032 ) ) ;
#46648 = LINE ( 'NONE', #62857, #89423 ) ;
#46649 = CARTESIAN_POINT ( 'NONE',  ( 7.150000000000015454, 41.65000000000000568, -68.91429206202192859 ) ) ;
#46650 = EDGE_CURVE ( 'NONE', #24684, #32861, #49163, .T. ) ;
#46651 = CARTESIAN_POINT ( 'NONE',  ( 26.02965699499564067, 37.04750560174652207, 9.465197022839127783 ) ) ;
#46652 = LINE ( 'NONE', #79552, #42185 ) ;
#46653 = AXIS2_PLACEMENT_3D ( 'NONE', #98130, #24279, #99180 ) ;
#46654 = B_SPLINE_CURVE_WITH_KNOTS ( 'NONE', 3,
 ( #75364, #59740, #1465, #49497 ),
 .UNSPECIFIED., .F., .F.,
 ( 4, 4 ),
 ( 0.0007474059274884787369, 0.02468721214969757730 ),
 .UNSPECIFIED. ) ;
#46655 = CARTESIAN_POINT ( 'NONE',  ( -24.20499783611711564, 27.76345924012371924, -31.17339665328801246 ) ) ;
#46656 = ORIENTED_EDGE ( 'NONE', *, *, #53366, .F. ) ;
#46657 = TOROIDAL_SURFACE ( 'NONE', #48329, 10.00000000000000000, 5.000000000000000000 ) ;
#46658 = CARTESIAN_POINT ( 'NONE',  ( 43.18011688740498499, 485.8502513089949844, 5.262111696943175154 ) ) ;
#46660 = CARTESIAN_POINT ( 'NONE',  ( 29.32191389812840754, -56.85782188410217231, 35.94437315274679889 ) ) ;
#46659 = CARTESIAN_POINT ( 'NONE',  ( -57.89926771889555113, -60.00000000000002132, 101.6232698676003139 ) ) ;
#46661 = CARTESIAN_POINT ( 'NONE',  ( -23.54482684487745558, 25.90709500613124305, 30.73892193297572462 ) ) ;
#46662 = EDGE_LOOP ( 'NONE', ( #52027, #56273, #21104 ) ) ;
#46663 = EDGE_CURVE ( 'NONE', #35844, #34646, #83659, .T. ) ;
#46664 = ORIENTED_EDGE ( 'NONE', *, *, #47901, .T. ) ;
#46665 = SURFACE_SIDE_STYLE ('',( #38598 ) ) ;
#46666 = CARTESIAN_POINT ( 'NONE',  ( -4.582575694955840717, 16.00000000000000000, -10.00000000000000000 ) ) ;
#46667 = CARTESIAN_POINT ( 'NONE',  ( 7.491624566500244775, 40.33173439531471161, -59.48415712631144459 ) ) ;
#46668 = DIRECTION ( 'NONE',  ( 0.000000000000000000, 0.000000000000000000, 1.000000000000000000 ) ) ;
#46669 = CARTESIAN_POINT ( 'NONE',  ( 89.64643850830432825, 6.123233995736568081E-16, -5.000000000000011546 ) ) ;
#46670 = CARTESIAN_POINT ( 'NONE',  ( -7.499999999999999112, 0.3744244963005058935, 2.466559942404519826E-15 ) ) ;
#46671 = ORIENTED_EDGE ( 'NONE', *, *, #104431, .F. ) ;
#46672 = CARTESIAN_POINT ( 'NONE',  ( 68.64488335302139888, -30.00000000000000000, 91.00168987598435422 ) ) ;
#46673 = CARTESIAN_POINT ( 'NONE',  ( -11.88733434657279808, 21.45620698160807294, 7.302873484819567551 ) ) ;
#46674 = MECHANICAL_DESIGN_GEOMETRIC_PRESENTATION_REPRESENTATION (  '', ( #7081 ), #70770 ) ;
#46677 = EDGE_CURVE ( 'NONE', #57533, #57762, #50032, .T. ) ;
#46676 = CARTESIAN_POINT ( 'NONE',  ( -4.472135954999578722, -65.00000000000000000, 4.000000000000002665 ) ) ;
#46675 = CIRCLE ( 'NONE', #129, 8.000000000000000000 ) ;
#46678 = CARTESIAN_POINT ( 'NONE',  ( 81.13835518361752008, -30.00000000000000711, 1.838030729709124733 ) ) ;
#46679 = CIRCLE ( 'NONE', #133, 57.86910460382442523 ) ;
#46680 = CARTESIAN_POINT ( 'NONE',  ( 6.500000000000000888, 0.000000000000000000, 1.734723475976807094E-15 ) ) ;
#46681 = ORIENTED_EDGE ( 'NONE', *, *, #55710, .T. ) ;
#46682 = CONICAL_SURFACE ( 'NONE', #22622, 4.172000000000009479, 0.9599310885968813656 ) ;
#46683 = ORIENTED_EDGE ( 'NONE', *, *, #70864, .F. ) ;
#46684 = EDGE_LOOP ( 'NONE', ( #13241, #11726, #16642, #32814, #68618, #33177 ) ) ;
#46685 = DIRECTION ( 'NONE',  ( -1.000000000000000000, 0.000000000000000000, 0.000000000000000000 ) ) ;
#46686 = CARTESIAN_POINT ( 'NONE',  ( 6.849999999999999645, 9.237604307034018802, 0.000000000000000000 ) ) ;
#46687 = DIRECTION ( 'NONE',  ( 0.000000000000000000, -1.000000000000000000, 0.000000000000000000 ) ) ;
#46689 = AXIS2_PLACEMENT_3D ( 'NONE', #45325, #21600, #102493 ) ;
#46688 = CARTESIAN_POINT ( 'NONE',  ( -37.70206801957033349, 409.1304537038757303, 6.512665395000928115 ) ) ;
#46690 = CARTESIAN_POINT ( 'NONE',  ( 0.000000000000000000, 0.000000000000000000, -6.838999999999999524 ) ) ;
#46691 = CARTESIAN_POINT ( 'NONE',  ( 35.59999999999999432, -3.309499999999999886, 0.000000000000000000 ) ) ;
#46692 = ORIENTED_EDGE ( 'NONE', *, *, #85794, .T. ) ;
#46693 = CARTESIAN_POINT ( 'NONE',  ( 30.42698073564668348, 7.740609016700362943, 41.86289218232744958 ) ) ;
#46694 = CIRCLE ( 'NONE', #77729, 1.000000000000000888 ) ;
#46695 = ORIENTED_EDGE ( 'NONE', *, *, #66782, .F. ) ;
#46696 = DIRECTION ( 'NONE',  ( -1.000000000000000000, -1.224606353822377258E-16, -0.000000000000000000 ) ) ;
#46697 = CARTESIAN_POINT ( 'NONE',  ( 60.37595104056737938, -38.34251102957333757, 97.59079878387926499 ) ) ;
#46698 = FACE_OUTER_BOUND ( 'NONE', #79282, .T. ) ;
#46699 = B_SPLINE_CURVE_WITH_KNOTS ( 'NONE', 3,
 ( #62381, #30019, #22988, #5195, #73075, #88238, #96861, #95274 ),
 .UNSPECIFIED., .F., .F.,
 ( 4, 2, 2, 4 ),
 ( 0.000000000000000000, 0.2500000000000000000, 0.5000000000000000000, 1.000000000000000000 ),
 .UNSPECIFIED. ) ;
#46700 = CARTESIAN_POINT ( 'NONE',  ( 1.333692126671238043, 297.3239193841515089, -10.00118529339073525 ) ) ;
#46701 = CARTESIAN_POINT ( 'NONE',  ( 62.79349362354685837, -42.95894226352011458, 81.57106949543961605 ) ) ;
#46702 = EDGE_LOOP ( 'NONE', ( #77207, #28121, #50577, #97798 ) ) ;
#46703 = CARTESIAN_POINT ( 'NONE',  ( 38.71676723733723691, 463.8587156194949443, 18.97100414386192924 ) ) ;
#46704 = CARTESIAN_POINT ( 'NONE',  ( -16.14595037822608603, 7.274337365578172232, 6.616591826369962348 ) ) ;
#46705 = CARTESIAN_POINT ( 'NONE',  ( 4.678819457397886517, 143.9212778189118467, 0.000000000000000000 ) ) ;
#46706 = CARTESIAN_POINT ( 'NONE',  ( 0.000000000000000000, 0.000000000000000000, 4.000000000000000000 ) ) ;
#46707 = EDGE_CURVE ( 'NONE', #38220, #104988, #31137, .T. ) ;
#46708 = ORIENTED_EDGE ( 'NONE', *, *, #84660, .F. ) ;
#46709 = AXIS2_PLACEMENT_3D ( 'NONE', #65062, #56418, #17056 ) ;
#46710 =( LENGTH_UNIT ( ) NAMED_UNIT ( * ) SI_UNIT ( .MILLI., .METRE. ) );
#46711 = CARTESIAN_POINT ( 'NONE',  ( -34.74708594651274751, -60.00000000000001421, -34.56281374097226688 ) ) ;
#46712 = AXIS2_PLACEMENT_3D ( 'NONE', #90291, #16400, #82186 ) ;
#46713 = EDGE_CURVE ( 'NONE', #47940, #28900, #9771, .T. ) ;
#46714 = EDGE_CURVE ( 'NONE', #16979, #31406, #39315, .T. ) ;
#46715 = CARTESIAN_POINT ( 'NONE',  ( 80.00000000000000000, -52.00000000000000000, -21.09707704303352926 ) ) ;
#46716 = CARTESIAN_POINT ( 'NONE',  ( -8.000000000000000000, -31.43750000409677270, -9.797174393178825657E-16 ) ) ;
#46717 = CARTESIAN_POINT ( 'NONE',  ( 7.137815226409024660, -5.000000000001136868, -4.175893272573466319 ) ) ;
#46718 = CARTESIAN_POINT ( 'NONE',  ( 86.30515197242765169, -50.14563283907419589, 191.1575415172119961 ) ) ;
#46719 = EDGE_CURVE ( 'NONE', #89196, #29099, #49709, .T. ) ;
#46720 = CARTESIAN_POINT ( 'NONE',  ( -5.220566466144580531, 6.884671715754390853, -27.36422395346735215 ) ) ;
#46721 = CARTESIAN_POINT ( 'NONE',  ( -4.460880975709559770, 9.623342354847359559, 4.999999999999999112 ) ) ;
#46722 = SURFACE_STYLE_FILL_AREA ( #80142 ) ;
#46723 = CARTESIAN_POINT ( 'NONE',  ( 18.13823877062313272, 304.6380157655604535, 9.891557580208379719 ) ) ;
#46724 = ORIENTED_EDGE ( 'NONE', *, *, #105016, .F. ) ;
#46725 = CARTESIAN_POINT ( 'NONE',  ( 13.60715398569422874, -51.55888882488000036, 30.29660545413128503 ) ) ;
#46726 = CARTESIAN_POINT ( 'NONE',  ( 0.000000000000000000, 0.000000000000000000, -9.078441367943003826 ) ) ;
#46728 =( BOUNDED_SURFACE ( )  B_SPLINE_SURFACE ( 3, 2, ( 
 ( #94978, #42018, #91129 ),
 ( #99728, #75449, #73307 ),
 ( #74376, #16686, #49577 ),
 ( #97581, #64711, #23750 ) ),
 .UNSPECIFIED., .F., .F., .F. ) 
 B_SPLINE_SURFACE_WITH_KNOTS ( ( 4, 4 ),
 ( 3, 3 ),
 ( 0.007402583550056900108, 0.03545809677458416909 ),
 ( 0.000000000000000000, 1.000000000000000000 ),
 .UNSPECIFIED. ) 
 GEOMETRIC_REPRESENTATION_ITEM ( )  RATIONAL_B_SPLINE_SURFACE ( (
 ( 1.000000000000000000, 0.8381405646299836532, 1.000000000000000000),
 ( 1.000000000000000000, 0.8381407646764915675, 1.000000000000000000),
 ( 1.000000000000000000, 0.8381408042060416452, 1.000000000000000000),
 ( 1.000000000000000000, 0.8381405998616443531, 1.000000000000000000) ) ) 
 REPRESENTATION_ITEM ( '' )  SURFACE ( )  );
#46727 = CARTESIAN_POINT ( 'NONE',  ( 22.57305893494933002, -60.00000000000001421, 40.62150767137644891 ) ) ;
#46729 = CARTESIAN_POINT ( 'NONE',  ( -99.80168451951495001, -29.99999999999999645, 186.4053763999687874 ) ) ;
#46730 = ADVANCED_FACE ( 'NONE', ( #44288 ), #24076, .T. ) ;
#46731 = VECTOR ( 'NONE', #96317, 1000.000000000000000 ) ;
#46732 = DIRECTION ( 'NONE',  ( -1.000000000000000000, -1.224606353822377258E-16, -0.000000000000000000 ) ) ;
#46733 = CARTESIAN_POINT ( 'NONE',  ( 52.17701213820809159, -57.67658653755371745, 83.19312597704137602 ) ) ;
#46735 = FACE_OUTER_BOUND ( 'NONE', #9505, .T. ) ;
#46734 = CARTESIAN_POINT ( 'NONE',  ( 9.041342019628906712, 43.82558486784927965, 14.35410957973725843 ) ) ;
#46736 = EDGE_CURVE ( 'NONE', #32960, #11528, #31680, .T. ) ;
#46737 = CARTESIAN_POINT ( 'NONE',  ( -20.94717588032531452, 41.83711825373250548, -78.41832805012246865 ) ) ;
#46738 = CARTESIAN_POINT ( 'NONE',  ( -17.60890209088405456, 50.00000000000000000, 62.65190115956760764 ) ) ;
#46739 = CARTESIAN_POINT ( 'NONE',  ( -9.999999999999998224, 15.00000000000000000, 1.836970198721029589E-15 ) ) ;
#46740 = CARTESIAN_POINT ( 'NONE',  ( 46.00000000000000000, 488.9831568219302653, 4.757012338623825443 ) ) ;
#46741 = CARTESIAN_POINT ( 'NONE',  ( 30.00000000000000000, 0.000000000000000000, 0.000000000000000000 ) ) ;
#46742 = DIRECTION ( 'NONE',  ( -1.000000000000000000, -0.000000000000000000, -0.000000000000000000 ) ) ;
#46743 = CARTESIAN_POINT ( 'NONE',  ( -87.30982930919684293, -31.68247253314202538, 188.1765524996390013 ) ) ;
#46744 = CIRCLE ( 'NONE', #81211, 1.000000000000000888 ) ;
#46745 = EDGE_LOOP ( 'NONE', ( #25203, #86096, #30938, #9061 ) ) ;
#46746 = CARTESIAN_POINT ( 'NONE',  ( 17.50000000000023803, 50.00318699355108976, 59.98279283212327329 ) ) ;
#46747 = CARTESIAN_POINT ( 'NONE',  ( -1.115477787493043715, -50.00000000000001421, 101.1904243682835585 ) ) ;
#46748 = CARTESIAN_POINT ( 'NONE',  ( -11.16598387641317203, -25.54968478433329437, 28.17206934784134731 ) ) ;
#46749 = CONICAL_SURFACE ( 'NONE', #60555, 4.172000000000001485, 0.9599310885968750373 ) ;
#46751 = CARTESIAN_POINT ( 'NONE',  ( -33.00000000000000000, 439.7597899781497972, 24.16317522621304192 ) ) ;
#46750 = CARTESIAN_POINT ( 'NONE',  ( -86.57246707375212225, -60.00000000000007105, -11.98479218909116462 ) ) ;
#46752 = ORIENTED_EDGE ( 'NONE', *, *, #95363, .T. ) ;
#46753 = CARTESIAN_POINT ( 'NONE',  ( -43.64095197017179828, 465.1110681766505763, 8.836794732693006083 ) ) ;
#46754 = CARTESIAN_POINT ( 'NONE',  ( 14.29190075645222180, 6.456385560667814438, -7.561819230143195902 ) ) ;
#46755 = DIRECTION ( 'NONE',  ( 0.000000000000000000, -1.000000000000000000, 0.000000000000000000 ) ) ;
#46756 = CIRCLE ( 'NONE', #55359, 5.000000000000002665 ) ;
#46757 = CARTESIAN_POINT ( 'NONE',  ( 15.93251508686769036, 3.184445033430845839, -1.451444771589639915 ) ) ;
#46758 = CARTESIAN_POINT ( 'NONE',  ( 65.85939646271809522, -59.99999999999997158, 121.8062760347599465 ) ) ;
#46759 = DIRECTION ( 'NONE',  ( 0.000000000000000000, -1.000000000000000000, 0.000000000000000000 ) ) ;
#46760 = ORIENTED_EDGE ( 'NONE', *, *, #82631, .F. ) ;
#46761 = FACE_OUTER_BOUND ( 'NONE', #82309, .T. ) ;
#46762 = FACE_OUTER_BOUND ( 'NONE', #91341, .T. ) ;
#46764 = CARTESIAN_POINT ( 'NONE',  ( 6.921856739985489781, 41.59435684990518922, -70.13580383465753698 ) ) ;
#46763 = CARTESIAN_POINT ( 'NONE',  ( 42.10926113833883022, -14.21045842199418452, 45.52176705710515847 ) ) ;
#46765 = CARTESIAN_POINT ( 'NONE',  ( 3.363235851038141710, 121.3096863609017078, -5.000000000000000000 ) ) ;
#46766 = CARTESIAN_POINT ( 'NONE',  ( -4.999999999999993783, -4.000000000000003553, 103.2791840072761858 ) ) ;
#46767 = ORIENTED_EDGE ( 'NONE', *, *, #9943, .F. ) ;
#46768 = VERTEX_POINT ( 'NONE', #59962 ) ;
#46769 = CARTESIAN_POINT ( 'NONE',  ( -24.48174174843943973, 306.7381792433261580, 9.359562147283707390 ) ) ;
#46770 = VERTEX_POINT ( 'NONE', #92825 ) ;
#46771 = CARTESIAN_POINT ( 'NONE',  ( 20.05055460606549644, 304.8393297837531577, 9.934348198929242812 ) ) ;
#46772 = PLANE ( 'NONE',  #9535 ) ;
#46773 = CARTESIAN_POINT ( 'NONE',  ( -1.469576158976823947E-15, -13.06250000409676915, 8.000000000000000000 ) ) ;
#46774 = ORIENTED_EDGE ( 'NONE', *, *, #63165, .T. ) ;
#46775 = EDGE_CURVE ( 'NONE', #17391, #94943, #70688, .T. ) ;
#46776 = CARTESIAN_POINT ( 'NONE',  ( -8.559508646656389885, -1.200000000000000030E-05, -2.781152949374503081 ) ) ;
#46777 = CARTESIAN_POINT ( 'NONE',  ( 5.000000000000000000, -14.21727251090713473, 9.320362779988997204 ) ) ;
#46779 = CARTESIAN_POINT ( 'NONE',  ( -111.9445188126430111, -59.99999999999511147, 192.8163573256921381 ) ) ;
#46778 = VECTOR ( 'NONE', #10681, 1000.000000000000000 ) ;
#46780 = EDGE_CURVE ( 'NONE', #55990, #74465, #55187, .T. ) ;
#46781 = CARTESIAN_POINT ( 'NONE',  ( 46.00000000000000000, 488.0336798547363628, -0.8984331811843099258 ) ) ;
#46782 = CARTESIAN_POINT ( 'NONE',  ( 70.42375229793672986, -60.00000000000000000, 143.5773913645265054 ) ) ;
#46783 = CARTESIAN_POINT ( 'NONE',  ( 6.281175601187038993, 3.752776749732557704, -6.500000000000006217 ) ) ;
#46784 = DIRECTION ( 'NONE',  ( -1.000000000000000000, -1.224606353822377258E-16, -0.000000000000000000 ) ) ;
#46785 = AXIS2_PLACEMENT_3D ( 'NONE', #37412, #22277, #70276 ) ;
#46787 = CARTESIAN_POINT ( 'NONE',  ( 9.411483143886608005, -60.35895712271108948, 33.95384518708878829 ) ) ;
#46786 = CARTESIAN_POINT ( 'NONE',  ( -95.73631051900581213, -30.00000000000000000, 71.50198832723137343 ) ) ;
#46788 = EDGE_CURVE ( 'NONE', #99943, #49522, #72447, .T. ) ;
#46789 = CARTESIAN_POINT ( 'NONE',  ( 0.000000000000000000, 0.000000000000000000, -6.275264681066861527 ) ) ;
#46790 = CARTESIAN_POINT ( 'NONE',  ( -47.02141968940689765, -36.07080552638146997, 45.21624500582201023 ) ) ;
#46791 = FACE_OUTER_BOUND ( 'NONE', #71310, .T. ) ;
#46792 = ORIENTED_EDGE ( 'NONE', *, *, #37988, .T. ) ;
#46793 = CARTESIAN_POINT ( 'NONE',  ( 1.832743656797419977E-15, 0.000000000000000000, -14.78272384904389192 ) ) ;
#46794 = DIRECTION ( 'NONE',  ( -0.000000000000000000, -0.000000000000000000, 1.000000000000000000 ) ) ;
#46795 = EDGE_CURVE ( 'NONE', #10346, #1638, #31316, .T. ) ;
#46796 = CARTESIAN_POINT ( 'NONE',  ( 89.06666666666666288, 1.023464760207051730E-14, 0.000000000000000000 ) ) ;
#46797 = ORIENTED_EDGE ( 'NONE', *, *, #12626, .T. ) ;
#46798 = CARTESIAN_POINT ( 'NONE',  ( -9.045860540270149741, -13.61258301273266191, 16.31186313544194277 ) ) ;
#46799 = ORIENTED_EDGE ( 'NONE', *, *, #106174, .F. ) ;
#46800 = CARTESIAN_POINT ( 'NONE',  ( 104.9189220841502106, -29.99999999999720046, 195.4889521351916528 ) ) ;
#46801 = CARTESIAN_POINT ( 'NONE',  ( -50.94745919686192082, 50.00000000000000000, -37.05882352941185331 ) ) ;
#46803 = EDGE_CURVE ( 'NONE', #82575, #38206, #65524, .T. ) ;
#46802 = CARTESIAN_POINT ( 'NONE',  ( 0.06730325657375718640, -1.557442666578432444, -8.000000000000001776 ) ) ;
#46804 = SURFACE_SIDE_STYLE ('',( #104502 ) ) ;
#46805 = CARTESIAN_POINT ( 'NONE',  ( 96.68547135186049957, -29.99999999999999289, 191.1807546223255940 ) ) ;
#46806 = DIRECTION ( 'NONE',  ( -1.000000000000000000, -0.000000000000000000, -0.000000000000000000 ) ) ;
#46807 = ORIENTED_EDGE ( 'NONE', *, *, #36730, .F. ) ;
#46808 = ORIENTED_EDGE ( 'NONE', *, *, #54205, .F. ) ;
#46809 = ORIENTED_EDGE ( 'NONE', *, *, #12747, .T. ) ;
#46810 = CARTESIAN_POINT ( 'NONE',  ( -28.32665330097506029, 36.29719140734747640, 9.120848346371911219 ) ) ;
#46811 = CARTESIAN_POINT ( 'NONE',  ( 43.00000000000000000, 461.4080316921935605, 3.462976341553817949 ) ) ;
#46812 = CARTESIAN_POINT ( 'NONE',  ( 56.22793774957824553, -1.232595164407830946E-29, 4.000000000000007105 ) ) ;
#46813 = ORIENTED_EDGE ( 'NONE', *, *, #84105, .F. ) ;
#46814 = CARTESIAN_POINT ( 'NONE',  ( 9.165151389911679658, 105.0000000000000000, 4.000000000000001776 ) ) ;
#46815 = ORIENTED_EDGE ( 'NONE', *, *, #56668, .F. ) ;
#46816 = LINE ( 'NONE', #38741, #31125 ) ;
#46817 = CARTESIAN_POINT ( 'NONE',  ( 101.1066808782305060, -38.45692254263880727, 200.1018791781253015 ) ) ;
#46818 = CARTESIAN_POINT ( 'NONE',  ( 10.70754322050349394, 12.38955932816331540, 10.00023628198462688 ) ) ;
#46819 = CARTESIAN_POINT ( 'NONE',  ( 84.49332496811159388, -45.28622975171930420, -7.233042096027321399 ) ) ;
#46820 = CARTESIAN_POINT ( 'NONE',  ( 81.87243278912710309, -37.99999999999996447, 157.2857030484634606 ) ) ;
#46821 = CARTESIAN_POINT ( 'NONE',  ( 39.47876275252662737, 315.8379454371342945, 7.014882839542285531 ) ) ;
#46822 = CARTESIAN_POINT ( 'NONE',  ( -43.43869229197126458, 464.9661605157749023, 13.42065392471464058 ) ) ;
#46823 = CARTESIAN_POINT ( 'NONE',  ( 0.000000000000000000, 0.000000000000000000, 0.000000000000000000 ) ) ;
#46824 = PRESENTATION_LAYER_ASSIGNMENT (  '', '', ( #79548 ) ) ;
#46825 = CARTESIAN_POINT ( 'NONE',  ( 2.103760375497109703, -0.1490785164325224010, 102.1576431125493940 ) ) ;
#46826 = ORIENTED_EDGE ( 'NONE', *, *, #4809, .F. ) ;
#46827 = CARTESIAN_POINT ( 'NONE',  ( 4.898587196589412829E-16, -10.81250000409677092, -8.000000000000000000 ) ) ;
#46828 = LINE ( 'NONE', #55955, #66780 ) ;
#46829 = CARTESIAN_POINT ( 'NONE',  ( 4.250000000000000000, 0.000000000000000000, -10.00000000000000000 ) ) ;
#46830 = ORIENTED_EDGE ( 'NONE', *, *, #50537, .T. ) ;
#46831 = DIRECTION ( 'NONE',  ( -1.000000000000000000, -0.000000000000000000, -0.000000000000000000 ) ) ;
#46832 = CARTESIAN_POINT ( 'NONE',  ( -26.54090941152919214, 306.2719066919671036, 10.71778513407069688 ) ) ;
#46833 = DIRECTION ( 'NONE',  ( -1.000000000000000000, -1.224606353822377258E-16, -0.000000000000000000 ) ) ;
#46834 = CARTESIAN_POINT ( 'NONE',  ( -13.87686815719945166, 43.16530573668475057, -91.42246037821334426 ) ) ;
#46835 = CARTESIAN_POINT ( 'NONE',  ( 8.000000000000000000, -16.99999999999999289, 0.000000000000000000 ) ) ;
#46836 = CARTESIAN_POINT ( 'NONE',  ( -29.18624803973531456, -31.90962671462940747, 40.10543586240345348 ) ) ;
#46837 = ADVANCED_FACE ( 'NONE', ( #104096 ), #50806, .F. ) ;
#46838 = COLOUR_RGB ( '', 0.31764706, 0.68627451, 0.89019608) ;
#46839 = CARTESIAN_POINT ( 'NONE',  ( -5.290067270632269114, 51.34639538792298907, -8.531152949374520844 ) ) ;
#46840 = ORIENTED_EDGE ( 'NONE', *, *, #64345, .T. ) ;
#46841 = CARTESIAN_POINT ( 'NONE',  ( 84.26380273736219806, -50.17260406813100104, 187.6069518689174345 ) ) ;
#46842 = CARTESIAN_POINT ( 'NONE',  ( -48.69302399950120019, 8.421789753111537991, 16.66702170536941807 ) ) ;
#46843 = DIRECTION ( 'NONE',  ( -1.000000000000000000, -1.224606353822377258E-16, -0.000000000000000000 ) ) ;
#46844 = ORIENTED_EDGE ( 'NONE', *, *, #9730, .F. ) ;
#46845 = CARTESIAN_POINT ( 'NONE',  ( 93.83727737954620807, -57.67472858147435488, 11.15358949908543984 ) ) ;
#46846 = CARTESIAN_POINT ( 'NONE',  ( 35.46984665180495711, 438.0686027085627074, 4.109636340053284265 ) ) ;
#46847 = CARTESIAN_POINT ( 'NONE',  ( -30.29857313018930043, 7.759641293511166715, 41.94607130693947994 ) ) ;
#46848 = CARTESIAN_POINT ( 'NONE',  ( 5.947762761376472973, 2.501851166488370914, -6.500000000000000000 ) ) ;
#46849 = EDGE_CURVE ( 'NONE', #84646, #82792, #105169, .T. ) ;
#46850 = ORIENTED_EDGE ( 'NONE', *, *, #92660, .F. ) ;
#46851 = PRESENTATION_LAYER_ASSIGNMENT (  '', '', ( #93377 ) ) ;
#46852 = CIRCLE ( 'NONE', #48543, 3.309500000000001663 ) ;
#46853 = CARTESIAN_POINT ( 'NONE',  ( 15.13815838105152167, -22.76677273537127988, 35.95324695099370871 ) ) ;
#46854 = CARTESIAN_POINT ( 'NONE',  ( 0.000000000000000000, 0.000000000000000000, 5.000000000000002665 ) ) ;
#46856 = FILL_AREA_STYLE ('',( #104025 ) ) ;
#46855 = CARTESIAN_POINT ( 'NONE',  ( 1.211595439868047741, -7.960739084487659767, -0.4504974108212048689 ) ) ;
#46857 = EDGE_CURVE ( 'NONE', #61442, #82593, #90836, .T. ) ;
#46858 = STYLED_ITEM ( 'NONE', ( #92503 ), #104728 ) ;
#46859 = CARTESIAN_POINT ( 'NONE',  ( 9.407137736676965289, 302.6622268192648448, -10.04029227552669568 ) ) ;
#46860 = CARTESIAN_POINT ( 'NONE',  ( 40.61216075948964033, 351.1469683695276558, 22.89433108575548914 ) ) ;
#46861 = CARTESIAN_POINT ( 'NONE',  ( -48.11205635439868900, -35.42149170368610811, -28.26377718570788744 ) ) ;
#46862 = CARTESIAN_POINT ( 'NONE',  ( 0.000000000000000000, 0.000000000000000000, -6.800000000000000711 ) ) ;
#46863 = ADVANCED_FACE ( 'NONE', ( #87412 ), #100004, .F. ) ;
#46864 = CYLINDRICAL_SURFACE ( 'NONE', #27915, 15.00000000000001421 ) ;
#46865 = ORIENTED_EDGE ( 'NONE', *, *, #72650, .F. ) ;
#46866 = CARTESIAN_POINT ( 'NONE',  ( -7.819539746246620737, -0.1116068871675765933, 19.30361860283825948 ) ) ;
#46867 = CYLINDRICAL_SURFACE ( 'NONE', #72746, 66.50000000000000000 ) ;
#46868 = CARTESIAN_POINT ( 'NONE',  ( 4.815811321232738251, -63.19923292302625839, 3.581116321197038932 ) ) ;
#46869 = CARTESIAN_POINT ( 'NONE',  ( -25.59063492799110762, -47.40907061882889195, -33.48575065794680938 ) ) ;
#46870 = ORIENTED_EDGE ( 'NONE', *, *, #65308, .T. ) ;
#46871 = CARTESIAN_POINT ( 'NONE',  ( 1.013163106017262338, 8.075304045852325530, -7.231838333420562037 ) ) ;
#46872 = ORIENTED_EDGE ( 'NONE', *, *, #34064, .T. ) ;
#46873 = DIRECTION ( 'NONE',  ( 1.224646799147349509E-16, 0.000000000000000000, -1.000000000000000000 ) ) ;
#46874 = DIRECTION ( 'NONE',  ( -1.000000000000000000, -1.224606353822377258E-16, -0.000000000000000000 ) ) ;
#46875 = CARTESIAN_POINT ( 'NONE',  ( -92.66121602952624414, -59.99999999999999289, -3.920577165534929964 ) ) ;
#46876 = ORIENTED_EDGE ( 'NONE', *, *, #18511, .T. ) ;
#46877 = DIRECTION ( 'NONE',  ( -1.000000000000000000, 0.000000000000000000, 0.000000000000000000 ) ) ;
#46878 = CARTESIAN_POINT ( 'NONE',  ( -9.482945380845299255, 27.55666941221070232, 3.177595346755240691 ) ) ;
#46880 = DIRECTION ( 'NONE',  ( -0.000000000000000000, -1.000000000000000000, -0.000000000000000000 ) ) ;
#46879 = CARTESIAN_POINT ( 'NONE',  ( 20.00000000000000711, 4.000000000000000888, 25.00000000000000000 ) ) ;
#46881 = CARTESIAN_POINT ( 'NONE',  ( -80.86179060450608347, -46.44313512650642650, 160.9680050460582663 ) ) ;
#46882 = EDGE_LOOP ( 'NONE', ( #15202, #6150, #16091, #50365 ) ) ;
#46883 = DIRECTION ( 'NONE',  ( -0.000000000000000000, -0.000000000000000000, -1.000000000000000000 ) ) ;
#46884 = AXIS2_PLACEMENT_3D ( 'NONE', #61058, #37870, #45929 ) ;
#46885 = ORIENTED_EDGE ( 'NONE', *, *, #25787, .F. ) ;
#46886 = CONICAL_SURFACE ( 'NONE', #105421, 4.171999999999999709, 0.7853981633974603804 ) ;
#46887 = ORIENTED_EDGE ( 'NONE', *, *, #48393, .F. ) ;
#46888 = CARTESIAN_POINT ( 'NONE',  ( 43.71037717921923615, 462.3391554988761527, 4.824299547763561513 ) ) ;
#46889 = CARTESIAN_POINT ( 'NONE',  ( -5.477443569834177239, -66.44117541007194916, 14.11469643991719813 ) ) ;
#46890 = DIRECTION ( 'NONE',  ( 0.000000000000000000, 0.000000000000000000, 1.000000000000000000 ) ) ;
#46891 = ORIENTED_EDGE ( 'NONE', *, *, #70206, .T. ) ;
#46892 = CARTESIAN_POINT ( 'NONE',  ( -34.92245169924841974, 464.4743357356041429, 18.75701277737645611 ) ) ;
#46893 = CARTESIAN_POINT ( 'NONE',  ( 0.000000000000000000, 6.123233995736770227E-16, -5.000000000000002665 ) ) ;
#46894 = CARTESIAN_POINT ( 'NONE',  ( -79.30961931381874308, -57.50609382800362823, 198.1725500959836666 ) ) ;
#46895 = CARTESIAN_POINT ( 'NONE',  ( 0.000000000000000000, 3.004629197474323585E-15, 8.000000000000000000 ) ) ;
#46896 = DIRECTION ( 'NONE',  ( -1.000000000000000000, 0.000000000000000000, 0.000000000000000000 ) ) ;
#46897 = CARTESIAN_POINT ( 'NONE',  ( 0.000000000000000000, 0.000000000000000000, 0.000000000000000000 ) ) ;
#46898 = CARTESIAN_POINT ( 'NONE',  ( 0.6420442155082901614, 27.35818369227503766, -40.57569272667392823 ) ) ;
#46899 = AXIS2_PLACEMENT_3D ( 'NONE', #86102, #12172, #62348 ) ;
#46900 = CARTESIAN_POINT ( 'NONE',  ( 94.98342851799053221, -59.99999999999993605, -11.07591208537989580 ) ) ;
#46901 = EDGE_CURVE ( 'NONE', #58211, #25469, #47972, .T. ) ;
#46902 = CARTESIAN_POINT ( 'NONE',  ( -45.38252603333997826, -14.21045842199430354, 49.92404905378138125 ) ) ;
#46903 = EDGE_CURVE ( 'NONE', #43420, #9728, #53510, .T. ) ;
#46904 = CARTESIAN_POINT ( 'NONE',  ( -55.54604552563809250, -42.97054307439768905, 62.92721107680804238 ) ) ;
#46905 = ORIENTED_EDGE ( 'NONE', *, *, #6813, .F. ) ;
#46906 =( NAMED_UNIT ( * ) PLANE_ANGLE_UNIT ( ) SI_UNIT ( $, .RADIAN. ) );
#46907 = ORIENTED_EDGE ( 'NONE', *, *, #16840, .T. ) ;
#46908 = CARTESIAN_POINT ( 'NONE',  ( -100.0299451350468161, -37.81394507940942162, 190.5172735492119216 ) ) ;
#46909 = CARTESIAN_POINT ( 'NONE',  ( 4.651477914329386962E-14, 52.17923068443710832, 7.749999999999496403 ) ) ;
#46910 = ORIENTED_EDGE ( 'NONE', *, *, #47748, .T. ) ;
#46911 = DIRECTION ( 'NONE',  ( 0.000000000000000000, 1.000000000000000000, 0.000000000000000000 ) ) ;
#46912 = B_SPLINE_CURVE_WITH_KNOTS ( 'NONE', 3,
 ( #5316, #5828, #46304, #79193, #103989, #30135 ),
 .UNSPECIFIED., .F., .F.,
 ( 4, 2, 4 ),
 ( 0.000000000000000000, 0.0004189869898914146498, 0.0008379739797828311427 ),
 .UNSPECIFIED. ) ;
#46913 = CARTESIAN_POINT ( 'NONE',  ( 110.5955579697139939, -38.35611409724038623, 181.9650721577582715 ) ) ;
#46914 = CARTESIAN_POINT ( 'NONE',  ( -9.797174393178825657E-16, -3.000000000000000000, 8.000000000000000000 ) ) ;
#46916 = EDGE_CURVE ( 'NONE', #73615, #65096, #89617, .T. ) ;
#46915 = FACE_OUTER_BOUND ( 'NONE', #9195, .T. ) ;
#46917 = CARTESIAN_POINT ( 'NONE',  ( 11.84999999999999787, 1.533819458162526451E-15, 0.000000000000000000 ) ) ;
#46918 = CARTESIAN_POINT ( 'NONE',  ( -39.13885763974980136, 324.4948203046521371, 17.18769520460729439 ) ) ;
#46919 = CIRCLE ( 'NONE', #55522, 4.250000000000000000 ) ;
#46920 = CARTESIAN_POINT ( 'NONE',  ( 0.5805565836007617886, -3.752776749732566142, 6.499999999999999112 ) ) ;
#46921 = CARTESIAN_POINT ( 'NONE',  ( 44.00534824917844645, 485.4287573672961003, 6.291782489092178743 ) ) ;
#46922 = DIRECTION ( 'NONE',  ( -0.5735764363510510444, -0.8191520442889883569, 0.000000000000000000 ) ) ;
#46923 = UNCERTAINTY_MEASURE_WITH_UNIT (LENGTH_MEASURE( 1.000000000000000082E-05 ), #70827, 'distance_accuracy_value', 'NONE');
#46924 = ORIENTED_EDGE ( 'NONE', *, *, #99371, .F. ) ;
#46925 = VERTEX_POINT ( 'NONE', #13486 ) ;
#46926 = CARTESIAN_POINT ( 'NONE',  ( 49.42319345579174694, -49.90093656948970846, 53.22847127201153938 ) ) ;
#46927 = AXIS2_PLACEMENT_3D ( 'NONE', #81659, #73575, #82204 ) ;
#46928 = CARTESIAN_POINT ( 'NONE',  ( -1.168375522601847960, 9.594968509503763343, 50.96085163187699152 ) ) ;
#46929 = CARTESIAN_POINT ( 'NONE',  ( -6.704772934685586883, 16.45971469038980217, 2.024104295774003415 ) ) ;
#46930 = CARTESIAN_POINT ( 'NONE',  ( -109.2921535902703596, -38.35623054118988762, 189.1334433219931270 ) ) ;
#46931 = ORIENTED_EDGE ( 'NONE', *, *, #36911, .T. ) ;
#46932 = CARTESIAN_POINT ( 'NONE',  ( 89.49617078063555198, -38.38859236215838422, -17.12117333382422402 ) ) ;
#46933 = CARTESIAN_POINT ( 'NONE',  ( 12.15278015503357523, 17.47224881724134349, -8.961376170971080413 ) ) ;
#46934 = CARTESIAN_POINT ( 'NONE',  ( 0.000000000000000000, 0.000000000000000000, -13.00000000000000000 ) ) ;
#46935 = FILL_AREA_STYLE ('',( #85843 ) ) ;
#46936 = CARTESIAN_POINT ( 'NONE',  ( -32.10320572247816528, 439.3861412500730808, 23.61825846262832584 ) ) ;
#46937 = CARTESIAN_POINT ( 'NONE',  ( -31.53901790643017478, 437.3649809074569816, 21.86268250587596995 ) ) ;
#46938 = CARTESIAN_POINT ( 'NONE',  ( 21.51569398614863715, 294.9107018935607130, -9.987480606144508499 ) ) ;
#46939 = CARTESIAN_POINT ( 'NONE',  ( -31.63473512700289092, 436.4561590364504013, 18.86554224087425879 ) ) ;
#46941 = AXIS2_PLACEMENT_3D ( 'NONE', #61715, #21264, #103733 ) ;
#46940 =( LENGTH_UNIT ( ) NAMED_UNIT ( * ) SI_UNIT ( .MILLI., .METRE. ) );
#46942 = CARTESIAN_POINT ( 'NONE',  ( 99.41552838720369323, -60.00000000000000711, 202.0437798234699471 ) ) ;
#46943 = CARTESIAN_POINT ( 'NONE',  ( -16.66900757617721140, 35.00972275561253610, 21.80698433968611383 ) ) ;
#46944 = ORIENTED_EDGE ( 'NONE', *, *, #73074, .T. ) ;
#46945 = CARTESIAN_POINT ( 'NONE',  ( 59.32604057062135183, -18.65621327707388488, 61.11290863963116493 ) ) ;
#46946 = CARTESIAN_POINT ( 'NONE',  ( -35.61732482767578034, 303.3743595346010125, -0.04560823654630981328 ) ) ;
#46947 = CARTESIAN_POINT ( 'NONE',  ( 7.801777176595948937, 33.58827985812632733, -1.786991866639921822 ) ) ;
#46948 =( LENGTH_UNIT ( ) NAMED_UNIT ( * ) SI_UNIT ( .MILLI., .METRE. ) );
#46949 = ORIENTED_EDGE ( 'NONE', *, *, #88378, .T. ) ;
#46951 = CARTESIAN_POINT ( 'NONE',  ( -9.300615953693611715, -52.70239146822830634, 23.32435243128603730 ) ) ;
#46950 = CARTESIAN_POINT ( 'NONE',  ( -92.04013207032886612, -38.35472338211468468, 35.72301976503869270 ) ) ;
#46952 = CARTESIAN_POINT ( 'NONE',  ( -20.34579289372443966, 303.8361034413807147, -9.003336996645776580 ) ) ;
#46953 = DIRECTION ( 'NONE',  ( 0.000000000000000000, -1.000000000000000000, 0.000000000000000000 ) ) ;
#46954 = DIRECTION ( 'NONE',  ( -0.5735764363510497121, 0.8191520442889892450, 1.003171929053521665E-16 ) ) ;
#46955 = CARTESIAN_POINT ( 'NONE',  ( 4.898587196589412829E-16, -30.12499999999999645, -8.000000000000000000 ) ) ;
#46956 = CARTESIAN_POINT ( 'NONE',  ( 8.737863884125493641, -3.000000000000002665, -79.96381019769830800 ) ) ;
#46957 = EDGE_CURVE ( 'NONE', #59097, #18574, #60388, .T. ) ;
#46958 = CARTESIAN_POINT ( 'NONE',  ( 29.68315524076926692, 13.47185074185900255, -42.10535821593530414 ) ) ;
#46959 = AXIS2_PLACEMENT_3D ( 'NONE', #74360, #23192, #6974 ) ;
#46960 = ORIENTED_EDGE ( 'NONE', *, *, #60902, .T. ) ;
#46961 = CARTESIAN_POINT ( 'NONE',  ( 83.71331492665446206, -39.45954491553350607, 176.1762179413915703 ) ) ;
#46962 = CARTESIAN_POINT ( 'NONE',  ( -45.99999999998839684, 463.0730145254914873, 8.174293518655169066 ) ) ;
#46963 = CARTESIAN_POINT ( 'NONE',  ( -36.60412653376215530, 439.8086773859736809, 24.20897003097096345 ) ) ;
#46964 = ORIENTED_EDGE ( 'NONE', *, *, #40254, .T. ) ;
#46965 = PRESENTATION_LAYER_ASSIGNMENT (  '', '', ( #43583 ) ) ;
#46966 = CARTESIAN_POINT ( 'NONE',  ( -37.71162116919980178, 389.8276394972959338, 6.083134903602375410 ) ) ;
#46967 = CARTESIAN_POINT ( 'NONE',  ( 7.597212443344973032, -5.000000000004688694, -19.53267873632396956 ) ) ;
#46968 = DIRECTION ( 'NONE',  ( 0.000000000000000000, 1.000000000000000000, 0.000000000000000000 ) ) ;
#46969 = CARTESIAN_POINT ( 'NONE',  ( -11.69538631874992340, 50.00000000000001421, -81.87730495799611674 ) ) ;
#46970 = PRESENTATION_STYLE_ASSIGNMENT (( #96073 ) ) ;
#46971 = AXIS2_PLACEMENT_3D ( 'NONE', #73246, #91070, #73790 ) ;
#46972 = FILL_AREA_STYLE ('',( #22205 ) ) ;
#46973 = EDGE_CURVE ( 'NONE', #45028, #103023, #61292, .T. ) ;
#46974 = VERTEX_POINT ( 'NONE', #455 ) ;
#46975 =( NAMED_UNIT ( * ) SI_UNIT ( $, .STERADIAN. ) SOLID_ANGLE_UNIT ( ) );
#46977 = CARTESIAN_POINT ( 'NONE',  ( -80.94296027622181100, -29.99999999999999289, 19.76001105705952909 ) ) ;
#46976 = CIRCLE ( 'NONE', #86593, 4.000000000000000888 ) ;
#46978 = CARTESIAN_POINT ( 'NONE',  ( -5.000000000000000888, -15.67301612170649072, -10.31008658364125985 ) ) ;
#46979 = LINE ( 'NONE', #71777, #90703 ) ;
#46981 = CARTESIAN_POINT ( 'NONE',  ( -13.39439044838818837, 7.828241060370396021, -8.562929616685366341 ) ) ;
#46980 = CARTESIAN_POINT ( 'NONE',  ( -3.672464763049774796E-06, -18.02989419364509516, 35.00496915990722613 ) ) ;
#46982 = CARTESIAN_POINT ( 'NONE',  ( -7.188101187500001821, -21.50000000204839168, -2.977408999572651371 ) ) ;
#46983 = CARTESIAN_POINT ( 'NONE',  ( 20.35953037385061037, 294.7626276629184758, -10.01895475554768566 ) ) ;
#46984 = CARTESIAN_POINT ( 'NONE',  ( -6.784953749642196996, 41.67963440881483450, -59.00226708758491156 ) ) ;
#46985 = EDGE_CURVE ( 'NONE', #10770, #17481, #26551, .T. ) ;
#46986 = EDGE_CURVE ( 'NONE', #93494, #7084, #98225, .T. ) ;
#46987 = VERTEX_POINT ( 'NONE', #40965 ) ;
#46988 = FACE_OUTER_BOUND ( 'NONE', #44855, .T. ) ;
#46989 = CARTESIAN_POINT ( 'NONE',  ( -4.267972493540475476, 11.49087057789210853, -5.000000000000000888 ) ) ;
#46990 = AXIS2_PLACEMENT_3D ( 'NONE', #90866, #74654, #50909 ) ;
#46991 = EDGE_CURVE ( 'NONE', #94742, #48471, #69004, .T. ) ;
#46992 = LINE ( 'NONE', #6001, #58702 ) ;
#46993 = ORIENTED_EDGE ( 'NONE', *, *, #39029, .F. ) ;
#46994 = DIRECTION ( 'NONE',  ( -0.000000000000000000, -0.000000000000000000, 1.000000000000000000 ) ) ;
#46995 = MECHANICAL_DESIGN_GEOMETRIC_PRESENTATION_REPRESENTATION (  '', ( #22871 ), #105519 ) ;
#46996 = ORIENTED_EDGE ( 'NONE', *, *, #33260, .T. ) ;
#46997 = CARTESIAN_POINT ( 'NONE',  ( -28.31912909058650385, 34.17181180593427570, 9.116382818698859580 ) ) ;
#46998 = CARTESIAN_POINT ( 'NONE',  ( -1.909182100399626325, -0.1358350450587593183, 102.2488568920600045 ) ) ;
#46999 = CARTESIAN_POINT ( 'NONE',  ( -43.29564266603537703, 39.41494058703111847, -48.56300739893791985 ) ) ;
#47000 = CARTESIAN_POINT ( 'NONE',  ( 6.449780583204264062, 2.701143306766772945, -6.840188146835520122 ) ) ;
#47001 = UNCERTAINTY_MEASURE_WITH_UNIT (LENGTH_MEASURE( 1.000000000000000082E-05 ), #63844, 'distance_accuracy_value', 'NONE');
#47002 = CARTESIAN_POINT ( 'NONE',  ( -112.1929976763688188, -60.00000000000002132, 169.7340247815773182 ) ) ;
#47003 = FILL_AREA_STYLE_COLOUR ( '', #103108 ) ;
#47004 = CARTESIAN_POINT ( 'NONE',  ( 30.35537264529554946, 338.7115663565144246, 18.05293407820170515 ) ) ;
#47005 = CARTESIAN_POINT ( 'NONE',  ( 6.367454298303730553, 53.78323910253516971, -6.627674447275911263 ) ) ;
#47006 = CARTESIAN_POINT ( 'NONE',  ( 17.73901682283262105, 34.63608873438791846, -22.27400293357690586 ) ) ;
#47007 = CARTESIAN_POINT ( 'NONE',  ( -83.95400002616862878, -35.96245533400819738, 173.2978818052737893 ) ) ;
#47008 = ORIENTED_EDGE ( 'NONE', *, *, #52102, .F. ) ;
#47009 = CARTESIAN_POINT ( 'NONE',  ( 44.27062040774965368, 41.35340516790330412, -49.63795927564910926 ) ) ;
#47010 =( BOUNDED_SURFACE ( )  B_SPLINE_SURFACE ( 3, 2, ( 
 ( #23468, #57910, #83259 ),
 ( #97849, #57379, #41210 ),
 ( #90293, #16402, #74096 ),
 ( #75156, #16950, #40147 ),
 ( #56851, #97316, #41739 ),
 ( #74626, #49828, #81643 ),
 ( #89244, #25605, #49285 ),
 ( #73025, #82188, #15342 ) ),
 .UNSPECIFIED., .F., .F., .F. ) 
 B_SPLINE_SURFACE_WITH_KNOTS ( ( 4, 2, 2, 4 ),
 ( 3, 3 ),
 ( 0.03861844051980971304, 0.04325213341840643266, 0.04556897986770479247, 0.04788582631700314535 ),
 ( 0.000000000000000000, 1.000000000000000000 ),
 .UNSPECIFIED. ) 
 GEOMETRIC_REPRESENTATION_ITEM ( )  RATIONAL_B_SPLINE_SURFACE ( (
 ( 1.000000000000000000, 0.8047781759831919013, 1.000000000000000000),
 ( 1.000000000000000000, 0.8123762462805835805, 1.000000000000000000),
 ( 1.000000000000000000, 0.8190659850615710225, 1.000000000000000000),
 ( 1.000000000000000000, 0.8191937571014150654, 1.000000000000000000),
 ( 1.000000000000000000, 0.8176092952781637280, 1.000000000000000000),
 ( 1.000000000000000000, 0.8122962088595298003, 1.000000000000000000),
 ( 1.000000000000000000, 0.8086311330828849231, 1.000000000000000000),
 ( 1.000000000000000000, 0.8047712282214323221, 1.000000000000000000) ) ) 
 REPRESENTATION_ITEM ( '' )  SURFACE ( )  );
#47011 = ORIENTED_EDGE ( 'NONE', *, *, #43514, .T. ) ;
#47012 = SURFACE_STYLE_FILL_AREA ( #29294 ) ;
#47013 = CARTESIAN_POINT ( 'NONE',  ( 4.696906829037970077, -66.43998147487890549, -3.734050370377312245 ) ) ;
#47014 = CARTESIAN_POINT ( 'NONE',  ( -84.89766952350503004, -52.70258195973874393, 12.33435398003158667 ) ) ;
#47015 = CARTESIAN_POINT ( 'NONE',  ( -13.49999999999999645, 0.000000000000000000, -13.00000000000000000 ) ) ;
#47016 = CARTESIAN_POINT ( 'NONE',  ( 3.646260779472994429, 22.19498946286545760, -5.000000000000000000 ) ) ;
#47017 = CARTESIAN_POINT ( 'NONE',  ( 25.21823338009918203, 1.482358050883964840E-15, 0.000000000000000000 ) ) ;
#47018 = DIRECTION ( 'NONE',  ( 0.000000000000000000, -1.000000000000000000, 0.000000000000000000 ) ) ;
#47019 = CARTESIAN_POINT ( 'NONE',  ( 99.17368802223589341, -30.00000000000007816, 199.4946398670649046 ) ) ;
#47020 = CARTESIAN_POINT ( 'NONE',  ( -94.42208465491292202, -30.00000000000002132, 63.29659460224121403 ) ) ;
#47021 = CARTESIAN_POINT ( 'NONE',  ( -63.03672031330412295, -49.91572035676450980, 85.83718877777337752 ) ) ;
#47022 = ORIENTED_EDGE ( 'NONE', *, *, #14085, .F. ) ;
#47023 = CARTESIAN_POINT ( 'NONE',  ( -51.64426891978533973, 39.42569251748471260, 39.58139286548590263 ) ) ;
#47024 = CARTESIAN_POINT ( 'NONE',  ( 84.45168914632041890, -60.00000000002949463, 202.6255676462649831 ) ) ;
#47025 = VERTEX_POINT ( 'NONE', #83018 ) ;
#47026 = CARTESIAN_POINT ( 'NONE',  ( 1.020029634130620755, -56.87793866973930079, 33.36930640455891961 ) ) ;
#47027 = CARTESIAN_POINT ( 'NONE',  ( 2.977408999572650927, -20.75000000204839523, -7.188101187500000933 ) ) ;
#47028 = AXIS2_PLACEMENT_3D ( 'NONE', #7907, #89904, #40813 ) ;
#47029 = CARTESIAN_POINT ( 'NONE',  ( -4.567209634097053161, -9.064002139144887948, -3.891254717191801493 ) ) ;
#47030 = EDGE_LOOP ( 'NONE', ( #58164, #458, #46277, #49841 ) ) ;
#47031 = B_SPLINE_CURVE_WITH_KNOTS ( 'NONE', 3,
 ( #34344, #42932, #34871, #41326 ),
 .UNSPECIFIED., .F., .F.,
 ( 4, 4 ),
 ( 0.000000000000000000, 1.000000000000000000 ),
 .UNSPECIFIED. ) ;
#47032 = CYLINDRICAL_SURFACE ( 'NONE', #49250, 4.000000000000000000 ) ;
#47033 = VERTEX_POINT ( 'NONE', #74903 ) ;
#47034 = FACE_OUTER_BOUND ( 'NONE', #33930, .T. ) ;
#47035 = VECTOR ( 'NONE', #12095, 1000.000000000000000 ) ;
#47036 = CARTESIAN_POINT ( 'NONE',  ( 0.000000000000000000, 4.898587196589413815E-16, -4.000000000000000888 ) ) ;
#47037 = CARTESIAN_POINT ( 'NONE',  ( -112.2540373697807325, -60.00000000000002842, 172.5324719884098101 ) ) ;
#47038 = CARTESIAN_POINT ( 'NONE',  ( 16.10302234481864403, 5.501632350609516386, 4.770674012950428811 ) ) ;
#47039 = CARTESIAN_POINT ( 'NONE',  ( 5.082755093536325930, -28.34375000204838813, -5.082755093536325042 ) ) ;
#47040 = FACE_OUTER_BOUND ( 'NONE', #36101, .T. ) ;
#47041 = ADVANCED_FACE ( 'NONE', ( #58204 ), #20926, .T. ) ;
#47042 = DIRECTION ( 'NONE',  ( -1.000000000000000000, -0.000000000000000000, -0.000000000000000000 ) ) ;
#47043 = CARTESIAN_POINT ( 'NONE',  ( -2.617478844990583031, 48.00000000000000000, -75.26027323389584467 ) ) ;
#47044 = ADVANCED_FACE ( 'NONE', ( #73853 ), #56947, .T. ) ;
#47045 = CARTESIAN_POINT ( 'NONE',  ( 0.000000000000000000, 42.00000000000000000, -56.99999999999999289 ) ) ;
#47046 = DIRECTION ( 'NONE',  ( -0.000000000000000000, 1.000000000000000000, -0.000000000000000000 ) ) ;
#47047 = CARTESIAN_POINT ( 'NONE',  ( 43.47770857297122404, 484.8227827122696567, 4.253339224811428565 ) ) ;
#47048 = CARTESIAN_POINT ( 'NONE',  ( -35.24657627339123422, -49.89919647416704862, 37.46166166223662941 ) ) ;
#47049 = ORIENTED_EDGE ( 'NONE', *, *, #20378, .F. ) ;
#47050 = CARTESIAN_POINT ( 'NONE',  ( 34.03145487526279567, -49.89646066257007817, 36.80204845843336869 ) ) ;
#47051 = CARTESIAN_POINT ( 'NONE',  ( 2.910977163136224011, -8.673617379884035472E-16, 22.23822744035697241 ) ) ;
#47052 = ADVANCED_FACE ( 'NONE', ( #39909 ), #60463, .T. ) ;
#47053 = ORIENTED_EDGE ( 'NONE', *, *, #71644, .F. ) ;
#47054 = CARTESIAN_POINT ( 'NONE',  ( 33.72687874471721869, 464.0440927329411238, 18.49751758896739418 ) ) ;
#47055 = CARTESIAN_POINT ( 'NONE',  ( -67.72166853775303252, -38.33445515793012248, 124.3162426451314957 ) ) ;
#47056 = EDGE_LOOP ( 'NONE', ( #95753, #18531, #15369, #14454 ) ) ;
#47058 = CARTESIAN_POINT ( 'NONE',  ( 36.91281931599076671, 303.7809130842520631, -7.959270006439831846 ) ) ;
#47057 = CARTESIAN_POINT ( 'NONE',  ( 5.933868275853403595, -5.000000000000000000, -15.37667404185483910 ) ) ;
#47059 = CARTESIAN_POINT ( 'NONE',  ( 16.11359103326339337, 37.20915759416860169, 21.97891983235034274 ) ) ;
#47060 = CARTESIAN_POINT ( 'NONE',  ( -4.852941176470586093, 40.00000000000132871, -70.80672828634229177 ) ) ;
#47061 = CARTESIAN_POINT ( 'NONE',  ( -16.64348903516517098, -1.200000000000000030E-05, 6.657797401561654560 ) ) ;
#47062 = CARTESIAN_POINT ( 'NONE',  ( -48.15279758643657004, 14.66099993221198616, -16.85535821593460426 ) ) ;
#47063 = SURFACE_STYLE_USAGE ( .BOTH. , #63811 ) ;
#47064 = CARTESIAN_POINT ( 'NONE',  ( 98.00817729099017583, -60.00000000000000000, 68.97682032673503727 ) ) ;
#47065 = DIRECTION ( 'NONE',  ( -1.000000000000000000, 0.000000000000000000, 0.000000000000000000 ) ) ;
#47066 = AXIS2_PLACEMENT_3D ( 'NONE', #18761, #74289, #18216 ) ;
#47067 = VECTOR ( 'NONE', #60648, 1000.000000000000000 ) ;
#47068 = DIRECTION ( 'NONE',  ( 0.000000000000000000, 1.000000000000000000, 0.000000000000000000 ) ) ;
#47069 = CARTESIAN_POINT ( 'NONE',  ( -33.70225418956815133, 490.4053771886481172, 11.54106678942738462 ) ) ;
#47070 = EDGE_LOOP ( 'NONE', ( #40520, #19168, #80457, #73464 ) ) ;
#47071 = MECHANICAL_DESIGN_GEOMETRIC_PRESENTATION_REPRESENTATION (  '', ( #62657 ), #67803 ) ;
#47072 = MECHANICAL_DESIGN_GEOMETRIC_PRESENTATION_REPRESENTATION (  '', ( #33329 ), #43689 ) ;
#47073 = CARTESIAN_POINT ( 'NONE',  ( -89.74886674459079927, -29.99999999998750866, -11.85434269913620220 ) ) ;
#47074 = ORIENTED_EDGE ( 'NONE', *, *, #27017, .F. ) ;
#47075 = CARTESIAN_POINT ( 'NONE',  ( 1.262844703064978993E-15, -3.000000000000002665, -95.00000000000000000 ) ) ;
#47076 = CARTESIAN_POINT ( 'NONE',  ( -15.28599664425101246, 3.173649883756319401, 3.309198297971303049 ) ) ;
#47077 = CARTESIAN_POINT ( 'NONE',  ( 8.167402502815940935, 39.27965345049515378, 4.999999999998771649 ) ) ;
#47078 = CARTESIAN_POINT ( 'NONE',  ( 32.18152564816683991, 409.5707777767445918, 25.68904866590993308 ) ) ;
#47079 = AXIS2_PLACEMENT_3D ( 'NONE', #76533, #60389, #77616 ) ;
#47080 = CARTESIAN_POINT ( 'NONE',  ( -5.082755093536325042, -26.46875000204838813, -5.082755093536325930 ) ) ;
#47081 = CARTESIAN_POINT ( 'NONE',  ( -43.00000000000009237, 484.2804969086082565, -2.982821241663377254 ) ) ;
#47082 = CARTESIAN_POINT ( 'NONE',  ( 7.960204194457797252E-15, 79.50000000000000000, -65.00000000000000000 ) ) ;
#47083 = DIRECTION ( 'NONE',  ( -0.5735764363510497121, 0.8191520442889892450, 1.003171929053521665E-16 ) ) ;
#47084 = ORIENTED_EDGE ( 'NONE', *, *, #10560, .F. ) ;
#47085 = EDGE_CURVE ( 'NONE', #49001, #106068, #74377, .T. ) ;
#47086 = B_SPLINE_CURVE_WITH_KNOTS ( 'NONE', 1,
 ( #78851, #6020, #70774 ),
 .UNSPECIFIED., .F., .F.,
 ( 2, 1, 2 ),
 ( 0.07762659913847776150, 1.000000000000000000, 1.289432564806017645 ),
 .UNSPECIFIED. ) ;
#47088 = ORIENTED_EDGE ( 'NONE', *, *, #50693, .F. ) ;
#47087 = CARTESIAN_POINT ( 'NONE',  ( 4.571008445750555538, -2.193282516568173968, 102.5889671997070849 ) ) ;
#47089 = CARTESIAN_POINT ( 'NONE',  ( 77.77861324456983994, -39.49362688318783654, 133.3549205718891812 ) ) ;
#47090 = SURFACE_SIDE_STYLE ('',( #88105 ) ) ;
#47091 = ORIENTED_EDGE ( 'NONE', *, *, #44864, .F. ) ;
#47092 = CARTESIAN_POINT ( 'NONE',  ( -12.50000000000001066, 39.67068617188025570, -64.72045672135165262 ) ) ;
#47093 = CARTESIAN_POINT ( 'NONE',  ( -0.3599032852998504395, 13.03488328047065359, -51.69862933869767829 ) ) ;
#47094 = CARTESIAN_POINT ( 'NONE',  ( 7.188101187500000044, -11.65625000204838635, 0.000000000000000000 ) ) ;
#47095 = CARTESIAN_POINT ( 'NONE',  ( -35.27718283856832926, -57.69548877625971528, 49.41932622563938793 ) ) ;
#47096 = CARTESIAN_POINT ( 'NONE',  ( 6.289812543865805239, -6.246946743711091266, -2.837966828325885871 ) ) ;
#47097 = EDGE_CURVE ( 'NONE', #68407, #98268, #101782, .T. ) ;
#47098 = EDGE_LOOP ( 'NONE', ( #26410, #20996, #25617, #22563, #31533 ) ) ;
#47099 = FILL_AREA_STYLE ('',( #82119 ) ) ;
#47100 =( NAMED_UNIT ( * ) SI_UNIT ( $, .STERADIAN. ) SOLID_ANGLE_UNIT ( ) );
#47101 = CYLINDRICAL_SURFACE ( 'NONE', #37227, 2.000000000000001776 ) ;
#47102 = CARTESIAN_POINT ( 'NONE',  ( -9.842984802582135373, 81.40930409524348477, 1.781981959250507952 ) ) ;
#47103 = CARTESIAN_POINT ( 'NONE',  ( 10.59999999999999609, 3.309500000000003439, 0.000000000000000000 ) ) ;
#47104 = ORIENTED_EDGE ( 'NONE', *, *, #76115, .F. ) ;
#47105 = CARTESIAN_POINT ( 'NONE',  ( -8.000000000000000000, -9.031250004096769146, -3.313708498984762496 ) ) ;
#47106 = CARTESIAN_POINT ( 'NONE',  ( -19.64607334565684837, -16.95621533664098735, 31.48343634207214592 ) ) ;
#47107 = CARTESIAN_POINT ( 'NONE',  ( 9.090909090909084611, 14.99999999999999645, 4.165977904505316687 ) ) ;
#47108 = AXIS2_PLACEMENT_3D ( 'NONE', #11299, #93310, #44228 ) ;
#47109 = CARTESIAN_POINT ( 'NONE',  ( -1.000000000000000222, -43.18879712711532193, 0.3952393630180867090 ) ) ;
#47110 = ADVANCED_FACE ( 'NONE', ( #57131 ), #82487, .F. ) ;
#47111 = CARTESIAN_POINT ( 'NONE',  ( -9.165151389911684987, 85.26735155607116212, -4.000000000000000000 ) ) ;
#47112 =( NAMED_UNIT ( * ) SI_UNIT ( $, .STERADIAN. ) SOLID_ANGLE_UNIT ( ) );
#47113 = VECTOR ( 'NONE', #88816, 1000.000000000000000 ) ;
#47114 = SHAPE_DEFINITION_REPRESENTATION ( #20094, #22667 ) ;
#47115 = CARTESIAN_POINT ( 'NONE',  ( 38.80499884327841187, 27.34286220386137245, 12.01623411786279760 ) ) ;
#47116 = EDGE_LOOP ( 'NONE', ( #573, #81737, #37550, #15567, #82266 ) ) ;
#47117 = CARTESIAN_POINT ( 'NONE',  ( 14.83349330513380693, 1.593028355512270962E-15, 0.000000000000000000 ) ) ;
#47118 = DIRECTION ( 'NONE',  ( -1.000000000000000000, -1.224606353822377258E-16, -0.000000000000000000 ) ) ;
#47119 = COLOUR_RGB ( '', 0.40784314, 0.44705882, 0.49803922) ;
#47120 = CARTESIAN_POINT ( 'NONE',  ( 0.000000000000000000, 0.000000000000000000, 0.000000000000000000 ) ) ;
#47121 = CARTESIAN_POINT ( 'NONE',  ( -21.69933433976674308, -26.44462722771605101, -38.46517870091099667 ) ) ;
#47122 = CARTESIAN_POINT ( 'NONE',  ( -81.10745130575307371, -30.00000000000000355, 140.6132671042336142 ) ) ;
#47123 = EDGE_CURVE ( 'NONE', #92851, #74216, #86331, .T. ) ;
#47124 = DIRECTION ( 'NONE',  ( -0.000000000000000000, -0.000000000000000000, -1.000000000000000000 ) ) ;
#47125 = ORIENTED_EDGE ( 'NONE', *, *, #58949, .T. ) ;
#47126 = CARTESIAN_POINT ( 'NONE',  ( 29.83349330513380693, 4.000000000000003553, 0.000000000000000000 ) ) ;
#47127 = CARTESIAN_POINT ( 'NONE',  ( 96.51954077749346084, -57.62215758448405722, 204.4834013014043137 ) ) ;
#47128 = DIRECTION ( 'NONE',  ( -1.000000000000000000, -1.224606353822377258E-16, -0.000000000000000000 ) ) ;
#47129 = EDGE_CURVE ( 'NONE', #52930, #6711, #57656, .T. ) ;
#47130 = CARTESIAN_POINT ( 'NONE',  ( -9.165151389911681434, 84.99999999999998579, -4.000000000000000000 ) ) ;
#47131 = B_SPLINE_CURVE_WITH_KNOTS ( 'NONE', 3,
 ( #13560, #29796, #38924, #46478, #22759, #95562 ),
 .UNSPECIFIED., .F., .F.,
 ( 4, 2, 4 ),
 ( 0.000000000000000000, 0.0003491763592121711088, 0.0006983527184243422175 ),
 .UNSPECIFIED. ) ;
#47132 = CARTESIAN_POINT ( 'NONE',  ( -16.10370002540618373, 21.82456013744392109, 0.8668566224997985570 ) ) ;
#47133 = CARTESIAN_POINT ( 'NONE',  ( -6.490443738817557318, 53.67433831593452709, 6.923344696077945670 ) ) ;
#47134 = CARTESIAN_POINT ( 'NONE',  ( -73.02673009549289418, -60.00000000000000000, 162.7051491287812723 ) ) ;
#47135 = ADVANCED_FACE ( 'NONE', ( #25342, #91130, #65773 ), #17240, .F. ) ;
#47136 = CARTESIAN_POINT ( 'NONE',  ( -5.619193549420574918, 4.261310591078547816, -5.875704392895148231 ) ) ;
#47137 = CARTESIAN_POINT ( 'NONE',  ( 0.000000000000000000, 152.0000000000000000, -5.000000000000000000 ) ) ;
#47138 = CARTESIAN_POINT ( 'NONE',  ( 54.34415824577756382, 50.00000000000000000, -32.38913437803500983 ) ) ;
#47139 = CARTESIAN_POINT ( 'NONE',  ( -86.19855657701549490, -28.27924645610051613, 183.2269261606164434 ) ) ;
#47141 = ORIENTED_EDGE ( 'NONE', *, *, #21536, .F. ) ;
#47140 = STYLED_ITEM ( 'NONE', ( #104408 ), #17528 ) ;
#47142 = CARTESIAN_POINT ( 'NONE',  ( 35.49450300380783574, 379.3078207793571437, 5.749337263989718672 ) ) ;
#47143 = VECTOR ( 'NONE', #65669, 1000.000000000000000 ) ;
#47144 = CARTESIAN_POINT ( 'NONE',  ( 64.78349330513380266, 4.000000000000014211, 0.000000000000000000 ) ) ;
#47145 = CARTESIAN_POINT ( 'NONE',  ( -20.41854916970525835, 303.8436858046150633, -10.00172532726429075 ) ) ;
#47146 =( GEOMETRIC_REPRESENTATION_CONTEXT ( 3 ) GLOBAL_UNCERTAINTY_ASSIGNED_CONTEXT ( ( #7903 ) ) GLOBAL_UNIT_ASSIGNED_CONTEXT ( ( #56106, #72321, #73360 ) ) REPRESENTATION_CONTEXT ( 'NONE', 'WORKASPACE' ) );
#47147 = CIRCLE ( 'NONE', #612, 2.000000000000000000 ) ;
#47148 = CARTESIAN_POINT ( 'NONE',  ( 40.03968747356719149, 489.2277061813577461, 11.31325917480963028 ) ) ;
#47149 = CARTESIAN_POINT ( 'NONE',  ( 34.83349330513379982, 1.593028355512270567E-15, 0.000000000000000000 ) ) ;
#47150 = CARTESIAN_POINT ( 'NONE',  ( 44.21332904831284338, 435.2494715644500616, 14.45449769377396976 ) ) ;
#47151 = ORIENTED_EDGE ( 'NONE', *, *, #72357, .F. ) ;
#47152 = DIRECTION ( 'NONE',  ( -1.000000000000000000, -1.224606353822377258E-16, -0.000000000000000000 ) ) ;
#47153 = CARTESIAN_POINT ( 'NONE',  ( 10.55307219781806616, 17.81967380046186022, 9.596392936463645995 ) ) ;
#47154 = CARTESIAN_POINT ( 'NONE',  ( -19.43146043915540488, 9.659702761776270386E-13, -11.19959342721046980 ) ) ;
#47155 = DIRECTION ( 'NONE',  ( -1.000000000000000000, -0.000000000000000000, -0.000000000000000000 ) ) ;
#47156 = CARTESIAN_POINT ( 'NONE',  ( 86.58060678326373250, -14.21045842199439235, 15.94037124058900901 ) ) ;
#47157 = CARTESIAN_POINT ( 'NONE',  ( -81.07615537427551544, -22.15355340867505518, 134.4957932511888714 ) ) ;
#47158 = VERTEX_POINT ( 'NONE', #102387 ) ;
#47159 = CARTESIAN_POINT ( 'NONE',  ( 8.309829428344436053, -30.00000000000008527, 36.98670151680749996 ) ) ;
#47160 = CARTESIAN_POINT ( 'NONE',  ( 69.36244709154269117, -57.68278289274119430, 149.4242506819062442 ) ) ;
#47161 = CARTESIAN_POINT ( 'NONE',  ( 33.10170411573166405, 314.2231804304243497, -7.291332407212943956 ) ) ;
#47162 = CARTESIAN_POINT ( 'NONE',  ( 0.000000000000000000, 4.898587196589412829E-16, -4.000000000000000000 ) ) ;
#47163 = ORIENTED_EDGE ( 'NONE', *, *, #86147, .T. ) ;
#47164 = FACE_OUTER_BOUND ( 'NONE', #13359, .T. ) ;
#47165 = CARTESIAN_POINT ( 'NONE',  ( 31.35596682365711274, 438.0939828603570732, 22.55458131664589061 ) ) ;
#47167 = CARTESIAN_POINT ( 'NONE',  ( -102.4400663919250292, -45.26551116408855790, 149.2539637247840858 ) ) ;
#47166 = DIRECTION ( 'NONE',  ( -0.9861333108787084800, -0.1659550938519104846, 0.000000000000000000 ) ) ;
#47168 = CARTESIAN_POINT ( 'NONE',  ( 7.188101187499999156, -20.75000000204839523, 2.977408999572654924 ) ) ;
#47169 = DIRECTION ( 'NONE',  ( 0.000000000000000000, 0.000000000000000000, 1.000000000000000000 ) ) ;
#47170 = CARTESIAN_POINT ( 'NONE',  ( 6.075691126275640563, 41.99394904787047977, -68.91429206828460963 ) ) ;
#47171 = ADVANCED_FACE ( 'NONE', ( #1544 ), #44701, .T. ) ;
#47172 = CARTESIAN_POINT ( 'NONE',  ( -9.215718466126777828E-16, -7.124194613927628872, -3.660532965668816363 ) ) ;
#47173 = CARTESIAN_POINT ( 'NONE',  ( 27.10511071441176867, -1.200000000000000030E-05, -8.806984339686344754 ) ) ;
#47174 = AXIS2_PLACEMENT_3D ( 'NONE', #99970, #68697, #101036 ) ;
#47175 = ORIENTED_EDGE ( 'NONE', *, *, #81707, .F. ) ;
#47176 = DIRECTION ( 'NONE',  ( 0.000000000000000000, 0.000000000000000000, -1.000000000000000000 ) ) ;
#47178 = CARTESIAN_POINT ( 'NONE',  ( 26.74761531504731238, -25.57238952923795594, 29.74515757345933054 ) ) ;
#47177 = CARTESIAN_POINT ( 'NONE',  ( -4.090533018665307274, -14.21045842199441722, 34.36071901318091903 ) ) ;
#47179 = CARTESIAN_POINT ( 'NONE',  ( -4.881589094946162888, 52.15742855003398404, -6.096815929868464323 ) ) ;
#47180 = ADVANCED_FACE ( 'NONE', ( #84618 ), #9639, .F. ) ;
#47181 = ORIENTED_EDGE ( 'NONE', *, *, #100937, .T. ) ;
#47182 = UNCERTAINTY_MEASURE_WITH_UNIT (LENGTH_MEASURE( 1.000000000000000082E-05 ), #105026, 'distance_accuracy_value', 'NONE');
#47183 = ORIENTED_EDGE ( 'NONE', *, *, #49470, .T. ) ;
#47185 = CARTESIAN_POINT ( 'NONE',  ( -0.08419721950864400561, 43.17555810750859990, -18.75000000000000355 ) ) ;
#47184 = CARTESIAN_POINT ( 'NONE',  ( 1.040949779275250140E-15, -0.5000000000000000000, -8.500000000000000000 ) ) ;
#47186 = DIRECTION ( 'NONE',  ( 0.000000000000000000, -1.000000000000000000, 0.000000000000000000 ) ) ;
#47187 = CARTESIAN_POINT ( 'NONE',  ( 7.500000000000009770, 40.18760374782148403, -59.65697284672557998 ) ) ;
#47188 =( GEOMETRIC_REPRESENTATION_CONTEXT ( 3 ) GLOBAL_UNCERTAINTY_ASSIGNED_CONTEXT ( ( #55604 ) ) GLOBAL_UNIT_ASSIGNED_CONTEXT ( ( #29536, #39194, #80681 ) ) REPRESENTATION_CONTEXT ( 'NONE', 'WORKASPACE' ) );
#47189 = CARTESIAN_POINT ( 'NONE',  ( -4.651132217449170270, -5.000000000000000000, -15.66661053588738106 ) ) ;
#47190 = CARTESIAN_POINT ( 'NONE',  ( 37.06438722625302518, -5.000000000000000888, 6.123233995736769241E-16 ) ) ;
#47191 = DIRECTION ( 'NONE',  ( -1.000000000000000000, -0.000000000000000000, -0.000000000000000000 ) ) ;
#47192 = VERTEX_POINT ( 'NONE', #68440 ) ;
#47193 = CARTESIAN_POINT ( 'NONE',  ( 3.334507628320575900, -60.00000000000000711, -42.61916129529188879 ) ) ;
#47194 = CARTESIAN_POINT ( 'NONE',  ( 22.00857090122901027, 25.77073524871309829, -32.31114556117190517 ) ) ;
#47195 = CARTESIAN_POINT ( 'NONE',  ( -13.59375373143781651, 24.77294821207336639, -0.6337968656602750439 ) ) ;
#47196 = VECTOR ( 'NONE', #31147, 1000.000000000000000 ) ;
#47197 = CARTESIAN_POINT ( 'NONE',  ( -0.000000000000000000, 53.37899725327129374, -25.05398456423234066 ) ) ;
#47198 = DIRECTION ( 'NONE',  ( -0.000000000000000000, 0.000000000000000000, -1.000000000000000000 ) ) ;
#47199 = CARTESIAN_POINT ( 'NONE',  ( 9.250997389131581983, 5.000000000000004441, 6.123233995736770227E-16 ) ) ;
#47200 = ORIENTED_EDGE ( 'NONE', *, *, #45932, .T. ) ;
#47201 = EDGE_CURVE ( 'NONE', #68161, #93742, #3629, .T. ) ;
#47202 = EDGE_LOOP ( 'NONE', ( #39, #46840, #91367, #32969 ) ) ;
#47203 = ORIENTED_EDGE ( 'NONE', *, *, #36323, .F. ) ;
#47204 = DIRECTION ( 'NONE',  ( -0.000000000000000000, 1.000000000000000000, -0.000000000000000000 ) ) ;
#47205 = DIRECTION ( 'NONE',  ( 0.000000000000000000, 0.000000000000000000, 1.000000000000000000 ) ) ;
#47206 = DIRECTION ( 'NONE',  ( -1.000000000000000000, -0.000000000000000000, -0.000000000000000000 ) ) ;
#47207 = CARTESIAN_POINT ( 'NONE',  ( -8.000000000000000000, -16.43750000409677270, -9.797174393178825657E-16 ) ) ;
#47208 =( NAMED_UNIT ( * ) SI_UNIT ( $, .STERADIAN. ) SOLID_ANGLE_UNIT ( ) );
#47209 = CARTESIAN_POINT ( 'NONE',  ( -46.00000000000000000, 488.0504108836653359, 1.820875518055464770 ) ) ;
#47210 = CARTESIAN_POINT ( 'NONE',  ( 6.289572920342628493, -6.243622107253699482, 2.843693100100563420 ) ) ;
#47211 = ORIENTED_EDGE ( 'NONE', *, *, #98698, .T. ) ;
#47212 = CARTESIAN_POINT ( 'NONE',  ( 34.83349330513380693, 4.000000000000002665, 0.000000000000000000 ) ) ;
#47213 = ORIENTED_EDGE ( 'NONE', *, *, #80554, .T. ) ;
#47214 = EDGE_CURVE ( 'NONE', #106028, #26488, #103673, .T. ) ;
#47215 = DIRECTION ( 'NONE',  ( -1.000000000000000000, -1.224606353822377258E-16, -0.000000000000000000 ) ) ;
#47216 = CARTESIAN_POINT ( 'NONE',  ( -10.51296777078104050, 50.00000000000000000, -92.64705882352942012 ) ) ;
#47217 = CARTESIAN_POINT ( 'NONE',  ( -40.62309488084728315, 485.6251729596530140, -4.313937499028603462 ) ) ;
#47218 = DIRECTION ( 'NONE',  ( 0.000000000000000000, -0.3420201433256727652, -0.9396926207859068736 ) ) ;
#47219 = CARTESIAN_POINT ( 'NONE',  ( 64.08887429804100577, -22.10312605409954756, 74.71187393261132570 ) ) ;
#47220 = CIRCLE ( 'NONE', #62793, 5.000000000000010658 ) ;
#47221 = ORIENTED_EDGE ( 'NONE', *, *, #85837, .F. ) ;
#47222 = DIRECTION ( 'NONE',  ( 0.000000000000000000, -1.000000000000000000, 0.000000000000000000 ) ) ;
#47223 = CARTESIAN_POINT ( 'NONE',  ( -38.88461863710598010, 437.7975295993174427, 4.475058894670826071 ) ) ;
#47224 = CIRCLE ( 'NONE', #50588, 4.000000000000001776 ) ;
#47225 = B_SPLINE_CURVE_WITH_KNOTS ( 'NONE', 3,
 ( #80096, #95245, #89269, #13765, #5168, #40174, #63422, #56337 ),
 .UNSPECIFIED., .F., .F.,
 ( 4, 2, 2, 4 ),
 ( 0.006061689441712474202, 0.007174127271521698983, 0.008286565101330923763, 0.01051144076094937159 ),
 .UNSPECIFIED. ) ;
#47226 = EDGE_CURVE ( 'NONE', #10730, #25883, #13917, .T. ) ;
#47227 = ADVANCED_FACE ( 'NONE', ( #94311 ), #84079, .T. ) ;
#47228 =( GEOMETRIC_REPRESENTATION_CONTEXT ( 3 ) GLOBAL_UNCERTAINTY_ASSIGNED_CONTEXT ( ( #42404 ) ) GLOBAL_UNIT_ASSIGNED_CONTEXT ( ( #38267, #90364, #57444 ) ) REPRESENTATION_CONTEXT ( 'NONE', 'WORKASPACE' ) );
#47230 = ORIENTED_EDGE ( 'NONE', *, *, #10147, .F. ) ;
#47229 = PRESENTATION_LAYER_ASSIGNMENT (  '', '', ( #33473 ) ) ;
#47231 = CARTESIAN_POINT ( 'NONE',  ( 48.02835407290545078, 16.78162100668605206, 14.35535821593427386 ) ) ;
#47232 = CARTESIAN_POINT ( 'NONE',  ( -7.105115778984035124, -60.00000000000002842, -36.77403448916896167 ) ) ;
#47233 = CARTESIAN_POINT ( 'NONE',  ( 40.34715123528543046, 6.123233995736770227E-16, -5.000000000000002665 ) ) ;
#47234 = B_SPLINE_CURVE_WITH_KNOTS ( 'NONE', 3,
 ( #67829, #19339, #20404, #86169, #53249, #18788, #19863, #43557, #11165, #44635, #93171, #27420, #51092, #101788, #51636, #44093, #84554, #26881, #76979, #59754, #60299, #84012, #85081, #60819, #68913, #93709, #10638, #76438, #43028, #75917, #3636, #36572, #69439, #2550 ),
 .UNSPECIFIED., .F., .F.,
 ( 4, 2, 2, 2, 2, 2, 2, 2, 2, 2, 2, 2, 2, 2, 2, 2, 4 ),
 ( 0.000000000000000000, 0.003935531903598469411, 0.007871063807196938822, 0.01180659571079540997, 0.01377436166259464988, 0.01574212761439389152, 0.02361319142159084422, 0.02754872332518931363, 0.03148425522878778998, 0.03935531903598470799, 0.04329085093958316699, 0.04722638284318161905, 0.05116191474678007112, 0.05509744665037853012, 0.05903297855397698218, 0.06100074450577621515, 0.06296851045757544119 ),
 .UNSPECIFIED. ) ;
#47235 = CARTESIAN_POINT ( 'NONE',  ( -1.469576158976823947E-15, -31.06250000409677270, 8.000000000000000000 ) ) ;
#47236 = CARTESIAN_POINT ( 'NONE',  ( 0.000000000000000000, -3.000000000000000000, 8.000000000000000000 ) ) ;
#47237 = CARTESIAN_POINT ( 'NONE',  ( 86.65396412451504204, -42.80459859885080220, 189.4102807469302832 ) ) ;
#47238 = SURFACE_SIDE_STYLE ('',( #88253 ) ) ;
#47239 = B_SPLINE_CURVE_WITH_KNOTS ( 'NONE', 3,
 ( #84868, #27199, #84336, #58468, #60089, #35281, #11488, #92955, #83788, #99978, #93505, #34220, #91375, #10432, #35825, #83265 ),
 .UNSPECIFIED., .F., .F.,
 ( 4, 2, 2, 1, 2, 2, 1, 2, 4 ),
 ( 0.000000000000000000, 0.2499999999999694134, 0.3749999999999552025, 0.3906249999999557576, 0.3984374999999557576, 0.4062499999999557576, 0.4374999999999586997, 0.4999999999999641398, 1.000000000000000000 ),
 .UNSPECIFIED. ) ;
#47240 = CARTESIAN_POINT ( 'NONE',  ( -9.838569038458777172, 7.857203345964940411, 0.000000000000000000 ) ) ;
#47241 = DIRECTION ( 'NONE',  ( -1.000000000000000000, -1.224606353822377258E-16, -0.000000000000000000 ) ) ;
#47242 = CARTESIAN_POINT ( 'NONE',  ( -4.165977904505308693, 15.00000000000000000, -9.090909090909091717 ) ) ;
#47243 = ORIENTED_EDGE ( 'NONE', *, *, #103079, .T. ) ;
#47244 = LINE ( 'NONE', #23541, #26489 ) ;
#47245 = CARTESIAN_POINT ( 'NONE',  ( -8.000000000000000000, -10.34374999999999112, -3.313708498984762496 ) ) ;
#47246 = CARTESIAN_POINT ( 'NONE',  ( 26.67261969005227940, -60.00000000000000000, 41.66386289415872568 ) ) ;
#47247 = CARTESIAN_POINT ( 'NONE',  ( -97.63767121502735336, -29.99999999999999645, 134.9972035148113605 ) ) ;
#47248 = ADVANCED_FACE ( 'NONE', ( #69500 ), #26077, .T. ) ;
#47249 = MECHANICAL_DESIGN_GEOMETRIC_PRESENTATION_REPRESENTATION (  '', ( #61063 ), #95453 ) ;
#47250 = CARTESIAN_POINT ( 'NONE',  ( -38.81358894280271699, 485.1131561813180042, -4.191378885296423995 ) ) ;
#47251 = CARTESIAN_POINT ( 'NONE',  ( 40.54584476168707852, -57.69097569962055161, 56.57753608882419627 ) ) ;
#47253 =( LENGTH_UNIT ( ) NAMED_UNIT ( * ) SI_UNIT ( .MILLI., .METRE. ) );
#47252 = CARTESIAN_POINT ( 'NONE',  ( 0.000000000000000000, 1.000000000000000888, -13.00000000000003730 ) ) ;
#47254 = EDGE_CURVE ( 'NONE', #21068, #55816, #82836, .T. ) ;
#47255 = CARTESIAN_POINT ( 'NONE',  ( -31.55411806780566408, 43.06427826655156110, -67.12025964001210809 ) ) ;
#47256 = CARTESIAN_POINT ( 'NONE',  ( -17.52057716778178786, 49.99999999999999289, 63.21064094274808554 ) ) ;
#47257 = CARTESIAN_POINT ( 'NONE',  ( -10.00000000000000000, 15.00000000000000000, 3.648665620917489250 ) ) ;
#47258 = CARTESIAN_POINT ( 'NONE',  ( -16.91076490362186036, -59.99999999999998579, 39.91562613777458068 ) ) ;
#47259 = VECTOR ( 'NONE', #12551, 1000.000000000000000 ) ;
#47260 = AXIS2_PLACEMENT_3D ( 'NONE', #51234, #27023, #68520 ) ;
#47261 = APPLICATION_CONTEXT ( 'automotive_design' ) ;
#47262 = FILL_AREA_STYLE_COLOUR ( '', #7203 ) ;
#47263 = AXIS2_PLACEMENT_3D ( 'NONE', #48105, #13619, #63264 ) ;
#47264 = CYLINDRICAL_SURFACE ( 'NONE', #48804, 5.000000000000000888 ) ;
#47265 = EDGE_CURVE ( 'NONE', #37712, #59582, #68979, .T. ) ;
#47266 = ORIENTED_EDGE ( 'NONE', *, *, #62385, .T. ) ;
#47267 = CARTESIAN_POINT ( 'NONE',  ( 41.18546553262711996, 436.5301601935307190, 21.34144970355281501 ) ) ;
#47268 = CARTESIAN_POINT ( 'NONE',  ( -13.17713355742532322, -18.58679757000995281, 27.05833942353407551 ) ) ;
#47270 = SURFACE_STYLE_FILL_AREA ( #87757 ) ;
#47269 = CARTESIAN_POINT ( 'NONE',  ( -86.94432264429229917, -59.99999999999998579, 29.30728585821892551 ) ) ;
#47271 = ORIENTED_EDGE ( 'NONE', *, *, #11747, .T. ) ;
#47272 = DIRECTION ( 'NONE',  ( 0.000000000000000000, -1.000000000000000000, 0.000000000000000000 ) ) ;
#47273 = PRESENTATION_STYLE_ASSIGNMENT (( #20947 ) ) ;
#47274 = CARTESIAN_POINT ( 'NONE',  ( 42.75202416080772139, 486.5826644063713502, 6.942705799351878149 ) ) ;
#47275 =( LENGTH_UNIT ( ) NAMED_UNIT ( * ) SI_UNIT ( .MILLI., .METRE. ) );
#47276 = CARTESIAN_POINT ( 'NONE',  ( 15.91255636217487712, 3.418437750269127218, -2.532291868533038226 ) ) ;
#47277 = CARTESIAN_POINT ( 'NONE',  ( 60.68637083643779562, -60.00000000000002132, 102.7753246229686113 ) ) ;
#47278 = CARTESIAN_POINT ( 'NONE',  ( -0.5681331142220417130, 54.25170640378875220, -7.883436127774885449 ) ) ;
#47279 = VERTEX_POINT ( 'NONE', #18856 ) ;
#47280 = CARTESIAN_POINT ( 'NONE',  ( -2.440247554416620890, -29.99999999999999289, 6.972723154969403758 ) ) ;
#47281 = CARTESIAN_POINT ( 'NONE',  ( -14.54015256618497176, 142.2617268803927573, 0.000000000000000000 ) ) ;
#47282 = B_SPLINE_CURVE_WITH_KNOTS ( 'NONE', 3,
 ( #6386, #5353, #64640, #97511 ),
 .UNSPECIFIED., .F., .F.,
 ( 4, 4 ),
 ( 3.469446951953614189E-18, 0.0002123325198249128231 ),
 .UNSPECIFIED. ) ;
#47284 = CYLINDRICAL_SURFACE ( 'NONE', #2920, 4.000000000000002665 ) ;
#47283 =( NAMED_UNIT ( * ) SI_UNIT ( $, .STERADIAN. ) SOLID_ANGLE_UNIT ( ) );
#47285 = CARTESIAN_POINT ( 'NONE',  ( -4.869065774733593699, -2.951204850257779011, 102.3543991519893979 ) ) ;
#47286 = ORIENTED_EDGE ( 'NONE', *, *, #32065, .F. ) ;
#47287 = CARTESIAN_POINT ( 'NONE',  ( -26.96123873314553165, 312.0017479745702076, 11.65844439973563773 ) ) ;
#47288 = VERTEX_POINT ( 'NONE', #61418 ) ;
#47289 = CARTESIAN_POINT ( 'NONE',  ( 22.14525041823859297, 304.2680615509976860, 10.02651133272836681 ) ) ;
#47290 = AXIS2_PLACEMENT_3D ( 'NONE', #92336, #18481, #60012 ) ;
#47291 = DIRECTION ( 'NONE',  ( -1.000000000000000000, -0.000000000000000000, -0.000000000000000000 ) ) ;
#47292 = CARTESIAN_POINT ( 'NONE',  ( 7.999999999999998224, -12.78125000409676915, 3.313708498984766049 ) ) ;
#47293 = EDGE_LOOP ( 'NONE', ( #81075, #34223, #53937, #91860, #33195 ) ) ;
#47294 = EDGE_CURVE ( 'NONE', #36720, #43900, #51700, .T. ) ;
#47295 = PRODUCT_DEFINITION_FORMATION_WITH_SPECIFIED_SOURCE ( 'ANY', '', #36449, .NOT_KNOWN. ) ;
#47296 = CARTESIAN_POINT ( 'NONE',  ( -1.724765290415802621, -3.000000000000002665, -69.73714729959421277 ) ) ;
#47297 = CARTESIAN_POINT ( 'NONE',  ( 6.999999999999998224, -12.54465221550629472, 8.223849511754997010 ) ) ;
#47298 = AXIS2_PLACEMENT_3D ( 'NONE', #100689, #17669, #41928 ) ;
#47299 = CARTESIAN_POINT ( 'NONE',  ( -103.3252443258257216, -59.99999999999994316, 203.1850994544522564 ) ) ;
#47300 = CARTESIAN_POINT ( 'NONE',  ( 6.585304930659545697, 4.021878819315965359, -6.500000000000000888 ) ) ;
#47301 = CARTESIAN_POINT ( 'NONE',  ( 79.80566310147598585, -59.99999999999998579, 195.7472193146226402 ) ) ;
#47302 = CARTESIAN_POINT ( 'NONE',  ( 0.000000000000000000, 0.000000000000000000, 0.000000000000000000 ) ) ;
#47303 = CARTESIAN_POINT ( 'NONE',  ( 1.100366063348540591, 25.39417708419738773, -40.11413014599601468 ) ) ;
#47305 = CARTESIAN_POINT ( 'NONE',  ( 10.04875798505854512, -18.58642205010649562, 26.99592638574074144 ) ) ;
#47304 = CARTESIAN_POINT ( 'NONE',  ( -114.4520492995273315, -60.00000000000003553, 166.3968728284598342 ) ) ;
#47306 = CARTESIAN_POINT ( 'NONE',  ( 82.68768327601632961, -37.99999999999995026, 21.01035113837339097 ) ) ;
#47308 = EDGE_CURVE ( 'NONE', #81828, #101117, #68928, .T. ) ;
#47307 = DIRECTION ( 'NONE',  ( -1.000000000000000000, -0.000000000000000000, -0.000000000000000000 ) ) ;
#47309 = CARTESIAN_POINT ( 'NONE',  ( -45.35675342690321088, -25.70246126498986428, 40.33334816179175419 ) ) ;
#47310 = PLANE ( 'NONE',  #78070 ) ;
#47311 = ORIENTED_EDGE ( 'NONE', *, *, #29619, .T. ) ;
#47312 = DIRECTION ( 'NONE',  ( -0.000000000000000000, -0.000000000000000000, -1.000000000000000000 ) ) ;
#47313 = CARTESIAN_POINT ( 'NONE',  ( 0.000000000000000000, 0.000000000000000000, 0.000000000000000000 ) ) ;
#47314 = EDGE_CURVE ( 'NONE', #76857, #93549, #70752, .T. ) ;
#47315 = DIRECTION ( 'NONE',  ( -1.000000000000000000, 0.000000000000000000, 0.000000000000000000 ) ) ;
#47316 = LINE ( 'NONE', #80212, #100263 ) ;
#47317 = ORIENTED_EDGE ( 'NONE', *, *, #29187, .T. ) ;
#47318 = CARTESIAN_POINT ( 'NONE',  ( -7.314871723833043404, -6.279301537700069602, 13.99616156953552704 ) ) ;
#47319 = ORIENTED_EDGE ( 'NONE', *, *, #84026, .F. ) ;
#47320 = CARTESIAN_POINT ( 'NONE',  ( 109.2084914459248495, -29.99999999998984634, 181.8260726147819071 ) ) ;
#47321 = DIRECTION ( 'NONE',  ( 0.000000000000000000, 1.000000000000000000, 0.000000000000000000 ) ) ;
#47322 = CARTESIAN_POINT ( 'NONE',  ( 6.275175096193794211, 41.94081482539142058, -59.38054156036670861 ) ) ;
#47323 = DIRECTION ( 'NONE',  ( 0.000000000000000000, 1.000000000000000000, 0.000000000000000000 ) ) ;
#47324 = CARTESIAN_POINT ( 'NONE',  ( 92.38157122146077427, -30.00000000000000355, 102.4062337837748800 ) ) ;
#47325 = PRODUCT_DEFINITION_SHAPE ( 'NONE', 'NONE',  #58835 ) ;
#47326 = DIRECTION ( 'NONE',  ( -1.000000000000000000, 0.000000000000000000, 0.000000000000000000 ) ) ;
#47327 = ORIENTED_EDGE ( 'NONE', *, *, #87673, .T. ) ;
#47328 = EDGE_CURVE ( 'NONE', #98966, #99927, #30653, .T. ) ;
#47329 = ORIENTED_EDGE ( 'NONE', *, *, #15608, .F. ) ;
#47330 = ORIENTED_EDGE ( 'NONE', *, *, #59750, .F. ) ;
#47331 = DIRECTION ( 'NONE',  ( 0.000000000000000000, 0.000000000000000000, 1.000000000000000000 ) ) ;
#47332 = CARTESIAN_POINT ( 'NONE',  ( -44.31081229532764354, 435.2284720930225603, 12.07948685322291382 ) ) ;
#47333 = DIRECTION ( 'NONE',  ( -1.000000000000000000, -0.000000000000000000, -0.000000000000000000 ) ) ;
#47334 = VERTEX_POINT ( 'NONE', #64078 ) ;
#47335 = LINE ( 'NONE', #87287, #61571 ) ;
#47336 = B_SPLINE_CURVE_WITH_KNOTS ( 'NONE', 3,
 ( #15657, #25385, #49076, #17277, #31871, #83059 ),
 .UNSPECIFIED., .F., .F.,
 ( 4, 2, 4 ),
 ( 0.000000000000000000, 0.001720102060488473651, 0.003440204120976947302 ),
 .UNSPECIFIED. ) ;
#47337 = ORIENTED_EDGE ( 'NONE', *, *, #94575, .T. ) ;
#47338 = CARTESIAN_POINT ( 'NONE',  ( -42.19180677453720563, 462.2931784592652207, 3.389262873192004477 ) ) ;
#47339 = CARTESIAN_POINT ( 'NONE',  ( 96.52417567451942659, -38.48283943534769946, 201.1700310018051994 ) ) ;
#47340 = DIRECTION ( 'NONE',  ( -1.000000000000000000, -1.224606353822377258E-16, -0.000000000000000000 ) ) ;
#47341 = COLOUR_RGB ( '', 0.09019608, 0.27058824, 0.51372549) ;
#47342 = CARTESIAN_POINT ( 'NONE',  ( 82.90087968821347886, -37.85046927419193707, 0.5094595297241235610 ) ) ;
#47343 = CARTESIAN_POINT ( 'NONE',  ( 83.62068454613667257, -38.00000000000004263, 173.3489829705700060 ) ) ;
#47344 = CIRCLE ( 'NONE', #26756, 4.172000000000009479 ) ;
#47345 = CARTESIAN_POINT ( 'NONE',  ( 29.20990149186424745, 312.7062169680672241, 12.31820844411544869 ) ) ;
#47346 = PRESENTATION_LAYER_ASSIGNMENT (  '', '', ( #66282 ) ) ;
#47347 = CARTESIAN_POINT ( 'NONE',  ( -52.56483885390523625, 40.83906611473335602, -38.23529411764706509 ) ) ;
#47348 = PRESENTATION_LAYER_ASSIGNMENT (  '', '', ( #4247 ) ) ;
#47349 = FACE_OUTER_BOUND ( 'NONE', #4762, .T. ) ;
#47350 = AXIS2_PLACEMENT_3D ( 'NONE', #30756, #71693, #63642 ) ;
#47351 = AXIS2_PLACEMENT_3D ( 'NONE', #92446, #25645, #17526 ) ;
#47352 = CARTESIAN_POINT ( 'NONE',  ( 0.000000000000000000, 0.000000000000000000, -13.00000000000000000 ) ) ;
#47354 = ORIENTED_EDGE ( 'NONE', *, *, #97004, .T. ) ;
#47353 =( BOUNDED_SURFACE ( )  B_SPLINE_SURFACE ( 3, 2, ( 
 ( #6342, #72162, #31210 ),
 ( #96971, #23106, #37178 ),
 ( #86251, #70039, #94868 ),
 ( #16582, #98548, #73744 ) ),
 .UNSPECIFIED., .F., .F., .F. ) 
 B_SPLINE_SURFACE_WITH_KNOTS ( ( 4, 4 ),
 ( 3, 3 ),
 ( -3.989863994746656317E-17, 0.001384307398017841327 ),
 ( 0.000000000000000000, 1.000000000000000000 ),
 .UNSPECIFIED. ) 
 GEOMETRIC_REPRESENTATION_ITEM ( )  RATIONAL_B_SPLINE_SURFACE ( (
 ( 1.000000000000000000, 0.7976994903569347706, 1.000000000000000000),
 ( 1.000000000000000000, 0.8073889694078232315, 1.000000000000000000),
 ( 1.000000000000000000, 0.8171087964277252702, 1.000000000000000000),
 ( 1.000000000000000000, 0.8266506655096979017, 1.000000000000000000) ) ) 
 REPRESENTATION_ITEM ( '' )  SURFACE ( )  );
#47355 = CARTESIAN_POINT ( 'NONE',  ( 15.59999999999999787, 1.533819458162526451E-15, 0.000000000000000000 ) ) ;
#47356 = CARTESIAN_POINT ( 'NONE',  ( -32.99999999999992184, 463.5362553048593099, 6.739467187734545561 ) ) ;
#47357 = CARTESIAN_POINT ( 'NONE',  ( -3.454256172262368363, 27.53752580628883706, 4.999999999999998224 ) ) ;
#47358 = ORIENTED_EDGE ( 'NONE', *, *, #60882, .T. ) ;
#47359 = CARTESIAN_POINT ( 'NONE',  ( -35.30297382066545708, 361.4833082129059676, 3.507038767897731280 ) ) ;
#47360 = CARTESIAN_POINT ( 'NONE',  ( -33.63754935668455914, 302.6102131421956756, 11.72270476798247962 ) ) ;
#47361 = CARTESIAN_POINT ( 'NONE',  ( 7.576187751213149468, 54.08017525257882596, -3.569500874023384895 ) ) ;
#47362 = UNCERTAINTY_MEASURE_WITH_UNIT (LENGTH_MEASURE( 1.000000000000000082E-05 ), #81869, 'distance_accuracy_value', 'NONE');
#47363 = CARTESIAN_POINT ( 'NONE',  ( 31.84999999999999787, -3.309499999999999886, 4.475777889183790779E-16 ) ) ;
#47364 = CARTESIAN_POINT ( 'NONE',  ( 7.999999999999998224, -15.59374999999999289, 3.313708498984766493 ) ) ;
#47365 = CARTESIAN_POINT ( 'NONE',  ( 28.52923163747771440, -23.57397691714684385, 38.13648777926081834 ) ) ;
#47366 = EDGE_LOOP ( 'NONE', ( #989, #77140, #79299, #45536, #100016 ) ) ;
#47367 = CARTESIAN_POINT ( 'NONE',  ( 84.69674785225238622, -46.56892218208203360, 186.7899396118458810 ) ) ;
#47368 = CARTESIAN_POINT ( 'NONE',  ( -48.76594521878733701, 8.294242253543364640, 16.61919356891297284 ) ) ;
#47369 = CARTESIAN_POINT ( 'NONE',  ( 3.568931636294630394, -0.9305242695747285575, 103.4741166605239471 ) ) ;
#47370 = ORIENTED_EDGE ( 'NONE', *, *, #67267, .T. ) ;
#47371 = CARTESIAN_POINT ( 'NONE',  ( 94.19505752079862759, -57.67256688133579701, 22.60860429288029749 ) ) ;
#47372 = CARTESIAN_POINT ( 'NONE',  ( 36.29541806397946146, 438.2518625957742984, 3.876047449288812174 ) ) ;
#47373 = DIRECTION ( 'NONE',  ( 1.000000000000000000, 1.224606353822377258E-16, 0.000000000000000000 ) ) ;
#47374 = CARTESIAN_POINT ( 'NONE',  ( 28.79633237789232325, 10.21664471455438772, 41.74470786255320576 ) ) ;
#47375 = EDGE_CURVE ( 'NONE', #85296, #76782, #58756, .T. ) ;
#47376 = PRODUCT_DEFINITION_FORMATION_WITH_SPECIFIED_SOURCE ( 'ANY', '', #101837, .NOT_KNOWN. ) ;
#47377 = B_SPLINE_CURVE_WITH_KNOTS ( 'NONE', 3,
 ( #99319, #10837, #50764, #25493, #34648, #101472, #42698, #58350, #2217, #84225, #100398, #59432, #83156, #43236, #42162, #68589, #26041, #67518, #8730, #84756, #26560, #91270, #35167, #90724, #9252, #2760, #17381, #58900, #35711, #92295, #50255, #68034, #75043, #1141, #34116, #27624, #100928, #59975, #92836, #91790, #16838, #1693, #49720, #19000, #43757, #10320, #66987, #41638, #51843, #75594, #99868, #18449, #74521, #51303, #76649, #85284, #103589, #28678, #5429, #4903, #12441, #11372 ),
 .UNSPECIFIED., .F., .F.,
 ( 4, 2, 2, 2, 2, 2, 2, 2, 2, 2, 2, 2, 2, 2, 2, 2, 2, 2, 2, 2, 2, 2, 2, 2, 2, 2, 2, 2, 2, 2, 4 ),
 ( 0.5710235574187877416, 0.5770410422503359227, 0.5830585270818841037, 0.5890760119134322848, 0.5920847543292063753, 0.5950934967449803548, 0.6011109815765285358, 0.6026153527844155811, 0.6041197239923026263, 0.6071284664080768279, 0.6131459512396248979, 0.6146503224475119431, 0.6161546936553989884, 0.6191634360711730789, 0.6251809209027212599, 0.6311984057342694410, 0.6372158905658175110, 0.6432333753973656920, 0.6552683450604619431, 0.6673033147235581941, 0.6913732540497506962, 0.7034082237128469473, 0.7154431933759433093, 0.7274781630390395604, 0.7395131327021358114, 0.7455306175336839924, 0.7515481023652321735, 0.7545568447810062640, 0.7575655871967803545, 0.7605743296125544450, 0.7635830720283285356 ),
 .UNSPECIFIED. ) ;
#47378 = CARTESIAN_POINT ( 'NONE',  ( 28.43956359133950684, 17.90386495480485252, 40.70637206596285296 ) ) ;
#47379 = CARTESIAN_POINT ( 'NONE',  ( -7.137815226409945701, -4.999999999999998224, 4.175893272574815462 ) ) ;
#47380 = CARTESIAN_POINT ( 'NONE',  ( 0.000000000000000000, 0.000000000000000000, 0.000000000000000000 ) ) ;
#47382 = CARTESIAN_POINT ( 'NONE',  ( -13.72579875526420068, 3.063920234766396966, 6.005637484505932377 ) ) ;
#47381 = DIRECTION ( 'NONE',  ( -1.000000000000000000, -0.000000000000000000, -0.000000000000000000 ) ) ;
#47383 = EDGE_CURVE ( 'NONE', #33590, #71421, #34168, .T. ) ;
#47384 = CARTESIAN_POINT ( 'NONE',  ( 42.61340452791766609, 486.8925439250689351, 7.464118458850313331 ) ) ;
#47385 = CARTESIAN_POINT ( 'NONE',  ( 9.999999999999957367, 15.00000000000001066, -3.836411046841929018 ) ) ;
#47386 = LINE ( 'NONE', #72722, #82129 ) ;
#47387 = CARTESIAN_POINT ( 'NONE',  ( -83.28021094808033808, -38.00000000000000000, -7.973042742588115850 ) ) ;
#47388 = CIRCLE ( 'NONE', #28742, 5.000000000000001776 ) ;
#47389 = ADVANCED_FACE ( 'NONE', ( #22571 ), #27769, .T. ) ;
#47390 = ORIENTED_EDGE ( 'NONE', *, *, #20313, .T. ) ;
#47391 = CARTESIAN_POINT ( 'NONE',  ( 6.289692432696722513, -6.589071317540692085, -2.245373559998704582 ) ) ;
#47392 = CARTESIAN_POINT ( 'NONE',  ( 30.00000000000000000, 1.040949779275250534E-15, -8.000000000000007105 ) ) ;
#47393 = CARTESIAN_POINT ( 'NONE',  ( 5.477432325710315020, -61.83520464429526697, 2.459915882346687344 ) ) ;
#47394 = CARTESIAN_POINT ( 'NONE',  ( -51.46469236758235155, -60.22827249275542272, -31.80550166486139574 ) ) ;
#47395 = ORIENTED_EDGE ( 'NONE', *, *, #97914, .F. ) ;
#47396 = B_SPLINE_CURVE_WITH_KNOTS ( 'NONE', 3,
 ( #541, #32453, #80960, #57210, #56684, #72865, #40513, #23295, #72352, #48589, #106291, #14624, #24366, #16231, #31913, #89606 ),
 .UNSPECIFIED., .F., .F.,
 ( 4, 2, 2, 2, 2, 2, 2, 4 ),
 ( 0.000000000000000000, 0.002593706636443856260, 0.005187413272887715122, 0.006484266591109646288, 0.007781119909331575719, 0.008429546568442540869, 0.009077973227553506885, 0.01037482654577543718 ),
 .UNSPECIFIED. ) ;
#47397 = CARTESIAN_POINT ( 'NONE',  ( 3.093533885182577325, 6.874201416486802607, -7.446478553994766436 ) ) ;
#47398 = ORIENTED_EDGE ( 'NONE', *, *, #103451, .F. ) ;
#47399 = VECTOR ( 'NONE', #30658, 1000.000000000000000 ) ;
#47400 = DIRECTION ( 'NONE',  ( 0.000000000000000000, -1.000000000000000000, 0.000000000000000000 ) ) ;
#47401 = CARTESIAN_POINT ( 'NONE',  ( -92.74294554908810539, -60.00000000000001421, -7.911394269966801396 ) ) ;
#47402 = ORIENTED_EDGE ( 'NONE', *, *, #39111, .F. ) ;
#47403 = CARTESIAN_POINT ( 'NONE',  ( 39.57197012660297730, -33.18875763605801410, -29.36643390136424969 ) ) ;
#47404 = AXIS2_PLACEMENT_3D ( 'NONE', #77853, #13095, #12041 ) ;
#47405 = CARTESIAN_POINT ( 'NONE',  ( -7.568397567301111017, 54.27789163617485713, -2.014810990348805841 ) ) ;
#47406 = CARTESIAN_POINT ( 'NONE',  ( 97.47947159951426954, -52.81402158103271205, 195.2340248519632553 ) ) ;
#47407 = AXIS2_PLACEMENT_3D ( 'NONE', #12779, #36054, #37646 ) ;
#47409 = LINE ( 'NONE', #6413, #92609 ) ;
#47408 = SURFACE_SIDE_STYLE ('',( #14494 ) ) ;
#47410 = CARTESIAN_POINT ( 'NONE',  ( -83.81111989978313659, -29.06180828734868626, 160.7833297484586126 ) ) ;
#47411 = ORIENTED_EDGE ( 'NONE', *, *, #60102, .T. ) ;
#47412 = CIRCLE ( 'NONE', #885, 0.5000000000000004441 ) ;
#47413 = VERTEX_POINT ( 'NONE', #70023 ) ;
#47414 = AXIS2_PLACEMENT_3D ( 'NONE', #84259, #59470, #67022 ) ;
#47415 = EDGE_LOOP ( 'NONE', ( #42661, #60540 ) ) ;
#47416 = CARTESIAN_POINT ( 'NONE',  ( 31.14080955122648220, 433.9629369115588702, 24.00288416902248656 ) ) ;
#47417 = CARTESIAN_POINT ( 'NONE',  ( -5.978750298146849218, -13.03636037196927511, 13.21647969580618742 ) ) ;
#47418 = VERTEX_POINT ( 'NONE', #45233 ) ;
#47419 = EDGE_CURVE ( 'NONE', #492, #49001, #86762, .T. ) ;
#47420 = SURFACE_STYLE_FILL_AREA ( #15053 ) ;
#47421 = CARTESIAN_POINT ( 'NONE',  ( -9.999999999999998224, 15.00000000000000000, 1.785846837348918736E-15 ) ) ;
#47422 = CARTESIAN_POINT ( 'NONE',  ( -85.03051761340829273, -57.56200303720294897, 202.2882931814572487 ) ) ;
#47423 = CARTESIAN_POINT ( 'NONE',  ( -1.002887009549091601E-15, -0.7818963811860187851, 8.000000000000000000 ) ) ;
#47424 = CARTESIAN_POINT ( 'NONE',  ( -62.06337123375774212, 48.00000000000000711, -19.99347512944444816 ) ) ;
#47425 = CARTESIAN_POINT ( 'NONE',  ( 16.08349330513380337, 4.000000000000003553, 0.000000000000000000 ) ) ;
#47426 = FACE_OUTER_BOUND ( 'NONE', #3591, .T. ) ;
#47427 = CARTESIAN_POINT ( 'NONE',  ( 75.59946810849663734, -59.99999999999992895, -32.85428466877961284 ) ) ;
#47428 = EDGE_CURVE ( 'NONE', #91520, #3430, #20993, .T. ) ;
#47430 = EDGE_CURVE ( 'NONE', #53605, #71336, #98319, .T. ) ;
#47429 = CARTESIAN_POINT ( 'NONE',  ( -66.01875947964627755, -14.21045842199442077, 101.7785962432973292 ) ) ;
#47431 = CARTESIAN_POINT ( 'NONE',  ( -53.63040634117179906, -18.70038625127083165, 49.64862236185882693 ) ) ;
#47432 = ORIENTED_EDGE ( 'NONE', *, *, #8767, .F. ) ;
#47433 = CARTESIAN_POINT ( 'NONE',  ( 3.013128138968859560, 20.49583289608097658, -6.321380353784028294 ) ) ;
#47434 = ORIENTED_EDGE ( 'NONE', *, *, #61037, .F. ) ;
#47435 = CARTESIAN_POINT ( 'NONE',  ( -99.02822291621761508, -37.77734143312120807, 191.8549729512566273 ) ) ;
#47436 = CARTESIAN_POINT ( 'NONE',  ( 32.87547266101556431, 465.6993878536748070, 10.91512469976365551 ) ) ;
#47437 = ORIENTED_EDGE ( 'NONE', *, *, #35901, .T. ) ;
#47438 = CARTESIAN_POINT ( 'NONE',  ( 19.06872869572427120, 49.63275118039182843, 61.79276190149701620 ) ) ;
#47439 = CARTESIAN_POINT ( 'NONE',  ( 89.92042692463260778, -38.39514772492996286, -16.19348958354982670 ) ) ;
#47440 = FACE_BOUND ( 'NONE', #87181, .T. ) ;
#47441 = FACE_OUTER_BOUND ( 'NONE', #4182, .T. ) ;
#47442 = CARTESIAN_POINT ( 'NONE',  ( -6.426132457094225536, 294.7471176151092891, 9.914747880764233301 ) ) ;
#47443 = CONICAL_SURFACE ( 'NONE', #55977, 3.309500000000001663, 0.9599310885968770357 ) ;
#47444 = CARTESIAN_POINT ( 'NONE',  ( -42.15357157759102336, 485.2432036427136381, -2.744622672921036788 ) ) ;
#47445 = CARTESIAN_POINT ( 'NONE',  ( 66.15617483897442241, -29.99999999999999645, 83.57477076473479372 ) ) ;
#47446 = DIRECTION ( 'NONE',  ( 1.000000000000000000, 0.000000000000000000, -0.000000000000000000 ) ) ;
#47447 = CARTESIAN_POINT ( 'NONE',  ( -3.352941176470583873, -48.79941684889506348, 104.5794940929807524 ) ) ;
#47448 = DIRECTION ( 'NONE',  ( -0.1792365085138481196, 0.7133058216316990885, 0.6775463665625343079 ) ) ;
#47449 = CARTESIAN_POINT ( 'NONE',  ( -35.04348997864995852, 484.2371297655225817, -0.9829126381465729256 ) ) ;
#47450 = EDGE_CURVE ( 'NONE', #347, #85798, #4226, .T. ) ;
#47451 = VERTEX_POINT ( 'NONE', #102922 ) ;
#47452 = ORIENTED_EDGE ( 'NONE', *, *, #71268, .F. ) ;
#47453 = CARTESIAN_POINT ( 'NONE',  ( 48.68234789899833714, -60.28324891123607898, 55.32515784904787637 ) ) ;
#47454 = CARTESIAN_POINT ( 'NONE',  ( -0.2948623160389114428, 13.62334926694027892, 49.28320643957499669 ) ) ;
#47455 = DIRECTION ( 'NONE',  ( 0.1659550938513499052, -0.9861333108788029600, 5.742823393231985512E-13 ) ) ;
#47456 = EDGE_CURVE ( 'NONE', #7582, #15655, #5322, .T. ) ;
#47457 = CARTESIAN_POINT ( 'NONE',  ( -108.7075558750168227, -38.35682683513768865, 191.0385089548209976 ) ) ;
#47458 = EDGE_LOOP ( 'NONE', ( #40266, #23964, #44659, #101427 ) ) ;
#47459 = CARTESIAN_POINT ( 'NONE',  ( 84.99785917221272769, -38.35913927195756656, -22.84962175036736909 ) ) ;
#47460 = CARTESIAN_POINT ( 'NONE',  ( 11.97147371475453248, 19.60245619413215223, -7.526067045436439784 ) ) ;
#47461 = CARTESIAN_POINT ( 'NONE',  ( 28.86650669486618881, 1.474610560812782335E-15, 0.000000000000000000 ) ) ;
#47462 = CARTESIAN_POINT ( 'NONE',  ( 21.09715123528542691, 1.340359594676612611E-15, 0.000000000000000000 ) ) ;
#47463 = CARTESIAN_POINT ( 'NONE',  ( 101.6986830034126683, -37.84844073324973834, 153.9942977854028072 ) ) ;
#47464 = CARTESIAN_POINT ( 'NONE',  ( 22.01999690012047495, 28.11337147615395438, 31.58836928536987187 ) ) ;
#47465 = CARTESIAN_POINT ( 'NONE',  ( -35.70850055078799556, 426.6386616601230912, 5.234124974471177083 ) ) ;
#47466 = FACE_OUTER_BOUND ( 'NONE', #53968, .T. ) ;
#47467 = CARTESIAN_POINT ( 'NONE',  ( 10.50000000000000000, -5.000000000000000000, -9.904958390907863119 ) ) ;
#47468 = EDGE_CURVE ( 'NONE', #28621, #22025, #72141, .T. ) ;
#47469 = CARTESIAN_POINT ( 'NONE',  ( 95.19103829490188673, -60.00000000000000000, 202.5701353115400991 ) ) ;
#47470 = AXIS2_PLACEMENT_3D ( 'NONE', #90783, #17962, #18502 ) ;
#47471 = FACE_OUTER_BOUND ( 'NONE', #30377, .T. ) ;
#47472 = ORIENTED_EDGE ( 'NONE', *, *, #34970, .T. ) ;
#47473 = CARTESIAN_POINT ( 'NONE',  ( 58.48759157769109862, -18.66117102831294261, 59.19987231648309489 ) ) ;
#47474 = CARTESIAN_POINT ( 'NONE',  ( -28.98077275437907474, 306.6777056724459385, -9.140503625966282186 ) ) ;
#47475 = CARTESIAN_POINT ( 'NONE',  ( 7.744329845603316720, 33.46288230153454890, -2.018701143083232008 ) ) ;
#47476 = CARTESIAN_POINT ( 'NONE',  ( -7.151597709147948123, 28.21070734947783976, 3.587174531012139678 ) ) ;
#47477 = ORIENTED_EDGE ( 'NONE', *, *, #67276, .T. ) ;
#47479 = CARTESIAN_POINT ( 'NONE',  ( -9.337186727013605747, -51.98687375574689895, 30.58335800272115534 ) ) ;
#47478 = CARTESIAN_POINT ( 'NONE',  ( -102.4962415325779546, -38.43804299320050433, 199.4167516955215547 ) ) ;
#47480 = DIRECTION ( 'NONE',  ( -1.000000000000000000, -1.224606353822377258E-16, -0.000000000000000000 ) ) ;
#47481 = CARTESIAN_POINT ( 'NONE',  ( 31.44900225665126570, 397.6393522637353044, 24.40758882435354948 ) ) ;
#47482 = LINE ( 'NONE', #73884, #97122 ) ;
#47483 = CARTESIAN_POINT ( 'NONE',  ( 7.999999999999998224, -33.59374999999999289, 3.313708498984766493 ) ) ;
#47484 = CARTESIAN_POINT ( 'NONE',  ( 8.737863884121400915, -4.999999999998638422, -90.03618980231146907 ) ) ;
#47485 = CIRCLE ( 'NONE', #18260, 4.000000000000000888 ) ;
#47486 = AXIS2_PLACEMENT_3D ( 'NONE', #19291, #100141, #92051 ) ;
#47487 = AXIS2_PLACEMENT_3D ( 'NONE', #78080, #93740, #12273 ) ;
#47488 = DIRECTION ( 'NONE',  ( 0.000000000000000000, -1.000000000000000000, 0.000000000000000000 ) ) ;
#47489 = AXIS2_PLACEMENT_3D ( 'NONE', #15712, #16781, #83105 ) ;
#47490 = EDGE_LOOP ( 'NONE', ( #5801, #76547, #7799, #46189 ) ) ;
#47491 = CARTESIAN_POINT ( 'NONE',  ( 86.03557063178290321, -18.41209965610634214, 166.1552846382974451 ) ) ;
#47492 = CARTESIAN_POINT ( 'NONE',  ( -2.100000000000004530, 0.000000000000000000, 0.000000000000000000 ) ) ;
#47493 = CARTESIAN_POINT ( 'NONE',  ( 37.24829320759891971, 27.71737586852629676, 13.42523556547244290 ) ) ;
#47494 = ORIENTED_EDGE ( 'NONE', *, *, #87986, .F. ) ;
#47495 = FACE_OUTER_BOUND ( 'NONE', #33142, .T. ) ;
#47496 = CIRCLE ( 'NONE', #13072, 8.857142857142855874 ) ;
#47497 = CARTESIAN_POINT ( 'NONE',  ( 7.347171990167045585, -3.439186728100360302, -18.43985286355972875 ) ) ;
#47498 = CARTESIAN_POINT ( 'NONE',  ( 34.83349330513380693, 4.898587196589411843E-16, -4.000000000000001776 ) ) ;
#47499 = LINE ( 'NONE', #81773, #77933 ) ;
#47500 = SURFACE_STYLE_FILL_AREA ( #79345 ) ;
#47501 = AXIS2_PLACEMENT_3D ( 'NONE', #16883, #49763, #91830 ) ;
#47502 =( LENGTH_UNIT ( ) NAMED_UNIT ( * ) SI_UNIT ( .MILLI., .METRE. ) );
#47503 = EDGE_LOOP ( 'NONE', ( #84037, #94917 ) ) ;
#47504 = EDGE_CURVE ( 'NONE', #45889, #64182, #96623, .T. ) ;
#47505 = AXIS2_PLACEMENT_3D ( 'NONE', #5836, #79731, #54363 ) ;
#47506 = CARTESIAN_POINT ( 'NONE',  ( 6.499999999999999112, 4.014041399406593769, -6.470356572124274841 ) ) ;
#47507 = CYLINDRICAL_SURFACE ( 'NONE', #1519, 7.500000000000000000 ) ;
#47508 = ADVANCED_FACE ( 'NONE', ( #30112 ), #93165, .T. ) ;
#47510 = CARTESIAN_POINT ( 'NONE',  ( -10.42678887926924958, 17.27620279768637701, -9.792472684408327410 ) ) ;
#47509 = CARTESIAN_POINT ( 'NONE',  ( -4.358015154622025378, -18.45760210153450487, 35.06886539972598626 ) ) ;
#47511 = ADVANCED_FACE ( 'NONE', ( #13357 ), #45056, .T. ) ;
#47512 = CARTESIAN_POINT ( 'NONE',  ( -5.082755093536325042, -17.09375000204838813, -5.082755093536325930 ) ) ;
#47513 = CARTESIAN_POINT ( 'NONE',  ( -29.35512824071851057, 13.99081654327141599, -42.06953762909878947 ) ) ;
#47514 = CARTESIAN_POINT ( 'NONE',  ( -6.943035977205679110, 41.50417750172036335, -58.81491712266881677 ) ) ;
#47515 = VERTEX_POINT ( 'NONE', #66173 ) ;
#47516 = DIRECTION ( 'NONE',  ( 0.000000000000000000, 1.000000000000000000, 0.000000000000000000 ) ) ;
#47517 = EDGE_CURVE ( 'NONE', #10424, #55309, #64004, .T. ) ;
#47518 = EDGE_CURVE ( 'NONE', #14808, #57343, #15498, .T. ) ;
#47519 = DIRECTION ( 'NONE',  ( -1.000000000000000000, 0.000000000000000000, 0.000000000000000000 ) ) ;
#47520 = CIRCLE ( 'NONE', #42367, 1.000000000000000888 ) ;
#47521 = CARTESIAN_POINT ( 'NONE',  ( -7.856068184137752652, 67.85260481710604097, 0.000000000000000000 ) ) ;
#47522 = CARTESIAN_POINT ( 'NONE',  ( -5.902907888919634694, -5.000000000000001776, -73.20788160634965891 ) ) ;
#47523 = CARTESIAN_POINT ( 'NONE',  ( 6.499999999999999112, 3.752776749732559036, -6.064240316920397333 ) ) ;
#47524 = ORIENTED_EDGE ( 'NONE', *, *, #38172, .T. ) ;
#47525 = DIRECTION ( 'NONE',  ( 0.000000000000000000, 0.000000000000000000, 1.000000000000000000 ) ) ;
#47526 = CARTESIAN_POINT ( 'NONE',  ( -33.00000000000000000, 489.5971041675261404, 10.80646835458718868 ) ) ;
#47527 = ORIENTED_EDGE ( 'NONE', *, *, #21689, .F. ) ;
#47528 = CARTESIAN_POINT ( 'NONE',  ( 0.000000000000000000, 0.000000000000000000, -2.000000000000000444 ) ) ;
#47529 = CARTESIAN_POINT ( 'NONE',  ( -2.679344702995778427, -0.3583992640727010626, 103.0669469696961897 ) ) ;
#47530 = CARTESIAN_POINT ( 'NONE',  ( 6.738100180926640093, 41.71798714554645215, -59.05424661244425266 ) ) ;
#47531 = B_SPLINE_CURVE_WITH_KNOTS ( 'NONE', 3,
 ( #36801, #93944, #53482, #51869 ),
 .UNSPECIFIED., .F., .F.,
 ( 4, 4 ),
 ( 0.000000000000000000, 0.001257843226828573311 ),
 .UNSPECIFIED. ) ;
#47532 =( NAMED_UNIT ( * ) PLANE_ANGLE_UNIT ( ) SI_UNIT ( $, .RADIAN. ) );
#47533 = CARTESIAN_POINT ( 'NONE',  ( -107.3255816732216203, -60.00000000000000000, 124.7109082821343691 ) ) ;
#47534 = DIRECTION ( 'NONE',  ( 0.000000000000000000, -0.5000000000000008882, 0.8660254037844381525 ) ) ;
#47535 = DIRECTION ( 'NONE',  ( 0.4165977904505306917, 0.000000000000000000, -0.9090909090909092827 ) ) ;
#47536 = DIRECTION ( 'NONE',  ( -1.000000000000000000, -1.224606353822377258E-16, -0.000000000000000000 ) ) ;
#47537 = CARTESIAN_POINT ( 'NONE',  ( -9.739726766101606259, -5.000000000000002665, -82.38252115500968387 ) ) ;
#47538 = CARTESIAN_POINT ( 'NONE',  ( -84.88372816773981810, -28.91961114234488761, 171.4482036657654760 ) ) ;
#47539 = AXIS2_PLACEMENT_3D ( 'NONE', #36062, #44115, #36592 ) ;
#47540 = EDGE_LOOP ( 'NONE', ( #21238, #78076, #17859, #4141, #13694 ) ) ;
#47541 = VERTEX_POINT ( 'NONE', #106626 ) ;
#47542 = CARTESIAN_POINT ( 'NONE',  ( 5.094000037296075867, -67.44634123771224665, -3.174960020027664420 ) ) ;
#47543 = CARTESIAN_POINT ( 'NONE',  ( -84.22203528576365272, -45.26556005254958848, 26.09078575504823405 ) ) ;
#47544 = DIRECTION ( 'NONE',  ( 0.000000000000000000, -1.000000000000000000, -0.000000000000000000 ) ) ;
#47545 = CARTESIAN_POINT ( 'NONE',  ( 37.56673239365841255, -1.200000000000000030E-05, -12.20617127781092215 ) ) ;
#47546 = AXIS2_PLACEMENT_3D ( 'NONE', #92902, #45437, #84823 ) ;
#47547 = CARTESIAN_POINT ( 'NONE',  ( 3.363293968486921859, 30.68813792664008844, -4.999999999999997335 ) ) ;
#47548 = DIRECTION ( 'NONE',  ( 0.000000000000000000, -1.000000000000000000, 0.000000000000000000 ) ) ;
#47549 = FACE_OUTER_BOUND ( 'NONE', #35142, .T. ) ;
#47550 = CARTESIAN_POINT ( 'NONE',  ( 107.3649583438541271, -29.99999999999998579, 190.7484263893222192 ) ) ;
#47551 = EDGE_CURVE ( 'NONE', #37712, #42350, #70838, .T. ) ;
#47552 = CARTESIAN_POINT ( 'NONE',  ( -107.3073691194147443, -59.99999999999994316, 109.8427349246714613 ) ) ;
#47553 = CARTESIAN_POINT ( 'NONE',  ( -63.78795251116700626, -32.53250583283151798, 79.11474259739455306 ) ) ;
#47554 = ORIENTED_EDGE ( 'NONE', *, *, #80421, .F. ) ;
#47555 = CARTESIAN_POINT ( 'NONE',  ( -39.07677920758315793, 39.42618461990478096, 52.28553321386016250 ) ) ;
#47556 = CARTESIAN_POINT ( 'NONE',  ( 71.86476928594946401, -59.99999999997545075, 174.6312134016923778 ) ) ;
#47558 = ORIENTED_EDGE ( 'NONE', *, *, #54679, .T. ) ;
#47557 = CONICAL_SURFACE ( 'NONE', #83677, 4.172000000000009479, 0.9599310885968813656 ) ;
#47559 = CARTESIAN_POINT ( 'NONE',  ( 13.50929957260945535, -55.29737542706585884, 23.32445699588452470 ) ) ;
#47560 = CARTESIAN_POINT ( 'NONE',  ( -5.082755093536326818, -18.59375000204838457, 5.082755093536325042 ) ) ;
#47561 = CARTESIAN_POINT ( 'NONE',  ( -4.472135954999583163, -9.726700964873602473, -4.000000000000001776 ) ) ;
#47562 = ORIENTED_EDGE ( 'NONE', *, *, #33390, .F. ) ;
#47563 = CARTESIAN_POINT ( 'NONE',  ( 58.67238219402268840, -4.000000000000000888, 4.898587196589422689E-16 ) ) ;
#47564 = VERTEX_POINT ( 'NONE', #32776 ) ;
#47565 = DIRECTION ( 'NONE',  ( 1.000000000000000000, 1.224606353822377258E-16, 0.000000000000000000 ) ) ;
#47566 = DIRECTION ( 'NONE',  ( 0.000000000000000000, 0.000000000000000000, -1.000000000000000000 ) ) ;
#47568 = AXIS2_PLACEMENT_3D ( 'NONE', #54000, #86420, #79351 ) ;
#47567 = CARTESIAN_POINT ( 'NONE',  ( -103.1916873065907652, -59.99999999999998579, 200.5090983659188169 ) ) ;
#47569 = CARTESIAN_POINT ( 'NONE',  ( 0.000000000000000000, 0.000000000000000000, 0.000000000000000000 ) ) ;
#47570 = CARTESIAN_POINT ( 'NONE',  ( -5.082755093536326818, -29.09375000204838813, 5.082755093536325042 ) ) ;
#47571 = CARTESIAN_POINT ( 'NONE',  ( 46.00000000000000000, 460.1242873147357386, 6.750975842511372171 ) ) ;
#47572 = LINE ( 'NONE', #40552, #5105 ) ;
#47573 = PRESENTATION_STYLE_ASSIGNMENT (( #71326 ) ) ;
#47574 = CARTESIAN_POINT ( 'NONE',  ( -9.999999999999992895, 48.00000000000000000, -86.30899693747680601 ) ) ;
#47575 = CARTESIAN_POINT ( 'NONE',  ( 10.92050665241513840, -10.68475269600504696, 18.23204539070182051 ) ) ;
#47576 = DIRECTION ( 'NONE',  ( 0.000000000000000000, 0.000000000000000000, 1.000000000000000000 ) ) ;
#47577 = CARTESIAN_POINT ( 'NONE',  ( 100.1590866098448629, -60.00000000000002842, 195.6606663522350118 ) ) ;
#47578 = CARTESIAN_POINT ( 'NONE',  ( -37.18009251321940667, -22.20738402244377951, 33.02752658207509739 ) ) ;
#47579 = ORIENTED_EDGE ( 'NONE', *, *, #22249, .T. ) ;
#47580 = CARTESIAN_POINT ( 'NONE',  ( 36.98729712581772588, -18.74392476602471547, 32.19149500795003860 ) ) ;
#47581 = CARTESIAN_POINT ( 'NONE',  ( -2.227375807148842313, -1.734723475976807094E-15, -17.01589776168603407 ) ) ;
#47582 = ORIENTED_EDGE ( 'NONE', *, *, #46916, .T. ) ;
#47583 = DIRECTION ( 'NONE',  ( 0.000000000000000000, 1.000000000000000000, 0.000000000000000000 ) ) ;
#47584 = CARTESIAN_POINT ( 'NONE',  ( -75.63917042766036047, -38.35856568444517478, 175.4764248205101467 ) ) ;
#47585 = ORIENTED_EDGE ( 'NONE', *, *, #24440, .T. ) ;
#47587 = FACE_OUTER_BOUND ( 'NONE', #55814, .T. ) ;
#47586 = CARTESIAN_POINT ( 'NONE',  ( 7.424909431085690237, -5.000000000000000888, -15.55223105906578240 ) ) ;
#47588 = CARTESIAN_POINT ( 'NONE',  ( 15.55441737893109355, 37.11602535008575643, 22.68899775139442099 ) ) ;
#47589 = CARTESIAN_POINT ( 'NONE',  ( 9.830769230769229594, 1.411358822780289120E-15, 0.000000000000000000 ) ) ;
#47590 = CARTESIAN_POINT ( 'NONE',  ( 0.6444792390971975093, 43.23217435222382221, -18.58392088066086600 ) ) ;
#47591 = CARTESIAN_POINT ( 'NONE',  ( -38.33028772603171319, 25.24378019603273415, 13.20968585612151536 ) ) ;
#47592 = CARTESIAN_POINT ( 'NONE',  ( -48.49215721461931139, 15.66554462474931420, -14.43870166537744382 ) ) ;
#47593 = CARTESIAN_POINT ( 'NONE',  ( -2.820573970604164593, -49.57105631822983582, 44.39822767282944227 ) ) ;
#47594 = EDGE_CURVE ( 'NONE', #71772, #37759, #8339, .T. ) ;
#47595 = AXIS2_PLACEMENT_3D ( 'NONE', #80338, #71713, #25763 ) ;
#47596 = CARTESIAN_POINT ( 'NONE',  ( 94.76699447141982091, -60.00000000000000711, 47.33153769421498680 ) ) ;
#47597 = FACE_OUTER_BOUND ( 'NONE', #90264, .T. ) ;
#47598 = AXIS2_PLACEMENT_3D ( 'NONE', #44405, #2862, #61123 ) ;
#47599 = CARTESIAN_POINT ( 'NONE',  ( -5.209797429415269576, 40.00000000002213341, -70.92874401597350698 ) ) ;
#47600 = DIRECTION ( 'NONE',  ( 0.5735764363510462704, 0.8191520442889915765, 0.000000000000000000 ) ) ;
#47601 = ORIENTED_EDGE ( 'NONE', *, *, #166, .F. ) ;
#47602 = CARTESIAN_POINT ( 'NONE',  ( -76.52889981649941831, -29.99999999999171152, -26.83830997453001288 ) ) ;
#47603 = ORIENTED_EDGE ( 'NONE', *, *, #5586, .F. ) ;
#47604 = LINE ( 'NONE', #39010, #86633 ) ;
#47605 = CARTESIAN_POINT ( 'NONE',  ( -16.03938085755613230, 4.451364308023405769, 3.146830695504104547 ) ) ;
#47606 = SURFACE_STYLE_USAGE ( .BOTH. , #64864 ) ;
#47607 = DIRECTION ( 'NONE',  ( 1.150791560227848544E-16, -0.3420201433256727652, 0.9396926207859068736 ) ) ;
#47608 = LINE ( 'NONE', #80503, #40883 ) ;
#47609 = CARTESIAN_POINT ( 'NONE',  ( -7.188101187500001821, -24.87500000204838457, -2.977408999572651371 ) ) ;
#47610 = DIRECTION ( 'NONE',  ( 0.000000000000000000, -1.000000000000000000, 0.000000000000000000 ) ) ;
#47611 = CARTESIAN_POINT ( 'NONE',  ( 0.000000000000000000, 0.000000000000000000, 0.000000000000000000 ) ) ;
#47612 = VERTEX_POINT ( 'NONE', #82358 ) ;
#47614 = EDGE_LOOP ( 'NONE', ( #12596, #85575, #45500 ) ) ;
#47613 = LINE ( 'NONE', #63832, #18476 ) ;
#47615 = CARTESIAN_POINT ( 'NONE',  ( 80.60767953697174448, -39.49744972330380222, 149.7863415175808086 ) ) ;
#47616 = CARTESIAN_POINT ( 'NONE',  ( -37.56673239365971284, 27.88554838446211548, -10.95617127780556466 ) ) ;
#47617 = ORIENTED_EDGE ( 'NONE', *, *, #5781, .F. ) ;
#47618 = CARTESIAN_POINT ( 'NONE',  ( 16.14595037822613932, 12.99999999999999289, 0.000000000000000000 ) ) ;
#47619 = CARTESIAN_POINT ( 'NONE',  ( -14.59153803998622223, 1.704952136599680923, 3.465235867604003150 ) ) ;
#47620 = CARTESIAN_POINT ( 'NONE',  ( -7.188101187500002709, -12.31250000204838635, 2.977408999572647819 ) ) ;
#47621 = CARTESIAN_POINT ( 'NONE',  ( 6.928203230275510549, 30.00000000000000355, -4.000000000000000000 ) ) ;
#47622 = CARTESIAN_POINT ( 'NONE',  ( -38.25590479036647906, -57.69571505705692260, 53.01769594715635492 ) ) ;
#47623 = CARTESIAN_POINT ( 'NONE',  ( 13.68615037905027876, 294.5456273187321017, 1.871922570298397703 ) ) ;
#47624 = CIRCLE ( 'NONE', #76891, 5.000000000000000888 ) ;
#47625 = ORIENTED_EDGE ( 'NONE', *, *, #7815, .T. ) ;
#47626 = FILL_AREA_STYLE ('',( #6111 ) ) ;
#47627 = VECTOR ( 'NONE', #13438, 1000.000000000000000 ) ;
#47628 = CARTESIAN_POINT ( 'NONE',  ( 4.086341046824350620, 138.2878350440129509, 4.999999999999999112 ) ) ;
#47629 = CARTESIAN_POINT ( 'NONE',  ( 22.47385306464369492, 18.64284798592518655, -31.17447444073591356 ) ) ;
#47630 = ADVANCED_FACE ( 'NONE', ( #64594, #40835 ), #16028, .T. ) ;
#47631 =( NAMED_UNIT ( * ) PLANE_ANGLE_UNIT ( ) SI_UNIT ( $, .RADIAN. ) );
#47632 = ORIENTED_EDGE ( 'NONE', *, *, #63720, .F. ) ;
#47633 = CARTESIAN_POINT ( 'NONE',  ( -1.469576158976823947E-15, -10.06250000409677092, 8.000000000000000000 ) ) ;
#47634 = CARTESIAN_POINT ( 'NONE',  ( 0.000000000000000000, 0.000000000000000000, 5.000000000000000000 ) ) ;
#47635 = AXIS2_PLACEMENT_3D ( 'NONE', #75569, #67491, #51815 ) ;
#47636 = CARTESIAN_POINT ( 'NONE',  ( 9.999999999997889688, 15.11700796859310714, 0.7408669144238181348 ) ) ;
#47637 = AXIS2_PLACEMENT_3D ( 'NONE', #69726, #70781, #103676 ) ;
#47638 = CARTESIAN_POINT ( 'NONE',  ( 16.33361799548379523, 1.482358050883964840E-15, 0.000000000000000000 ) ) ;
#47639 = CARTESIAN_POINT ( 'NONE',  ( 2.449293598294706907E-16, 12.00000000000000000, 2.000000000000000000 ) ) ;
#47640 = CARTESIAN_POINT ( 'NONE',  ( 5.290067270632321517, 52.08006895350504095, 6.031152949374479100 ) ) ;
#47641 = APPLICATION_PROTOCOL_DEFINITION ( 'draft international standard', 'automotive_design', 1998, #58288 ) ;
#47642 = CARTESIAN_POINT ( 'NONE',  ( -9.275399896789910059, -13.35898335746451160, 16.51081693063991906 ) ) ;
#47643 = ORIENTED_EDGE ( 'NONE', *, *, #84968, .F. ) ;
#47645 = CONICAL_SURFACE ( 'NONE', #14917, 9.000000000000000000, 0.7853981633974509435 ) ;
#47644 = CARTESIAN_POINT ( 'NONE',  ( -5.000000000000000888, -46.26658367591656429, 42.58845726862488590 ) ) ;
#47646 = CIRCLE ( 'NONE', #20146, 7.500000000000006217 ) ;
#47647 = EDGE_CURVE ( 'NONE', #48268, #18270, #60541, .T. ) ;
#47649 = CARTESIAN_POINT ( 'NONE',  ( -3.463524195881185097, 15.83536129559750805, -6.085255580401768505 ) ) ;
#47648 =( BOUNDED_SURFACE ( )  B_SPLINE_SURFACE ( 3, 2, ( 
 ( #80936, #105746, #81988 ),
 ( #41020, #7566, #65821 ),
 ( #48026, #73901, #61188 ),
 ( #38911, #7047, #32952 ),
 ( #63724, #96609, #15145 ),
 ( #73362, #98184, #14594 ),
 ( #106261, #39446, #105226 ),
 ( #39963, #47506, #80399 ) ),
 .UNSPECIFIED., .F., .F., .F. ) 
 B_SPLINE_SURFACE_WITH_KNOTS ( ( 4, 2, 2, 4 ),
 ( 3, 3 ),
 ( 0.03170918191602133118, 0.03570420671717101924, 0.03770171911774586326, 0.03969923151832070035 ),
 ( 0.000000000000000000, 1.000000000000000000 ),
 .UNSPECIFIED. ) 
 GEOMETRIC_REPRESENTATION_ITEM ( )  RATIONAL_B_SPLINE_SURFACE ( (
 ( 1.000000000000000000, 0.8047781070930545289, 1.000000000000000000),
 ( 1.000000000000000000, 0.8123787894255036779, 1.000000000000000000),
 ( 1.000000000000000000, 0.8190667557155233425, 1.000000000000000000),
 ( 1.000000000000000000, 0.8191933945820393248, 1.000000000000000000),
 ( 1.000000000000000000, 0.8176087340367195200, 1.000000000000000000),
 ( 1.000000000000000000, 0.8122956952721525070, 1.000000000000000000),
 ( 1.000000000000000000, 0.8086308540101730946, 1.000000000000000000),
 ( 1.000000000000000000, 0.8047712493762132491, 1.000000000000000000) ) ) 
 REPRESENTATION_ITEM ( '' )  SURFACE ( )  );
#47650 = PLANE ( 'NONE',  #12289 ) ;
#47651 =( LENGTH_UNIT ( ) NAMED_UNIT ( * ) SI_UNIT ( .MILLI., .METRE. ) );
#47652 = EDGE_CURVE ( 'NONE', #73295, #103730, #35314, .T. ) ;
#47653 = CARTESIAN_POINT ( 'NONE',  ( 0.000000000000000000, 0.000000000000000000, -5.575057142857143155 ) ) ;
#47654 = ORIENTED_EDGE ( 'NONE', *, *, #87921, .F. ) ;
#47655 = CARTESIAN_POINT ( 'NONE',  ( 8.000000000000000000, -9.687500004096769146, 0.000000000000000000 ) ) ;
#47656 = CARTESIAN_POINT ( 'NONE',  ( 98.66545750752896993, -57.62490083480406611, 204.2383384864311040 ) ) ;
#47657 = CARTESIAN_POINT ( 'NONE',  ( 72.65333306677447922, -47.40884695679693550, -22.95069231350860406 ) ) ;
#47658 =( LENGTH_UNIT ( ) NAMED_UNIT ( * ) SI_UNIT ( .MILLI., .METRE. ) );
#47659 = CARTESIAN_POINT ( 'NONE',  ( -16.10103572754771761, 21.87195731844465740, -0.4457938394067768595 ) ) ;
#47660 = CARTESIAN_POINT ( 'NONE',  ( 34.47211195129249717, 489.5752767497880882, 11.69752549375474437 ) ) ;
#47661 = CARTESIAN_POINT ( 'NONE',  ( -74.33330251140726830, -59.99999999999999289, 175.5315321299100901 ) ) ;
#47662 = EDGE_CURVE ( 'NONE', #31480, #105180, #12308, .T. ) ;
#47663 =( NAMED_UNIT ( * ) PLANE_ANGLE_UNIT ( ) SI_UNIT ( $, .RADIAN. ) );
#47664 = LINE ( 'NONE', #28896, #14919 ) ;
#47665 = CARTESIAN_POINT ( 'NONE',  ( 50.18984356158254201, 50.00000000000000000, 38.51389699555568313 ) ) ;
#47666 = AXIS2_PLACEMENT_3D ( 'NONE', #38966, #22269, #13599 ) ;
#47667 = CARTESIAN_POINT ( 'NONE',  ( -84.67480933483595607, -50.19323684364298543, 188.5573917989278243 ) ) ;
#47668 = ORIENTED_EDGE ( 'NONE', *, *, #50411, .F. ) ;
#47669 = CARTESIAN_POINT ( 'NONE',  ( 35.68999143317073219, 432.5319086955427679, 4.688598029357957664 ) ) ;
#47670 = ORIENTED_EDGE ( 'NONE', *, *, #20735, .T. ) ;
#47671 = DIRECTION ( 'NONE',  ( 0.8714291948010992606, 0.000000000000000000, -0.4905213129399249583 ) ) ;
#47672 = CARTESIAN_POINT ( 'NONE',  ( -31.49856340160977908, 312.6924388527738756, -7.915384035900890680 ) ) ;
#47673 = CARTESIAN_POINT ( 'NONE',  ( 41.99899754399194052, 488.0172855231593303, 9.044990669317995113 ) ) ;
#47674 = CARTESIAN_POINT ( 'NONE',  ( 43.00000000000000000, 437.9690125970931831, 14.09127711025711349 ) ) ;
#47675 = ORIENTED_EDGE ( 'NONE', *, *, #81987, .T. ) ;
#47676 = CARTESIAN_POINT ( 'NONE',  ( 19.47229003637610489, 49.99999999999998579, 59.94434553428096990 ) ) ;
#47677 = CARTESIAN_POINT ( 'NONE',  ( 5.799999999999999822, 4.618802153517003184, -8.000000000000000000 ) ) ;
#47678 = CARTESIAN_POINT ( 'NONE',  ( -16.57301948836873251, -1.734723475976807094E-15, -4.453875240786733691 ) ) ;
#47679 = LINE ( 'NONE', #72497, #46262 ) ;
#47680 = ADVANCED_FACE ( 'NONE', ( #100663 ), #51579, .T. ) ;
#47681 = CARTESIAN_POINT ( 'NONE',  ( 89.21410497458975897, -29.99999999999997513, 9.589292377912048693 ) ) ;
#47682 = CARTESIAN_POINT ( 'NONE',  ( -79.72895134235473336, -18.67626752654355116, 125.0978594537113793 ) ) ;
#47683 = ORIENTED_EDGE ( 'NONE', *, *, #97287, .F. ) ;
#47684 = CARTESIAN_POINT ( 'NONE',  ( 46.52147948847155590, -60.00000000000000000, 69.35914673975356948 ) ) ;
#47685 = PRESENTATION_STYLE_ASSIGNMENT (( #45597 ) ) ;
#47686 = CARTESIAN_POINT ( 'NONE',  ( 74.66765723773309560, -57.58775781631299395, 189.6186382585397894 ) ) ;
#47687 = CARTESIAN_POINT ( 'NONE',  ( 27.10511071441197117, 34.47735702144345282, 10.05698433968570704 ) ) ;
#47688 = AXIS2_PLACEMENT_3D ( 'NONE', #67571, #93440, #1191 ) ;
#47689 = CARTESIAN_POINT ( 'NONE',  ( 36.14035709840733546, 304.2251051115202927, 0.1608020814845102231 ) ) ;
#47690 = CARTESIAN_POINT ( 'NONE',  ( 70.89460441624491693, -1.232595164407830946E-29, 4.000000000000007105 ) ) ;
#47691 = ORIENTED_EDGE ( 'NONE', *, *, #93065, .T. ) ;
#47692 = COLOUR_RGB ( '', 0.09019608, 0.27058824, 0.51372549) ;
#47693 = CARTESIAN_POINT ( 'NONE',  ( 7.500000000000000000, 4.330127018922203419, -0.9999999999999974465 ) ) ;
#47695 = CARTESIAN_POINT ( 'NONE',  ( -103.5544495963808913, -45.26538628390532892, 161.0521102863736473 ) ) ;
#47694 = DIRECTION ( 'NONE',  ( 0.000000000000000000, -0.000000000000000000, -1.000000000000000000 ) ) ;
#47696 = CARTESIAN_POINT ( 'NONE',  ( 2.977408999572651815, -20.93750000204838457, 7.188101187500000933 ) ) ;
#47697 = CARTESIAN_POINT ( 'NONE',  ( 58.92761780597729881, 6.856755485862130937E-15, 0.000000000000000000 ) ) ;
#47698 = CARTESIAN_POINT ( 'NONE',  ( 9.948513602187992078, 81.13022056656140535, 1.045942665286136108 ) ) ;
#47699 = FACE_OUTER_BOUND ( 'NONE', #21538, .T. ) ;
#47700 = EDGE_CURVE ( 'NONE', #2917, #32311, #10533, .T. ) ;
#47701 = CARTESIAN_POINT ( 'NONE',  ( -7.500000000000000000, 3.202583086481786356, -7.213046687578396288 ) ) ;
#47702 = FACE_OUTER_BOUND ( 'NONE', #87819, .T. ) ;
#47703 = ORIENTED_EDGE ( 'NONE', *, *, #94511, .T. ) ;
#47704 = CARTESIAN_POINT ( 'NONE',  ( -7.149999999999890221, 41.65000000000012648, -59.82695526680724640 ) ) ;
#47705 = MECHANICAL_DESIGN_GEOMETRIC_PRESENTATION_REPRESENTATION (  '', ( #52878 ), #39119 ) ;
#47707 = CARTESIAN_POINT ( 'NONE',  ( 30.31142205078400309, -25.59748758447105743, 30.73189178319717740 ) ) ;
#47706 = DIRECTION ( 'NONE',  ( -0.000000000000000000, 1.000000000000000000, -0.000000000000000000 ) ) ;
#47708 = CARTESIAN_POINT ( 'NONE',  ( 18.09999999999999787, 1.533819458162526451E-15, 0.000000000000000000 ) ) ;
#47709 = ORIENTED_EDGE ( 'NONE', *, *, #85036, .F. ) ;
#47710 = ORIENTED_EDGE ( 'NONE', *, *, #9543, .T. ) ;
#47711 = AXIS2_PLACEMENT_3D ( 'NONE', #92868, #92334, #101504 ) ;
#47713 = CARTESIAN_POINT ( 'NONE',  ( 1.990040563172386960E-15, 46.21383923812596350, 16.25000000000000000 ) ) ;
#47712 = SURFACE_STYLE_USAGE ( .BOTH. , #44697 ) ;
#47714 = CARTESIAN_POINT ( 'NONE',  ( -10.28624191511830155, -1.200000000000000030E-05, -14.15779740156157018 ) ) ;
#47715 = CARTESIAN_POINT ( 'NONE',  ( 24.34999999999999787, 3.309500000000003439, 4.052968581778167743E-16 ) ) ;
#47716 =( GEOMETRIC_REPRESENTATION_CONTEXT ( 3 ) GLOBAL_UNCERTAINTY_ASSIGNED_CONTEXT ( ( #88198 ) ) GLOBAL_UNIT_ASSIGNED_CONTEXT ( ( #21090, #38316, #4329 ) ) REPRESENTATION_CONTEXT ( 'NONE', 'WORKASPACE' ) );
#47717 = CARTESIAN_POINT ( 'NONE',  ( 4.000000000000000000, 4.898587196589412829E-16, -3.432199999999999918 ) ) ;
#47718 = DIRECTION ( 'NONE',  ( 0.000000000000000000, -1.000000000000000000, 0.000000000000000000 ) ) ;
#47719 = ORIENTED_EDGE ( 'NONE', *, *, #5587, .F. ) ;
#47720 = EDGE_CURVE ( 'NONE', #81108, #18895, #95249, .T. ) ;
#47721 = DIRECTION ( 'NONE',  ( 0.5735764363510462704, 0.8191520442889915765, 0.000000000000000000 ) ) ;
#47722 = CARTESIAN_POINT ( 'NONE',  ( 89.93595484110375082, -30.00000000000008882, 189.8158637124989525 ) ) ;
#47723 = LINE ( 'NONE', #30524, #54833 ) ;
#47724 = CIRCLE ( 'NONE', #25366, 5.000000000000010658 ) ;
#47725 = DIRECTION ( 'NONE',  ( -1.000000000000000000, -1.224606353822377258E-16, -0.000000000000000000 ) ) ;
#47726 = EDGE_CURVE ( 'NONE', #31429, #62903, #104376, .T. ) ;
#47727 = CARTESIAN_POINT ( 'NONE',  ( 0.000000000000000000, 0.000000000000000000, 0.000000000000000000 ) ) ;
#47728 = VERTEX_POINT ( 'NONE', #13767 ) ;
#47729 = ORIENTED_EDGE ( 'NONE', *, *, #41458, .F. ) ;
#47730 = ORIENTED_EDGE ( 'NONE', *, *, #76256, .F. ) ;
#47731 = DIRECTION ( 'NONE',  ( 0.5735764363510557073, -0.8191520442889850262, 1.003171929053516612E-16 ) ) ;
#47732 = DIRECTION ( 'NONE',  ( 0.000000000000000000, -1.000000000000000000, 0.000000000000000000 ) ) ;
#47733 = CARTESIAN_POINT ( 'NONE',  ( 33.09106007554123607, 433.0116111952169717, 24.60471978344146393 ) ) ;
#47734 = CARTESIAN_POINT ( 'NONE',  ( -44.28506098230518262, 335.5159265879102009, -0.1714402822340226062 ) ) ;
#47735 = CARTESIAN_POINT ( 'NONE',  ( -4.296575424418834999, -67.78488758413351434, 13.66189604103251476 ) ) ;
#47736 = DIRECTION ( 'NONE',  ( 1.000000000000000000, -0.000000000000000000, -0.000000000000000000 ) ) ;
#47737 = FACE_OUTER_BOUND ( 'NONE', #70773, .T. ) ;
#47738 = VERTEX_POINT ( 'NONE', #62883 ) ;
#47739 = CARTESIAN_POINT ( 'NONE',  ( -10.12078790316828858, 44.02769531064037523, 12.91599879790107686 ) ) ;
#47740 = VERTEX_POINT ( 'NONE', #47199 ) ;
#47741 = AXIS2_PLACEMENT_3D ( 'NONE', #62242, #3980, #95127 ) ;
#47742 = FACE_OUTER_BOUND ( 'NONE', #28280, .T. ) ;
#47743 = CARTESIAN_POINT ( 'NONE',  ( -39.08667504540946425, 49.99999999999999289, -56.76470588249692639 ) ) ;
#47744 = FILL_AREA_STYLE_COLOUR ( '', #64524 ) ;
#47745 = AXIS2_PLACEMENT_3D ( 'NONE', #96012, #63110, #21617 ) ;
#47746 = CARTESIAN_POINT ( 'NONE',  ( 20.11650669486618881, 1.474610560812782335E-15, 0.000000000000000000 ) ) ;
#47747 = CARTESIAN_POINT ( 'NONE',  ( 69.23840392680455125, -29.06012857090818002, 93.48888568600646920 ) ) ;
#47748 = EDGE_CURVE ( 'NONE', #15547, #81100, #24354, .T. ) ;
#47749 = VERTEX_POINT ( 'NONE', #78510 ) ;
#47750 = CARTESIAN_POINT ( 'NONE',  ( 41.75487894852329163, 464.7989896699401129, 15.72965077414808732 ) ) ;
#47751 = CIRCLE ( 'NONE', #85657, 6.499999999999999112 ) ;
#47752 = CARTESIAN_POINT ( 'NONE',  ( 0.06682554136338431094, -6.264794173742282091, -2.149058192116895416 ) ) ;
#47753 = ORIENTED_EDGE ( 'NONE', *, *, #2015, .F. ) ;
#47754 = CARTESIAN_POINT ( 'NONE',  ( 46.89590902281800311, 18.03207604452820689, 16.16381118462976474 ) ) ;
#47755 = VECTOR ( 'NONE', #9234, 1000.000000000000000 ) ;
#47756 = CARTESIAN_POINT ( 'NONE',  ( 0.000000000000000000, 67.00000000000002842, 0.000000000000000000 ) ) ;
#47757 = CARTESIAN_POINT ( 'NONE',  ( 4.898587196589412829E-16, -30.31250000409677270, -8.000000000000000000 ) ) ;
#47758 = CARTESIAN_POINT ( 'NONE',  ( 2.094395098902538166, -3.000000000000000000, -8.000000000000000000 ) ) ;
#47759 = CARTESIAN_POINT ( 'NONE',  ( 86.41025636765816387, -53.78809460387265773, 192.3578921812466831 ) ) ;
#47760 = CIRCLE ( 'NONE', #59888, 4.000000000000000888 ) ;
#47761 = UNCERTAINTY_MEASURE_WITH_UNIT (LENGTH_MEASURE( 1.000000000000000082E-05 ), #41269, 'distance_accuracy_value', 'NONE');
#47762 = CARTESIAN_POINT ( 'NONE',  ( 9.989113211954165905, 33.97299273548994591, 0.5334031035449001701 ) ) ;
#47763 = DIRECTION ( 'NONE',  ( 0.000000000000000000, -0.8273160954975392611, 0.5617366626193331935 ) ) ;
#47764 =( NAMED_UNIT ( * ) PLANE_ANGLE_UNIT ( ) SI_UNIT ( $, .RADIAN. ) );
#47765 = ORIENTED_EDGE ( 'NONE', *, *, #73923, .F. ) ;
#47766 = CARTESIAN_POINT ( 'NONE',  ( 7.000000000000000000, 0.000000000000000000, -8.125150395352576993 ) ) ;
#47767 = CARTESIAN_POINT ( 'NONE',  ( 33.15869397692891596, -60.00000000000001421, 44.95690229595550136 ) ) ;
#47768 = CARTESIAN_POINT ( 'NONE',  ( -91.37582729904079315, -29.99999999999999645, 190.6461204354261270 ) ) ;
#47769 = EDGE_CURVE ( 'NONE', #66563, #46054, #50181, .T. ) ;
#47770 = VECTOR ( 'NONE', #63901, 1000.000000000000000 ) ;
#47771 = CARTESIAN_POINT ( 'NONE',  ( -39.29284405225726573, 485.1982890239684707, -4.348287318897845921 ) ) ;
#47772 = CIRCLE ( 'NONE', #96002, 4.000000000000001776 ) ;
#47773 = CARTESIAN_POINT ( 'NONE',  ( 52.18313839522158304, -57.67658158394408474, 83.21036237335373187 ) ) ;
#47774 = EDGE_CURVE ( 'NONE', #56514, #102690, #49390, .T. ) ;
#47775 = CARTESIAN_POINT ( 'NONE',  ( 6.641837668257387861, 41.74662779905570176, -59.04567176600482981 ) ) ;
#47776 = DIRECTION ( 'NONE',  ( 1.000000000000000000, 0.000000000000000000, 0.000000000000000000 ) ) ;
#47777 = CARTESIAN_POINT ( 'NONE',  ( -13.00000000000003730, -10.00000000000000888, 0.000000000000000000 ) ) ;
#47778 = AXIS2_PLACEMENT_3D ( 'NONE', #79471, #10614, #26859 ) ;
#47779 = CARTESIAN_POINT ( 'NONE',  ( -8.335663544843971096, -60.00000000000001421, 39.63523635428892788 ) ) ;
#47780 =( GEOMETRIC_REPRESENTATION_CONTEXT ( 3 ) GLOBAL_UNCERTAINTY_ASSIGNED_CONTEXT ( ( #11440 ) ) GLOBAL_UNIT_ASSIGNED_CONTEXT ( ( #73649, #72599, #97393 ) ) REPRESENTATION_CONTEXT ( 'NONE', 'WORKASPACE' ) );
#47781 = VECTOR ( 'NONE', #103536, 1000.000000000000114 ) ;
#47782 = STYLED_ITEM ( 'NONE', ( #22545 ), #37891 ) ;
#47783 = CARTESIAN_POINT ( 'NONE',  ( 11.89481087122913294, 16.74404509406153352, 9.279772923664232565 ) ) ;
#47784 = CARTESIAN_POINT ( 'NONE',  ( -85.99000842721079607, -57.44596555551432715, 193.1195461926678831 ) ) ;
#47785 = EDGE_LOOP ( 'NONE', ( #8841, #50174, #6683, #13315, #93467, #26507 ) ) ;
#47786 = CARTESIAN_POINT ( 'NONE',  ( 17.49999999999901235, 48.51938947814463177, 62.60970113050974817 ) ) ;
#47787 = CARTESIAN_POINT ( 'NONE',  ( -14.61251300444708789, -42.95777107779967707, 31.17356395705397532 ) ) ;
#47788 = VECTOR ( 'NONE', #19226, 1000.000000000000000 ) ;
#47790 = DIRECTION ( 'NONE',  ( 0.000000000000000000, -1.000000000000000000, 0.000000000000000000 ) ) ;
#47789 = DIRECTION ( 'NONE',  ( -1.000000000000000000, -1.224606353822377258E-16, -0.000000000000000000 ) ) ;
#47791 = EDGE_CURVE ( 'NONE', #2944, #37934, #86110, .T. ) ;
#47792 = ORIENTED_EDGE ( 'NONE', *, *, #8110, .T. ) ;
#47793 = DIRECTION ( 'NONE',  ( -1.000000000000000000, -0.000000000000000000, -0.000000000000000000 ) ) ;
#47794 = MECHANICAL_DESIGN_GEOMETRIC_PRESENTATION_REPRESENTATION (  '', ( #11621 ), #13389 ) ;
#47795 = CARTESIAN_POINT ( 'NONE',  ( -5.538604458984424994, -4.999999999982783550, -16.33373421806852122 ) ) ;
#47796 = CARTESIAN_POINT ( 'NONE',  ( -13.93041290236829965, 43.14806440719855374, -91.34884852387233423 ) ) ;
#47797 = CARTESIAN_POINT ( 'NONE',  ( 7.320805580757752118, 41.41776788117373798, -59.82972163162600054 ) ) ;
#47798 = CARTESIAN_POINT ( 'NONE',  ( 64.13793778944149437, -60.00000000000001421, 114.9505950962200984 ) ) ;
#47799 = EDGE_CURVE ( 'NONE', #78892, #93357, #3710, .T. ) ;
#47800 = CONICAL_SURFACE ( 'NONE', #77084, 6.499999999999999112, 1.047197551196600296 ) ;
#47801 = CARTESIAN_POINT ( 'NONE',  ( -2.637755229554568666E-21, 53.39766064372320642, -10.24999999999999822 ) ) ;
#47802 = ORIENTED_EDGE ( 'NONE', *, *, #43782, .T. ) ;
#47803 = LINE ( 'NONE', #6283, #75669 ) ;
#47804 = CARTESIAN_POINT ( 'NONE',  ( -35.45036406932566564, 436.3203772529605544, 5.179456583033978490 ) ) ;
#47806 = DIRECTION ( 'NONE',  ( 0.000000000000000000, 0.000000000000000000, 1.000000000000000000 ) ) ;
#47805 = CARTESIAN_POINT ( 'NONE',  ( 35.98705420554111356, -30.00000000000000355, 43.73599804831894033 ) ) ;
#47807 = SURFACE_SIDE_STYLE ('',( #105008 ) ) ;
#47808 = VERTEX_POINT ( 'NONE', #63424 ) ;
#47810 = CARTESIAN_POINT ( 'NONE',  ( -24.31407123536968840, 306.6633020399330576, 10.34267655207518644 ) ) ;
#47809 = STYLED_ITEM ( 'NONE', ( #82580 ), #102368 ) ;
#47811 = ORIENTED_EDGE ( 'NONE', *, *, #61911, .T. ) ;
#47812 = CARTESIAN_POINT ( 'NONE',  ( 21.05814741031886328, 305.0197153841863269, 9.972911420270587968 ) ) ;
#47813 = CARTESIAN_POINT ( 'NONE',  ( 44.83349330513380693, 4.000000000000003553, 0.000000000000000000 ) ) ;
#47814 = DIRECTION ( 'NONE',  ( -1.000000000000000000, -1.224606353822377258E-16, -0.000000000000000000 ) ) ;
#47816 = EDGE_CURVE ( 'NONE', #103256, #24472, #28965, .T. ) ;
#47815 = ORIENTED_EDGE ( 'NONE', *, *, #96032, .T. ) ;
#47817 = CARTESIAN_POINT ( 'NONE',  ( -4.852941176470598528, -3.000000000000002665, -70.80672828634229177 ) ) ;
#47818 = SURFACE_SIDE_STYLE ('',( #6298 ) ) ;
#47819 = CARTESIAN_POINT ( 'NONE',  ( -92.71863003665913538, -60.00000000000486722, 204.8833018290717405 ) ) ;
#47820 = CARTESIAN_POINT ( 'NONE',  ( 5.817833032102705637, -1.364745674334431280, -6.500000000000000888 ) ) ;
#47821 = CARTESIAN_POINT ( 'NONE',  ( 87.50920607001037865, -60.00000000000000000, 201.2124321505406783 ) ) ;
#47822 = DIRECTION ( 'NONE',  ( -0.000000000000000000, 0.000000000000000000, 1.000000000000000000 ) ) ;
#47823 = DIRECTION ( 'NONE',  ( -1.000000000000000000, -1.224606353822377258E-16, -0.000000000000000000 ) ) ;
#47825 = CARTESIAN_POINT ( 'NONE',  ( 8.025689105212569174, -22.06735756619769262, 27.56016688982502316 ) ) ;
#47824 = CARTESIAN_POINT ( 'NONE',  ( -106.2142031390243488, -14.21045842199427867, 184.2056779555663582 ) ) ;
#47827 = CARTESIAN_POINT ( 'NONE',  ( 101.4591949053181850, -38.00000000000000711, 151.1652513569568441 ) ) ;
#47826 = UNCERTAINTY_MEASURE_WITH_UNIT (LENGTH_MEASURE( 1.000000000000000082E-05 ), #26078, 'distance_accuracy_value', 'NONE');
#47828 = DIRECTION ( 'NONE',  ( 0.000000000000000000, -1.000000000000000000, 0.000000000000000000 ) ) ;
#47829 = AXIS2_PLACEMENT_3D ( 'NONE', #78622, #77585, #87275 ) ;
#47830 = CARTESIAN_POINT ( 'NONE',  ( -46.27878468182461091, -36.07324587582905195, 44.25640521768517743 ) ) ;
#47831 = CARTESIAN_POINT ( 'NONE',  ( 33.09999999999999432, -3.309499999999999886, 4.475777889183790779E-16 ) ) ;
#47832 = ORIENTED_EDGE ( 'NONE', *, *, #46795, .T. ) ;
#47833 = FACE_OUTER_BOUND ( 'NONE', #59184, .T. ) ;
#47834 = CYLINDRICAL_SURFACE ( 'NONE', #68058, 1.000000000000000888 ) ;
#47835 = CARTESIAN_POINT ( 'NONE',  ( 0.5805565836007654523, 7.505553499465139389, 1.865978384307260116E-16 ) ) ;
#47836 = CARTESIAN_POINT ( 'NONE',  ( 11.89663243729389386, 304.5916485594502205, -10.05529748560153358 ) ) ;
#47837 = DIRECTION ( 'NONE',  ( -1.000000000000000000, -1.224606353822377258E-16, -0.000000000000000000 ) ) ;
#47838 = ORIENTED_EDGE ( 'NONE', *, *, #66029, .T. ) ;
#47839 = CARTESIAN_POINT ( 'NONE',  ( 4.551587301587291634, -48.79941684889506348, 104.4018401814738013 ) ) ;
#47840 = AXIS2_PLACEMENT_3D ( 'NONE', #18219, #67290, #52677 ) ;
#47841 = ORIENTED_EDGE ( 'NONE', *, *, #97861, .F. ) ;
#47842 = CARTESIAN_POINT ( 'NONE',  ( 103.4783626894312363, -29.99999999999954170, 197.0598667280581253 ) ) ;
#47843 = CARTESIAN_POINT ( 'NONE',  ( 46.00000000000000711, 461.2856817983021074, 8.847499008863380254 ) ) ;
#47844 = CARTESIAN_POINT ( 'NONE',  ( 5.711454417755754243, 41.98245396441496524, -59.41190390763706830 ) ) ;
#47845 = CARTESIAN_POINT ( 'NONE',  ( -28.12328997684540610, 24.73290587908618932, -14.06164498842269772 ) ) ;
#47846 = CARTESIAN_POINT ( 'NONE',  ( 94.04323099157159049, -30.00000000000000000, 112.2223748969013002 ) ) ;
#47847 = EDGE_CURVE ( 'NONE', #80344, #3777, #53193, .T. ) ;
#47848 = CARTESIAN_POINT ( 'NONE',  ( -20.20168668923396993, 303.8505198094663911, 9.936726593992792900 ) ) ;
#47849 = EDGE_LOOP ( 'NONE', ( #17311, #60751, #26314, #41382, #68226 ) ) ;
#47850 = B_SPLINE_CURVE_WITH_KNOTS ( 'NONE', 3,
 ( #46565, #14176, #30949, #46044, #13117, #37987, #21270, #78928 ),
 .UNSPECIFIED., .F., .F.,
 ( 4, 2, 2, 4 ),
 ( 2.359479019930958006E-17, 0.002589981853911959252, 0.003884972780867916760, 0.005179963707823875135 ),
 .UNSPECIFIED. ) ;
#47851 = ORIENTED_EDGE ( 'NONE', *, *, #88966, .F. ) ;
#47852 = ORIENTED_EDGE ( 'NONE', *, *, #37842, .T. ) ;
#47853 = CARTESIAN_POINT ( 'NONE',  ( -32.94994279514429536, 464.9549361168403721, 15.12478419439328547 ) ) ;
#47854 = CARTESIAN_POINT ( 'NONE',  ( 21.98993715557173800, 25.96775721187310637, 31.66727678396639334 ) ) ;
#47855 = TOROIDAL_SURFACE ( 'NONE', #34133, 8.000000000000000000, 4.000000000000000000 ) ;
#47856 = CARTESIAN_POINT ( 'NONE',  ( -37.88504238421005965, 463.4171042825123550, 19.90923349044086166 ) ) ;
#47857 = EDGE_CURVE ( 'NONE', #41582, #89804, #31282, .T. ) ;
#47858 = VERTEX_POINT ( 'NONE', #22444 ) ;
#47859 = CARTESIAN_POINT ( 'NONE',  ( -16.05785784214753775, 4.775831776487168945, 3.710403933803116949 ) ) ;
#47860 = ORIENTED_EDGE ( 'NONE', *, *, #5219, .F. ) ;
#47861 = FACE_OUTER_BOUND ( 'NONE', #18116, .T. ) ;
#47862 = CARTESIAN_POINT ( 'NONE',  ( 86.25238321531877261, -38.62902508625902698, 199.1927999813084398 ) ) ;
#47863 = CARTESIAN_POINT ( 'NONE',  ( 10.93132941745003350, 11.18092413548305153, 9.853954356400903336 ) ) ;
#47864 = CARTESIAN_POINT ( 'NONE',  ( 83.26452227477953727, -37.81628373900264961, -6.777217245169891768 ) ) ;
#47865 = CARTESIAN_POINT ( 'NONE',  ( 86.35483434040011730, -38.00000000000002842, 187.4088181658582357 ) ) ;
#47866 = TOROIDAL_SURFACE ( 'NONE', #104692, 10.00000000000000000, 0.5000000000000000000 ) ;
#47867 = CARTESIAN_POINT ( 'NONE',  ( 39.29144825744032943, 326.5384315043369838, 17.65690345107428172 ) ) ;
#47868 = SURFACE_SIDE_STYLE ('',( #40323 ) ) ;
#47869 = DIRECTION ( 'NONE',  ( -1.000000000000000000, 0.000000000000000000, 0.000000000000000000 ) ) ;
#47870 = EDGE_CURVE ( 'NONE', #95088, #85724, #21381, .T. ) ;
#47871 = DIRECTION ( 'NONE',  ( -0.000000000000000000, 1.000000000000000000, 0.000000000000000000 ) ) ;
#47872 = CARTESIAN_POINT ( 'NONE',  ( -4.526657684027646233, -47.90665221903876869, 103.5746540667394697 ) ) ;
#47873 = CARTESIAN_POINT ( 'NONE',  ( 0.000000000000000000, 0.000000000000000000, -2.868028571428571372 ) ) ;
#47874 = CARTESIAN_POINT ( 'NONE',  ( 7.500000000000007105, -4.999999999999999112, -68.91429205785459544 ) ) ;
#47875 = DIRECTION ( 'NONE',  ( 0.000000000000000000, 0.000000000000000000, 1.000000000000000000 ) ) ;
#47876 = EDGE_LOOP ( 'NONE', ( #103209, #16521, #15499, #54244 ) ) ;
#47877 = CARTESIAN_POINT ( 'NONE',  ( -42.69811214730273718, 434.9611672192514220, 18.34625614733213439 ) ) ;
#47879 = CARTESIAN_POINT ( 'NONE',  ( -25.54576300332514904, 305.0804997338725002, 10.43511780733714289 ) ) ;
#47878 = DIRECTION ( 'NONE',  ( 1.000000000000000000, 0.000000000000000000, 0.000000000000000000 ) ) ;
#47880 = CARTESIAN_POINT ( 'NONE',  ( 63.56127108291158123, 6.975173280561618775E-15, 0.000000000000000000 ) ) ;
#47881 = CARTESIAN_POINT ( 'NONE',  ( 87.14793098496349444, -38.00000000001091394, 189.0872956505646414 ) ) ;
#47882 = CARTESIAN_POINT ( 'NONE',  ( 5.656854249492380582, -13.81249999999999112, -5.656854249492379694 ) ) ;
#47883 = CARTESIAN_POINT ( 'NONE',  ( 23.50650070960475091, -28.00707568674144810, 37.72505729721246581 ) ) ;
#47884 =( NAMED_UNIT ( * ) PLANE_ANGLE_UNIT ( ) SI_UNIT ( $, .RADIAN. ) );
#47885 = EDGE_LOOP ( 'NONE', ( #5460, #42886, #95604, #37182, #99813, #47851 ) ) ;
#47886 = CARTESIAN_POINT ( 'NONE',  ( 84.86246358733825446, -42.95551756591085990, 185.2907791911740105 ) ) ;
#47887 = EDGE_CURVE ( 'NONE', #72001, #63698, #17493, .T. ) ;
#47888 = VECTOR ( 'NONE', #71725, 1000.000000000000000 ) ;
#47889 = PRESENTATION_STYLE_ASSIGNMENT (( #58117 ) ) ;
#47890 = CARTESIAN_POINT ( 'NONE',  ( 4.441657994896950790, -1.157544474175618676, 104.3851447015617708 ) ) ;
#47891 = EDGE_LOOP ( 'NONE', ( #95218, #61536, #78308, #88703 ) ) ;
#47892 = CARTESIAN_POINT ( 'NONE',  ( 93.83829941600403401, -57.67411610650783871, 13.07459177711520937 ) ) ;
#47893 = CARTESIAN_POINT ( 'NONE',  ( 36.59119455513890529, 438.2489652597744225, 3.879698295689091747 ) ) ;
#47894 = CARTESIAN_POINT ( 'NONE',  ( 37.33349330513379982, 1.593028355512270962E-15, 0.000000000000000000 ) ) ;
#47895 = DIRECTION ( 'NONE',  ( 0.000000000000000000, 0.000000000000000000, 1.000000000000000000 ) ) ;
#47896 = ADVANCED_FACE ( 'NONE', ( #37575 ), #70440, .T. ) ;
#47897 = VECTOR ( 'NONE', #104848, 1000.000000000000000 ) ;
#47898 = CARTESIAN_POINT ( 'NONE',  ( -58.10800684958269358, -37.99999999999999289, 66.73714291064102611 ) ) ;
#47899 = CARTESIAN_POINT ( 'NONE',  ( 4.175893272575727622, -4.999999999998865796, -7.137815226411304614 ) ) ;
#47900 = CARTESIAN_POINT ( 'NONE',  ( 42.61650669486618881, 1.474610560812782335E-15, 0.000000000000000000 ) ) ;
#47901 = EDGE_CURVE ( 'NONE', #101241, #59097, #13239, .T. ) ;
#47902 = CONICAL_SURFACE ( 'NONE', #15186, 4.172000000000001485, 0.9599310885968750373 ) ;
#47904 = LINE ( 'NONE', #98060, #105032 ) ;
#47903 = CARTESIAN_POINT ( 'NONE',  ( 7.500000000000000888, -3.000671055698259870, -20.99923901233272971 ) ) ;
#47905 = ORIENTED_EDGE ( 'NONE', *, *, #93960, .F. ) ;
#47906 = CARTESIAN_POINT ( 'NONE',  ( 9.497389752372439986, 295.1492747691102636, -10.04143169208125208 ) ) ;
#47907 = CARTESIAN_POINT ( 'NONE',  ( -16.48411172411860903, 43.52942502979619377, -6.657797401562040918 ) ) ;
#47908 = CARTESIAN_POINT ( 'NONE',  ( 5.290067270632161645, -1.200000000000000030E-05, -7.281152949374595451 ) ) ;
#47909 = CARTESIAN_POINT ( 'NONE',  ( 69.92761780597730592, 6.856755485862130937E-15, 0.000000000000000000 ) ) ;
#47910 = CARTESIAN_POINT ( 'NONE',  ( -83.30746707032521670, -37.99999999999999289, -6.324111559126246895 ) ) ;
#47911 = ORIENTED_EDGE ( 'NONE', *, *, #99775, .F. ) ;
#47912 = CARTESIAN_POINT ( 'NONE',  ( 5.819846122303832914, -4.937269551422636127, -4.448398286273207880 ) ) ;
#47913 = CARTESIAN_POINT ( 'NONE',  ( 0.000000000000000000, 6.928203230275505220, -4.000000000000007994 ) ) ;
#47914 = CARTESIAN_POINT ( 'NONE',  ( 5.093234209761996034, -62.55532226535091667, 3.176141468578046023 ) ) ;
#47916 = CARTESIAN_POINT ( 'NONE',  ( -31.16334379427010859, -21.77022426646608366, -28.58710611576712068 ) ) ;
#47915 = CARTESIAN_POINT ( 'NONE',  ( -13.50000000000000000, -7.794228634059985339, -11.79422863405993382 ) ) ;
#47917 = EDGE_CURVE ( 'NONE', #41052, #20613, #91557, .T. ) ;
#47918 = ORIENTED_EDGE ( 'NONE', *, *, #5247, .F. ) ;
#47919 = MECHANICAL_DESIGN_GEOMETRIC_PRESENTATION_REPRESENTATION (  '', ( #106526 ), #22187 ) ;
#47920 = AXIS2_PLACEMENT_3D ( 'NONE', #65491, #72510, #40671 ) ;
#47921 = EDGE_LOOP ( 'NONE', ( #96345, #52838, #60458, #99056, #61463, #24458 ) ) ;
#47922 = AXIS2_PLACEMENT_3D ( 'NONE', #66324, #57157, #90070 ) ;
#47923 =( NAMED_UNIT ( * ) PLANE_ANGLE_UNIT ( ) SI_UNIT ( $, .RADIAN. ) );
#47924 = CARTESIAN_POINT ( 'NONE',  ( -4.639619758716991171, 4.826867782832367837, -0.1499059597315244019 ) ) ;
#47925 = CARTESIAN_POINT ( 'NONE',  ( -92.37071800302067004, -60.00000000000000000, 0.5499908112625699896 ) ) ;
#47926 = ORIENTED_EDGE ( 'NONE', *, *, #32464, .F. ) ;
#47927 = CARTESIAN_POINT ( 'NONE',  ( -8.162336134653097375, 41.33266196706049556, -58.07023218170494516 ) ) ;
#47928 = DIRECTION ( 'NONE',  ( 0.000000000000000000, 0.000000000000000000, -1.000000000000000000 ) ) ;
#47929 = AXIS2_PLACEMENT_3D ( 'NONE', #64368, #97241, #23386 ) ;
#47930 = CARTESIAN_POINT ( 'NONE',  ( 98.06839251664504786, -45.26758170594511199, 193.7448716299151954 ) ) ;
#47932 = CARTESIAN_POINT ( 'NONE',  ( 8.099999999999999645, 3.752776749732565253, 6.499999999999997335 ) ) ;
#47931 = CARTESIAN_POINT ( 'NONE',  ( 12.61650669486618881, 0.000000000000000000, 4.000000000000000888 ) ) ;
#47933 = CARTESIAN_POINT ( 'NONE',  ( -80.45966997233487916, -53.39463783365103922, 168.0513147114344861 ) ) ;
#47934 = VERTEX_POINT ( 'NONE', #95774 ) ;
#47935 = EDGE_LOOP ( 'NONE', ( #32486, #50843, #53688, #49579, #13780 ) ) ;
#47936 = ORIENTED_EDGE ( 'NONE', *, *, #32316, .T. ) ;
#47937 = DIRECTION ( 'NONE',  ( 0.000000000000000000, 0.000000000000000000, -1.000000000000000000 ) ) ;
#47938 = CARTESIAN_POINT ( 'NONE',  ( -5.000000000000000000, -14.43521912202174207, 12.17944458656183571 ) ) ;
#47939 = CARTESIAN_POINT ( 'NONE',  ( 0.000000000000000000, 41.79151656018385097, 0.000000000000000000 ) ) ;
#47940 = VERTEX_POINT ( 'NONE', #56875 ) ;
#47941 = CARTESIAN_POINT ( 'NONE',  ( 0.000000000000000000, -50.00000000000000000, 112.0000000000000000 ) ) ;
#47942 = CARTESIAN_POINT ( 'NONE',  ( -110.0428892116504755, 17.51648154115788358, -55.02144460582525198 ) ) ;
#47943 = CIRCLE ( 'NONE', #42811, 4.000000000000001776 ) ;
#47944 = CARTESIAN_POINT ( 'NONE',  ( -9.999999999999998224, 15.23416508905776112, -0.7060372491550682694 ) ) ;
#47945 = CARTESIAN_POINT ( 'NONE',  ( -76.22482491972903063, -57.54008153533397518, 193.6369246664269781 ) ) ;
#47946 = CARTESIAN_POINT ( 'NONE',  ( -4.590682673078522846, -66.06791757312157642, 3.864023243754608927 ) ) ;
#47947 = CARTESIAN_POINT ( 'NONE',  ( -28.60676286294164328, 48.00000000000000711, 58.59397763554174077 ) ) ;
#47948 = DIRECTION ( 'NONE',  ( 0.5564727496918402405, -0.8308658609248562588, -0.000000000000000000 ) ) ;
#47949 = CARTESIAN_POINT ( 'NONE',  ( -36.87655955837857391, 437.4206410680704948, 3.315070609669444224 ) ) ;
#47950 = CARTESIAN_POINT ( 'NONE',  ( -2.727034095388735757, -14.21045842199435860, -37.36840973699904822 ) ) ;
#47951 = CARTESIAN_POINT ( 'NONE',  ( 6.243930039575695118E-05, -60.00000000000000000, 42.00000000000000711 ) ) ;
#47952 = B_SPLINE_CURVE_WITH_KNOTS ( 'NONE', 3,
 ( #90701, #42672, #1666, #75571, #24403, #83132 ),
 .UNSPECIFIED., .F., .F.,
 ( 4, 2, 4 ),
 ( 2.380729205304141141E-07, 0.003943479449179690573, 0.007886720825438852528 ),
 .UNSPECIFIED. ) ;
#47953 = CARTESIAN_POINT ( 'NONE',  ( -51.44312181940702544, -53.37577997994360146, 58.22593905968521000 ) ) ;
#47954 = AXIS2_PLACEMENT_3D ( 'NONE', #38607, #39663, #80093 ) ;
#47955 = CARTESIAN_POINT ( 'NONE',  ( 3.585913242228626174, 19.64393302524088725, -6.012923278400477578 ) ) ;
#47956 = ORIENTED_EDGE ( 'NONE', *, *, #79742, .T. ) ;
#47957 = CARTESIAN_POINT ( 'NONE',  ( -100.7084081391693076, -60.27494346565931238, 195.3574602886342007 ) ) ;
#47958 = CARTESIAN_POINT ( 'NONE',  ( -1.959911964389828398, 298.2559866373201203, -10.00257402834333931 ) ) ;
#47959 = MECHANICAL_DESIGN_GEOMETRIC_PRESENTATION_REPRESENTATION (  '', ( #56586 ), #91043 ) ;
#47960 = ORIENTED_EDGE ( 'NONE', *, *, #11413, .T. ) ;
#47961 = CARTESIAN_POINT ( 'NONE',  ( 19.17148997711927905, 49.74984135236479688, 61.61528624114195196 ) ) ;
#47962 = CARTESIAN_POINT ( 'NONE',  ( 106.5345532972019953, -38.36891180064773721, 195.6038345425867817 ) ) ;
#47963 = CARTESIAN_POINT ( 'NONE',  ( 48.28161701412305717, 14.38519811849424990, 16.83766359355561093 ) ) ;
#47964 = CARTESIAN_POINT ( 'NONE',  ( -8.813378757748752790, 294.6780630559476890, 9.900069857271436291 ) ) ;
#47965 = DIRECTION ( 'NONE',  ( -1.000000000000000000, -1.224606353822377258E-16, -0.000000000000000000 ) ) ;
#47966 = CARTESIAN_POINT ( 'NONE',  ( 84.65202442565809804, -30.00000000000000000, 167.0145454972611390 ) ) ;
#47967 =( BOUNDED_CURVE ( )  B_SPLINE_CURVE ( 2, ( #88328, #105554, #41351 ),
 .UNSPECIFIED., .F., .F. ) 
 B_SPLINE_CURVE_WITH_KNOTS ( ( 3, 3 ),
 ( 0.000000000000000000, 1.000000000000000000 ),
 .UNSPECIFIED. ) 
 CURVE ( )  GEOMETRIC_REPRESENTATION_ITEM ( )  RATIONAL_B_SPLINE_CURVE ( ( 1.000000000000000000, 1.857142857142858317, 1.000000000000000000 ) ) 
 REPRESENTATION_ITEM ( '' )  );
#47968 = CARTESIAN_POINT ( 'NONE',  ( 11.89108997990703109, 303.5914306638122753, -10.05534273549331559 ) ) ;
#47969 = CARTESIAN_POINT ( 'NONE',  ( 37.38602481900366570, 490.8442832704907914, 12.40593855171325899 ) ) ;
#47970 = CARTESIAN_POINT ( 'NONE',  ( 0.000000000000000000, 0.000000000000000000, -7.259124522925831435 ) ) ;
#47971 = EDGE_CURVE ( 'NONE', #33707, #27454, #49311, .T. ) ;
#47972 = LINE ( 'NONE', #96026, #84467 ) ;
#47973 = EDGE_CURVE ( 'NONE', #44884, #37257, #69160, .T. ) ;
#47974 = AXIS2_PLACEMENT_3D ( 'NONE', #67452, #90117, #83089 ) ;
#47975 = ORIENTED_EDGE ( 'NONE', *, *, #2619, .F. ) ;
#47976 = ORIENTED_EDGE ( 'NONE', *, *, #73557, .F. ) ;
#47977 = CARTESIAN_POINT ( 'NONE',  ( 49.28648764494346324, -56.82522282173033545, 55.29322352173170430 ) ) ;
#47978 = CARTESIAN_POINT ( 'NONE',  ( 6.348226085585078948, 41.72645248587730293, -58.84140401153305788 ) ) ;
#47979 = DIRECTION ( 'NONE',  ( -2.168404344971008868E-17, 1.000000000000000000, 0.000000000000000000 ) ) ;
#47980 = ADVANCED_FACE ( 'NONE', ( #40702 ), #23495, .T. ) ;
#47981 = CARTESIAN_POINT ( 'NONE',  ( -109.5635314813388845, -38.35614484551107495, 188.1144259547864692 ) ) ;
#47982 = EDGE_LOOP ( 'NONE', ( #68397, #16869, #16187, #1419 ) ) ;
#47983 = CARTESIAN_POINT ( 'NONE',  ( 92.04832879187223682, -38.35408280619313359, 35.20174921906648535 ) ) ;
#47984 = CARTESIAN_POINT ( 'NONE',  ( 11.09863704574016374, 8.438406359958083414, -9.825331742445492011 ) ) ;
#47985 = CARTESIAN_POINT ( 'NONE',  ( 7.898971854500428100E-15, 50.50000000000000000, -64.50000000000000000 ) ) ;
#47986 = CARTESIAN_POINT ( 'NONE',  ( 13.50000000000000355, -1.317096457811609111, -1.029992063861229212E-15 ) ) ;
#47987 = CARTESIAN_POINT ( 'NONE',  ( 103.3874261300967135, -45.28277477373939064, 158.7075077770578559 ) ) ;
#47988 = DIRECTION ( 'NONE',  ( -1.000000000000000000, -1.224606353822377258E-16, -0.000000000000000000 ) ) ;
#47989 = EDGE_CURVE ( 'NONE', #59570, #96544, #18696, .T. ) ;
#47990 = CARTESIAN_POINT ( 'NONE',  ( -34.05318764567596190, 330.1458591810355188, -3.797486262497478116 ) ) ;
#47991 = CARTESIAN_POINT ( 'NONE',  ( 82.42421628608209971, 1.030564683017419500E-14, 0.000000000000000000 ) ) ;
#47992 = CARTESIAN_POINT ( 'NONE',  ( 12.49999999999999822, -4.999999999999999112, -34.12705337364891278 ) ) ;
#47993 = CARTESIAN_POINT ( 'NONE',  ( 100.0145631082506128, -60.00000000000001421, 201.8807573114297895 ) ) ;
#47994 = CIRCLE ( 'NONE', #42858, 8.000000000000000000 ) ;
#47995 = EDGE_CURVE ( 'NONE', #36994, #92586, #36462, .T. ) ;
#47996 = CARTESIAN_POINT ( 'NONE',  ( -15.50010513532795642, 34.90187412562523406, 23.01084172723449939 ) ) ;
#47997 = ORIENTED_EDGE ( 'NONE', *, *, #57053, .T. ) ;
#47998 = CARTESIAN_POINT ( 'NONE',  ( 56.87964969553961225, -49.90805661006463367, 69.03665511646475750 ) ) ;
#47999 = CARTESIAN_POINT ( 'NONE',  ( -31.22333652669472670, 298.2284108743594970, -9.257293644257531540 ) ) ;
#48000 = CARTESIAN_POINT ( 'NONE',  ( 9.995225837605406838, -50.02526524736600066, 26.59626811386029743 ) ) ;
#48001 = SURFACE_STYLE_FILL_AREA ( #46434 ) ;
#48002 = ORIENTED_EDGE ( 'NONE', *, *, #58110, .F. ) ;
#48004 = CARTESIAN_POINT ( 'NONE',  ( -9.995361331467700339, -50.02485175282393470, 26.59863933490087362 ) ) ;
#48003 = CARTESIAN_POINT ( 'NONE',  ( -98.56958724828976415, -38.35590500345170994, 80.52781705630614795 ) ) ;
#48005 = DIRECTION ( 'NONE',  ( 0.1270361284032155702, -0.9918980905719708696, 0.000000000000000000 ) ) ;
#48006 = CARTESIAN_POINT ( 'NONE',  ( 74.56127108291157413, -4.000000000000000000, 4.898587196589421703E-16 ) ) ;
#48007 = DIRECTION ( 'NONE',  ( 0.000000000000000000, 0.000000000000000000, -1.000000000000000000 ) ) ;
#48008 = CARTESIAN_POINT ( 'NONE',  ( 4.401442555609581635E-16, -10.15625000204838457, -7.188101187500000044 ) ) ;
#48009 = FILL_AREA_STYLE_COLOUR ( '', #12327 ) ;
#48010 = AXIS2_PLACEMENT_3D ( 'NONE', #47355, #7951, #106647 ) ;
#48011 = DIRECTION ( 'NONE',  ( -0.5735764363510461594, 0.8191520442889916875, 1.003171929053524870E-16 ) ) ;
#48012 = ORIENTED_EDGE ( 'NONE', *, *, #23065, .T. ) ;
#48013 = CARTESIAN_POINT ( 'NONE',  ( 84.06432143690391001, -35.94819419959944895, 174.2791522909043351 ) ) ;
#48014 = CARTESIAN_POINT ( 'NONE',  ( 2.745304562109406987, -9.118674939225453357, -12.27857983297191957 ) ) ;
#48015 = CARTESIAN_POINT ( 'NONE',  ( -35.04511767293112712, 439.6082740367514248, 24.02922479211273910 ) ) ;
#48016 = VERTEX_POINT ( 'NONE', #65522 ) ;
#48017 = DIRECTION ( 'NONE',  ( 0.000000000000000000, 0.000000000000000000, -1.000000000000000000 ) ) ;
#48018 = CARTESIAN_POINT ( 'NONE',  ( 8.044970079964597787, -4.999999999999987566, -15.82739658861712151 ) ) ;
#48019 = CARTESIAN_POINT ( 'NONE',  ( 25.85848788125878528, 35.03499038825931677, -8.997391814579291491 ) ) ;
#48020 = CARTESIAN_POINT ( 'NONE',  ( 14.37349357814347250, 2.004823033966244950, -4.269535008049492042 ) ) ;
#48021 = CARTESIAN_POINT ( 'NONE',  ( -39.04193823264170504, 42.03880034757720097, -56.82620883133870393 ) ) ;
#48022 = DIRECTION ( 'NONE',  ( 0.000000000000000000, -1.000000000000000000, 0.000000000000000000 ) ) ;
#48023 = EDGE_LOOP ( 'NONE', ( #18002, #61084, #28910, #48775 ) ) ;
#48024 = EDGE_CURVE ( 'NONE', #88009, #30348, #32105, .T. ) ;
#48025 = SURFACE_STYLE_FILL_AREA ( #31371 ) ;
#48026 = CARTESIAN_POINT ( 'NONE',  ( 6.499999999999998224, -1.417018949932255412, -5.722407714415304270 ) ) ;
#48027 = CARTESIAN_POINT ( 'NONE',  ( 0.3381073927595607542, 25.18058069739937821, 40.71490780997189773 ) ) ;
#48028 = ADVANCED_FACE ( 'NONE', ( #73590 ), #37479, .F. ) ;
#48029 = EDGE_CURVE ( 'NONE', #90738, #72747, #81674, .T. ) ;
#48032 = CIRCLE ( 'NONE', #13624, 10.00000000000000178 ) ;
#48031 = CARTESIAN_POINT ( 'NONE',  ( -11.99663858561632601, 8.161776382637276228, -8.765865389969762944 ) ) ;
#48030 = CARTESIAN_POINT ( 'NONE',  ( 43.02621584241281028, 434.6128289108257832, 16.97888786058996047 ) ) ;
#48033 = VECTOR ( 'NONE', #53106, 999.9999999999998863 ) ;
#48034 = CARTESIAN_POINT ( 'NONE',  ( 5.082755093536324154, -17.84375000204838457, 5.082755093536326818 ) ) ;
#48035 = CARTESIAN_POINT ( 'NONE',  ( -28.49053509030305520, 18.29756676117400005, -40.46890581211962967 ) ) ;
#48036 = DIRECTION ( 'NONE',  ( 0.000000000000000000, 0.000000000000000000, -1.000000000000000000 ) ) ;
#48037 = AXIS2_PLACEMENT_3D ( 'NONE', #69356, #19252, #34876 ) ;
#48038 = ORIENTED_EDGE ( 'NONE', *, *, #52938, .F. ) ;
#48039 = CARTESIAN_POINT ( 'NONE',  ( -4.250000000000000000, 5.204748896376250699E-16, -10.00000000000000000 ) ) ;
#48040 = CARTESIAN_POINT ( 'NONE',  ( 7.897825807688775512, 1.532833846124507238, -7.633607627188419897 ) ) ;
#48041 = CARTESIAN_POINT ( 'NONE',  ( -8.203969886209304008, 114.5837526204806522, -2.539157851778924031E-12 ) ) ;
#48042 = CARTESIAN_POINT ( 'NONE',  ( -8.990409435379676850, -5.000000000000000888, -71.93151781322266913 ) ) ;
#48043 = DIRECTION ( 'NONE',  ( -0.000000000000000000, -0.000000000000000000, 1.000000000000000000 ) ) ;
#48044 = EDGE_CURVE ( 'NONE', #8019, #53170, #83933, .T. ) ;
#48045 = ORIENTED_EDGE ( 'NONE', *, *, #66520, .F. ) ;
#48046 = CARTESIAN_POINT ( 'NONE',  ( 0.000000000000000000, 0.000000000000000000, 0.000000000000000000 ) ) ;
#48047 = DIRECTION ( 'NONE',  ( 0.000000000000000000, -1.000000000000000000, 0.000000000000000000 ) ) ;
#48048 = VERTEX_POINT ( 'NONE', #16978 ) ;
#48049 = AXIS2_PLACEMENT_3D ( 'NONE', #36856, #28774, #20695 ) ;
#48050 = EDGE_CURVE ( 'NONE', #13645, #35586, #9849, .T. ) ;
#48051 = CARTESIAN_POINT ( 'NONE',  ( 4.699999999999999289, 6.499999999999999112, 0.000000000000000000 ) ) ;
#48052 = FACE_OUTER_BOUND ( 'NONE', #10291, .T. ) ;
#48053 = CARTESIAN_POINT ( 'NONE',  ( -42.99950361083188000, 39.44597763921156997, -48.95955523496266437 ) ) ;
#48054 = UNCERTAINTY_MEASURE_WITH_UNIT (LENGTH_MEASURE( 1.000000000000000082E-05 ), #77020, 'distance_accuracy_value', 'NONE');
#48055 = CARTESIAN_POINT ( 'NONE',  ( -106.5960259156999541, -59.99999999999999289, 120.1111938281909914 ) ) ;
#48056 = CARTESIAN_POINT ( 'NONE',  ( 0.000000000000000000, 0.000000000000000000, -13.00000000000000000 ) ) ;
#48057 = CARTESIAN_POINT ( 'NONE',  ( -3.269135563215229023, 294.8518027752268722, -10.00000000024436453 ) ) ;
#48058 = DIRECTION ( 'NONE',  ( 0.000000000000000000, -1.000000000000000000, 0.000000000000000000 ) ) ;
#48059 = CARTESIAN_POINT ( 'NONE',  ( 38.51502786939607859, 460.0233756673479206, 2.043034587344076947 ) ) ;
#48061 = EDGE_CURVE ( 'NONE', #62849, #41885, #66218, .T. ) ;
#48060 = B_SPLINE_CURVE_WITH_KNOTS ( 'NONE', 3,
 ( #77910, #60680, #11556, #9974 ),
 .UNSPECIFIED., .F., .F.,
 ( 4, 4 ),
 ( 2.442512830937285646E-17, 0.0004064560158402741601 ),
 .UNSPECIFIED. ) ;
#48063 = CARTESIAN_POINT ( 'NONE',  ( -14.29190075645216851, 7.765108448528613039, 6.049455384109680978 ) ) ;
#48062 = CARTESIAN_POINT ( 'NONE',  ( 9.999999999999996447, -5.000000000000002665, -83.69100306251233690 ) ) ;
#48064 = VECTOR ( 'NONE', #67577, 1000.000000000000000 ) ;
#48065 = CARTESIAN_POINT ( 'NONE',  ( -82.34390938163903684, -50.00253640360821095, 179.4910488424855828 ) ) ;
#48066 = ORIENTED_EDGE ( 'NONE', *, *, #14632, .F. ) ;
#48067 = ORIENTED_EDGE ( 'NONE', *, *, #8222, .F. ) ;
#48068 = DIRECTION ( 'NONE',  ( 0.000000000000000000, 0.000000000000000000, 1.000000000000000000 ) ) ;
#48069 = CARTESIAN_POINT ( 'NONE',  ( 32.22120753352782430, 464.6691781026583499, 10.60621122532595884 ) ) ;
#48070 = CARTESIAN_POINT ( 'NONE',  ( 27.10511071441204578, 34.75829513984540142, 7.556984339685363317 ) ) ;
#48071 = CYLINDRICAL_SURFACE ( 'NONE', #15196, 1.250000000000001110 ) ;
#48072 = CARTESIAN_POINT ( 'NONE',  ( 8.763463954822906743, 19.59837311309046370, -1.228393653933357778E-12 ) ) ;
#48073 = CARTESIAN_POINT ( 'NONE',  ( -12.51707952085838471, -5.000000000000000000, -88.70144047758928707 ) ) ;
#48074 = CARTESIAN_POINT ( 'NONE',  ( 0.000000000000000000, 29.56666008184760130, -34.51297463494397988 ) ) ;
#48075 = VECTOR ( 'NONE', #73222, 1000.000000000000000 ) ;
#48076 = CARTESIAN_POINT ( 'NONE',  ( 105.8555784348092885, -14.21045842199437637, 186.2209013957143782 ) ) ;
#48077 = CARTESIAN_POINT ( 'NONE',  ( -113.7193438732989961, -60.00000000000000000, 185.6039524652145474 ) ) ;
#48078 = CARTESIAN_POINT ( 'NONE',  ( -62.38895926707620987, -32.53592809500086247, 75.23077026582143390 ) ) ;
#48079 = VERTEX_POINT ( 'NONE', #66579 ) ;
#48080 = CARTESIAN_POINT ( 'NONE',  ( 0.7145311798163270778, 9.237604307034018802, 3.185620757954082679E-16 ) ) ;
#48081 = CARTESIAN_POINT ( 'NONE',  ( 94.83079671683508138, -59.99999999999024425, -0.6452062745601389038 ) ) ;
#48082 = CONICAL_SURFACE ( 'NONE', #46424, 34.51297463494397988, 1.221730476396026610 ) ;
#48083 = ORIENTED_EDGE ( 'NONE', *, *, #83854, .F. ) ;
#48084 = CARTESIAN_POINT ( 'NONE',  ( 9.180358464578489104E-06, -29.02944131831594632, 28.72789017932170097 ) ) ;
#48085 = CONICAL_SURFACE ( 'NONE', #98068, 4.000000000000001776, 0.9599310885968808105 ) ;
#48086 = CARTESIAN_POINT ( 'NONE',  ( 7.188101187500000044, -12.03125000204838635, 0.000000000000000000 ) ) ;
#48087 = PRESENTATION_STYLE_ASSIGNMENT (( #15198 ) ) ;
#48088 = ORIENTED_EDGE ( 'NONE', *, *, #75151, .F. ) ;
#48089 = CARTESIAN_POINT ( 'NONE',  ( 7.144701066121058375, -30.00000000000003553, 0.9176209997231349336 ) ) ;
#48090 = ORIENTED_EDGE ( 'NONE', *, *, #61163, .F. ) ;
#48091 = DIRECTION ( 'NONE',  ( 0.000000000000000000, 0.000000000000000000, -1.000000000000000000 ) ) ;
#48092 = DIRECTION ( 'NONE',  ( 0.000000000000000000, 0.000000000000000000, 1.000000000000000000 ) ) ;
#48093 = CARTESIAN_POINT ( 'NONE',  ( -97.54655262679582961, -60.00000000000001421, 202.4652287849740446 ) ) ;
#48094 = CARTESIAN_POINT ( 'NONE',  ( 9.864453787710772303, -57.59356044529621244, 25.34106120123098549 ) ) ;
#48095 = CARTESIAN_POINT ( 'NONE',  ( -2.977408999572654480, -27.50000000204838813, 7.188101187499999156 ) ) ;
#48096 = CARTESIAN_POINT ( 'NONE',  ( 34.25540317603680762, 485.0620278916508141, -1.482526247038510991 ) ) ;
#48097 = CARTESIAN_POINT ( 'NONE',  ( 64.78349330513380266, -4.000000000000000888, 4.898587196589422689E-16 ) ) ;
#48098 = DIRECTION ( 'NONE',  ( 0.8191520442889884679, 0.000000000000000000, 0.5735764363510509334 ) ) ;
#48099 = DIRECTION ( 'NONE',  ( 0.000000000000000000, 1.000000000000000000, 0.000000000000000000 ) ) ;
#48100 = CARTESIAN_POINT ( 'NONE',  ( -6.928203230275508773, 105.0000000000000000, 4.000000000000001776 ) ) ;
#48101 = CARTESIAN_POINT ( 'NONE',  ( 0.000000000000000000, -30.00000000000000000, 0.000000000000000000 ) ) ;
#48102 = EDGE_CURVE ( 'NONE', #17510, #31444, #43373, .T. ) ;
#48103 = CARTESIAN_POINT ( 'NONE',  ( 98.85644268318139893, -60.00000000000000000, 196.2379177705476252 ) ) ;
#48104 = CARTESIAN_POINT ( 'NONE',  ( -31.90879697719113750, -22.14461511112060066, 30.64637690011016247 ) ) ;
#48105 = CARTESIAN_POINT ( 'NONE',  ( 84.15356149169568312, 1.016364837396684119E-14, 0.000000000000000000 ) ) ;
#48106 = CARTESIAN_POINT ( 'NONE',  ( 41.45969462480130829, -46.43236721762693975, 41.56346318067672030 ) ) ;
#48107 = CARTESIAN_POINT ( 'NONE',  ( 4.453875240780039491, -1.734723475976807094E-15, 16.57301948837323380 ) ) ;
#48108 = EDGE_LOOP ( 'NONE', ( #96504, #61041, #69355, #29352, #49672 ) ) ;
#48109 = EDGE_CURVE ( 'NONE', #79581, #55752, #51979, .T. ) ;
#48110 = CARTESIAN_POINT ( 'NONE',  ( -43.34934355818133866, 465.4850867214047980, 10.08239944467068661 ) ) ;
#48111 = AXIS2_PLACEMENT_3D ( 'NONE', #41720, #43319, #100481 ) ;
#48112 = ADVANCED_FACE ( 'NONE', ( #25634 ), #49508, .T. ) ;
#48113 = CARTESIAN_POINT ( 'NONE',  ( -67.66808814965415309, -38.33453704423400410, 124.0875110596533375 ) ) ;
#48114 = ORIENTED_EDGE ( 'NONE', *, *, #17917, .F. ) ;
#48116 = CARTESIAN_POINT ( 'NONE',  ( -31.00389226642222340, 485.8187364282109115, 14.27494812388583512 ) ) ;
#48115 = CARTESIAN_POINT ( 'NONE',  ( 7.441633456671346458, -4.999999999999998224, -15.55954248125250139 ) ) ;
#48117 = FACE_OUTER_BOUND ( 'NONE', #82685, .T. ) ;
#48118 = DIRECTION ( 'NONE',  ( 0.000000000000000000, -1.000000000000000000, 0.000000000000000000 ) ) ;
#48119 = CARTESIAN_POINT ( 'NONE',  ( 1.250250887278956835, 43.55730586753710298, -17.65695166392345428 ) ) ;
#48120 = PLANE ( 'NONE',  #60101 ) ;
#48121 = DIRECTION ( 'NONE',  ( 0.000000000000000000, 0.000000000000000000, 1.000000000000000000 ) ) ;
#48122 = DIRECTION ( 'NONE',  ( -1.000000000000000000, -1.224606353822377258E-16, -0.000000000000000000 ) ) ;
#48123 = AXIS2_PLACEMENT_3D ( 'NONE', #72776, #90035, #16143 ) ;
#48124 = EDGE_CURVE ( 'NONE', #45709, #12173, #60642, .T. ) ;
#48125 = CARTESIAN_POINT ( 'NONE',  ( 94.01771362528924669, -60.00000000000000711, 41.47442360232466285 ) ) ;
#48126 = DIRECTION ( 'NONE',  ( -0.5735764363510494901, -0.8191520442889894671, 0.000000000000000000 ) ) ;
#48127 = EDGE_CURVE ( 'NONE', #76519, #39308, #87421, .T. ) ;
#48128 = EDGE_CURVE ( 'NONE', #14310, #73863, #25460, .T. ) ;
#48129 = LINE ( 'NONE', #55156, #16371 ) ;
#48130 = DIRECTION ( 'NONE',  ( -1.000000000000000000, 0.000000000000000000, 0.000000000000000000 ) ) ;
#48131 = ORIENTED_EDGE ( 'NONE', *, *, #9820, .T. ) ;
#48132 = CARTESIAN_POINT ( 'NONE',  ( -89.18872655255631798, -29.99999999994696864, 13.78793652477736842 ) ) ;
#48133 = ORIENTED_EDGE ( 'NONE', *, *, #24204, .T. ) ;
#48134 = DIRECTION ( 'NONE',  ( -1.000000000000000000, -1.224606353822377258E-16, -0.000000000000000000 ) ) ;
#48135 = CARTESIAN_POINT ( 'NONE',  ( -15.05785784214673129, 3.824195276770050445, -4.604276673498577388 ) ) ;
#48136 = CARTESIAN_POINT ( 'NONE',  ( 8.830611806670223274, 18.20472706776127580, 4.999999999999999112 ) ) ;
#48137 = FACE_OUTER_BOUND ( 'NONE', #12211, .T. ) ;
#48138 = DIRECTION ( 'NONE',  ( -1.000000000000000000, -1.224606353822377258E-16, -0.000000000000000000 ) ) ;
#48139 = CARTESIAN_POINT ( 'NONE',  ( -7.188101187500001821, -26.37500000204838457, -2.977408999572651371 ) ) ;
#48140 = DIRECTION ( 'NONE',  ( 0.5735764363510440500, 0.8191520442889932418, 0.000000000000000000 ) ) ;
#48141 = CARTESIAN_POINT ( 'NONE',  ( 7.442703790580194934, 40.98154234363288140, -69.28862639872464513 ) ) ;
#48142 = ORIENTED_EDGE ( 'NONE', *, *, #96705, .F. ) ;
#48143 = CIRCLE ( 'NONE', #1622, 5.000000000000002665 ) ;
#48145 = ORIENTED_EDGE ( 'NONE', *, *, #14904, .T. ) ;
#48144 = LINE ( 'NONE', #39559, #78713 ) ;
#48146 = CARTESIAN_POINT ( 'NONE',  ( 83.77344519934696621, -22.14388846856150650, 150.6883876448328010 ) ) ;
#48147 = CIRCLE ( 'NONE', #36128, 2.000000000000001332 ) ;
#48148 = CARTESIAN_POINT ( 'NONE',  ( -38.18740872092708827, 27.41008126919087928, -13.30320916973952627 ) ) ;
#48149 = VERTEX_POINT ( 'NONE', #84365 ) ;
#48150 = CARTESIAN_POINT ( 'NONE',  ( -60.68810323480906987, 50.00000000000000711, 17.09759988054065261 ) ) ;
#48151 = CARTESIAN_POINT ( 'NONE',  ( 7.213352437320217803, -87.01836473007681150, -3.463014597543483841 ) ) ;
#48152 = CARTESIAN_POINT ( 'NONE',  ( -5.082755093536326818, -13.71875000204838457, 5.082755093536325042 ) ) ;
#48153 = CARTESIAN_POINT ( 'NONE',  ( 7.986452802927061612, 26.02690242308113966, 0.5332468218996363474 ) ) ;
#48154 = CARTESIAN_POINT ( 'NONE',  ( -37.03244656124025624, -57.69633701093174949, 51.43040253561569131 ) ) ;
#48155 = CARTESIAN_POINT ( 'NONE',  ( 11.99465477046492623, 294.5867369860492886, 1.880684200158333930 ) ) ;
#48156 = ORIENTED_EDGE ( 'NONE', *, *, #21466, .T. ) ;
#48157 =( NAMED_UNIT ( * ) PLANE_ANGLE_UNIT ( ) SI_UNIT ( $, .RADIAN. ) );
#48158 = DIRECTION ( 'NONE',  ( 0.000000000000000000, 0.000000000000000000, -1.000000000000000000 ) ) ;
#48159 = STYLED_ITEM ( 'NONE', ( #81712 ), #90878 ) ;
#48160 = DIRECTION ( 'NONE',  ( 0.5735764363510462704, 0.8191520442889915765, 0.000000000000000000 ) ) ;
#48161 = EDGE_CURVE ( 'NONE', #76918, #20213, #42297, .T. ) ;
#48162 = B_SPLINE_CURVE_WITH_KNOTS ( 'NONE', 3,
 ( #46327, #5342, #8902, #24592, #41802, #246, #72579, #74690, #105481, #57439, #97377, #64509, #105996, #56375, #40211, #89310, #15405, #48292, #50414, #93564, #92478, #11552, #19711, #60157, #93020, #69296, #2406, #84933, #91441, #2936, #68218, #101650, #27807, #1321 ),
 .UNSPECIFIED., .F., .F.,
 ( 4, 2, 2, 2, 2, 2, 2, 2, 2, 2, 2, 2, 2, 2, 2, 2, 4 ),
 ( 0.01263889472610568200, 0.01342810546992895954, 0.01421731621375223881, 0.01500652695757551634, 0.01579573770139879388, 0.01658494844522207315, 0.01737415918904534895, 0.01816336993286862822, 0.01895258067669190749, 0.01974179142051518676, 0.02053100216433846603, 0.02132021290816174183, 0.02210942365198502110, 0.02289863439580829690, 0.02368784513963157617, 0.02447705588345485544, 0.02526626662727813125 ),
 .UNSPECIFIED. ) ;
#48163 = CARTESIAN_POINT ( 'NONE',  ( -8.000000000000000000, 0.000000000000000000, -1.875285714285714445 ) ) ;
#48164 = ORIENTED_EDGE ( 'NONE', *, *, #93691, .T. ) ;
#48165 = CARTESIAN_POINT ( 'NONE',  ( 4.898587196589412829E-16, -10.81250000409677092, -8.000000000000000000 ) ) ;
#48166 = CARTESIAN_POINT ( 'NONE',  ( -19.51791082181538783, -16.90378180463951452, 31.48562786591203988 ) ) ;
#48167 = CARTESIAN_POINT ( 'NONE',  ( -38.50844621391336631, 490.3070771754929638, 12.08756601353534421 ) ) ;
#48168 = AXIS2_PLACEMENT_3D ( 'NONE', #16177, #97096, #105714 ) ;
#48169 = CARTESIAN_POINT ( 'NONE',  ( 1.250721446675217452, 51.63789146372492667, -9.152276705697273584 ) ) ;
#48170 = CARTESIAN_POINT ( 'NONE',  ( -9.645512969475857901, 88.01103150675727704, -2.645801731561387538 ) ) ;
#48171 = DIRECTION ( 'NONE',  ( 0.1804394941736726932, -0.5071212677061492924, 0.8427749455118236366 ) ) ;
#48172 = PRODUCT_CONTEXT ( 'NONE', #17676, 'mechanical' ) ;
#48173 = CARTESIAN_POINT ( 'NONE',  ( 38.31552673953900268, 27.59984468902660026, 11.19255079935879849 ) ) ;
#48174 = VERTEX_POINT ( 'NONE', #18049 ) ;
#48175 = CARTESIAN_POINT ( 'NONE',  ( -4.894569681090269242, -46.92198688625742165, 42.70842733634118815 ) ) ;
#48176 = DIRECTION ( 'NONE',  ( 0.000000000000000000, -1.000000000000000000, 0.000000000000000000 ) ) ;
#48177 = CARTESIAN_POINT ( 'NONE',  ( -69.28690090100495524, -38.19429424212712121, -31.44801709845743787 ) ) ;
#48178 = CARTESIAN_POINT ( 'NONE',  ( -3.567823017641476468, -49.06830718686870085, 103.5075034329448016 ) ) ;
#48179 = CARTESIAN_POINT ( 'NONE',  ( 0.000000000000000000, 0.000000000000000000, 0.000000000000000000 ) ) ;
#48180 = CIRCLE ( 'NONE', #105100, 9.999999999999998224 ) ;
#48181 = ORIENTED_EDGE ( 'NONE', *, *, #99945, .T. ) ;
#48182 = B_SPLINE_CURVE_WITH_KNOTS ( 'NONE', 3,
 ( #70717, #13519, #35729, #20632, #37321, #101492, #60521, #61582, #19556, #44317, #36270, #86392, #53472, #12459, #45913, #78269, #4381, #103089 ),
 .UNSPECIFIED., .F., .F.,
 ( 4, 2, 2, 2, 2, 2, 2, 2, 4 ),
 ( 0.000000000000000000, 0.06250000000000000000, 0.1250000000000000000, 0.1875000000000000000, 0.2500000000000000000, 0.3125000000000000000, 0.3750000000000000000, 0.4375000000000000000, 0.5000000000000000000 ),
 .UNSPECIFIED. ) ;
#48183 = CARTESIAN_POINT ( 'NONE',  ( 3.313708498984799800, -9.406250004096770923, -7.999999999999961808 ) ) ;
#48184 = CARTESIAN_POINT ( 'NONE',  ( 101.3723521623251145, -57.63037166266066436, 203.5050614878415729 ) ) ;
#48185 = STYLED_ITEM ( 'NONE', ( #36039 ), #34271 ) ;
#48186 = EDGE_CURVE ( 'NONE', #75208, #17393, #85733, .T. ) ;
#48187 = CARTESIAN_POINT ( 'NONE',  ( 35.85615118283584479, 463.5955582468889133, 19.55698106745834153 ) ) ;
#48188 = CARTESIAN_POINT ( 'NONE',  ( 19.83349330513380693, 4.000000000000003553, 0.000000000000000000 ) ) ;
#48189 = CARTESIAN_POINT ( 'NONE',  ( -6.526324006461421412, 53.62377623897270240, 7.079659290374570091 ) ) ;
#48190 = CARTESIAN_POINT ( 'NONE',  ( -73.04440972101423313, -60.00000000000000711, 162.8656828868589912 ) ) ;
#48191 = CARTESIAN_POINT ( 'NONE',  ( -45.17824257314219949, 354.4244853104167987, 3.762393652172960845 ) ) ;
#48192 = DIRECTION ( 'NONE',  ( 0.000000000000000000, 1.000000000000000000, 0.000000000000000000 ) ) ;
#48193 = TOROIDAL_SURFACE ( 'NONE', #20711, 66.00000000000000000, 0.5000000000000000000 ) ;
#48194 = EDGE_CURVE ( 'NONE', #49541, #7953, #32294, .T. ) ;
#48195 = CARTESIAN_POINT ( 'NONE',  ( -57.09426686934756390, 50.00000000000000000, -27.25041924766811618 ) ) ;
#48196 = CARTESIAN_POINT ( 'NONE',  ( -85.23003832000186719, -39.32874488855976125, 184.5462598398625005 ) ) ;
#48197 = ORIENTED_EDGE ( 'NONE', *, *, #94907, .F. ) ;
#48198 = CARTESIAN_POINT ( 'NONE',  ( 31.10268009770144104, 314.3950341270036120, -7.730101311383788421 ) ) ;
#48199 = AXIS2_PLACEMENT_3D ( 'NONE', #65637, #33828, #99583 ) ;
#48200 = ORIENTED_EDGE ( 'NONE', *, *, #96434, .F. ) ;
#48201 = CARTESIAN_POINT ( 'NONE',  ( 63.56127108291158123, 6.975173280561618775E-15, 0.000000000000000000 ) ) ;
#48202 = FACE_OUTER_BOUND ( 'NONE', #4625, .T. ) ;
#48203 = CARTESIAN_POINT ( 'NONE',  ( -85.19250957274734048, -60.20006492606454174, -15.74789945096170207 ) ) ;
#48204 = DIRECTION ( 'NONE',  ( 1.000000000000000000, -0.000000000000000000, 2.742080092235280244E-17 ) ) ;
#48205 = DIRECTION ( 'NONE',  ( 0.000000000000000000, 0.000000000000000000, -1.000000000000000000 ) ) ;
#48206 = ORIENTED_EDGE ( 'NONE', *, *, #82117, .T. ) ;
#48207 = CARTESIAN_POINT ( 'NONE',  ( -33.00000000000000000, 439.7597899781497972, 24.16317522621304192 ) ) ;
#48208 = CARTESIAN_POINT ( 'NONE',  ( 11.08838757566412170, 8.467236466350284374, -9.834809068639062346 ) ) ;
#48209 = CARTESIAN_POINT ( 'NONE',  ( -8.569529079651847070, -1.734723475976807094E-15, 14.86825985028331942 ) ) ;
#48210 = CARTESIAN_POINT ( 'NONE',  ( 74.56127108291157413, -4.000000000000000888, 4.898587196589422689E-16 ) ) ;
#48211 = VECTOR ( 'NONE', #70147, 999.9999999999998863 ) ;
#48212 = CARTESIAN_POINT ( 'NONE',  ( 94.49477393579812201, -60.00000000000003553, -13.88944369105108301 ) ) ;
#48213 = CARTESIAN_POINT ( 'NONE',  ( -78.42949214982630224, -32.55659982916139228, 130.6045153880263854 ) ) ;
#48214 = ORIENTED_EDGE ( 'NONE', *, *, #27728, .T. ) ;
#48215 = CARTESIAN_POINT ( 'NONE',  ( -1.309564884278361513E-05, -14.21045842199434972, 34.36840973699906243 ) ) ;
#48216 = CARTESIAN_POINT ( 'NONE',  ( 6.928203230275510549, 85.00000000000000000, -4.000000000000000000 ) ) ;
#48217 = CARTESIAN_POINT ( 'NONE',  ( 89.04854951302100119, -57.60430045889667383, 203.7548466016606596 ) ) ;
#48218 = CARTESIAN_POINT ( 'NONE',  ( 28.19101533190163522, 34.18031863878626808, 9.431734573481964645 ) ) ;
#48219 = CARTESIAN_POINT ( 'NONE',  ( 40.85601670693966980, 312.5844051700327100, -5.777679661402379985 ) ) ;
#48220 = CONICAL_SURFACE ( 'NONE', #1723, 4.172000000000001485, 0.9599310885968750373 ) ;
#48221 = CARTESIAN_POINT ( 'NONE',  ( 18.71538461538461462, 1.411358822780289120E-15, 0.000000000000000000 ) ) ;
#48222 = EDGE_LOOP ( 'NONE', ( #21799, #70442, #90967, #102896, #4455 ) ) ;
#48223 = CARTESIAN_POINT ( 'NONE',  ( -22.43229796258882658, 26.08192010338115097, 30.96913259774117577 ) ) ;
#48224 = CARTESIAN_POINT ( 'NONE',  ( 0.000000000000000000, 0.000000000000000000, -6.235812796514431433 ) ) ;
#48225 = CARTESIAN_POINT ( 'NONE',  ( 2.977408999572651815, -16.43750000204838457, 7.188101187500000933 ) ) ;
#48226 = LINE ( 'NONE', #8306, #87743 ) ;
#48227 = SURFACE_STYLE_USAGE ( .BOTH. , #39647 ) ;
#48228 = CYLINDRICAL_SURFACE ( 'NONE', #33086, 5.000000000000000888 ) ;
#48229 = DIRECTION ( 'NONE',  ( -0.000000000000000000, -0.000000000000000000, 1.000000000000000000 ) ) ;
#48230 = CARTESIAN_POINT ( 'NONE',  ( 46.08349330513379982, 1.593028355512270567E-15, 0.000000000000000000 ) ) ;
#48231 = VERTEX_POINT ( 'NONE', #9927 ) ;
#48232 = EDGE_CURVE ( 'NONE', #52343, #45785, #104639, .T. ) ;
#48233 = CARTESIAN_POINT ( 'NONE',  ( 43.18057774162367934, 485.1460640375465800, 5.477159825588830522 ) ) ;
#48235 = CARTESIAN_POINT ( 'NONE',  ( 27.93076071969897001, -25.57948163322986801, 30.03616920575478133 ) ) ;
#48234 = CARTESIAN_POINT ( 'NONE',  ( -18.99999999999999289, 4.000000000000000888, -1.500000000000000444 ) ) ;
#48236 = AXIS2_PLACEMENT_3D ( 'NONE', #34158, #26085, #58943 ) ;
#48237 = CARTESIAN_POINT ( 'NONE',  ( -24.00177444567219354, 25.16455187703150997, 32.94427520949815857 ) ) ;
#48238 = ORIENTED_EDGE ( 'NONE', *, *, #14487, .F. ) ;
#48239 = ADVANCED_FACE ( 'NONE', ( #27229, #67653 ), #86518, .T. ) ;
#48240 = ORIENTED_EDGE ( 'NONE', *, *, #923, .F. ) ;
#48242 = CARTESIAN_POINT ( 'NONE',  ( 36.05499942621670328, 461.6905473683075911, 3.778726173785988074 ) ) ;
#48241 = SURFACE_STYLE_FILL_AREA ( #64971 ) ;
#48243 = DIRECTION ( 'NONE',  ( -0.000000000000000000, -1.000000000000000000, -0.000000000000000000 ) ) ;
#48244 = DIRECTION ( 'NONE',  ( 0.000000000000000000, -1.000000000000000000, 0.000000000000000000 ) ) ;
#48245 = CARTESIAN_POINT ( 'NONE',  ( 5.500000036871884213, 42.00000000000000000, -68.91429207046176941 ) ) ;
#48246 = CARTESIAN_POINT ( 'NONE',  ( -30.00000000000000000, 489.8687857340703431, 6.490256706953523747 ) ) ;
#48247 = FACE_OUTER_BOUND ( 'NONE', #2382, .T. ) ;
#48248 = ORIENTED_EDGE ( 'NONE', *, *, #96255, .T. ) ;
#48249 = CARTESIAN_POINT ( 'NONE',  ( 45.18230306424334941, -60.00000000000002132, -38.79808340435986480 ) ) ;
#48250 = CARTESIAN_POINT ( 'NONE',  ( 89.21430567429679570, -29.99999999999982947, 189.0176709876100745 ) ) ;
#48251 = DIRECTION ( 'NONE',  ( 0.000000000000000000, -1.000000000000000000, 0.000000000000000000 ) ) ;
#48252 = EDGE_CURVE ( 'NONE', #57762, #40845, #36665, .T. ) ;
#48253 = DIRECTION ( 'NONE',  ( 0.000000000000000000, -1.000000000000000000, 0.000000000000000000 ) ) ;
#48254 = EDGE_CURVE ( 'NONE', #21252, #104058, #13641, .T. ) ;
#48255 = CARTESIAN_POINT ( 'NONE',  ( 46.81343110146973885, 13.24251555485277443, -15.91224400466348676 ) ) ;
#48256 = ORIENTED_EDGE ( 'NONE', *, *, #102318, .F. ) ;
#48257 = VECTOR ( 'NONE', #33030, 1000.000000000000000 ) ;
#48258 = ORIENTED_EDGE ( 'NONE', *, *, #24443, .T. ) ;
#48259 = ORIENTED_EDGE ( 'NONE', *, *, #47456, .F. ) ;
#48260 = CARTESIAN_POINT ( 'NONE',  ( 0.000000000000000000, 0.000000000000000000, 0.000000000000000000 ) ) ;
#48261 = SURFACE_STYLE_USAGE ( .BOTH. , #106501 ) ;
#48262 = FILL_AREA_STYLE ('',( #64479 ) ) ;
#48263 = CARTESIAN_POINT ( 'NONE',  ( 29.57346108177781474, 314.0826370294551566, 12.66639719735920444 ) ) ;
#48264 = CARTESIAN_POINT ( 'NONE',  ( -41.11855258730697926, 320.9326643076389018, 4.345040179154948667 ) ) ;
#48265 = CARTESIAN_POINT ( 'NONE',  ( -4.946033322322218595, -62.76289455679260954, 12.87575235908490434 ) ) ;
#48266 = CARTESIAN_POINT ( 'NONE',  ( 0.000000000000000000, 0.000000000000000000, 5.000000000000002665 ) ) ;
#48268 = VERTEX_POINT ( 'NONE', #69260 ) ;
#48267 = AXIS2_PLACEMENT_3D ( 'NONE', #75788, #59627, #1882 ) ;
#48269 = CARTESIAN_POINT ( 'NONE',  ( -9.034516203396696810, 43.90155024610201195, 14.11102724417178678 ) ) ;
#48270 = B_SPLINE_CURVE_WITH_KNOTS ( 'NONE', 3,
 ( #84439, #34852, #10529, #52582, #43447, #60710, #68798, #76862, #18667, #35926, #85506, #101679, #2436, #68252, #27838, #19745, #50977, #34320, #9456, #42370, #35385, #92512, #26241, #101144, #50447, #27305, #67196, #2969, #83358, #10004, #93055, #75802, #11051, #67720, #51521, #19221, #1897, #52051, #75256, #59104, #43974, #84966, #18122, #42911, #26766, #59638, #31843, #72796, #6470, #56613, #21642, #72280 ),
 .UNSPECIFIED., .F., .F.,
 ( 4, 2, 2, 2, 2, 2, 2, 2, 2, 2, 2, 2, 2, 2, 2, 2, 2, 2, 2, 2, 2, 2, 2, 2, 2, 4 ),
 ( -6.000000002246681564E-08, 0.001182188478371536859, 0.002364436956743095914, 0.004728933913486179329, 0.009457927826972347893, 0.01064017630534381913, 0.01182242478371529383, 0.01418692174045836640, 0.01536917021882990876, 0.01655141869720145112, 0.01891591565394454277, 0.02128041261068763790, 0.02364490956743073996, 0.02837390348091693021, 0.03310289739440312046, 0.03783189130788931070, 0.04728987913486153855, 0.05674786696183375945, 0.06620585478880598729, 0.07566384261577820125, 0.08512183044275041521, 0.09457981826972264305, 0.1134957939236672514, 0.1324117695776118597, 0.1418697574045841570, 0.1513277452315564819 ),
 .UNSPECIFIED. ) ;
#48271 = EDGE_LOOP ( 'NONE', ( #1193, #80184 ) ) ;
#48272 = CARTESIAN_POINT ( 'NONE',  ( -1.469576158976823947E-15, -22.06250000409676915, 8.000000000000000000 ) ) ;
#48273 = CARTESIAN_POINT ( 'NONE',  ( -12.13034742782427955, 48.00000000000000000, -93.82352941176471006 ) ) ;
#48274 = DIRECTION ( 'NONE',  ( -1.000000000000000000, -0.000000000000000000, -0.000000000000000000 ) ) ;
#48275 = B_SPLINE_CURVE_WITH_KNOTS ( 'NONE', 3,
 ( #52193, #100218, #1505, #67339, #26385, #59247, #84042, #34991 ),
 .UNSPECIFIED., .F., .F.,
 ( 4, 2, 2, 4 ),
 ( -1.406834188354659210E-05, 0.0004804345972576759484, 0.0007276860668282884121, 0.0009749375363989009301 ),
 .UNSPECIFIED. ) ;
#48276 = CARTESIAN_POINT ( 'NONE',  ( -44.36055083073691918, -59.99999999999993605, 48.27248335138339286 ) ) ;
#48277 = CARTESIAN_POINT ( 'NONE',  ( 68.76507998961908186, -36.00945847659178867, 95.91866453639596557 ) ) ;
#48278 = ORIENTED_EDGE ( 'NONE', *, *, #56497, .F. ) ;
#48279 = CARTESIAN_POINT ( 'NONE',  ( 39.44782958596293554, 464.6967695243274079, 18.31680536522812730 ) ) ;
#48280 = DIRECTION ( 'NONE',  ( -1.000000000000000000, 0.000000000000000000, 0.000000000000000000 ) ) ;
#48281 =( BOUNDED_SURFACE ( )  B_SPLINE_SURFACE ( 2, 3, ( 
 ( #55357, #72088, #39214, #104995, #106030, #48330, #89870, #73669, #277, #66119, #80699, #55872 ),
 ( #81222, #48855, #64541, #73125, #6817, #7870, #74200, #57477, #90403, #25163, #58015, #23568 ),
 ( #72614, #33247, #32722, #98997, #31658, #90943, #15439, #65059, #56950, #40775, #16505, #31139 ),
 ( #15976, #17053, #65592, #7341, #49391, #82300, #89349, #49930, #40250, #32175, #47795, #56415 ),
 ( #97956, #24105, #106572, #98478, #6274, #41311, #24630, #39736, #105517, #81747, #8410, #64026 ),
 ( #96903, #23037, #97408, #88809, #14900, #51525, #10008, #26245, #43452, #83363, #9462, #27312 ),
 ( #19227, #43979, #25717, #50452, #42373, #91476, #59109, #58576, #812, #76329, #68258, #76866 ) ),
 .UNSPECIFIED., .F., .F., .F. ) 
 B_SPLINE_SURFACE_WITH_KNOTS ( ( 3, 2, 2, 3 ),
 ( 4, 2, 2, 2, 2, 4 ),
 ( -0.01000000000000000021, 0.000000000000000000, 1.000000000000000000, 1.010000000000000009 ),
 ( 0.000000000000000000, 0.001801747411056191499, 0.003603494822112382999, 0.005405242233168574065, 0.006306115938696670031, 0.007206989644224765998 ),
 .UNSPECIFIED. ) 
 GEOMETRIC_REPRESENTATION_ITEM ( )  RATIONAL_B_SPLINE_SURFACE ( (
 ( 1.000000000000000000, 1.000000000000000000, 1.000000000000000000, 1.000000000000000000, 1.000000000000000000, 1.000000000000000000, 1.000000000000000000, 1.000000000000000000, 1.000000000000000000, 1.000000000000000000, 1.000000000000000000, 1.000000000000000000),
 ( 1.000000000000000000, 1.000000000000000000, 1.000000000000000000, 1.000000000000000000, 1.000000000000000000, 1.000000000000000000, 1.000000000000000000, 1.000000000000000000, 1.000000000000000000, 1.000000000000000000, 1.000000000000000000, 1.000000000000000000),
 ( 1.000000000000000000, 1.000000000000000000, 1.000000000000000000, 1.000000000000000000, 1.000000000000000000, 1.000000000000000000, 1.000000000000000000, 1.000000000000000000, 1.000000000000000000, 1.000000000000000000, 1.000000000000000000, 1.000000000000000000),
 ( 1.857142857142858317, 1.857142857142858317, 1.857142857142858317, 1.857142857142858317, 1.857142857142858317, 1.857142857142858317, 1.857142857142858317, 1.857142857142858317, 1.857142857142858317, 1.857142857142858317, 1.857142857142858317, 1.857142857142858317),
 ( 1.000000000000000000, 1.000000000000000000, 1.000000000000000000, 1.000000000000000000, 1.000000000000000000, 1.000000000000000000, 1.000000000000000000, 1.000000000000000000, 1.000000000000000000, 1.000000000000000000, 1.000000000000000000, 1.000000000000000000),
 ( 1.000000000000000000, 1.000000000000000000, 1.000000000000000000, 1.000000000000000000, 1.000000000000000000, 1.000000000000000000, 1.000000000000000000, 1.000000000000000000, 1.000000000000000000, 1.000000000000000000, 1.000000000000000000, 1.000000000000000000),
 ( 1.000000000000000000, 1.000000000000000000, 1.000000000000000000, 1.000000000000000000, 1.000000000000000000, 1.000000000000000000, 1.000000000000000000, 1.000000000000000000, 1.000000000000000000, 1.000000000000000000, 1.000000000000000000, 1.000000000000000000) ) ) 
 REPRESENTATION_ITEM ( '' )  SURFACE ( )  );
#48282 = AXIS2_PLACEMENT_3D ( 'NONE', #35172, #2768, #10325 ) ;
#48283 = CARTESIAN_POINT ( 'NONE',  ( 19.34999999999999787, -3.309499999999999886, 4.475777889183790779E-16 ) ) ;
#48284 = ORIENTED_EDGE ( 'NONE', *, *, #68061, .T. ) ;
#48285 = FILL_AREA_STYLE_COLOUR ( '', #100350 ) ;
#48286 = CARTESIAN_POINT ( 'NONE',  ( 47.14583847125359739, 17.20522387600192715, 16.50112645797992528 ) ) ;
#48287 = CARTESIAN_POINT ( 'NONE',  ( -36.65199127662805978, 490.9971735395452015, 12.47305305857717350 ) ) ;
#48288 = ADVANCED_FACE ( 'NONE', ( #70310 ), #47800, .T. ) ;
#48289 = VECTOR ( 'NONE', #35295, 1000.000000000000000 ) ;
#48290 = CARTESIAN_POINT ( 'NONE',  ( -3.313708498984765161, -32.65625000409677625, 7.999999999999998224 ) ) ;
#48291 = CARTESIAN_POINT ( 'NONE',  ( 0.000000000000000000, -5.000000000000000000, 10.00000000000000000 ) ) ;
#48292 = CARTESIAN_POINT ( 'NONE',  ( 10.00004721872061531, 245.9998819531884635, -0.2617599822266503118 ) ) ;
#48293 = DIRECTION ( 'NONE',  ( -1.000000000000000000, 0.000000000000000000, 0.000000000000000000 ) ) ;
#48294 = CIRCLE ( 'NONE', #99966, 4.000000000000001776 ) ;
#48295 = CARTESIAN_POINT ( 'NONE',  ( 9.797372177749753774, 33.46509494847563815, 2.014953862275838503 ) ) ;
#48296 = CARTESIAN_POINT ( 'NONE',  ( 13.50000000000000355, 6.533945317241105499, -0.8419589098297789453 ) ) ;
#48297 = SURFACE_STYLE_FILL_AREA ( #62926 ) ;
#48298 = VERTEX_POINT ( 'NONE', #5560 ) ;
#48299 = FACE_OUTER_BOUND ( 'NONE', #17926, .T. ) ;
#48300 = CARTESIAN_POINT ( 'NONE',  ( -5.656854249492379694, -10.43749999999999112, -5.656854249492380582 ) ) ;
#48301 = CARTESIAN_POINT ( 'NONE',  ( 9.890468211898383544, -60.00000000000000000, 39.64862895235242490 ) ) ;
#48302 = CARTESIAN_POINT ( 'NONE',  ( -98.04267884131168387, -30.00000000000000355, 190.4907426802132591 ) ) ;
#48303 = EDGE_CURVE ( 'NONE', #89572, #69385, #65004, .T. ) ;
#48304 = CARTESIAN_POINT ( 'NONE',  ( -37.56673239365863282, -1.200000000000000030E-05, -10.95617127781024536 ) ) ;
#48305 = CARTESIAN_POINT ( 'NONE',  ( 40.76935397657385352, -57.69044601521297011, 56.95604026165146649 ) ) ;
#48306 = AXIS2_PLACEMENT_3D ( 'NONE', #20662, #53501, #78296 ) ;
#48307 = CARTESIAN_POINT ( 'NONE',  ( 61.85555555555556140, 6.915964383211875250E-15, 0.000000000000000000 ) ) ;
#48308 = CARTESIAN_POINT ( 'NONE',  ( 19.31349756789174066, -25.58635144299420006, -38.49263360045101479 ) ) ;
#48309 = AXIS2_PLACEMENT_3D ( 'NONE', #103463, #20489, #60894 ) ;
#48310 =( NAMED_UNIT ( * ) PLANE_ANGLE_UNIT ( ) SI_UNIT ( $, .RADIAN. ) );
#48311 = UNCERTAINTY_MEASURE_WITH_UNIT (LENGTH_MEASURE( 1.000000000000000082E-05 ), #53769, 'distance_accuracy_value', 'NONE');
#48312 = SURFACE_STYLE_FILL_AREA ( #80157 ) ;
#48313 = CARTESIAN_POINT ( 'NONE',  ( -16.90281938967774877, -59.99999999999997868, 39.91503433071412132 ) ) ;
#48314 = LINE ( 'NONE', #99526, #53727 ) ;
#48315 = ADVANCED_FACE ( 'NONE', ( #38487, #71350, #30397, #78916, #61161 ), #94349, .F. ) ;
#48316 = DIRECTION ( 'NONE',  ( -1.000000000000000000, 0.000000000000000000, 0.000000000000000000 ) ) ;
#48317 = CARTESIAN_POINT ( 'NONE',  ( -86.88653354982636756, -39.10394614662991586, 188.8703255679024267 ) ) ;
#48318 = ORIENTED_EDGE ( 'NONE', *, *, #20675, .T. ) ;
#48319 = CARTESIAN_POINT ( 'NONE',  ( 17.49999999999998934, 49.46308821774509568, 63.99046601234773135 ) ) ;
#48320 = CARTESIAN_POINT ( 'NONE',  ( 29.87260017596017292, 13.22901743408738717, 42.09629626707183547 ) ) ;
#48321 = CARTESIAN_POINT ( 'NONE',  ( -15.42473530526779868, -25.55047207056445302, 28.31187399038664054 ) ) ;
#48322 = DIRECTION ( 'NONE',  ( -1.000000000000000000, -0.000000000000000000, -0.000000000000000000 ) ) ;
#48323 = EDGE_CURVE ( 'NONE', #53830, #20373, #53063, .T. ) ;
#48325 = CARTESIAN_POINT ( 'NONE',  ( -33.49722639937191104, 439.8559922839228307, 24.25305334379669731 ) ) ;
#48324 = CARTESIAN_POINT ( 'NONE',  ( 19.00000000000001066, 4.000000000000000000, -1.500000000000000000 ) ) ;
#48326 = ORIENTED_EDGE ( 'NONE', *, *, #34703, .F. ) ;
#48327 = STYLED_ITEM ( 'NONE', ( #16687 ), #47135 ) ;
#48328 = DIRECTION ( 'NONE',  ( -1.000000000000000000, -1.224606353822377258E-16, -0.000000000000000000 ) ) ;
#48329 = AXIS2_PLACEMENT_3D ( 'NONE', #54745, #95238, #5161 ) ;
#48330 = CARTESIAN_POINT ( 'NONE',  ( -7.084012698788995976, -4.012402067415701268, -17.39015006382141237 ) ) ;
#48331 = DIRECTION ( 'NONE',  ( 0.000000000000000000, 0.000000000000000000, 1.000000000000000000 ) ) ;
#48332 = CARTESIAN_POINT ( 'NONE',  ( 33.81879868294056735, 301.0020191845601971, -0.6124722288186084107 ) ) ;
#48333 = CARTESIAN_POINT ( 'NONE',  ( 4.175533140205454075, -48.44478104465394352, 102.9090322054120747 ) ) ;
#48334 = FACE_OUTER_BOUND ( 'NONE', #70858, .T. ) ;
#48335 = CARTESIAN_POINT ( 'NONE',  ( 73.52189759326324747, -59.99999999999997868, 167.4063777988524464 ) ) ;
#48336 = CARTESIAN_POINT ( 'NONE',  ( -28.76346532419124458, 309.5219921958590135, -8.933260212751790164 ) ) ;
#48337 = ORIENTED_EDGE ( 'NONE', *, *, #81881, .T. ) ;
#48338 = CARTESIAN_POINT ( 'NONE',  ( -42.20041562234357002, 435.2369744135583574, 7.788607701745487333 ) ) ;
#48339 = SURFACE_STYLE_USAGE ( .BOTH. , #54839 ) ;
#48341 = CARTESIAN_POINT ( 'NONE',  ( -32.28930913497458022, 488.2717154064632723, 9.213726894912692700 ) ) ;
#48340 = CARTESIAN_POINT ( 'NONE',  ( 31.71028148999514329, -14.21045842199427156, 37.70122135646843731 ) ) ;
#48342 = CARTESIAN_POINT ( 'NONE',  ( 4.258869285391234882, 140.4044011673899774, -5.000000000000000000 ) ) ;
#48343 = CARTESIAN_POINT ( 'NONE',  ( -4.031080902170445235, -1.378107924927794770, 103.0284855429834607 ) ) ;
#48344 = ORIENTED_EDGE ( 'NONE', *, *, #14629, .F. ) ;
#48345 = EDGE_CURVE ( 'NONE', #24752, #16303, #80532, .T. ) ;
#48346 = COLOUR_RGB ( '', 0.72549020, 0.75294118, 0.79215686) ;
#48347 = CARTESIAN_POINT ( 'NONE',  ( -25.61096549847395565, 308.3358331228886300, 9.743382623630527206 ) ) ;
#48348 = VERTEX_POINT ( 'NONE', #36909 ) ;
#48349 = DIRECTION ( 'NONE',  ( 0.8191520442889881348, 0.000000000000000000, 0.5735764363510513775 ) ) ;
#48350 = AXIS2_PLACEMENT_3D ( 'NONE', #51047, #99607, #26837 ) ;
#48351 =( LENGTH_UNIT ( ) NAMED_UNIT ( * ) SI_UNIT ( .MILLI., .METRE. ) );
#48352 = CARTESIAN_POINT ( 'NONE',  ( 0.000000000000000000, 0.000000000000000000, 1.734723475976807094E-15 ) ) ;
#48353 = CARTESIAN_POINT ( 'NONE',  ( -5.000000000000000000, 0.000000000000000000, -9.974599999999998801 ) ) ;
#48354 = EDGE_LOOP ( 'NONE', ( #76384, #98086, #75451, #91383 ) ) ;
#48355 = CARTESIAN_POINT ( 'NONE',  ( -64.91565662648044110, 48.00000000000000000, 6.815324757466639127 ) ) ;
#48356 = CARTESIAN_POINT ( 'NONE',  ( 6.691148393531305416, -12.00380193953478702, 9.409600457876800661 ) ) ;
#48357 = CARTESIAN_POINT ( 'NONE',  ( -82.67652743962570128, -60.00000000002928857, 201.6796312862459786 ) ) ;
#48358 = CIRCLE ( 'NONE', #65623, 4.172000000000009479 ) ;
#48359 = CARTESIAN_POINT ( 'NONE',  ( 6.443810749341881916, -2.669419465175184136, -6.839891222013585015 ) ) ;
#48360 = CARTESIAN_POINT ( 'NONE',  ( 71.31537837103485344, -59.99999999999998579, 149.1299768214489063 ) ) ;
#48361 = FACE_OUTER_BOUND ( 'NONE', #13101, .T. ) ;
#48362 = LINE ( 'NONE', #95880, #60669 ) ;
#48363 = AXIS2_PLACEMENT_3D ( 'NONE', #57098, #106715, #88955 ) ;
#48365 = CARTESIAN_POINT ( 'NONE',  ( 16.70053533077139818, -35.99219286291273789, 30.12149763659517632 ) ) ;
#48364 = CARTESIAN_POINT ( 'NONE',  ( -113.7193438732989961, -60.00000000000000000, 185.6039524652145474 ) ) ;
#48366 = CARTESIAN_POINT ( 'NONE',  ( 98.63481415922996121, -37.99999999999972289, 192.2156350310174275 ) ) ;
#48367 = FACE_OUTER_BOUND ( 'NONE', #88411, .T. ) ;
#48368 = CARTESIAN_POINT ( 'NONE',  ( -44.50213627361837609, -25.70502922763081699, 39.42336395404723959 ) ) ;
#48369 = CIRCLE ( 'NONE', #55219, 5.000000000000010658 ) ;
#48370 = CARTESIAN_POINT ( 'NONE',  ( -0.8391198807171517116, 34.96075513128997159, -27.56988711285785953 ) ) ;
#48371 = VERTEX_POINT ( 'NONE', #21258 ) ;
#48372 = FACE_OUTER_BOUND ( 'NONE', #21903, .T. ) ;
#48373 = CARTESIAN_POINT ( 'NONE',  ( 16.11717644235050173, 21.56691778980479057, 2.165075456547000066 ) ) ;
#48374 = CARTESIAN_POINT ( 'NONE',  ( -3.068960578197905686, -68.89415226316417318, 13.02640661468439198 ) ) ;
#48375 = DIRECTION ( 'NONE',  ( -1.000000000000000000, -0.000000000000000000, -0.000000000000000000 ) ) ;
#48376 = CARTESIAN_POINT ( 'NONE',  ( 35.66932529116966322, 438.9565575286536045, 4.011496722538590909 ) ) ;
#48377 = EDGE_LOOP ( 'NONE', ( #1432, #3943, #5402, #25706, #33465 ) ) ;
#48378 = ORIENTED_EDGE ( 'NONE', *, *, #55041, .T. ) ;
#48379 = CARTESIAN_POINT ( 'NONE',  ( 108.7023100198421446, -30.00000000000508393, 185.2916543307226789 ) ) ;
#48380 =( NAMED_UNIT ( * ) SI_UNIT ( $, .STERADIAN. ) SOLID_ANGLE_UNIT ( ) );
#48381 = CARTESIAN_POINT ( 'NONE',  ( 5.668940197363838251, 41.88723871811491506, -59.02759513106027356 ) ) ;
#48383 = EDGE_CURVE ( 'NONE', #79906, #70259, #78766, .T. ) ;
#48382 = CARTESIAN_POINT ( 'NONE',  ( 1.489880555935390203E-15, 34.19642918197134662, 12.16579798332631412 ) ) ;
#48384 = CARTESIAN_POINT ( 'NONE',  ( 97.89223034704271242, -30.00000000000000355, 136.7744468160770737 ) ) ;
#48385 = ADVANCED_FACE ( 'NONE', ( #64347 ), #97738, .F. ) ;
#48386 = DIRECTION ( 'NONE',  ( 1.000000000000000000, 1.224606353822377258E-16, 0.000000000000000000 ) ) ;
#48387 = VERTEX_POINT ( 'NONE', #23907 ) ;
#48388 = PRESENTATION_LAYER_ASSIGNMENT (  '', '', ( #44961 ) ) ;
#48389 = VERTEX_POINT ( 'NONE', #79969 ) ;
#48390 = ORIENTED_EDGE ( 'NONE', *, *, #45539, .F. ) ;
#48391 = CARTESIAN_POINT ( 'NONE',  ( -1.833333333403031284, 42.00000000000000000, -60.21711271837360613 ) ) ;
#48392 = CARTESIAN_POINT ( 'NONE',  ( -5.625019081819782052, 41.66287055468434630, -70.61600276915974916 ) ) ;
#48393 = EDGE_CURVE ( 'NONE', #93010, #53023, #92557, .T. ) ;
#48394 = CARTESIAN_POINT ( 'NONE',  ( 7.500961644777538868E-15, 43.50000000000000711, -61.00000000000000000 ) ) ;
#48395 = ORIENTED_EDGE ( 'NONE', *, *, #60818, .T. ) ;
#48396 = CARTESIAN_POINT ( 'NONE',  ( 9.948688207305192321, 108.8702314949018444, -1.044946705213434024 ) ) ;
#48397 = PRESENTATION_LAYER_ASSIGNMENT (  '', '', ( #89760 ) ) ;
#48398 = ORIENTED_EDGE ( 'NONE', *, *, #33886, .F. ) ;
#48399 = CARTESIAN_POINT ( 'NONE',  ( 69.67238219402268840, -1.232595164407830946E-29, 4.000000000000007105 ) ) ;
#48400 = CARTESIAN_POINT ( 'NONE',  ( 79.85080175595479091, -38.77068210228555500, 192.7140471300223510 ) ) ;
#48401 = CARTESIAN_POINT ( 'NONE',  ( 10.35528044502231992, 10.95055699629187629, 10.44180044207346647 ) ) ;
#48402 = CARTESIAN_POINT ( 'NONE',  ( 83.78310723525129333, -37.99999999999999289, 174.8088074860800418 ) ) ;
#48403 = CARTESIAN_POINT ( 'NONE',  ( 38.99788563095989247, 323.4896271503449725, 16.92816184090444409 ) ) ;
#48404 = CARTESIAN_POINT ( 'NONE',  ( 9.658328022721198280, 45.55814826547295837, -15.25063005797932014 ) ) ;
#48405 =( LENGTH_UNIT ( ) NAMED_UNIT ( * ) SI_UNIT ( .MILLI., .METRE. ) );
#48406 = FACE_OUTER_BOUND ( 'NONE', #43789, .T. ) ;
#48407 = CARTESIAN_POINT ( 'NONE',  ( 42.77863378085803703, 403.5742920147162067, 19.98408815037751651 ) ) ;
#48408 = CARTESIAN_POINT ( 'NONE',  ( -36.87655955837857391, 438.2068510013161244, 3.933030107424709598 ) ) ;
#48409 = VECTOR ( 'NONE', #32366, 1000.000000000000000 ) ;
#48410 = CARTESIAN_POINT ( 'NONE',  ( -5.851594670652180419, 4.707302824160916721, 5.000000000000000000 ) ) ;
#48411 = ORIENTED_EDGE ( 'NONE', *, *, #61861, .T. ) ;
#48412 = B_SPLINE_CURVE_WITH_KNOTS ( 'NONE', 3,
 ( #67994, #59927, #44256, #74996 ),
 .UNSPECIFIED., .F., .F.,
 ( 4, 4 ),
 ( 0.000000000000000000, 0.001800036990446803433 ),
 .UNSPECIFIED. ) ;
#48413 = CARTESIAN_POINT ( 'NONE',  ( -33.30691720919135435, 302.0691436612021334, 11.59134413587671908 ) ) ;
#48414 = DIRECTION ( 'NONE',  ( 0.9738156377458858648, 0.000000000000000000, 0.2273391820201123570 ) ) ;
#48415 = UNCERTAINTY_MEASURE_WITH_UNIT (LENGTH_MEASURE( 1.000000000000000082E-05 ), #75956, 'distance_accuracy_value', 'NONE');
#48416 = CARTESIAN_POINT ( 'NONE',  ( 97.15356149169568312, -5.000000000000020428, 0.000000000000000000 ) ) ;
#48417 = CARTESIAN_POINT ( 'NONE',  ( 7.999999999999998224, -12.59374999999999467, 3.313708498984766493 ) ) ;
#48418 = CARTESIAN_POINT ( 'NONE',  ( 12.80902418639212748, -21.46289778021456129, 35.62032504730713356 ) ) ;
#48419 = CARTESIAN_POINT ( 'NONE',  ( -6.928203230275511437, 104.7352073274642805, 4.000000000000001776 ) ) ;
#48420 = ADVANCED_FACE ( 'NONE', ( #34526 ), #40894, .T. ) ;
#48421 = B_SPLINE_CURVE_WITH_KNOTS ( 'NONE', 3,
 ( #678, #24511, #75124, #17459, #23983, #57347, #25027, #17986, #34187, #16369, #83754, #50846, #9862, #42774, #105903, #56825 ),
 .UNSPECIFIED., .F., .F.,
 ( 4, 2, 2, 2, 2, 2, 2, 4 ),
 ( 0.000000000000000000, 0.0009812749226899852590, 0.001962549845379970518, 0.002943824768069955994, 0.003925099690759941903, 0.005887649536139912855, 0.006868924458829897897, 0.007850199381519883807 ),
 .UNSPECIFIED. ) ;
#48422 = DIRECTION ( 'NONE',  ( 1.000000000000000000, -0.000000000000000000, 1.224646799147353207E-16 ) ) ;
#48423 = VERTEX_POINT ( 'NONE', #30937 ) ;
#48424 = CARTESIAN_POINT ( 'NONE',  ( 86.26413129325493401, -21.18033766835324272, 178.9871004810926252 ) ) ;
#48425 = EDGE_CURVE ( 'NONE', #57533, #48149, #46068, .T. ) ;
#48426 = CARTESIAN_POINT ( 'NONE',  ( 3.484792534604217007, 15.95825086476136967, -9.380155525692146057 ) ) ;
#48427 = VERTEX_POINT ( 'NONE', #72418 ) ;
#48428 = CARTESIAN_POINT ( 'NONE',  ( 95.40603510496622164, -57.67176892321496240, 36.33773616593676081 ) ) ;
#48429 = AXIS2_PLACEMENT_3D ( 'NONE', #44732, #52262, #69532 ) ;
#48430 = CARTESIAN_POINT ( 'NONE',  ( 35.45036406932484141, 436.3203772529680009, 5.179456583036507133 ) ) ;
#48431 = CARTESIAN_POINT ( 'NONE',  ( 3.400000000000000355, 0.000000000000000000, -4.987924522925830217 ) ) ;
#48432 = EDGE_CURVE ( 'NONE', #80162, #100984, #103480, .T. ) ;
#48433 = VECTOR ( 'NONE', #50567, 1000.000000000000000 ) ;
#48434 = CARTESIAN_POINT ( 'NONE',  ( -60.27117132039084169, -38.00000000000001421, 72.18992984672541979 ) ) ;
#48435 = AXIS2_PLACEMENT_3D ( 'NONE', #82860, #90966, #59130 ) ;
#48436 = CARTESIAN_POINT ( 'NONE',  ( 2.094395098902661179, -4.999999999999998224, 8.000000000000000000 ) ) ;
#48437 = CARTESIAN_POINT ( 'NONE',  ( -1.015826369456739098, 8.073766409989460158, -7.642786413615525909 ) ) ;
#48439 = CARTESIAN_POINT ( 'NONE',  ( -12.35207828293850696, 7.405331434952278080, 8.319135986740995747 ) ) ;
#48438 = CARTESIAN_POINT ( 'NONE',  ( -3.482999479109682994E-15, 5.309483803148794756, 3.803704290982253600 ) ) ;
#48440 = CIRCLE ( 'NONE', #32935, 6.499999999999999112 ) ;
#48441 = EDGE_LOOP ( 'NONE', ( #98723, #52009, #6833, #33668 ) ) ;
#48442 = CARTESIAN_POINT ( 'NONE',  ( -6.750000000000015099, -11.69134295108991495, 0.000000000000000000 ) ) ;
#48443 = CARTESIAN_POINT ( 'NONE',  ( -28.09909703978631867, 36.32432838617303617, -9.569561972001043415 ) ) ;
#48444 = CARTESIAN_POINT ( 'NONE',  ( 9.216463528758916723, 15.13241195026071928, -3.884543032214160085 ) ) ;
#48445 = DIRECTION ( 'NONE',  ( 0.000000000000000000, 0.000000000000000000, 1.000000000000000000 ) ) ;
#48446 = CARTESIAN_POINT ( 'NONE',  ( 33.80014854764886678, 484.1533675814796425, 1.810747741435669189 ) ) ;
#48447 = VERTEX_POINT ( 'NONE', #14697 ) ;
#48448 = CARTESIAN_POINT ( 'NONE',  ( -7.372046728244052716, -0.06650713447798785316, 19.15741096255421638 ) ) ;
#48449 = CARTESIAN_POINT ( 'NONE',  ( 4.905194654929172948, -62.97605604980157068, 3.459476078998854121 ) ) ;
#48450 = EDGE_CURVE ( 'NONE', #58313, #15045, #27155, .T. ) ;
#48452 = CARTESIAN_POINT ( 'NONE',  ( -62.09692702121698460, -34.58946200273062743, -24.66260175802744570 ) ) ;
#48451 = DIRECTION ( 'NONE',  ( -1.000000000000000000, -1.224606353822377258E-16, -0.000000000000000000 ) ) ;
#48453 = ORIENTED_EDGE ( 'NONE', *, *, #2446, .F. ) ;
#48454 = COLOUR_RGB ( '', 0.08235294, 0.09019608, 0.10196078) ;
#48455 = B_SPLINE_CURVE_WITH_KNOTS ( 'NONE', 3,
 ( #77027, #101832, #60864, #10163, #43076, #93753, #75964, #96419, #5277, #55392, #102906, #94831, #29583, #54862, #79150, #14395, #20977, #53810, #86741, #88322 ),
 .UNSPECIFIED., .F., .F.,
 ( 4, 2, 2, 2, 2, 2, 2, 2, 2, 4 ),
 ( 0.002962320935262360670, 0.003468250424844080467, 0.003974179914425800264, 0.004480109404007520495, 0.004986038893589240725, 0.005491968383170961823, 0.005744933127961822372, 0.005997897872752681186, 0.006503827362334404019, 0.007009756851916126852 ),
 .UNSPECIFIED. ) ;
#48456 = ORIENTED_EDGE ( 'NONE', *, *, #87664, .T. ) ;
#48457 = CARTESIAN_POINT ( 'NONE',  ( -27.10511071441183617, 34.75829513984614039, 7.556984339678626483 ) ) ;
#48458 = CIRCLE ( 'NONE', #19293, 3.309500000000001663 ) ;
#48459 = EDGE_CURVE ( 'NONE', #57765, #24986, #39005, .T. ) ;
#48460 = CARTESIAN_POINT ( 'NONE',  ( 11.24754375996996991, 43.18744335144261726, -14.96124022301595424 ) ) ;
#48461 = CIRCLE ( 'NONE', #63985, 7.500000000000003553 ) ;
#48462 = CARTESIAN_POINT ( 'NONE',  ( 16.84999999999999787, 1.533819458162526451E-15, 0.000000000000000000 ) ) ;
#48463 = CARTESIAN_POINT ( 'NONE',  ( -81.46144558510007982, -60.00000000000000000, -27.04857943224691041 ) ) ;
#48465 = EDGE_CURVE ( 'NONE', #24684, #8257, #15012, .T. ) ;
#48464 = VERTEX_POINT ( 'NONE', #105839 ) ;
#48466 = CARTESIAN_POINT ( 'NONE',  ( 12.77564109741936704, -23.94125442111781510, -30.51326413066097487 ) ) ;
#48467 = DIRECTION ( 'NONE',  ( 0.000000000000000000, -1.000000000000000000, 0.000000000000000000 ) ) ;
#48468 = CARTESIAN_POINT ( 'NONE',  ( 94.30024162164785650, -37.70548019052495192, 192.9918295364696235 ) ) ;
#48469 = CARTESIAN_POINT ( 'NONE',  ( -46.96202111036851790, 13.62308641270877985, 14.94990935055617953 ) ) ;
#48470 = CARTESIAN_POINT ( 'NONE',  ( -79.40492842379534011, -60.33402592105881013, 168.9271176041871740 ) ) ;
#48471 = VERTEX_POINT ( 'NONE', #71885 ) ;
#48472 = VERTEX_POINT ( 'NONE', #55157 ) ;
#48473 = ORIENTED_EDGE ( 'NONE', *, *, #23065, .F. ) ;
#48474 = CARTESIAN_POINT ( 'NONE',  ( 34.49859336298668921, 464.8458904554861988, 18.22488476267798774 ) ) ;
#48475 = CARTESIAN_POINT ( 'NONE',  ( -4.999999999999919176, -15.02849299145000472, 13.75080192255916067 ) ) ;
#48476 = SURFACE_STYLE_FILL_AREA ( #97553 ) ;
#48477 = VERTEX_POINT ( 'NONE', #105322 ) ;
#48478 = CARTESIAN_POINT ( 'NONE',  ( 28.17977184163764193, 5.000000000000002665, 0.000000000000000000 ) ) ;
#48479 = CARTESIAN_POINT ( 'NONE',  ( -0.000000000000000000, 46.03420836107012093, -33.38430095398285147 ) ) ;
#48480 = CARTESIAN_POINT ( 'NONE',  ( 69.18888888888888289, 6.915964383211875250E-15, 0.000000000000000000 ) ) ;
#48481 = CARTESIAN_POINT ( 'NONE',  ( -112.7923893646043183, -57.67119337860199124, 188.3631819635289446 ) ) ;
#48482 = CARTESIAN_POINT ( 'NONE',  ( -4.472135954999577834, -65.13579204946555024, 4.000000000000002665 ) ) ;
#48483 = DIRECTION ( 'NONE',  ( 0.000000000000000000, 0.7456561006171790185, 0.6663309835302448914 ) ) ;
#48484 = CARTESIAN_POINT ( 'NONE',  ( 1.469576158976823356E-15, 50.00000000000000000, -73.00000000000001421 ) ) ;
#48485 = FACE_BOUND ( 'NONE', #83545, .T. ) ;
#48486 = CARTESIAN_POINT ( 'NONE',  ( -16.60966916665065085, -29.99999999999998934, -39.45625820571179787 ) ) ;
#48487 = CARTESIAN_POINT ( 'NONE',  ( -12.27152016684560820, -14.21045842199446874, 34.40193250091021326 ) ) ;
#48488 = CARTESIAN_POINT ( 'NONE',  ( -51.93045568178391846, -53.37659915090458895, 59.21916723660311277 ) ) ;
#48489 = CARTESIAN_POINT ( 'NONE',  ( 7.999999999999998224, -27.59374999999999289, 3.313708498984766049 ) ) ;
#48490 = ORIENTED_EDGE ( 'NONE', *, *, #72882, .F. ) ;
#48491 = CARTESIAN_POINT ( 'NONE',  ( -98.44231968215002837, -60.34206883299947322, 196.4449518206358789 ) ) ;
#48492 = LINE ( 'NONE', #56040, #92566 ) ;
#48493 = ORIENTED_EDGE ( 'NONE', *, *, #769, .F. ) ;
#48494 = CARTESIAN_POINT ( 'NONE',  ( -17.71335089818147424, 34.18409044421883181, -23.86027278727303624 ) ) ;
#48495 = CARTESIAN_POINT ( 'NONE',  ( 89.08324256299194133, -38.38303541736249969, -17.92597912426925433 ) ) ;
#48496 = DIRECTION ( 'NONE',  ( -0.000000000000000000, 1.000000000000000000, -0.000000000000000000 ) ) ;
#48497 = CARTESIAN_POINT ( 'NONE',  ( -7.188101187500000044, -11.28125000204838457, -8.802885111219163269E-16 ) ) ;
#48498 = VECTOR ( 'NONE', #43648, 1000.000000000000114 ) ;
#48499 = DIRECTION ( 'NONE',  ( -1.000000000000000000, -1.224606353822377258E-16, -0.000000000000000000 ) ) ;
#48501 = CARTESIAN_POINT ( 'NONE',  ( 85.24653099856575977, -30.00000000000000000, 172.6093818142646796 ) ) ;
#48500 = UNCERTAINTY_MEASURE_WITH_UNIT (LENGTH_MEASURE( 1.000000000000000082E-05 ), #82929, 'distance_accuracy_value', 'NONE');
#48502 = DIRECTION ( 'NONE',  ( 0.000000000000000000, -1.000000000000000000, 0.000000000000000000 ) ) ;
#48503 = CARTESIAN_POINT ( 'NONE',  ( 32.94330508143927716, 1.340359594676612611E-15, 0.000000000000000000 ) ) ;
#48504 = EDGE_CURVE ( 'NONE', #25066, #102350, #45414, .T. ) ;
#48505 = CARTESIAN_POINT ( 'NONE',  ( 43.00000000000000000, 488.9831568219304927, 4.757012338623754388 ) ) ;
#48506 = B_SPLINE_CURVE_WITH_KNOTS ( 'NONE', 3,
 ( #105166, #11492, #68710, #51958 ),
 .UNSPECIFIED., .F., .F.,
 ( 4, 4 ),
 ( 3.469446951953614189E-18, 0.001900242520396456082 ),
 .UNSPECIFIED. ) ;
#48507 = ORIENTED_EDGE ( 'NONE', *, *, #72986, .F. ) ;
#48508 = ORIENTED_EDGE ( 'NONE', *, *, #62756, .F. ) ;
#48509 = CARTESIAN_POINT ( 'NONE',  ( 49.10960368247432228, -32.59430926536067830, 47.09906247322906125 ) ) ;
#48510 = CARTESIAN_POINT ( 'NONE',  ( 6.828042838857774299, 41.63841260098274688, -58.95291818684747653 ) ) ;
#48511 = AXIS2_PLACEMENT_3D ( 'NONE', #49706, #91256, #17366 ) ;
#48512 = EDGE_CURVE ( 'NONE', #64041, #51129, #9656, .T. ) ;
#48513 = CARTESIAN_POINT ( 'NONE',  ( 8.559508646656398767, 51.83514083332404709, 1.531152949374243510 ) ) ;
#48514 = COLOUR_RGB ( '', 0.08235294, 0.09019608, 0.10196078) ;
#48515 = VERTEX_POINT ( 'NONE', #52790 ) ;
#48516 = CARTESIAN_POINT ( 'NONE',  ( -107.5459679601182472, -38.35637404592787902, 134.5943931340658821 ) ) ;
#48517 = EDGE_LOOP ( 'NONE', ( #60426, #48493 ) ) ;
#48518 = CARTESIAN_POINT ( 'NONE',  ( 28.08046125550390926, 34.37078321048628737, -8.021011108984579252 ) ) ;
#48519 = CARTESIAN_POINT ( 'NONE',  ( 98.50113857120987859, -38.35583664951423799, 79.61398634377471240 ) ) ;
#48520 = CARTESIAN_POINT ( 'NONE',  ( 10.94261262135061230, 16.63582817876949704, -9.322719357341762603 ) ) ;
#48521 = CYLINDRICAL_SURFACE ( 'NONE', #3494, 5.000000000000002665 ) ;
#48522 = CARTESIAN_POINT ( 'NONE',  ( 103.7141658930947017, -52.71714772886510758, 149.2188361930400049 ) ) ;
#48523 = CARTESIAN_POINT ( 'NONE',  ( -32.02876608638647582, 439.3983902163913626, 23.59623870271461854 ) ) ;
#48524 = CARTESIAN_POINT ( 'NONE',  ( 22.65274949039523023, 28.20149500596346925, 30.83785112677286477 ) ) ;
#48525 = CARTESIAN_POINT ( 'NONE',  ( -26.72816845841281719, 307.3634948383742085, -8.441436268651763442 ) ) ;
#48526 = CARTESIAN_POINT ( 'NONE',  ( 4.806394388394678252, -64.29623592462039028, 13.02651880581780830 ) ) ;
#48527 = CARTESIAN_POINT ( 'NONE',  ( 79.59876633705728466, -60.00000000000001421, 195.4925107952827545 ) ) ;
#48528 = CARTESIAN_POINT ( 'NONE',  ( -43.04469050570866528, 434.7734435962897805, 9.248231035232430841 ) ) ;
#48529 = VERTEX_POINT ( 'NONE', #11789 ) ;
#48530 = CARTESIAN_POINT ( 'NONE',  ( 58.21454800639202887, -39.49099975802815976, 67.71415432429243708 ) ) ;
#48531 = SURFACE_STYLE_USAGE ( .BOTH. , #24827 ) ;
#48532 = EDGE_CURVE ( 'NONE', #45434, #21657, #89095, .T. ) ;
#48533 = DIRECTION ( 'NONE',  ( -0.000000000000000000, -1.000000000000000000, -0.000000000000000000 ) ) ;
#48534 = AXIS2_PLACEMENT_3D ( 'NONE', #47949, #106181, #98109 ) ;
#48535 = CARTESIAN_POINT ( 'NONE',  ( -5.909135300144294334, -5.000000000000000000, -15.35560945501324248 ) ) ;
#48536 = ORIENTED_EDGE ( 'NONE', *, *, #56547, .F. ) ;
#48538 = DIRECTION ( 'NONE',  ( 0.000000000000000000, 1.000000000000000000, 1.224646799147353207E-16 ) ) ;
#48537 = CARTESIAN_POINT ( 'NONE',  ( -55.91766210057292597, -29.99999999994657074, 79.88469606658499345 ) ) ;
#48539 = CARTESIAN_POINT ( 'NONE',  ( 8.000000000000001776, -3.000000000000000444, -1.047197551196596965 ) ) ;
#48540 = CARTESIAN_POINT ( 'NONE',  ( 23.21665375867825531, 305.7593017747301474, 9.134900160712305706 ) ) ;
#48541 = CARTESIAN_POINT ( 'NONE',  ( 15.59999999999999787, -3.309499999999999886, 4.475777889183790779E-16 ) ) ;
#48542 = CARTESIAN_POINT ( 'NONE',  ( -8.000000000000000000, -31.34374999999999645, -3.313708498984762496 ) ) ;
#48543 = AXIS2_PLACEMENT_3D ( 'NONE', #447, #32889, #80333 ) ;
#48544 = DIRECTION ( 'NONE',  ( 0.000000000000000000, 1.000000000000000000, 0.000000000000000000 ) ) ;
#48545 = AXIS2_PLACEMENT_3D ( 'NONE', #83350, #68789, #84429 ) ;
#48546 = EDGE_CURVE ( 'NONE', #67219, #25066, #82237, .T. ) ;
#48547 = DIRECTION ( 'NONE',  ( 0.000000000000000000, -1.000000000000000000, 0.000000000000000000 ) ) ;
#48548 = ORIENTED_EDGE ( 'NONE', *, *, #70282, .F. ) ;
#48549 = CARTESIAN_POINT ( 'NONE',  ( 83.95431419311037757, -35.95954853935870688, 173.2961117203365404 ) ) ;
#48550 = CARTESIAN_POINT ( 'NONE',  ( 1.444456719620631269, -6.067207855676811867, -13.76482066788863534 ) ) ;
#48551 = DIRECTION ( 'NONE',  ( 0.000000000000000000, -1.000000000000000000, 0.000000000000000000 ) ) ;
#48552 = ORIENTED_EDGE ( 'NONE', *, *, #45410, .F. ) ;
#48553 = DIRECTION ( 'NONE',  ( 0.02699252395738975518, 0.001721171576548164101, -0.9996341536876447442 ) ) ;
#48554 = CARTESIAN_POINT ( 'NONE',  ( 7.464071982068412936, -3.053493056030892383, -19.53076229013005261 ) ) ;
#48555 = CARTESIAN_POINT ( 'NONE',  ( 26.01059492157061115, 35.07599308518503278, -8.179937502207174305 ) ) ;
#48556 = DIRECTION ( 'NONE',  ( 0.000000000000000000, 1.000000000000000000, -0.000000000000000000 ) ) ;
#48557 = CARTESIAN_POINT ( 'NONE',  ( -28.45466774514982333, 11.90937068246394048, -41.11752270887390637 ) ) ;
#48558 = ADVANCED_FACE ( 'NONE', ( #76526 ), #96035, .T. ) ;
#48559 = VERTEX_POINT ( 'NONE', #102411 ) ;
#48560 = FILL_AREA_STYLE ('',( #89574 ) ) ;
#48561 = CARTESIAN_POINT ( 'NONE',  ( 38.18636683152726619, 25.28304573692243551, 13.29490163854971385 ) ) ;
#48562 = SURFACE_STYLE_FILL_AREA ( #15672 ) ;
#48564 = CARTESIAN_POINT ( 'NONE',  ( -11.59717644377422019, 15.61894086526454473, -9.655125550077977792 ) ) ;
#48563 = CARTESIAN_POINT ( 'NONE',  ( -25.20238367481141140, -29.17817727520965931, 38.35064085007479662 ) ) ;
#48565 = CARTESIAN_POINT ( 'NONE',  ( -7.188101187500000044, -12.40625000204838635, -8.802885111219163269E-16 ) ) ;
#48566 = CARTESIAN_POINT ( 'NONE',  ( 19.24564409877616811, 294.6757776630491321, -10.03741501079465515 ) ) ;
#48567 = DIRECTION ( 'NONE',  ( 0.000000000000000000, 0.000000000000000000, 1.000000000000000000 ) ) ;
#48568 = B_SPLINE_CURVE_WITH_KNOTS ( 'NONE', 3,
 ( #79421, #5536, #102646, #21757, #103181, #87530, #94576, #45489 ),
 .UNSPECIFIED., .F., .F.,
 ( 4, 2, 2, 4 ),
 ( 0.000000000000000000, 0.002114848577942575209, 0.003172272866913863031, 0.004229697155885150418 ),
 .UNSPECIFIED. ) ;
#48569 = ORIENTED_EDGE ( 'NONE', *, *, #18802, .T. ) ;
#48570 = CARTESIAN_POINT ( 'NONE',  ( -17.49999999999997513, 49.99999999999970157, 59.56761335716139882 ) ) ;
#48571 = DIRECTION ( 'NONE',  ( 0.000000000000000000, -0.000000000000000000, 1.000000000000000000 ) ) ;
#48572 = AXIS2_PLACEMENT_3D ( 'NONE', #52952, #19579, #85881 ) ;
#48573 = CARTESIAN_POINT ( 'NONE',  ( -9.230092720033631792, 139.8575112583843350, 0.000000000000000000 ) ) ;
#48574 = CARTESIAN_POINT ( 'NONE',  ( -33.00540147334746166, 487.4196752801198613, 9.523982417603901851 ) ) ;
#48575 = EDGE_CURVE ( 'NONE', #69405, #35442, #39115, .T. ) ;
#48576 = CARTESIAN_POINT ( 'NONE',  ( 0.000000000000000000, 70.00000000000000000, 0.000000000000000000 ) ) ;
#48577 = ORIENTED_EDGE ( 'NONE', *, *, #89928, .F. ) ;
#48578 = CARTESIAN_POINT ( 'NONE',  ( -4.815811321232738251, -86.80076707697375582, 3.581116321197038044 ) ) ;
#48579 = FACE_BOUND ( 'NONE', #106499, .T. ) ;
#48581 = ORIENTED_EDGE ( 'NONE', *, *, #64374, .F. ) ;
#48580 = AXIS2_PLACEMENT_3D ( 'NONE', #94595, #35301, #69250 ) ;
#48582 = ADVANCED_FACE ( 'NONE', ( #19949 ), #10200, .F. ) ;
#48583 = CARTESIAN_POINT ( 'NONE',  ( 25.60851123651792705, 48.00000000000000000, -75.29411764705884025 ) ) ;
#48584 = CARTESIAN_POINT ( 'NONE',  ( -24.00311689919816160, 41.61929283342283981, -74.30204191058474805 ) ) ;
#48585 = CARTESIAN_POINT ( 'NONE',  ( -111.0840224819099973, -60.00000000000000711, 152.9628786121542703 ) ) ;
#48586 = CARTESIAN_POINT ( 'NONE',  ( 29.33036678664061014, 18.69950024370078978, -39.65481841613269154 ) ) ;
#48587 = CARTESIAN_POINT ( 'NONE',  ( 43.03265099500004709, 484.2747968070555089, -0.8099405866658345721 ) ) ;
#48588 = LINE ( 'NONE', #39991, #3840 ) ;
#48589 = CARTESIAN_POINT ( 'NONE',  ( -13.09485420365440334, 1.508326549344240153, 14.92433821123424664 ) ) ;
#48591 = CARTESIAN_POINT ( 'NONE',  ( -15.50996574327916022, 2.604740765350743281, 0.8136923573409686750 ) ) ;
#48590 = CARTESIAN_POINT ( 'NONE',  ( 0.000000000000000000, -5.000000000000002665, -75.00000000000001421 ) ) ;
#48592 = CARTESIAN_POINT ( 'NONE',  ( -82.89588075628438446, -46.49890956395007180, 179.0000094130285220 ) ) ;
#48593 = ORIENTED_EDGE ( 'NONE', *, *, #82338, .T. ) ;
#48594 = CARTESIAN_POINT ( 'NONE',  ( 4.852941176470593199, -5.250000000000004441, -70.80672828634229177 ) ) ;
#48595 = ADVANCED_FACE ( 'NONE', ( #92716 ), #16483, .F. ) ;
#48596 = ORIENTED_EDGE ( 'NONE', *, *, #10204, .F. ) ;
#48597 = ORIENTED_EDGE ( 'NONE', *, *, #66044, .T. ) ;
#48598 = DIRECTION ( 'NONE',  ( 0.8191520442889974607, 1.003171929053531649E-16, -0.5735764363510379438 ) ) ;
#48599 =( BOUNDED_CURVE ( )  B_SPLINE_CURVE ( 2, ( #70868, #30426, #62268 ),
 .UNSPECIFIED., .F., .F. ) 
 B_SPLINE_CURVE_WITH_KNOTS ( ( 3, 3 ),
 ( 0.000000000000000000, 1.000000000000000000 ),
 .UNSPECIFIED. ) 
 CURVE ( )  GEOMETRIC_REPRESENTATION_ITEM ( )  RATIONAL_B_SPLINE_CURVE ( ( 1.000000000000000000, 1.857142857142858317, 1.000000000000000000 ) ) 
 REPRESENTATION_ITEM ( '' )  );
#48600 = ADVANCED_BREP_SHAPE_REPRESENTATION ( '', ( #19502, #10728 ), #66175 ) ;
#48601 = TOROIDAL_SURFACE ( 'NONE', #91677, 12.00000000000000711, 3.000000000000000000 ) ;
#48602 = CARTESIAN_POINT ( 'NONE',  ( -2.153051538919529300E-10, 304.8518027762758607, 9.936999415352289589 ) ) ;
#48603 = TOROIDAL_SURFACE ( 'NONE', #67582, 12.00000000000001066, 3.000000000000000000 ) ;
#48604 = CARTESIAN_POINT ( 'NONE',  ( 8.224467148766224867, 36.45870262746186086, 1.229177290248652582E-12 ) ) ;
#48605 = CARTESIAN_POINT ( 'NONE',  ( 5.782876476886952055, -5.000000000000000000, -96.70368651365731694 ) ) ;
#48606 = CARTESIAN_POINT ( 'NONE',  ( 16.33361799548379523, 1.482358050883964840E-15, 0.000000000000000000 ) ) ;
#48607 = CARTESIAN_POINT ( 'NONE',  ( 112.5893299866519897, -60.00000000000007105, 145.0945492492805045 ) ) ;
#48608 = CARTESIAN_POINT ( 'NONE',  ( -109.4306967521916221, -29.99999999999999645, 166.0290040158848797 ) ) ;
#48609 = CIRCLE ( 'NONE', #17626, 57.21727615095610275 ) ;
#48610 = CARTESIAN_POINT ( 'NONE',  ( -62.26494006864544417, -56.86950266710078949, 87.13957684240361345 ) ) ;
#48611 = ORIENTED_EDGE ( 'NONE', *, *, #37577, .F. ) ;
#48612 = CARTESIAN_POINT ( 'NONE',  ( 2.911225856420454949, 38.95261502387059238, 63.66761955064095702 ) ) ;
#48613 = CARTESIAN_POINT ( 'NONE',  ( 104.9932229724631867, -59.99999999999998579, 96.28837625296324632 ) ) ;
#48614 = ORIENTED_EDGE ( 'NONE', *, *, #80414, .T. ) ;
#48615 = CARTESIAN_POINT ( 'NONE',  ( 1.016806655238071233, -53.39687650318582257, 32.78912937680000539 ) ) ;
#48616 = CARTESIAN_POINT ( 'NONE',  ( -7.188101187500000044, -14.28125000204838457, -8.802885111219163269E-16 ) ) ;
#48617 = EDGE_LOOP ( 'NONE', ( #74534, #46865, #23261, #53778, #44046 ) ) ;
#48618 = DIRECTION ( 'NONE',  ( 0.000000000000000000, -1.000000000000000000, 0.000000000000000000 ) ) ;
#48619 = VERTEX_POINT ( 'NONE', #36098 ) ;
#48620 = CARTESIAN_POINT ( 'NONE',  ( 8.929771841637641927, -5.000000000000000000, 6.123233995736768255E-16 ) ) ;
#48621 = CARTESIAN_POINT ( 'NONE',  ( -7.897850199329715437, 1.533397866934074427, -7.634054012537970557 ) ) ;
#48622 = CARTESIAN_POINT ( 'NONE',  ( -110.5108575042119412, -60.00000000000002132, 147.2781094354880338 ) ) ;
#48623 = CARTESIAN_POINT ( 'NONE',  ( 9.215420734788352775, -54.26716484181712019, 23.11721482942554928 ) ) ;
#48624 = CARTESIAN_POINT ( 'NONE',  ( -7.188101187500000044, -29.28125000204838813, -8.802885111219163269E-16 ) ) ;
#48625 = CARTESIAN_POINT ( 'NONE',  ( 43.64647135119551535, 462.3514304094902627, 4.815965046162477670 ) ) ;
#48626 = CARTESIAN_POINT ( 'NONE',  ( 5.744562646538028616, 12.99999999999999289, 4.000000000000000000 ) ) ;
#48627 = CARTESIAN_POINT ( 'NONE',  ( -6.046331486648977460, 53.95713668298893140, -6.273411955836167841 ) ) ;
#48628 = CARTESIAN_POINT ( 'NONE',  ( -11.02516228146338229, -4.987106852743500518, -12.57633211456099787 ) ) ;
#48629 = FACE_OUTER_BOUND ( 'NONE', #10065, .T. ) ;
#48630 = CARTESIAN_POINT ( 'NONE',  ( 9.389245980427306293, -2.447416405268217243, 14.81682632889905626 ) ) ;
#48631 = CARTESIAN_POINT ( 'NONE',  ( -24.46403792248046472, 27.44444016472271031, 32.08006538382075234 ) ) ;
#48632 = EDGE_CURVE ( 'NONE', #85394, #76952, #63323, .T. ) ;
#48633 = CARTESIAN_POINT ( 'NONE',  ( 106.2155570736864547, -59.99999999999999289, 163.8884563533469247 ) ) ;
#48634 = CARTESIAN_POINT ( 'NONE',  ( -33.01570200386896659, -60.31662611196244228, 38.17099334662022159 ) ) ;
#48635 = CARTESIAN_POINT ( 'NONE',  ( -2.321165800182301009, -49.78473794090700721, 102.3911379722517552 ) ) ;
#48636 = CARTESIAN_POINT ( 'NONE',  ( 40.18194788804924400, -39.51852554140211282, 38.87859757349198020 ) ) ;
#48637 = ORIENTED_EDGE ( 'NONE', *, *, #89402, .T. ) ;
#48638 = EDGE_CURVE ( 'NONE', #45881, #34259, #15497, .T. ) ;
#48639 = CARTESIAN_POINT ( 'NONE',  ( 44.26374899284098063, 435.3115877955005431, 11.30001004033899648 ) ) ;
#48640 = CARTESIAN_POINT ( 'NONE',  ( -57.67084418237976706, -38.34431147036926291, 89.26121482714037825 ) ) ;
#48641 = ORIENTED_EDGE ( 'NONE', *, *, #80036, .T. ) ;
#48643 = CARTESIAN_POINT ( 'NONE',  ( -25.95507789760542039, 309.1386286255022924, 10.94030088463808070 ) ) ;
#48642 = DIRECTION ( 'NONE',  ( 0.000000000000000000, 0.000000000000000000, 1.000000000000000000 ) ) ;
#48644 = CARTESIAN_POINT ( 'NONE',  ( 0.000000000000000000, 36.79151656018385097, 0.000000000000000000 ) ) ;
#48645 = CARTESIAN_POINT ( 'NONE',  ( -7.229692795438678488, 41.58551687973270816, -59.68506457723876935 ) ) ;
#48646 = DIRECTION ( 'NONE',  ( -0.5735764363510497121, 0.8191520442889892450, 1.003171929053521665E-16 ) ) ;
#48647 = CARTESIAN_POINT ( 'NONE',  ( -38.56574518832086085, 25.19011887711810260, 12.97560723393621984 ) ) ;
#48649 = CARTESIAN_POINT ( 'NONE',  ( 5.646888413699858944, -88.44974155970389518, 2.040714635159925905 ) ) ;
#48648 = MECHANICAL_DESIGN_GEOMETRIC_PRESENTATION_REPRESENTATION (  '', ( #100560 ), #2137 ) ;
#48650 = CARTESIAN_POINT ( 'NONE',  ( -1.469576158976823947E-15, -25.06250000409677270, 8.000000000000000000 ) ) ;
#48651 = CARTESIAN_POINT ( 'NONE',  ( 100.9404511582781083, -59.99999999999999289, 86.55166955914968696 ) ) ;
#48653 = CARTESIAN_POINT ( 'NONE',  ( -5.363597346089342466, 41.33266196706077267, -58.39526881795508473 ) ) ;
#48652 = AXIS2_PLACEMENT_3D ( 'NONE', #39310, #105609, #23665 ) ;
#48654 = COLOUR_RGB ( '', 0.72549020, 0.75294118, 0.79215686) ;
#48655 = DIRECTION ( 'NONE',  ( 0.000000000000000000, -1.000000000000000000, 0.000000000000000000 ) ) ;
#48656 = CARTESIAN_POINT ( 'NONE',  ( 9.432319653620828248, -4.999999999999999112, -70.68463330170209247 ) ) ;
#48657 = EDGE_LOOP ( 'NONE', ( #81157, #86220, #39690, #26745, #77895 ) ) ;
#48658 = EDGE_CURVE ( 'NONE', #61495, #60319, #101841, .T. ) ;
#48659 = CARTESIAN_POINT ( 'NONE',  ( -96.64935847557207182, -29.99999999999981171, 191.1839691282570186 ) ) ;
#48660 = ORIENTED_EDGE ( 'NONE', *, *, #66248, .T. ) ;
#48661 = CARTESIAN_POINT ( 'NONE',  ( -9.611186809632508599, -57.00672508581456555, 29.76794951015613933 ) ) ;
#48662 = CARTESIAN_POINT ( 'NONE',  ( 8.763392006798923717, 19.59990099439337996, 5.000000000000613731 ) ) ;
#48663 = CARTESIAN_POINT ( 'NONE',  ( 79.82022815836235452, 1.016364837396684119E-14, 0.000000000000000000 ) ) ;
#48664 = CARTESIAN_POINT ( 'NONE',  ( -22.81472563493007399, 27.48372958372127073, -33.14224123365035979 ) ) ;
#48665 = CIRCLE ( 'NONE', #5638, 4.000000000000007105 ) ;
#48666 = CARTESIAN_POINT ( 'NONE',  ( 7.188101187500000044, -25.53125000204838813, 0.000000000000000000 ) ) ;
#48667 = FILL_AREA_STYLE ('',( #89687 ) ) ;
#48668 = EDGE_CURVE ( 'NONE', #8019, #102339, #29591, .T. ) ;
#48669 = CYLINDRICAL_SURFACE ( 'NONE', #96047, 4.000000000000000000 ) ;
#48670 = ORIENTED_EDGE ( 'NONE', *, *, #78441, .F. ) ;
#48672 = ORIENTED_EDGE ( 'NONE', *, *, #52977, .T. ) ;
#48671 = DIRECTION ( 'NONE',  ( -0.000000000000000000, 1.000000000000000000, -0.000000000000000000 ) ) ;
#48673 = CARTESIAN_POINT ( 'NONE',  ( 79.80652143352665462, -53.37714176188983117, 161.8226454331678212 ) ) ;
#48674 = CARTESIAN_POINT ( 'NONE',  ( -32.06611684416825625, 38.95383793066319100, 55.63518754859966720 ) ) ;
#48675 = CARTESIAN_POINT ( 'NONE',  ( 44.46823338009918558, 5.000000000000002665, 0.000000000000000000 ) ) ;
#48676 = VERTEX_POINT ( 'NONE', #101324 ) ;
#48677 = CARTESIAN_POINT ( 'NONE',  ( -56.29028211295952389, 50.00000000000000711, -28.72872561009205938 ) ) ;
#48678 = CARTESIAN_POINT ( 'NONE',  ( -14.59067579026470796, 1.706082412479009269, -3.468700283484645652 ) ) ;
#48679 = CARTESIAN_POINT ( 'NONE',  ( -7.188101187500000933, -12.50000000204838813, -2.977408999572651371 ) ) ;
#48680 = CARTESIAN_POINT ( 'NONE',  ( 8.000086790516061086, 25.99982641893993929, 0.2639471549312826792 ) ) ;
#48682 = CARTESIAN_POINT ( 'NONE',  ( -39.01690548088378563, -57.69424739071683916, 54.12508632231112671 ) ) ;
#48681 = MECHANICAL_DESIGN_GEOMETRIC_PRESENTATION_REPRESENTATION (  '', ( #34954 ), #19423 ) ;
#48683 = CARTESIAN_POINT ( 'NONE',  ( -20.28383506696344085, 302.8321527159674815, -2.004176749255730083 ) ) ;
#48684 = ORIENTED_EDGE ( 'NONE', *, *, #20017, .T. ) ;
#48685 = COLOUR_RGB ( '', 0.09019608, 0.27058824, 0.51372549) ;
#48686 = AXIS2_PLACEMENT_3D ( 'NONE', #20068, #102532, #94457 ) ;
#48687 = LINE ( 'NONE', #16334, #61320 ) ;
#48688 = CARTESIAN_POINT ( 'NONE',  ( 7.493944697689368439, 40.57567825174881904, -59.86116849737391021 ) ) ;
#48689 = EDGE_CURVE ( 'NONE', #103256, #70516, #105050, .T. ) ;
#48690 = CARTESIAN_POINT ( 'NONE',  ( 0.3382572194634697604, 34.18413605192029792, -29.71481628158403865 ) ) ;
#48691 = VERTEX_POINT ( 'NONE', #94839 ) ;
#48692 = CARTESIAN_POINT ( 'NONE',  ( 4.401442555609581635E-16, -29.28125000204838813, -7.188101187500000044 ) ) ;
#48693 = CARTESIAN_POINT ( 'NONE',  ( -6.292450455944076815, -13.05272214707127354, 32.05976969049422820 ) ) ;
#48694 = CARTESIAN_POINT ( 'NONE',  ( -37.50059943756536995, 490.7879993827801286, 12.38039871356563992 ) ) ;
#48695 = CARTESIAN_POINT ( 'NONE',  ( -1.000000000000000222, -51.24679913437124412, 3.817907945684937410 ) ) ;
#48696 = CARTESIAN_POINT ( 'NONE',  ( -8.000000000000000000, -16.34374999999999289, -3.313708498984762496 ) ) ;
#48697 = CARTESIAN_POINT ( 'NONE',  ( 35.04441504084191905, 439.6183875618604020, 24.03893527320687085 ) ) ;
#48698 = APPLICATION_PROTOCOL_DEFINITION ( 'draft international standard', 'automotive_design', 1998, #91391 ) ;
#48699 = CARTESIAN_POINT ( 'NONE',  ( -9.482856158761276077, 32.44307115854724799, 3.177891129109638779 ) ) ;
#48700 = ORIENTED_EDGE ( 'NONE', *, *, #52675, .F. ) ;
#48701 = CARTESIAN_POINT ( 'NONE',  ( -4.999999999269103768, -46.35544566583474335, 40.27905619162775253 ) ) ;
#48702 = CARTESIAN_POINT ( 'NONE',  ( -0.7060372491586903720, 15.23416508904650968, 9.999999999999998224 ) ) ;
#48703 = CARTESIAN_POINT ( 'NONE',  ( 12.13034742782427955, 41.99999999999999289, -93.82352941176471006 ) ) ;
#48704 = CARTESIAN_POINT ( 'NONE',  ( 25.35164555241593476, -27.85376369652950146, -38.37886305012078481 ) ) ;
#48705 = CARTESIAN_POINT ( 'NONE',  ( 66.74444444444444002, 6.915964383211875250E-15, 0.000000000000000000 ) ) ;
#48706 = CARTESIAN_POINT ( 'NONE',  ( 13.88435755492751511, 42.00000000000000000, -90.88030988993200765 ) ) ;
#48707 = ADVANCED_FACE ( 'NONE', ( #10692, #37689 ), #20984, .T. ) ;
#48708 = ORIENTED_EDGE ( 'NONE', *, *, #19561, .F. ) ;
#48709 = DIRECTION ( 'NONE',  ( -0.000000000000000000, -1.000000000000000000, -0.000000000000000000 ) ) ;
#48710 = CARTESIAN_POINT ( 'NONE',  ( 103.7853185863665857, -57.67100931241723316, 91.47519850164491118 ) ) ;
#48711 = EDGE_CURVE ( 'NONE', #94714, #49975, #67170, .T. ) ;
#48712 = CARTESIAN_POINT ( 'NONE',  ( 35.85186990248600125, 464.1122956640385269, 19.44147592471152208 ) ) ;
#48713 = CARTESIAN_POINT ( 'NONE',  ( -9.735143570771413124, 51.35512128393092723, -2.348594097114156565 ) ) ;
#48714 = FACE_BOUND ( 'NONE', #61279, .T. ) ;
#48715 = CARTESIAN_POINT ( 'NONE',  ( 6.516354785991091835E-11, 40.83842593836580903, 65.00000000086684793 ) ) ;
#48716 = CARTESIAN_POINT ( 'NONE',  ( -74.24642577967240697, -59.99999999999999289, 174.6858703907944914 ) ) ;
#48717 = COLOUR_RGB ( '', 0.09019608, 0.27058824, 0.51372549) ;
#48718 = CARTESIAN_POINT ( 'NONE',  ( -40.95595929481465447, 405.2208686710653183, 27.85131585683114963 ) ) ;
#48719 = CARTESIAN_POINT ( 'NONE',  ( -30.55228927099183522, 298.7536840786443690, 10.80461237140096209 ) ) ;
#48720 = CARTESIAN_POINT ( 'NONE',  ( -85.70838396571514295, -32.07329945039565189, 182.3208811495701980 ) ) ;
#48721 = ORIENTED_EDGE ( 'NONE', *, *, #22608, .F. ) ;
#48722 = CARTESIAN_POINT ( 'NONE',  ( 29.69961346318338258, 311.1410465299570660, -8.538517479574506908 ) ) ;
#48723 = EDGE_CURVE ( 'NONE', #26330, #93114, #84414, .T. ) ;
#48724 = ORIENTED_EDGE ( 'NONE', *, *, #62915, .T. ) ;
#48725 = DIRECTION ( 'NONE',  ( -1.000000000000000000, -1.224606353822377258E-16, -0.000000000000000000 ) ) ;
#48726 = CARTESIAN_POINT ( 'NONE',  ( -6.701893397842001221, 41.44328394191487774, -70.59544911652842814 ) ) ;
#48727 = CARTESIAN_POINT ( 'NONE',  ( -84.40081900408691240, -45.27047985170548827, -3.485582449796192250 ) ) ;
#48728 = CARTESIAN_POINT ( 'NONE',  ( 10.41054107240687188, 1.482358050883964840E-15, 0.000000000000000000 ) ) ;
#48729 = CARTESIAN_POINT ( 'NONE',  ( 0.000000000000000000, 0.000000000000000000, -8.553285714285713937 ) ) ;
#48730 = ORIENTED_EDGE ( 'NONE', *, *, #46677, .T. ) ;
#48731 = CARTESIAN_POINT ( 'NONE',  ( -0.9999999999999943379, 0.000000000000000000, 101.0455488498966758 ) ) ;
#48732 = CARTESIAN_POINT ( 'NONE',  ( 13.22785222780199277, 24.11548868975563309, -3.450552616380675452 ) ) ;
#48733 = CARTESIAN_POINT ( 'NONE',  ( 5.820808985959283532, -2.898778190268130493E-12, -21.65942590380460686 ) ) ;
#48734 = DIRECTION ( 'NONE',  ( -0.000000000000000000, -0.000000000000000000, -1.000000000000000000 ) ) ;
#48735 = CARTESIAN_POINT ( 'NONE',  ( -34.13564290404001156, -60.00000000000002132, -42.84076297484070039 ) ) ;
#48736 = CARTESIAN_POINT ( 'NONE',  ( -77.77839600099601114, -39.49706976687358662, 133.3567172694711473 ) ) ;
#48737 = ORIENTED_EDGE ( 'NONE', *, *, #29325, .F. ) ;
#48738 = CARTESIAN_POINT ( 'NONE',  ( 45.38117173420300787, -14.21045842199442077, 49.92181071548740334 ) ) ;
#48739 = CARTESIAN_POINT ( 'NONE',  ( 7.999885325681428405, 88.99977065129938580, 0.2682325777720055426 ) ) ;
#48740 = CARTESIAN_POINT ( 'NONE',  ( 111.7962455800622479, -57.67099614711071354, 192.0613627441538540 ) ) ;
#48741 = EDGE_LOOP ( 'NONE', ( #104045, #61400, #94799, #84879 ) ) ;
#48742 = CARTESIAN_POINT ( 'NONE',  ( 28.08684260795691401, 34.36902632031492999, 8.016442903659967811 ) ) ;
#48743 = DIRECTION ( 'NONE',  ( -1.000000000000000000, -1.224606353822377258E-16, -0.000000000000000000 ) ) ;
#48744 = ORIENTED_EDGE ( 'NONE', *, *, #52281, .T. ) ;
#48745 = CARTESIAN_POINT ( 'NONE',  ( 0.5361747445545236301, 13.87998248976673921, -6.984311481106284525 ) ) ;
#48746 = DIRECTION ( 'NONE',  ( -1.000000000000000000, -0.000000000000000000, -0.000000000000000000 ) ) ;
#48747 = CARTESIAN_POINT ( 'NONE',  ( 5.799999999999999822, -6.928203230275505220, 4.000000000000007994 ) ) ;
#48748 = CARTESIAN_POINT ( 'NONE',  ( 7.188101187499999156, -16.25000000204838813, 2.977408999572654924 ) ) ;
#48749 = CARTESIAN_POINT ( 'NONE',  ( 44.35000000000000142, -3.309499999999999886, 0.000000000000000000 ) ) ;
#48750 = CIRCLE ( 'NONE', #2253, 4.000000000000007105 ) ;
#48751 = CARTESIAN_POINT ( 'NONE',  ( 9.176855344542989457, 84.47039573022591696, -3.973472207155925862 ) ) ;
#48752 = FILL_AREA_STYLE ('',( #15878 ) ) ;
#48753 = ORIENTED_EDGE ( 'NONE', *, *, #15666, .T. ) ;
#48754 = CARTESIAN_POINT ( 'NONE',  ( -16.64348903516521005, 45.88445698070336221, -4.157797401561533768 ) ) ;
#48755 = EDGE_CURVE ( 'NONE', #52756, #28006, #104602, .T. ) ;
#48756 = ORIENTED_EDGE ( 'NONE', *, *, #18727, .F. ) ;
#48757 = CARTESIAN_POINT ( 'NONE',  ( -7.255115699379916627, 41.55406131346213527, -69.27528309631122738 ) ) ;
#48758 = VECTOR ( 'NONE', #29627, 1000.000000000000000 ) ;
#48760 = CARTESIAN_POINT ( 'NONE',  ( 31.41265888251252392, -60.32177928414881052, 37.38922941594847060 ) ) ;
#48759 = CARTESIAN_POINT ( 'NONE',  ( -16.35964837410663364, -14.21045842199427156, 34.56001531359335388 ) ) ;
#48761 = CARTESIAN_POINT ( 'NONE',  ( 30.63716938955784386, 313.5010800886507241, -6.952601511637969800 ) ) ;
#48763 = ORIENTED_EDGE ( 'NONE', *, *, #22339, .T. ) ;
#48762 =( BOUNDED_SURFACE ( )  B_SPLINE_SURFACE ( 2, 3, ( 
 ( #69949, #21419, #36028, #36558, #102309, #54259, #29014, #87202, #54799, #13278, #44081, #102847, #5214, #103890, #30036, #21949, #87732, #3083, #68902, #53236, #60805, #69427, #45677, #19849, #52684, #11687, #86158, #61879, #94774, #61725, #95688, #94651, #52559, #79498, #20797, #28331, #53107, #3498, #70880, #4556, #61207, #12624, #46601, #30446, #63340, #37493 ),
 ( #87080, #86030, #28883, #69822, #21303, #5609, #96234, #70356, #94097, #11563, #29914, #95170, #21832, #54671, #20261, #85483, #61753, #38534, #86564, #12102, #5088, #103774, #53629, #38021, #13154, #45561, #45032, #103252, #77917, #102182, #29398, #4026, #78430, #36954, #102720, #46083, #62281, #71396, #54140, #78964, #62801, #87608, #44494, #13689, #104295, #77382 ),
 ( #36437, #69307, #81081, #65442, #56258, #7717, #14217, #14748, #80547, #56800, #7190, #106410, #34569, #48704, #22364, #23414, #81594, #73511, #17830, #50681, #40625, #75513, #32571, #39593, #83598, #88656, #32031, #99791, #97795, #47121, #22888, #25962, #23960, #1607, #63869, #58821, #40106, #96756, #89193, #105886, #30985, #15293, #48177, #55726, #91712, #72465 ) ),
 .UNSPECIFIED., .F., .F., .F. ) 
 B_SPLINE_SURFACE_WITH_KNOTS ( ( 3, 3 ),
 ( 4, 2, 2, 2, 2, 2, 2, 2, 2, 2, 2, 2, 2, 2, 2, 2, 2, 2, 2, 2, 2, 2, 4 ),
 ( 0.000000000000000000, 1.000000000000000000 ),
 ( 0.000000000000000000, 0.004671298967716180570, 0.009342597935432361139, 0.01868519587086472228, 0.02802779380629708342, 0.03737039174172944456, 0.04671298967716180917, 0.05605558761259416684, 0.06539818554802652451, 0.07006948451574271375, 0.07240513399960080143, 0.07474078348345888911, 0.07941208245117506448, 0.08408338141889125372, 0.09342597935432361833, 0.1027685772897559691, 0.1121111752251883337, 0.1214537731606206983, 0.1307963710960530490, 0.1354676700637692521, 0.1401389690314854275, 0.1448102679992016029, 0.1494815669669177782 ),
 .UNSPECIFIED. ) 
 GEOMETRIC_REPRESENTATION_ITEM ( )  RATIONAL_B_SPLINE_SURFACE ( (
 ( 1.000000000000000000, 1.000000000000000000, 1.000000000000000000, 1.000000000000000000, 1.000000000000000000, 1.000000000000000000, 1.000000000000000000, 1.000000000000000000, 1.000000000000000000, 1.000000000000000000, 1.000000000000000000, 1.000000000000000000, 1.000000000000000000, 1.000000000000000000, 1.000000000000000000, 1.000000000000000000, 1.000000000000000000, 1.000000000000000000, 1.000000000000000000, 1.000000000000000000, 1.000000000000000000, 1.000000000000000000, 1.000000000000000000, 1.000000000000000000, 1.000000000000000000, 1.000000000000000000, 1.000000000000000000, 1.000000000000000000, 1.000000000000000000, 1.000000000000000000, 1.000000000000000000, 1.000000000000000000, 1.000000000000000000, 1.000000000000000000, 1.000000000000000000, 1.000000000000000000, 1.000000000000000000, 1.000000000000000000, 1.000000000000000000, 1.000000000000000000, 1.000000000000000000, 1.000000000000000000, 1.000000000000000000, 1.000000000000000000, 1.000000000000000000, 1.000000000000000000),
 ( 1.857142857142858317, 1.857142857142858317, 1.857142857142858317, 1.857142857142858317, 1.857142857142858317, 1.857142857142858317, 1.857142857142858317, 1.857142857142858317, 1.857142857142858317, 1.857142857142858317, 1.857142857142858317, 1.857142857142858317, 1.857142857142858317, 1.857142857142858317, 1.857142857142858317, 1.857142857142858317, 1.857142857142858317, 1.857142857142858317, 1.857142857142858317, 1.857142857142858317, 1.857142857142858317, 1.857142857142858317, 1.857142857142858317, 1.857142857142858317, 1.857142857142858317, 1.857142857142858317, 1.857142857142858317, 1.857142857142858317, 1.857142857142858317, 1.857142857142858317, 1.857142857142858317, 1.857142857142858317, 1.857142857142858317, 1.857142857142858317, 1.857142857142858317, 1.857142857142858317, 1.857142857142858317, 1.857142857142858317, 1.857142857142860093, 1.857142857142860093, 1.857142857142858317, 1.857142857142858317, 1.857142857142858317, 1.857142857142858317, 1.857142857142858317, 1.857142857142858317),
 ( 1.000000000000000000, 1.000000000000000000, 1.000000000000000000, 1.000000000000000000, 1.000000000000000000, 1.000000000000000000, 1.000000000000000000, 1.000000000000000000, 1.000000000000000000, 1.000000000000000000, 1.000000000000000000, 1.000000000000000000, 1.000000000000000000, 1.000000000000000000, 1.000000000000000000, 1.000000000000000000, 1.000000000000000000, 1.000000000000000000, 1.000000000000000000, 1.000000000000000000, 1.000000000000000000, 1.000000000000000000, 1.000000000000000000, 1.000000000000000000, 1.000000000000000000, 1.000000000000000000, 1.000000000000000000, 1.000000000000000000, 1.000000000000000000, 1.000000000000000000, 1.000000000000000000, 1.000000000000000000, 1.000000000000000000, 1.000000000000000000, 1.000000000000000000, 1.000000000000000000, 1.000000000000000000, 1.000000000000000000, 1.000000000000000000, 1.000000000000000000, 1.000000000000000000, 1.000000000000000000, 1.000000000000000000, 1.000000000000000000, 1.000000000000000000, 1.000000000000000000) ) ) 
 REPRESENTATION_ITEM ( '' )  SURFACE ( )  );
#48764 = ADVANCED_FACE ( 'NONE', ( #6314 ), #95352, .F. ) ;
#48765 = EDGE_CURVE ( 'NONE', #2566, #67515, #55056, .T. ) ;
#48766 = ORIENTED_EDGE ( 'NONE', *, *, #17646, .F. ) ;
#48768 = CARTESIAN_POINT ( 'NONE',  ( 37.55537146824799066, 460.8431059341384639, 2.817977571237513690 ) ) ;
#48767 = CARTESIAN_POINT ( 'NONE',  ( 3.400000000000000355, 0.000000000000000000, -7.259124522925831435 ) ) ;
#48769 = FACE_OUTER_BOUND ( 'NONE', #6879, .T. ) ;
#48770 = CARTESIAN_POINT ( 'NONE',  ( -15.60207464173859648, 302.5584671467747739, -10.06235099409590283 ) ) ;
#48771 = CARTESIAN_POINT ( 'NONE',  ( 20.77592568779148863, -5.000000000000000000, 6.123233995736768255E-16 ) ) ;
#48772 =( BOUNDED_SURFACE ( )  B_SPLINE_SURFACE ( 3, 2, ( 
 ( #11611, #68823, #18688 ),
 ( #67744, #20314, #4074 ),
 ( #69872, #93620, #43998 ),
 ( #61256, #76347, #35408 ),
 ( #52603, #59659, #53160 ),
 ( #100629, #68276, #37005 ),
 ( #102766, #76884, #69352 ),
 ( #51546, #94142, #60212 ),
 ( #19248, #45079, #101172 ),
 ( #84460, #61804, #86077 ),
 ( #35951, #20845, #12674 ),
 ( #27333, #12148, #93078 ),
 ( #77959, #101703, #3000 ),
 ( #3545, #53676, #52075 ) ),
 .UNSPECIFIED., .F., .F., .F. ) 
 B_SPLINE_SURFACE_WITH_KNOTS ( ( 4, 2, 2, 2, 2, 2, 4 ),
 ( 3, 3 ),
 ( -6.682588510331655129E-15, 0.0008334212029357339607, 0.001250131804406942344, 0.001666842405878150510, 0.002083553007349358676, 0.002500263608820566842, 0.003333684811762983608 ),
 ( 0.000000000000000000, 1.000000000000000000 ),
 .UNSPECIFIED. ) 
 GEOMETRIC_REPRESENTATION_ITEM ( )  RATIONAL_B_SPLINE_SURFACE ( (
 ( 1.000000000000000000, 0.8805984182408446159, 1.000000000000000000),
 ( 1.000000000000000000, 0.8998845875341654477, 1.000000000000000000),
 ( 1.000000000000000000, 0.9147006518920367535, 1.000000000000000000),
 ( 1.000000000000000000, 0.9294517919825534547, 1.000000000000000000),
 ( 1.000000000000000000, 0.9330010648506072979, 1.000000000000000000),
 ( 1.000000000000000000, 0.9375969056690098835, 1.000000000000000000),
 ( 1.000000000000000000, 0.9385966513831063285, 1.000000000000000000),
 ( 1.000000000000000000, 0.9384391173341486425, 1.000000000000000000),
 ( 1.000000000000000000, 0.9372974232555458807, 1.000000000000000000),
 ( 1.000000000000000000, 0.9336465948887834321, 1.000000000000000000),
 ( 1.000000000000000000, 0.9311806706621335028, 1.000000000000000000),
 ( 1.000000000000000000, 0.9227779475329482839, 1.000000000000000000),
 ( 1.000000000000000000, 0.9161682460698783448, 1.000000000000000000),
 ( 1.000000000000000000, 0.9103180234519290259, 1.000000000000000000) ) ) 
 REPRESENTATION_ITEM ( '' )  SURFACE ( )  );
#48773 = CARTESIAN_POINT ( 'NONE',  ( 1.249410016421840464, 45.80241883944731995, 17.33540574942934143 ) ) ;
#48774 = CARTESIAN_POINT ( 'NONE',  ( -7.500000000000001776, 2.932633423934438710, -0.4709827563909262937 ) ) ;
#48775 = ORIENTED_EDGE ( 'NONE', *, *, #81840, .F. ) ;
#48776 = CARTESIAN_POINT ( 'NONE',  ( 8.319959379298547120, -59.99999999999998579, -42.48049722093006864 ) ) ;
#48777 = CARTESIAN_POINT ( 'NONE',  ( -10.12154985177026845, 46.15835141668621588, 12.90779740156129130 ) ) ;
#48778 = CARTESIAN_POINT ( 'NONE',  ( 38.09999999999999432, 3.309500000000003439, 0.000000000000000000 ) ) ;
#48779 = CYLINDRICAL_SURFACE ( 'NONE', #63384, 7.000000000000000000 ) ;
#48780 = CARTESIAN_POINT ( 'NONE',  ( -5.000000000000000000, -32.50000000000000000, 12.61250543006184088 ) ) ;
#48781 = ORIENTED_EDGE ( 'NONE', *, *, #75060, .F. ) ;
#48782 = EDGE_CURVE ( 'NONE', #78936, #63464, #20723, .T. ) ;
#48783 = VERTEX_POINT ( 'NONE', #54870 ) ;
#48784 = VERTEX_POINT ( 'NONE', #87799 ) ;
#48785 = CARTESIAN_POINT ( 'NONE',  ( 1.090085246657715112, 54.05151059601869434, 8.383057650847046460 ) ) ;
#48786 = FACE_OUTER_BOUND ( 'NONE', #73983, .T. ) ;
#48787 = CARTESIAN_POINT ( 'NONE',  ( -35.05824969151932891, 439.1559171757481863, 24.08323619564622931 ) ) ;
#48788 = DIRECTION ( 'NONE',  ( 0.000000000000000000, 0.000000000000000000, -1.000000000000000000 ) ) ;
#48789 = CARTESIAN_POINT ( 'NONE',  ( -37.63230006911589953, 374.2148764567931494, 4.687993092313281984 ) ) ;
#48790 = CARTESIAN_POINT ( 'NONE',  ( -4.821429483474614308, -68.14062186280141020, 13.85322958606745658 ) ) ;
#48791 = CARTESIAN_POINT ( 'NONE',  ( -46.00000000000000000, 488.0078051104092651, -0.5538049991128992655 ) ) ;
#48792 = CARTESIAN_POINT ( 'NONE',  ( 12.50000000000000355, 27.29089671806294248, -44.83733606656386428 ) ) ;
#48793 = EDGE_LOOP ( 'NONE', ( #30990, #98819, #45320, #5176, #69978, #18774, #26699 ) ) ;
#48794 = ADVANCED_FACE ( 'NONE', ( #13879 ), #53383, .T. ) ;
#48795 = CARTESIAN_POINT ( 'NONE',  ( 30.93151921796046011, 9.249586871975902014, 40.69907933257861998 ) ) ;
#48796 = ORIENTED_EDGE ( 'NONE', *, *, #47551, .T. ) ;
#48797 = CARTESIAN_POINT ( 'NONE',  ( 8.881504343373315180, 51.45494909527817384, -3.999881655714555784 ) ) ;
#48798 = CARTESIAN_POINT ( 'NONE',  ( 0.000000000000000000, 0.000000000000000000, -10.00000000000000000 ) ) ;
#48799 = FILL_AREA_STYLE ('',( #9947 ) ) ;
#48800 = CONICAL_SURFACE ( 'NONE', #103929, 5.000000000000010658, 0.9599310885968697082 ) ;
#48801 = ADVANCED_FACE ( 'NONE', ( #14402 ), #27554, .T. ) ;
#48802 = CARTESIAN_POINT ( 'NONE',  ( -8.348350756690260610, -59.99999999999997158, 33.88065270824813524 ) ) ;
#48803 = CARTESIAN_POINT ( 'NONE',  ( 65.24931495339168919, -25.57815227503792244, 79.70468693739232435 ) ) ;
#48804 = AXIS2_PLACEMENT_3D ( 'NONE', #20935, #53771, #80161 ) ;
#48805 = ORIENTED_EDGE ( 'NONE', *, *, #77588, .F. ) ;
#48806 = CARTESIAN_POINT ( 'NONE',  ( 17.50000000000002842, 48.19572006404330722, 64.09945636913033695 ) ) ;
#48807 = CIRCLE ( 'NONE', #29912, 3.400000000000000355 ) ;
#48808 = LINE ( 'NONE', #104954, #4136 ) ;
#48809 = CARTESIAN_POINT ( 'NONE',  ( -69.44743540119901581, -57.67117814800237596, -34.85819734733303221 ) ) ;
#48810 = ORIENTED_EDGE ( 'NONE', *, *, #73688, .F. ) ;
#48811 =( NAMED_UNIT ( * ) PLANE_ANGLE_UNIT ( ) SI_UNIT ( $, .RADIAN. ) );
#48812 = CARTESIAN_POINT ( 'NONE',  ( 47.78256487607184511, 15.50824688150972008, 16.83670797542556130 ) ) ;
#48813 = CARTESIAN_POINT ( 'NONE',  ( -37.67950550370962048, 491.6872717898309020, 12.48612654748556494 ) ) ;
#48814 = CARTESIAN_POINT ( 'NONE',  ( -1.469576158976823947E-15, -25.06250000409677270, 8.000000000000000000 ) ) ;
#48815 = CARTESIAN_POINT ( 'NONE',  ( -4.175893272574848325, -4.999999999999998224, 7.137815226409911951 ) ) ;
#48816 = CARTESIAN_POINT ( 'NONE',  ( -1.000000000000002442, -4.000000000000000000, 27.00000000000000000 ) ) ;
#48817 = CARTESIAN_POINT ( 'NONE',  ( 6.162888688655344893, 3.752776749732562589, -6.500000000000000888 ) ) ;
#48818 = CARTESIAN_POINT ( 'NONE',  ( -10.52078253383812267, 6.756245462352918452, 5.000000000000000888 ) ) ;
#48819 = CARTESIAN_POINT ( 'NONE',  ( 8.866506694866188809, 0.000000000000000000, 4.000000000000000888 ) ) ;
#48820 = PRESENTATION_LAYER_ASSIGNMENT (  '', '', ( #14410 ) ) ;
#48821 =( LENGTH_UNIT ( ) NAMED_UNIT ( * ) SI_UNIT ( .MILLI., .METRE. ) );
#48822 = ORIENTED_EDGE ( 'NONE', *, *, #80082, .T. ) ;
#48823 = DIRECTION ( 'NONE',  ( 0.000000000000000000, 0.000000000000000000, 1.000000000000000000 ) ) ;
#48824 = CARTESIAN_POINT ( 'NONE',  ( 13.37207953394533355, 1.482358050883964840E-15, 0.000000000000000000 ) ) ;
#48825 = CARTESIAN_POINT ( 'NONE',  ( -4.999999999999998224, -31.04507124266364926, -0.1867410044140281056 ) ) ;
#48826 = CIRCLE ( 'NONE', #71250, 4.000000000000001776 ) ;
#48827 = CARTESIAN_POINT ( 'NONE',  ( -94.02161711668794908, -30.00000000000000000, 191.2771078561046352 ) ) ;
#48828 = ADVANCED_FACE ( 'NONE', ( #67244 ), #56995, .T. ) ;
#48829 = PRESENTATION_LAYER_ASSIGNMENT (  '', '', ( #95366 ) ) ;
#48830 = AXIS2_PLACEMENT_3D ( 'NONE', #71216, #13501, #45370 ) ;
#48831 = DIRECTION ( 'NONE',  ( -0.000000000000000000, -1.000000000000000000, -0.000000000000000000 ) ) ;
#48832 = CARTESIAN_POINT ( 'NONE',  ( 56.10950871050302879, -57.67607768850538719, 94.75155346926845823 ) ) ;
#48834 = CARTESIAN_POINT ( 'NONE',  ( -9.742515530865327733, 7.313333228401042163, 1.762264882286370682 ) ) ;
#48833 = CARTESIAN_POINT ( 'NONE',  ( 15.90423112858387711, -2.036632359883284504, 14.86380772883778789 ) ) ;
#48835 = EDGE_CURVE ( 'NONE', #13365, #9366, #22386, .T. ) ;
#48836 = EDGE_CURVE ( 'NONE', #66259, #8430, #81792, .T. ) ;
#48837 = CARTESIAN_POINT ( 'NONE',  ( 8.958840525176039904, -22.36732914119846072, -38.54358237171171453 ) ) ;
#48838 = CARTESIAN_POINT ( 'NONE',  ( -1.218909386241671555, 43.73109126565793048, 17.18057086054097127 ) ) ;
#48839 = DIRECTION ( 'NONE',  ( -1.000000000000000000, -1.224606353822377258E-16, -0.000000000000000000 ) ) ;
#48840 = CARTESIAN_POINT ( 'NONE',  ( -28.18018267510046826, -60.00000000000001421, 42.21498033703696962 ) ) ;
#48841 = CARTESIAN_POINT ( 'NONE',  ( 13.57036353025074682, 20.18065266528832069, 6.968136590762834537 ) ) ;
#48842 = CARTESIAN_POINT ( 'NONE',  ( 0.000000000000000000, 24.35682532067546902, -46.94949242731048145 ) ) ;
#48843 = CARTESIAN_POINT ( 'NONE',  ( -86.67732985869325546, -50.12485329941275580, 191.5830762183649938 ) ) ;
#48844 = ORIENTED_EDGE ( 'NONE', *, *, #50377, .F. ) ;
#48845 = CARTESIAN_POINT ( 'NONE',  ( 17.50000000000004974, 49.76444793455075200, 62.19248936617555046 ) ) ;
#48846 = CARTESIAN_POINT ( 'NONE',  ( 12.31569210610433274, -4.628390024190414564, 20.34132785121827780 ) ) ;
#48847 = CARTESIAN_POINT ( 'NONE',  ( -9.346815707592632805, -53.40262838734317796, 32.79379019251283012 ) ) ;
#48848 = EDGE_CURVE ( 'NONE', #44820, #9732, #42961, .T. ) ;
#48849 = FACE_OUTER_BOUND ( 'NONE', #60664, .T. ) ;
#48851 = CARTESIAN_POINT ( 'NONE',  ( 0.9330442100808692407, -70.05675763226146557, 13.03100537459355124 ) ) ;
#48850 = CARTESIAN_POINT ( 'NONE',  ( 33.00000000000000000, 500.0000000000002274, -15.00000000000000711 ) ) ;
#48852 = EDGE_LOOP ( 'NONE', ( #104359, #7540, #102546, #36353 ) ) ;
#48854 = SURFACE_STYLE_USAGE ( .BOTH. , #89869 ) ;
#48853 = AXIS2_PLACEMENT_3D ( 'NONE', #73429, #22804, #65359 ) ;
#48855 = CARTESIAN_POINT ( 'NONE',  ( -7.499143977330837707, -3.006661276316075604, -20.23006715386054566 ) ) ;
#48856 = DIRECTION ( 'NONE',  ( -0.000000000000000000, 1.000000000000000000, -0.000000000000000000 ) ) ;
#48857 = CARTESIAN_POINT ( 'NONE',  ( 28.95612569419542126, 306.6521615867090418, -9.146490758560222645 ) ) ;
#48858 = CARTESIAN_POINT ( 'NONE',  ( 22.61650669486618526, 1.474610560812782335E-15, 0.000000000000000000 ) ) ;
#48859 = SURFACE_SIDE_STYLE ('',( #8945 ) ) ;
#48860 = CARTESIAN_POINT ( 'NONE',  ( 73.51724252604583398, -60.00000000000000711, 167.3604022711870982 ) ) ;
#48861 = CARTESIAN_POINT ( 'NONE',  ( 109.5916899561874942, -30.00000000000003197, 172.2594225519244446 ) ) ;
#48862 = CARTESIAN_POINT ( 'NONE',  ( -35.69739812508499455, 430.4862580793411553, 4.964222856391316441 ) ) ;
#48863 = ORIENTED_EDGE ( 'NONE', *, *, #6280, .T. ) ;
#48864 = DIRECTION ( 'NONE',  ( -0.5735764363510497121, 0.8191520442889892450, 1.003171929053521665E-16 ) ) ;
#48865 = CARTESIAN_POINT ( 'NONE',  ( -9.989113211954183669, 253.9729927354898393, 0.5334031035449283698 ) ) ;
#48866 = SURFACE_STYLE_USAGE ( .BOTH. , #91488 ) ;
#48867 = CIRCLE ( 'NONE', #2385, 5.000000000000002665 ) ;
#48869 = CARTESIAN_POINT ( 'NONE',  ( 35.58361799548379167, 1.482358050883964840E-15, 0.000000000000000000 ) ) ;
#48868 = CARTESIAN_POINT ( 'NONE',  ( 28.84074934710125859, -30.00000000000002842, 39.52209614246421410 ) ) ;
#48870 = CARTESIAN_POINT ( 'NONE',  ( 3.352941176470599860, -1.200583151104954061, 104.5794940929807524 ) ) ;
#48871 = CARTESIAN_POINT ( 'NONE',  ( 43.99367409911575777, 462.7719748078419002, 5.584664003622480166 ) ) ;
#48872 = ORIENTED_EDGE ( 'NONE', *, *, #33227, .T. ) ;
#48873 = COLOUR_RGB ( '', 0.40784314, 0.44705882, 0.49803922) ;
#48874 = CARTESIAN_POINT ( 'NONE',  ( -22.55365577865696736, 305.4547471613416292, 9.067395197859438483 ) ) ;
#48875 = CIRCLE ( 'NONE', #62690, 6.499999999999999112 ) ;
#48876 = ORIENTED_EDGE ( 'NONE', *, *, #39029, .T. ) ;
#48877 = CARTESIAN_POINT ( 'NONE',  ( 16.08349330513380337, 1.593028355512270962E-15, 0.000000000000000000 ) ) ;
#48878 = LINE ( 'NONE', #42940, #1934 ) ;
#48879 = ORIENTED_EDGE ( 'NONE', *, *, #89799, .F. ) ;
#48880 = CARTESIAN_POINT ( 'NONE',  ( 6.386171959437453083, -11.88579060466483561, 10.72108492130595359 ) ) ;
#48881 = CARTESIAN_POINT ( 'NONE',  ( -60.70436703292030245, -60.00000000001957545, 111.1961515286286613 ) ) ;
#48882 = LINE ( 'NONE', #50478, #30802 ) ;
#48883 = CARTESIAN_POINT ( 'NONE',  ( 81.98299855092518840, -60.00000000000000000, 198.0498435237767012 ) ) ;
#48885 = CARTESIAN_POINT ( 'NONE',  ( 16.63567752523875853, -32.51137318948865129, 29.53593408679408228 ) ) ;
#48884 = CARTESIAN_POINT ( 'NONE',  ( -107.9655701563618067, -29.99999999999997158, 188.7577781645654795 ) ) ;
#48887 = CARTESIAN_POINT ( 'NONE',  ( 97.36093972260707119, -38.00000000000009237, 192.7743595253038791 ) ) ;
#48886 = UNCERTAINTY_MEASURE_WITH_UNIT (LENGTH_MEASURE( 1.000000000000000082E-05 ), #114, 'distance_accuracy_value', 'NONE');
#48888 = DIRECTION ( 'NONE',  ( -0.000000000000000000, -1.000000000000000000, -0.000000000000000000 ) ) ;
#48889 = EDGE_CURVE ( 'NONE', #31781, #57508, #26290, .T. ) ;
#48890 = CARTESIAN_POINT ( 'NONE',  ( -44.43505828091571175, -22.24746064786846134, 38.44332992766335622 ) ) ;
#48891 = CARTESIAN_POINT ( 'NONE',  ( 10.73176661990081371, 1.340359594676612611E-15, 0.000000000000000000 ) ) ;
#48892 = ORIENTED_EDGE ( 'NONE', *, *, #93163, .F. ) ;
#48893 = FILL_AREA_STYLE ('',( #90439 ) ) ;
#48894 = DIRECTION ( 'NONE',  ( -1.000000000000000000, 0.000000000000000000, 0.000000000000000000 ) ) ;
#48895 = CARTESIAN_POINT ( 'NONE',  ( 6.362732954939756880, -11.89495883945591359, 10.82964177580675980 ) ) ;
#48896 = CARTESIAN_POINT ( 'NONE',  ( 0.05533025579361913748, 6.264553569211839701, -2.149474931388137833 ) ) ;
#48897 = CARTESIAN_POINT ( 'NONE',  ( 18.67440746815751851, 303.6203069488627193, -10.04920595787936755 ) ) ;
#48898 = CARTESIAN_POINT ( 'NONE',  ( 30.35537264529554946, 338.7115663565144246, 18.05293407820170515 ) ) ;
#48899 = ORIENTED_EDGE ( 'NONE', *, *, #43163, .T. ) ;
#48900 = CARTESIAN_POINT ( 'NONE',  ( 3.857142857142846992, -48.79941684889506348, 103.1763305333244176 ) ) ;
#48901 = ORIENTED_EDGE ( 'NONE', *, *, #60962, .F. ) ;
#48902 = CARTESIAN_POINT ( 'NONE',  ( 80.85658148696911951, -30.00000000000000000, 6.669769987989186966 ) ) ;
#48903 = CARTESIAN_POINT ( 'NONE',  ( 18.89111011270470541, 41.89281849971280280, -81.21350009779806101 ) ) ;
#48904 = AXIS2_PLACEMENT_3D ( 'NONE', #17284, #15139, #31878 ) ;
#48905 = CARTESIAN_POINT ( 'NONE',  ( 12.39578842395471803, -8.431745484732024565, -0.8377008405913674016 ) ) ;
#48906 = CARTESIAN_POINT ( 'NONE',  ( 19.32152200343512760, 18.64316884711617561, -33.52312678240317467 ) ) ;
#48907 = CARTESIAN_POINT ( 'NONE',  ( 94.31383618571270233, -29.99999999999999645, 113.8495007026067611 ) ) ;
#48908 =( BOUNDED_SURFACE ( )  B_SPLINE_SURFACE ( 3, 2, ( 
 ( #76599, #2709, #91221 ),
 ( #101425, #60455, #93330 ),
 ( #52321, #36199, #85234 ),
 ( #44249, #77141, #99263 ) ),
 .UNSPECIFIED., .F., .F., .F. ) 
 B_SPLINE_SURFACE_WITH_KNOTS ( ( 4, 4 ),
 ( 3, 3 ),
 ( 2.632442874794804766E-16, 0.0002132038012140852017 ),
 ( 0.000000000000000000, 1.000000000000000000 ),
 .UNSPECIFIED. ) 
 GEOMETRIC_REPRESENTATION_ITEM ( )  RATIONAL_B_SPLINE_SURFACE ( (
 ( 1.000000000000000000, 0.8360809698953636238, 1.000000000000000000),
 ( 1.000000000000000000, 0.8350457441348965171, 1.000000000000000000),
 ( 1.000000000000000000, 0.8339645259288112067, 1.000000000000000000),
 ( 1.000000000000000000, 0.8328393170034699144, 1.000000000000000000) ) ) 
 REPRESENTATION_ITEM ( '' )  SURFACE ( )  );
#48909 = AXIS2_PLACEMENT_3D ( 'NONE', #61322, #96343, #103362 ) ;
#48910 = DIRECTION ( 'NONE',  ( -0.000000000000000000, 1.000000000000000000, -0.000000000000000000 ) ) ;
#48911 = EDGE_LOOP ( 'NONE', ( #37151, #82161, #28054, #52865, #100493 ) ) ;
#48912 = ORIENTED_EDGE ( 'NONE', *, *, #77644, .T. ) ;
#48913 = EDGE_LOOP ( 'NONE', ( #103519, #98246, #61324, #98272 ) ) ;
#48914 = CARTESIAN_POINT ( 'NONE',  ( 5.500000000000641265, 42.00000000000000000, -59.88032989331720302 ) ) ;
#48915 = CARTESIAN_POINT ( 'NONE',  ( -6.757705282517541434, 41.35007050579768162, -70.67351639275690900 ) ) ;
#48916 = CARTESIAN_POINT ( 'NONE',  ( -39.61570363597765976, 464.1137630033862820, 18.30708429227111367 ) ) ;
#48917 = ORIENTED_EDGE ( 'NONE', *, *, #34332, .F. ) ;
#48918 = CARTESIAN_POINT ( 'NONE',  ( 9.948181520647857212, 108.8689280276037863, 1.049088206181482574 ) ) ;
#48919 = ORIENTED_EDGE ( 'NONE', *, *, #90778, .T. ) ;
#48920 = FACE_OUTER_BOUND ( 'NONE', #55730, .T. ) ;
#48921 = CARTESIAN_POINT ( 'NONE',  ( 82.14726820479680214, -38.83665063316719568, 196.0510034214655946 ) ) ;
#48922 = CARTESIAN_POINT ( 'NONE',  ( 6.162888688655344005, 3.752776749732565253, 6.499999999999997335 ) ) ;
#48923 = CARTESIAN_POINT ( 'NONE',  ( 38.31672866701944002, 310.9721894403955389, 5.785870559332880525 ) ) ;
#48924 = PRESENTATION_STYLE_ASSIGNMENT (( #16044 ) ) ;
#48925 = EDGE_CURVE ( 'NONE', #25099, #88621, #86689, .T. ) ;
#48926 = EDGE_CURVE ( 'NONE', #67342, #33663, #89571, .T. ) ;
#48927 = DIRECTION ( 'NONE',  ( 0.000000000000000000, 0.000000000000000000, -1.000000000000000000 ) ) ;
#48928 = CARTESIAN_POINT ( 'NONE',  ( -40.71513924616806435, 459.9692486989940789, 1.994549889840158130 ) ) ;
#48929 = CARTESIAN_POINT ( 'NONE',  ( -4.928386788250817219, -48.42812442315221944, 104.2441249819463280 ) ) ;
#48930 = FACE_OUTER_BOUND ( 'NONE', #91238, .T. ) ;
#48932 = B_SPLINE_CURVE_WITH_KNOTS ( 'NONE', 3,
 ( #32090, #80080, #46147, #38085, #14812, #73035, #70942, #88721, #103834, #24017, #29979, #54735, #62867, #105945, #64453, #95752, #14281, #63930, #72000, #97326, #89253, #21894, #40159, #87671 ),
 .UNSPECIFIED., .F., .F.,
 ( 4, 2, 2, 2, 2, 2, 2, 2, 2, 2, 2, 4 ),
 ( 0.004982639409921950195, 0.005234721249241282466, 0.005486803088560614737, 0.005990966767199287953, 0.006495130445837961168, 0.006999294124476635251, 0.007251375963795970991, 0.007503457803115307599, 0.008007621481753979947, 0.008511785160392651428, 0.008763866999711987169, 0.009015948839031322909 ),
 .UNSPECIFIED. ) ;
#48931 = CIRCLE ( 'NONE', #66197, 8.500000000000000000 ) ;
#48933 = CARTESIAN_POINT ( 'NONE',  ( -5.482452937080444677, 5.333397824891131123, 5.000000000000000888 ) ) ;
#48934 = ORIENTED_EDGE ( 'NONE', *, *, #43685, .T. ) ;
#48935 = DIRECTION ( 'NONE',  ( 1.000000000000000000, 1.224606353822377258E-16, 0.000000000000000000 ) ) ;
#48937 = CARTESIAN_POINT ( 'NONE',  ( -22.88986873834216595, 295.1619009228529649, 10.00292581962222549 ) ) ;
#48936 = PRESENTATION_STYLE_ASSIGNMENT (( #25247 ) ) ;
#48938 = CARTESIAN_POINT ( 'NONE',  ( 7.561938253469114635, 54.28095178519542685, -2.009802758568550285 ) ) ;
#48939 = LINE ( 'NONE', #31225, #19806 ) ;
#48940 = CARTESIAN_POINT ( 'NONE',  ( -8.000000000000000000, -11.84374999999999289, -3.313708498984762496 ) ) ;
#48941 = CARTESIAN_POINT ( 'NONE',  ( 31.34101644064316616, -33.33332329661044469, 41.37796191375046817 ) ) ;
#48942 = CARTESIAN_POINT ( 'NONE',  ( 1.175710136697877717, 302.5234377367743264, 9.930896799880603254 ) ) ;
#48944 = B_SPLINE_CURVE_WITH_KNOTS ( 'NONE', 3,
 ( #59899, #92770, #10771, #43690, #95972, #45827, #70095, #86831 ),
 .UNSPECIFIED., .F., .F.,
 ( 4, 2, 2, 4 ),
 ( 5.204170427930421283E-18, 0.002631563437787210521, 0.003947345156680811228, 0.005263126875574411501 ),
 .UNSPECIFIED. ) ;
#48943 = STYLED_ITEM ( 'NONE', ( #7814 ), #87198 ) ;
#48945 =( LENGTH_UNIT ( ) NAMED_UNIT ( * ) SI_UNIT ( .MILLI., .METRE. ) );
#48946 = ORIENTED_EDGE ( 'NONE', *, *, #79774, .F. ) ;
#48947 = CARTESIAN_POINT ( 'NONE',  ( 85.39226384298076766, -35.72026385061843712, 183.0101103138053986 ) ) ;
#48948 = CARTESIAN_POINT ( 'NONE',  ( 1.749942564367553022, 15.56091200510339512, -9.852211596319794040 ) ) ;
#48949 = CARTESIAN_POINT ( 'NONE',  ( -9.433863491267240775, 141.8798491995066797, 4.999999999999050537 ) ) ;
#48950 = ORIENTED_EDGE ( 'NONE', *, *, #41698, .F. ) ;
#48951 = STYLED_ITEM ( 'NONE', ( #98488 ), #85152 ) ;
#48952 = CARTESIAN_POINT ( 'NONE',  ( 91.53261005776035120, -57.66219477115423331, -20.10647474121806155 ) ) ;
#48953 = CARTESIAN_POINT ( 'NONE',  ( 34.53029562236230277, 437.2884171348799782, 5.234332900499188312 ) ) ;
#48954 = SURFACE_STYLE_FILL_AREA ( #6378 ) ;
#48955 = CARTESIAN_POINT ( 'NONE',  ( -81.48731548190207263, -30.00000000000001066, -3.427914186170737398 ) ) ;
#48956 = CARTESIAN_POINT ( 'NONE',  ( 28.56680886105595008, 18.54011861096320501, 40.29036177351405712 ) ) ;
#48957 = CARTESIAN_POINT ( 'NONE',  ( -2.094395098902661179, -4.999999999999998224, 8.000000000000000000 ) ) ;
#48958 = CARTESIAN_POINT ( 'NONE',  ( -3.750000000000007105, 6.495190528383286477, 1.734723475976807094E-15 ) ) ;
#48960 = CARTESIAN_POINT ( 'NONE',  ( 5.260074602449203133E-16, -0.7818963811860513147, -8.000000000000000000 ) ) ;
#48959 = DIRECTION ( 'NONE',  ( 1.000000000000000000, 0.000000000000000000, 0.000000000000000000 ) ) ;
#48961 = DIRECTION ( 'NONE',  ( 0.000000000000000000, 0.000000000000000000, 1.000000000000000000 ) ) ;
#48962 = CARTESIAN_POINT ( 'NONE',  ( -31.33350209457356428, 438.6527987165884497, 22.86578116056119825 ) ) ;
#48963 = CARTESIAN_POINT ( 'NONE',  ( 5.982126593009819970, -81.02665772107070552, 0.5333292889181888707 ) ) ;
#48964 = CARTESIAN_POINT ( 'NONE',  ( -8.400251092734315250, -22.83500361551703861, -30.52644813539184199 ) ) ;
#48965 = CYLINDRICAL_SURFACE ( 'NONE', #58030, 2.000000000000001776 ) ;
#48966 = CARTESIAN_POINT ( 'NONE',  ( -99.53543709402866568, -38.00000000000000000, 191.3481644649123155 ) ) ;
#48967 = B_SPLINE_CURVE_WITH_KNOTS ( 'NONE', 3,
 ( #5048, #37981, #27774, #20215, #85435, #61716, #11517, #12060 ),
 .UNSPECIFIED., .F., .F.,
 ( 4, 2, 2, 4 ),
 ( 0.007886720825438776200, 0.009850969036564001177, 0.01181521724768922615, 0.01574371366993967264 ),
 .UNSPECIFIED. ) ;
#48968 = VECTOR ( 'NONE', #54929, 1000.000000000000000 ) ;
#48969 = VERTEX_POINT ( 'NONE', #51028 ) ;
#48970 = FACE_OUTER_BOUND ( 'NONE', #9096, .T. ) ;
#48971 = FILL_AREA_STYLE ('',( #75389 ) ) ;
#48972 = CARTESIAN_POINT ( 'NONE',  ( 7.922281120364393914, -4.573931137438281169, -8.047472243342934206 ) ) ;
#48973 = ADVANCED_FACE ( 'NONE', ( #83941 ), #62026, .T. ) ;
#48974 = CARTESIAN_POINT ( 'NONE',  ( -31.20322697673447720, -22.08705006449989838, -31.98265270787211634 ) ) ;
#48975 = AXIS2_PLACEMENT_3D ( 'NONE', #98694, #1040, #57699 ) ;
#48976 = EDGE_CURVE ( 'NONE', #13541, #52531, #51667, .T. ) ;
#48978 = CARTESIAN_POINT ( 'NONE',  ( -52.55046997570821787, -21.76995662024391365, -25.00977836231365004 ) ) ;
#48977 = DIRECTION ( 'NONE',  ( -1.000000000000000000, -1.224606353822377258E-16, -0.000000000000000000 ) ) ;
#48979 = PRODUCT_DEFINITION_FORMATION_WITH_SPECIFIED_SOURCE ( 'ANY', '', #27484, .NOT_KNOWN. ) ;
#48980 = ORIENTED_EDGE ( 'NONE', *, *, #9885, .F. ) ;
#48981 = AXIS2_PLACEMENT_3D ( 'NONE', #18888, #35596, #91682 ) ;
#48982 = EDGE_LOOP ( 'NONE', ( #16695, #18997, #89534, #4745, #64085, #77974 ) ) ;
#48983 = CARTESIAN_POINT ( 'NONE',  ( -25.99577189627797935, 34.94014516354030064, 9.388825123540007311 ) ) ;
#48984 = CARTESIAN_POINT ( 'NONE',  ( 11.49357173040307778, 43.46406798798316373, -13.79729247989035557 ) ) ;
#48985 = DIRECTION ( 'NONE',  ( -1.000000000000000000, -1.224606353822377258E-16, -0.000000000000000000 ) ) ;
#48986 = CARTESIAN_POINT ( 'NONE',  ( -87.06860877932031428, -60.00000000000000000, -22.64416279712467528 ) ) ;
#48987 = ORIENTED_EDGE ( 'NONE', *, *, #54026, .T. ) ;
#48988 = CARTESIAN_POINT ( 'NONE',  ( 0.01372220897661846455, -5.309964801958114933, 3.802871176606136050 ) ) ;
#48989 = CARTESIAN_POINT ( 'NONE',  ( -9.852235012526417535, 15.56087475005695353, 1.749814335632529749 ) ) ;
#48990 = CARTESIAN_POINT ( 'NONE',  ( 100.9499868790999813, -60.25997814283888943, 195.1806730477072165 ) ) ;
#48991 = EDGE_CURVE ( 'NONE', #40836, #96386, #38552, .T. ) ;
#48993 = CARTESIAN_POINT ( 'NONE',  ( -46.97259151695102730, 12.59255281441348728, 16.28847157548942448 ) ) ;
#48992 = CYLINDRICAL_SURFACE ( 'NONE', #19911, 5.000000000000002665 ) ;
#48994 = ORIENTED_EDGE ( 'NONE', *, *, #52769, .T. ) ;
#48995 = ORIENTED_EDGE ( 'NONE', *, *, #20223, .F. ) ;
#48996 = EDGE_LOOP ( 'NONE', ( #82470, #81802, #58316, #90857, #47074 ) ) ;
#48997 = CARTESIAN_POINT ( 'NONE',  ( 31.44885746337475751, 398.4224732248688383, 24.43061767113179883 ) ) ;
#48998 = CIRCLE ( 'NONE', #2519, 5.000000000000011546 ) ;
#48999 = CARTESIAN_POINT ( 'NONE',  ( -6.125000000000000000, -15.62228920881131700, 14.41094225130410855 ) ) ;
#49000 = SURFACE_STYLE_USAGE ( .BOTH. , #39877 ) ;
#49001 = VERTEX_POINT ( 'NONE', #58063 ) ;
#49002 = CONICAL_SURFACE ( 'NONE', #66266, 3.309500000000001663, 0.9599310885968770357 ) ;
#49003 = CARTESIAN_POINT ( 'NONE',  ( -42.36735105583831995, 487.4262793961416946, 8.281278960744069551 ) ) ;
#49004 = CARTESIAN_POINT ( 'NONE',  ( -122.4708123290697444, 1.499999999999992450, 61.23540616453485796 ) ) ;
#49005 = CARTESIAN_POINT ( 'NONE',  ( 0.06809871960542653035, -6.146186931204441706, -5.354491962338080668 ) ) ;
#49006 = CARTESIAN_POINT ( 'NONE',  ( -50.71028374685950268, -57.67771315371629726, 79.11066721451838646 ) ) ;
#49007 = CARTESIAN_POINT ( 'NONE',  ( 7.188101187500001821, -29.56250000204838813, -2.977408999572650483 ) ) ;
#49008 = CARTESIAN_POINT ( 'NONE',  ( 7.212994264445059756, -67.01711344340039034, 3.463766307298588920 ) ) ;
#49009 = DIRECTION ( 'NONE',  ( 0.000000000000000000, 0.2105263157894737835, -0.9775881905793005755 ) ) ;
#49010 = CARTESIAN_POINT ( 'NONE',  ( 2.563280883360062656, 15.30085158941011159, -9.673800154115147265 ) ) ;
#49011 = CARTESIAN_POINT ( 'NONE',  ( 47.46761990717632784, -14.21045842199427511, -33.06011575854734730 ) ) ;
#49012 = CARTESIAN_POINT ( 'NONE',  ( 0.000000000000000000, 0.000000000000000000, -13.00000000000000000 ) ) ;
#49013 = ADVANCED_FACE ( 'NONE', ( #90986 ), #61883, .F. ) ;
#49014 = CARTESIAN_POINT ( 'NONE',  ( -52.27550221499717509, -56.84507427995361439, 61.26800082247714130 ) ) ;
#49015 = CARTESIAN_POINT ( 'NONE',  ( -1.469576158976823947E-15, -27.87499999999999645, 8.000000000000000000 ) ) ;
#49016 = ORIENTED_EDGE ( 'NONE', *, *, #70293, .T. ) ;
#49017 = AXIS2_PLACEMENT_3D ( 'NONE', #26148, #52485, #42268 ) ;
#49018 = CARTESIAN_POINT ( 'NONE',  ( -99.74672076233166251, -45.25374114503119216, 192.8211023940378936 ) ) ;
#49019 = AXIS2_PLACEMENT_3D ( 'NONE', #19081, #84835, #83755 ) ;
#49020 = MECHANICAL_DESIGN_GEOMETRIC_PRESENTATION_REPRESENTATION (  '', ( #4247 ), #21521 ) ;
#49021 = CARTESIAN_POINT ( 'NONE',  ( -2.435618412542380096, 294.8338784867304412, -9.717600221842332076 ) ) ;
#49022 = CARTESIAN_POINT ( 'NONE',  ( 9.389245980427297411, -2.447416405268218131, 14.81682632889905626 ) ) ;
#49023 = EDGE_LOOP ( 'NONE', ( #45076, #22676, #23795, #79154, #37968, #65318, #104007 ) ) ;
#49024 = CARTESIAN_POINT ( 'NONE',  ( -17.97954184224904495, 34.27542366261327800, -23.34466436009411083 ) ) ;
#49025 = COLOUR_RGB ( '', 0.66274510, 0.83137255, 0.94901961) ;
#49026 = CARTESIAN_POINT ( 'NONE',  ( 110.6919933160486664, -38.35613597905214789, 162.9682471850780132 ) ) ;
#49027 = DIRECTION ( 'NONE',  ( 0.5735764363510557073, -0.8191520442889850262, 1.003171929053516612E-16 ) ) ;
#49028 = CARTESIAN_POINT ( 'NONE',  ( 0.000000000000000000, 4.898587196589413815E-16, -4.000000000000000888 ) ) ;
#49029 = CARTESIAN_POINT ( 'NONE',  ( -9.565054828409994769, 294.6554042961246864, 1.895259989615173168 ) ) ;
#49030 = AXIS2_PLACEMENT_3D ( 'NONE', #61866, #20911, #69417 ) ;
#49031 = CARTESIAN_POINT ( 'NONE',  ( 41.08349330513380693, -4.000000000000000000, 4.898587196589415787E-16 ) ) ;
#49032 = CARTESIAN_POINT ( 'NONE',  ( 83.98821470635078867, -29.99999999999999645, 160.9053504413435860 ) ) ;
#49033 = CARTESIAN_POINT ( 'NONE',  ( 36.65209206386361274, 491.4469928998128694, 12.33162904370259128 ) ) ;
#49034 = EDGE_CURVE ( 'NONE', #35387, #56862, #103363, .T. ) ;
#49035 = CARTESIAN_POINT ( 'NONE',  ( -32.03361802173512274, 464.8552804869456168, 13.91311180126945857 ) ) ;
#49036 = DIRECTION ( 'NONE',  ( 0.000000000000000000, -1.000000000000000000, 0.000000000000000000 ) ) ;
#49037 = VERTEX_POINT ( 'NONE', #53184 ) ;
#49038 = ORIENTED_EDGE ( 'NONE', *, *, #35850, .T. ) ;
#49039 = CARTESIAN_POINT ( 'NONE',  ( 49.90722959797657410, -53.36482695313026170, 55.25312740662995026 ) ) ;
#49040 = CARTESIAN_POINT ( 'NONE',  ( 6.839476587632750793, 41.56703181668088831, -58.82533975359289968 ) ) ;
#49041 = CARTESIAN_POINT ( 'NONE',  ( 8.881086064414537518, 51.45508042954168104, 3.999917844499591535 ) ) ;
#49042 = EDGE_LOOP ( 'NONE', ( #88749, #40985, #25620, #3668 ) ) ;
#49043 = CARTESIAN_POINT ( 'NONE',  ( -102.5472473342257587, -38.35641472935498086, 103.2659507031501960 ) ) ;
#49044 = ORIENTED_EDGE ( 'NONE', *, *, #74834, .T. ) ;
#49045 = DIRECTION ( 'NONE',  ( 0.000000000000000000, -1.000000000000000000, 0.000000000000000000 ) ) ;
#49046 = CARTESIAN_POINT ( 'NONE',  ( 98.48880034582394671, -38.35583643892559991, 79.54055716815213373 ) ) ;
#49047 = CARTESIAN_POINT ( 'NONE',  ( 10.12831231167428925, 12.29606514004753492, -10.56315130349414844 ) ) ;
#49048 = CARTESIAN_POINT ( 'NONE',  ( 5.656854249492378806, -15.68749999999999289, 5.656854249492381470 ) ) ;
#49049 = CARTESIAN_POINT ( 'NONE',  ( 102.4711514760015518, -45.28286875496431207, 149.2602369284549866 ) ) ;
#49050 = CARTESIAN_POINT ( 'NONE',  ( -10.00000000000000355, 105.0000000000000000, -4.000000000000001776 ) ) ;
#49051 = DIRECTION ( 'NONE',  ( -0.000000000000000000, -1.000000000000000000, -0.000000000000000000 ) ) ;
#49052 = CARTESIAN_POINT ( 'NONE',  ( -29.51136820535556282, 310.7658785638236623, -8.630889702403234054 ) ) ;
#49053 = CARTESIAN_POINT ( 'NONE',  ( 6.289812543865804351, 5.581224740283310837, -3.991031161979334385 ) ) ;
#49054 = CARTESIAN_POINT ( 'NONE',  ( 75.69597243072205117, -60.00000000000000000, 185.5364934770681486 ) ) ;
#49055 = EDGE_CURVE ( 'NONE', #31789, #67191, #94313, .T. ) ;
#49056 = AXIS2_PLACEMENT_3D ( 'NONE', #24067, #73628, #41275 ) ;
#49057 = DIRECTION ( 'NONE',  ( 0.000000000000000000, 0.000000000000000000, -1.000000000000000000 ) ) ;
#49058 = ORIENTED_EDGE ( 'NONE', *, *, #99417, .F. ) ;
#49059 = CARTESIAN_POINT ( 'NONE',  ( 58.04481121138562116, -56.85611253634766626, 75.20185096419942283 ) ) ;
#49060 = EDGE_CURVE ( 'NONE', #13955, #38472, #456, .T. ) ;
#49061 = CARTESIAN_POINT ( 'NONE',  ( -24.94621240166074472, 303.9363870782586332, -9.765254933829170980 ) ) ;
#49062 = CARTESIAN_POINT ( 'NONE',  ( 9.611186809632508599, -50.99327491418545577, 29.76794951015613933 ) ) ;
#49063 = CARTESIAN_POINT ( 'NONE',  ( -15.38845442529095209, 22.75486601555547495, 2.273822911181871298 ) ) ;
#49064 = CARTESIAN_POINT ( 'NONE',  ( -7.279541227045297269, -4.999999999999999112, -15.48747486643692106 ) ) ;
#49066 = CARTESIAN_POINT ( 'NONE',  ( 43.00000000000000000, 500.0000000000002274, 0.000000000000000000 ) ) ;
#49065 = CARTESIAN_POINT ( 'NONE',  ( -59.60688997945907630, -30.00000000000668976, 90.58845735111052022 ) ) ;
#49067 = CARTESIAN_POINT ( 'NONE',  ( -33.16823963622213967, 390.8948510558434464, 25.58094942542993877 ) ) ;
#49068 = CARTESIAN_POINT ( 'NONE',  ( -38.78856572157635441, 25.16510362771173703, -12.51935735473968592 ) ) ;
#49069 = CARTESIAN_POINT ( 'NONE',  ( 27.99999999999999645, 1.592040838891559095E-15, 13.00000000000000000 ) ) ;
#49070 = CARTESIAN_POINT ( 'NONE',  ( 5.656854249492378806, -32.18749999999999289, 5.656854249492381470 ) ) ;
#49071 = FACE_OUTER_BOUND ( 'NONE', #38344, .T. ) ;
#49072 = EDGE_CURVE ( 'NONE', #16452, #103302, #77455, .T. ) ;
#49073 = CARTESIAN_POINT ( 'NONE',  ( 32.84237740334622657, 485.2251842821286800, 5.746442123025142124 ) ) ;
#49074 = EDGE_LOOP ( 'NONE', ( #51413, #38724, #34385, #75733 ) ) ;
#49075 = CARTESIAN_POINT ( 'NONE',  ( 82.27827146869219632, -49.99153877646314470, 179.0196594568768091 ) ) ;
#49076 = CARTESIAN_POINT ( 'NONE',  ( 30.00000000000000000, 489.2891479521253473, 5.498062499254755764 ) ) ;
#49077 = CARTESIAN_POINT ( 'NONE',  ( -40.97825696304336418, 438.0977617246737168, 22.33876858701082213 ) ) ;
#49078 = ORIENTED_EDGE ( 'NONE', *, *, #23592, .T. ) ;
#49079 = CARTESIAN_POINT ( 'NONE',  ( 12.34835181856063002, -4.332967528434596538, -12.86601580078908214 ) ) ;
#49080 = ADVANCED_FACE ( 'NONE', ( #61277 ), #106713, .T. ) ;
#49081 =( NAMED_UNIT ( * ) SI_UNIT ( $, .STERADIAN. ) SOLID_ANGLE_UNIT ( ) );
#49082 = CARTESIAN_POINT ( 'NONE',  ( 25.89606338949664277, 35.00197463208161963, -9.163675292473188350 ) ) ;
#49083 = SURFACE_STYLE_FILL_AREA ( #98179 ) ;
#49084 = CARTESIAN_POINT ( 'NONE',  ( 11.36650669486618881, 1.474610560812782335E-15, 0.000000000000000000 ) ) ;
#49085 = VECTOR ( 'NONE', #42161, 1000.000000000000000 ) ;
#49086 = CARTESIAN_POINT ( 'NONE',  ( 37.72659966023548606, 25.70133307342159057, 10.95617127780997180 ) ) ;
#49087 = CARTESIAN_POINT ( 'NONE',  ( 1.126303995421776394, 25.38703625300498601, 40.13366474932937678 ) ) ;
#49089 = CARTESIAN_POINT ( 'NONE',  ( -11.51257484515206997, 12.49334646015600292, -10.00308483352378630 ) ) ;
#49088 = CARTESIAN_POINT ( 'NONE',  ( -9.802581847862906983, -20.13751096416813624, 35.36442285224644166 ) ) ;
#49090 = COLOUR_RGB ( '', 0.66274510, 0.83137255, 0.94901961) ;
#49091 = CARTESIAN_POINT ( 'NONE',  ( -2.977408999572654480, -13.62500000204838457, 7.188101187499999156 ) ) ;
#49092 = CARTESIAN_POINT ( 'NONE',  ( -28.54518584606556431, 18.48129625438333790, -40.33591358207613098 ) ) ;
#49093 = AXIS2_PLACEMENT_3D ( 'NONE', #62871, #69368, #4096 ) ;
#49094 = SURFACE_SIDE_STYLE ('',( #42611 ) ) ;
#49095 = CIRCLE ( 'NONE', #90472, 4.000000000000007105 ) ;
#49096 = AXIS2_PLACEMENT_3D ( 'NONE', #80334, #40420, #6447 ) ;
#49097 = ORIENTED_EDGE ( 'NONE', *, *, #73346, .T. ) ;
#49098 = CARTESIAN_POINT ( 'NONE',  ( -17.49999999999490896, 48.96861188085171079, 62.56461476143485356 ) ) ;
#49099 = CARTESIAN_POINT ( 'NONE',  ( 23.54214819851715390, 25.90553154796090141, 30.74632383150428083 ) ) ;
#49100 = AXIS2_PLACEMENT_3D ( 'NONE', #62137, #87985, #104147 ) ;
#49101 = CARTESIAN_POINT ( 'NONE',  ( -3.422808420448540279, 123.4701245564265122, -4.999999999999999112 ) ) ;
#49102 = CARTESIAN_POINT ( 'NONE',  ( -6.827804075699749120, -4.999999999995546673, -71.19745154229521233 ) ) ;
#49103 = EDGE_CURVE ( 'NONE', #90027, #32720, #91281, .T. ) ;
#49104 = CARTESIAN_POINT ( 'NONE',  ( 0.000000000000000000, 0.000000000000000000, 4.000000000000000000 ) ) ;
#49105 = ORIENTED_EDGE ( 'NONE', *, *, #73497, .T. ) ;
#49106 = CARTESIAN_POINT ( 'NONE',  ( -4.478476647430158941, -85.27352079182048783, 3.992942460563208229 ) ) ;
#49107 = DIRECTION ( 'NONE',  ( 0.000000000000000000, 0.000000000000000000, -1.000000000000000000 ) ) ;
#49108 = ORIENTED_EDGE ( 'NONE', *, *, #9403, .T. ) ;
#49109 = EDGE_CURVE ( 'NONE', #63343, #100372, #27488, .T. ) ;
#49110 = DIRECTION ( 'NONE',  ( 1.000000000000000000, 0.000000000000000000, 0.000000000000000000 ) ) ;
#49111 = CARTESIAN_POINT ( 'NONE',  ( 37.96538461538461462, -4.171999999999999709, 5.616230220889763424E-16 ) ) ;
#49112 = CARTESIAN_POINT ( 'NONE',  ( -98.17166580661555031, -59.99999999999999289, 69.98620740965910159 ) ) ;
#49113 = CARTESIAN_POINT ( 'NONE',  ( 29.09597697838555064, 14.54318144277619496, -41.96748357178393007 ) ) ;
#49114 = CARTESIAN_POINT ( 'NONE',  ( 0.000000000000000000, -1.500000000000000000, 0.000000000000000000 ) ) ;
#49115 = CARTESIAN_POINT ( 'NONE',  ( 24.93816302196866275, 307.4233949143036284, 10.52291764336465008 ) ) ;
#49116 = CARTESIAN_POINT ( 'NONE',  ( -32.14399312865362646, 464.7181097252859558, 11.03234060977934483 ) ) ;
#49118 = CARTESIAN_POINT ( 'NONE',  ( 30.00000000001042721, 488.0736639502548542, 7.689181908884415328 ) ) ;
#49117 = CARTESIAN_POINT ( 'NONE',  ( 0.000000000000000000, -5.000000000000002665, -73.00000000000001421 ) ) ;
#49119 = CARTESIAN_POINT ( 'NONE',  ( -85.29290479114395396, -25.40355077146805129, 170.0323860005369454 ) ) ;
#49120 = VERTEX_POINT ( 'NONE', #47190 ) ;
#49121 = CARTESIAN_POINT ( 'NONE',  ( 4.852941176470593199, 9.833333333333344584, -70.80672828634229177 ) ) ;
#49122 = VERTEX_POINT ( 'NONE', #46669 ) ;
#49123 = AXIS2_PLACEMENT_3D ( 'NONE', #17955, #92886, #68642 ) ;
#49124 = ORIENTED_EDGE ( 'NONE', *, *, #98646, .T. ) ;
#49125 = DIRECTION ( 'NONE',  ( -0.000000000000000000, -1.000000000000000000, -0.000000000000000000 ) ) ;
#49126 = EDGE_CURVE ( 'NONE', #91320, #58206, #13711, .T. ) ;
#49127 = DIRECTION ( 'NONE',  ( -0.000000000000000000, 1.000000000000000000, 0.000000000000000000 ) ) ;
#49128 = ORIENTED_EDGE ( 'NONE', *, *, #86312, .F. ) ;
#49129 = B_SPLINE_CURVE_WITH_KNOTS ( 'NONE', 3,
 ( #66269, #9611, #99156, #58173 ),
 .UNSPECIFIED., .F., .F.,
 ( 4, 4 ),
 ( 0.000000000000000000, 1.000000000000000000 ),
 .UNSPECIFIED. ) ;
#49130 = B_SPLINE_CURVE_WITH_KNOTS ( 'NONE', 3,
 ( #59021, #76780, #90854, #49846 ),
 .UNSPECIFIED., .F., .F.,
 ( 4, 4 ),
 ( 0.0009723127763595034020, 0.02104041089405187664 ),
 .UNSPECIFIED. ) ;
#49131 = DIRECTION ( 'NONE',  ( 0.000000000000000000, -1.000000000000000000, 0.000000000000000000 ) ) ;
#49132 = DIRECTION ( 'NONE',  ( 0.000000000000000000, 0.000000000000000000, -1.000000000000000000 ) ) ;
#49133 = CARTESIAN_POINT ( 'NONE',  ( 30.00000000000000000, 461.8802764867031669, 14.89328939272360053 ) ) ;
#49134 = CARTESIAN_POINT ( 'NONE',  ( 8.732981572811874926, -5.000000000000000000, -94.70094745737053188 ) ) ;
#49135 = CARTESIAN_POINT ( 'NONE',  ( -43.32251133971205093, 485.6545735287840557, 4.688172406475217713 ) ) ;
#49136 = CARTESIAN_POINT ( 'NONE',  ( 103.2975989548790494, -14.21045842199431064, 133.3107955441116985 ) ) ;
#49137 = CARTESIAN_POINT ( 'NONE',  ( -104.9451182028910239, -14.21045842199441367, 145.4712626202903323 ) ) ;
#49138 = ADVANCED_FACE ( 'NONE', ( #70430 ), #72318, .F. ) ;
#49139 = CARTESIAN_POINT ( 'NONE',  ( -62.36043780488878241, -49.91630522361305111, 83.85778711176541833 ) ) ;
#49140 = VERTEX_POINT ( 'NONE', #13759 ) ;
#49141 = CARTESIAN_POINT ( 'NONE',  ( -43.32509445547438531, 484.2781405677309863, -0.02261530909676546380 ) ) ;
#49142 = CARTESIAN_POINT ( 'NONE',  ( 101.2350610320152526, -59.99999999996104094, 74.14752333521899175 ) ) ;
#49143 = ORIENTED_EDGE ( 'NONE', *, *, #38488, .T. ) ;
#49144 = CARTESIAN_POINT ( 'NONE',  ( 0.9975031403653140671, -32.51050350380973697, 29.30806721023733630 ) ) ;
#49145 = CARTESIAN_POINT ( 'NONE',  ( 5.082755093536324154, -12.21875000204838635, 5.082755093536326818 ) ) ;
#49146 = CARTESIAN_POINT ( 'NONE',  ( -13.49999999999999822, -6.526560492696116711, -0.8398270946102923684 ) ) ;
#49147 = VERTEX_POINT ( 'NONE', #5680 ) ;
#49148 = CARTESIAN_POINT ( 'NONE',  ( 7.186686048019178763, -30.00000000000000355, -0.4953821823922022194 ) ) ;
#49149 = ORIENTED_EDGE ( 'NONE', *, *, #13613, .F. ) ;
#49150 = SURFACE_SIDE_STYLE ('',( #16265 ) ) ;
#49151 = AXIS2_PLACEMENT_3D ( 'NONE', #62797, #54668, #30444 ) ;
#49152 = CARTESIAN_POINT ( 'NONE',  ( -106.4349217454702341, -60.00000000000002132, 197.8028031639909159 ) ) ;
#49153 = FACE_OUTER_BOUND ( 'NONE', #18841, .T. ) ;
#49154 = CARTESIAN_POINT ( 'NONE',  ( -5.082755093536325042, -26.46875000204838813, -5.082755093536325930 ) ) ;
#49155 = CARTESIAN_POINT ( 'NONE',  ( -4.000000000000001776, 4.898587196589415787E-16, -8.000000000000000000 ) ) ;
#49156 = PLANE ( 'NONE',  #104669 ) ;
#49157 = CARTESIAN_POINT ( 'NONE',  ( -3.586716539735087750, 19.64243682284886461, -6.012447941353936898 ) ) ;
#49158 = LINE ( 'NONE', #8184, #63302 ) ;
#49159 = CARTESIAN_POINT ( 'NONE',  ( 32.89862776688912049, 464.9311084009901833, 10.99515925127326810 ) ) ;
#49160 = EDGE_CURVE ( 'NONE', #43590, #12840, #72520, .T. ) ;
#49161 = CARTESIAN_POINT ( 'NONE',  ( -23.38277283915476445, 28.07830159701456907, 30.71447743823551235 ) ) ;
#49162 = AXIS2_PLACEMENT_3D ( 'NONE', #57550, #90477, #16584 ) ;
#49163 = LINE ( 'NONE', #25480, #77615 ) ;
#49164 = CARTESIAN_POINT ( 'NONE',  ( -32.20452792638825912, -22.14816194189014453, 30.75548861735132178 ) ) ;
#49165 = CARTESIAN_POINT ( 'NONE',  ( 38.83382506401130030, -32.59866074387370816, 36.29133770639072765 ) ) ;
#49166 = COLOUR_RGB ( '', 0.66274510, 0.83137255, 0.94901961) ;
#49167 = AXIS2_PLACEMENT_3D ( 'NONE', #20194, #21246, #28817 ) ;
#49168 = DIRECTION ( 'NONE',  ( -1.000000000000000000, 0.000000000000000000, 0.000000000000000000 ) ) ;
#49169 = EDGE_LOOP ( 'NONE', ( #31277, #60723, #11339, #14834 ) ) ;
#49170 = CARTESIAN_POINT ( 'NONE',  ( -8.000086790516061086, 89.00017358106009624, 0.2639471549312795151 ) ) ;
#49171 = CARTESIAN_POINT ( 'NONE',  ( -77.48386536772069633, -38.51251665548984704, 186.4267636295656700 ) ) ;
#49172 = ORIENTED_EDGE ( 'NONE', *, *, #13306, .T. ) ;
#49174 = CARTESIAN_POINT ( 'NONE',  ( 25.93947128054312756, 296.0094280503604978, 10.18659011856751384 ) ) ;
#49173 = DIRECTION ( 'NONE',  ( 0.000000000000000000, 0.000000000000000000, 1.000000000000000000 ) ) ;
#49175 = CARTESIAN_POINT ( 'NONE',  ( -11.10298186479972316, 8.427547193095088929, 9.820813330727961699 ) ) ;
#49176 = CARTESIAN_POINT ( 'NONE',  ( -13.00000000000003730, 249.9999999999999432, 0.000000000000000000 ) ) ;
#49177 = CARTESIAN_POINT ( 'NONE',  ( -7.043655074372488833, 41.66078712639146175, -59.26733995391339249 ) ) ;
#49178 = AXIS2_PLACEMENT_3D ( 'NONE', #75172, #42284, #50368 ) ;
#49179 = CIRCLE ( 'NONE', #18201, 4.000000000000007105 ) ;
#49180 = DIRECTION ( 'NONE',  ( 0.000000000000000000, 0.000000000000000000, -1.000000000000000000 ) ) ;
#49181 = CARTESIAN_POINT ( 'NONE',  ( -38.66164730681681050, 25.17357370736559474, 12.83228708202576307 ) ) ;
#49182 = PRESENTATION_LAYER_ASSIGNMENT (  '', '', ( #90537 ) ) ;
#49183 = CARTESIAN_POINT ( 'NONE',  ( -31.35596682365705945, 438.0939828603719093, 22.55458131664414267 ) ) ;
#49184 = CARTESIAN_POINT ( 'NONE',  ( -5.656854249492379694, -25.62500000409677270, -5.656854249492380582 ) ) ;
#49185 = CARTESIAN_POINT ( 'NONE',  ( 103.6214353051173021, -60.00000000000001421, 102.2210354960218126 ) ) ;
#49186 = AXIS2_PLACEMENT_3D ( 'NONE', #91524, #58069, #82353 ) ;
#49187 = B_SPLINE_CURVE_WITH_KNOTS ( 'NONE', 3,
 ( #83938, #12168, #87147, #54208, #93641, #20866, #45100, #70948, #44564, #101719 ),
 .UNSPECIFIED., .F., .F.,
 ( 4, 2, 2, 2, 4 ),
 ( 0.000000000000000000, 0.0008124082233779007355, 0.001624816446755801471, 0.002437224670133701990, 0.003249632893511602942 ),
 .UNSPECIFIED. ) ;
#49188 = CARTESIAN_POINT ( 'NONE',  ( -6.018823944621538580, -50.31891336156137839, 39.64063426992244388 ) ) ;
#49189 = AXIS2_PLACEMENT_3D ( 'NONE', #71379, #37476, #44472 ) ;
#49190 = DIRECTION ( 'NONE',  ( 0.000000000000000000, 0.000000000000000000, 1.000000000000000000 ) ) ;
#49191 = EDGE_LOOP ( 'NONE', ( #2369, #11854, #68358, #42421 ) ) ;
#49192 = EDGE_CURVE ( 'NONE', #1352, #33529, #27555, .T. ) ;
#49193 = CARTESIAN_POINT ( 'NONE',  ( -98.46708292002269047, -30.00000000000004619, 189.8972334866360541 ) ) ;
#49194 = ORIENTED_EDGE ( 'NONE', *, *, #62511, .T. ) ;
#49195 = CARTESIAN_POINT ( 'NONE',  ( 46.00000000000000000, 500.0000000000002274, 0.000000000000000000 ) ) ;
#49196 = CARTESIAN_POINT ( 'NONE',  ( -15.92744018389476857, 3.245174460798382121, 1.809927857081228497 ) ) ;
#49197 = CARTESIAN_POINT ( 'NONE',  ( 8.763463954820251089, 132.4016268868482200, 6.150641887046839534E-13 ) ) ;
#49198 = LINE ( 'NONE', #82098, #8783 ) ;
#49199 = CARTESIAN_POINT ( 'NONE',  ( 9.483056940782024213, 27.55612209893422815, -3.177305548492607379 ) ) ;
#49200 = CARTESIAN_POINT ( 'NONE',  ( -7.188101187500000044, -27.78125000204838813, -8.802885111219163269E-16 ) ) ;
#49201 = FACE_OUTER_BOUND ( 'NONE', #38769, .T. ) ;
#49203 = EDGE_CURVE ( 'NONE', #42513, #8439, #31580, .T. ) ;
#49202 = FACE_OUTER_BOUND ( 'NONE', #33016, .T. ) ;
#49204 = ORIENTED_EDGE ( 'NONE', *, *, #57974, .T. ) ;
#49205 = B_SPLINE_CURVE_WITH_KNOTS ( 'NONE', 3,
 ( #75527, #18384, #60964, #1071, #10776, #101413, #10259, #34046, #43695, #27025 ),
 .UNSPECIFIED., .F., .F.,
 ( 4, 2, 2, 2, 4 ),
 ( 0.000000000000000000, 0.5000000000000000000, 0.7500000000000000000, 0.8750000000000000000, 1.000000000000000000 ),
 .UNSPECIFIED. ) ;
#49207 = VERTEX_POINT ( 'NONE', #104922 ) ;
#49206 = CARTESIAN_POINT ( 'NONE',  ( 0.000000000000000000, -30.00000000000000000, 0.000000000000000000 ) ) ;
#49208 = CARTESIAN_POINT ( 'NONE',  ( 78.98612558784607529, -60.31715732648605410, 164.7471663665724861 ) ) ;
#49209 = DIRECTION ( 'NONE',  ( -1.000000000000000000, 0.000000000000000000, 0.000000000000000000 ) ) ;
#49210 =( NAMED_UNIT ( * ) SI_UNIT ( $, .STERADIAN. ) SOLID_ANGLE_UNIT ( ) );
#49211 = EDGE_LOOP ( 'NONE', ( #106125, #76447, #50427, #14593, #4768, #38401 ) ) ;
#49212 = EDGE_CURVE ( 'NONE', #102768, #30747, #31063, .T. ) ;
#49213 = CARTESIAN_POINT ( 'NONE',  ( -62.81518964951828110, 49.99999999999998579, -4.977225890182330303 ) ) ;
#49214 = CARTESIAN_POINT ( 'NONE',  ( 6.928203230275507885, -85.00000000000000000, -4.000000000000001776 ) ) ;
#49215 = CARTESIAN_POINT ( 'NONE',  ( 7.188101187500000044, -13.15625000204838280, 0.000000000000000000 ) ) ;
#49216 = CARTESIAN_POINT ( 'NONE',  ( 2.845670519300376476E-15, 38.67090180175566871, 23.23666318551310539 ) ) ;
#49217 = PRESENTATION_LAYER_ASSIGNMENT (  '', '', ( #44085 ) ) ;
#49218 = CARTESIAN_POINT ( 'NONE',  ( 58.62000344007604014, -60.00000000000000000, -30.08217214727655886 ) ) ;
#49219 = DIRECTION ( 'NONE',  ( -0.7071067811865314745, 8.659560562355128841E-17, -0.7071067811865635599 ) ) ;
#49220 = SURFACE_SIDE_STYLE ('',( #90224 ) ) ;
#49221 = ORIENTED_EDGE ( 'NONE', *, *, #55180, .T. ) ;
#49222 = CARTESIAN_POINT ( 'NONE',  ( 0.000000000000000000, 45.50000000000000711, 0.000000000000000000 ) ) ;
#49223 = CARTESIAN_POINT ( 'NONE',  ( -3.313708498984798467, -19.53124999999999289, -7.999999999999961808 ) ) ;
#49224 = DIRECTION ( 'NONE',  ( -1.000000000000000000, 0.000000000000000000, 0.000000000000000000 ) ) ;
#49225 = CARTESIAN_POINT ( 'NONE',  ( -1.320432766682874540E-15, -30.03125000204838813, 7.188101187500000044 ) ) ;
#49226 = CARTESIAN_POINT ( 'NONE',  ( 23.51672044067690948, -28.03177904939224518, 37.77843793023890839 ) ) ;
#49227 = CARTESIAN_POINT ( 'NONE',  ( -6.701893397842001221, 41.44328394191487774, -70.59544911652842814 ) ) ;
#49228 = CARTESIAN_POINT ( 'NONE',  ( 35.58576704944795210, 439.9331698772741106, 24.32295159899808468 ) ) ;
#49229 = CONICAL_SURFACE ( 'NONE', #9578, 3.309500000000007880, 0.9599310885968770357 ) ;
#49230 = PRODUCT_CONTEXT ( 'NONE', #54819, 'mechanical' ) ;
#49231 = CARTESIAN_POINT ( 'NONE',  ( 49.22360526642682998, 7.740778690624840586, 15.97911514197205030 ) ) ;
#49232 = ORIENTED_EDGE ( 'NONE', *, *, #50933, .T. ) ;
#49233 = CARTESIAN_POINT ( 'NONE',  ( -34.53191791165069446, 437.2926915873502480, 5.227229271294363322 ) ) ;
#49234 = DIRECTION ( 'NONE',  ( 0.000000000000000000, -1.000000000000000000, 0.000000000000000000 ) ) ;
#49235 = DIRECTION ( 'NONE',  ( -1.000000000000000000, -1.224606353822377258E-16, -0.000000000000000000 ) ) ;
#49236 =( BOUNDED_CURVE ( )  B_SPLINE_CURVE ( 1, ( #66991, #58903 ),
 .UNSPECIFIED., .F., .F. ) 
 B_SPLINE_CURVE_WITH_KNOTS ( ( 2, 2 ),
 ( 0.000000000000000000, 1.000000000000000000 ),
 .UNSPECIFIED. ) 
 CURVE ( )  GEOMETRIC_REPRESENTATION_ITEM ( )  RATIONAL_B_SPLINE_CURVE ( ( 0.9660719911213342392, 0.9660719911213342392 ) ) 
 REPRESENTATION_ITEM ( '' )  );
#49237 = LINE ( 'NONE', #40627, #84199 ) ;
#49238 = EDGE_CURVE ( 'NONE', #103023, #2439, #29397, .T. ) ;
#49239 = ORIENTED_EDGE ( 'NONE', *, *, #105370, .F. ) ;
#49240 = CARTESIAN_POINT ( 'NONE',  ( -4.852941176470593199, -5.250000000000004441, -70.80672828634229177 ) ) ;
#49241 = CARTESIAN_POINT ( 'NONE',  ( 107.5440841644286536, -57.67122823495125061, 113.6602115610031944 ) ) ;
#49242 = EDGE_CURVE ( 'NONE', #84586, #72526, #67255, .T. ) ;
#49243 = CARTESIAN_POINT ( 'NONE',  ( 14.91270732344407257, 41.98564553269472555, -86.62216337287246404 ) ) ;
#49244 = DIRECTION ( 'NONE',  ( 0.5735764363510490460, 0.8191520442889896891, 0.000000000000000000 ) ) ;
#49245 = DIRECTION ( 'NONE',  ( -0.000000000000000000, -0.000000000000000000, 1.000000000000000000 ) ) ;
#49246 = MECHANICAL_DESIGN_GEOMETRIC_PRESENTATION_REPRESENTATION (  '', ( #64749 ), #16467 ) ;
#49247 = CARTESIAN_POINT ( 'NONE',  ( 37.24678017888829373, 25.86898843256250302, 10.95617127780997535 ) ) ;
#49248 = CARTESIAN_POINT ( 'NONE',  ( -77.64205621890488374, -60.00000000000002132, 192.0628139380899881 ) ) ;
#49249 = AXIS2_PLACEMENT_3D ( 'NONE', #79308, #62612, #8998 ) ;
#49250 = AXIS2_PLACEMENT_3D ( 'NONE', #45997, #78346, #71841 ) ;
#49251 = AXIS2_PLACEMENT_3D ( 'NONE', #33649, #74076, #15851 ) ;
#49252 =( LENGTH_UNIT ( ) NAMED_UNIT ( * ) SI_UNIT ( .MILLI., .METRE. ) );
#49253 = FACE_OUTER_BOUND ( 'NONE', #34545, .T. ) ;
#49254 = CARTESIAN_POINT ( 'NONE',  ( -62.34828826644581312, 50.00000000000000000, -10.72527895994686986 ) ) ;
#49255 = CARTESIAN_POINT ( 'NONE',  ( -84.96146178370577218, -46.57119306001131775, 187.4521374934294329 ) ) ;
#49256 = ORIENTED_EDGE ( 'NONE', *, *, #60293, .T. ) ;
#49257 = CARTESIAN_POINT ( 'NONE',  ( 29.49339759867818600, 311.0110510053014536, -7.568740214377905673 ) ) ;
#49258 = AXIS2_PLACEMENT_3D ( 'NONE', #68510, #51225, #92765 ) ;
#49259 = ORIENTED_EDGE ( 'NONE', *, *, #6030, .T. ) ;
#49260 = CARTESIAN_POINT ( 'NONE',  ( -7.896571385775229324, -13.78997999345754444, 1.305932416347439284 ) ) ;
#49261 = SURFACE_SIDE_STYLE ('',( #7216 ) ) ;
#49262 = CARTESIAN_POINT ( 'NONE',  ( -84.46166934361085055, -45.26796119114888484, -8.211886439601322252 ) ) ;
#49263 =( NAMED_UNIT ( * ) PLANE_ANGLE_UNIT ( ) SI_UNIT ( $, .RADIAN. ) );
#49264 = CARTESIAN_POINT ( 'NONE',  ( 6.463647488011505793, 2.646730816809989673, -6.840026438643558748 ) ) ;
#49265 = ORIENTED_EDGE ( 'NONE', *, *, #7820, .F. ) ;
#49266 = CARTESIAN_POINT ( 'NONE',  ( -3.352941176470600304, -1.200583151104954283, 104.5794940929807524 ) ) ;
#49267 = CARTESIAN_POINT ( 'NONE',  ( 10.88267043231995501, 9.048817955964610249, -10.02405438266481497 ) ) ;
#49268 = CARTESIAN_POINT ( 'NONE',  ( 2.227375807149031495, -1.734723475976807094E-15, 17.01589776168603407 ) ) ;
#49269 = CARTESIAN_POINT ( 'NONE',  ( -36.87655955837859523, 438.2068510013161813, 3.933030107424713595 ) ) ;
#49270 = CARTESIAN_POINT ( 'NONE',  ( -16.60966916665065085, -29.99999999999998934, -39.45625820571179787 ) ) ;
#49271 = CARTESIAN_POINT ( 'NONE',  ( -78.21160035621433337, -25.61278769304882985, 123.8358509973067498 ) ) ;
#49272 = ORIENTED_EDGE ( 'NONE', *, *, #38768, .T. ) ;
#49273 = CARTESIAN_POINT ( 'NONE',  ( 73.77841798646971938, -29.99999999999998934, 147.9493570314868123 ) ) ;
#49274 = CARTESIAN_POINT ( 'NONE',  ( 41.82792046605465686, -5.000000000000009770, 0.000000000000000000 ) ) ;
#49275 = CARTESIAN_POINT ( 'NONE',  ( 109.9110342544350516, -57.66832763311409593, 196.2850603310193094 ) ) ;
#49276 = ORIENTED_EDGE ( 'NONE', *, *, #40089, .F. ) ;
#49277 = CARTESIAN_POINT ( 'NONE',  ( 28.04511907431318818, 34.20682782302920799, 9.635168561359211736 ) ) ;
#49278 = DIRECTION ( 'NONE',  ( 0.000000000000000000, -1.000000000000000000, -0.000000000000000000 ) ) ;
#49279 = ORIENTED_EDGE ( 'NONE', *, *, #78838, .F. ) ;
#49280 = PRESENTATION_LAYER_ASSIGNMENT (  '', '', ( #1058 ) ) ;
#49281 = DIRECTION ( 'NONE',  ( -0.5735764363510494901, -0.8191520442889894671, 0.000000000000000000 ) ) ;
#49282 = DIRECTION ( 'NONE',  ( -1.000000000000000000, -0.000000000000000000, -0.000000000000000000 ) ) ;
#49283 = CARTESIAN_POINT ( 'NONE',  ( 0.000000000000000000, 50.50000000000000000, 65.00000000000000000 ) ) ;
#49284 = CARTESIAN_POINT ( 'NONE',  ( 2.977408999572650927, -21.87500000204838813, -7.188101187500001821 ) ) ;
#49285 = CARTESIAN_POINT ( 'NONE',  ( 7.298354728638322797, -4.926141412640330230, -7.913704048099935662 ) ) ;
#49286 = CIRCLE ( 'NONE', #82000, 5.000000000000004441 ) ;
#49287 = FACE_OUTER_BOUND ( 'NONE', #17728, .T. ) ;
#49288 = CARTESIAN_POINT ( 'NONE',  ( -7.499999999999999112, 1.613867362011851325, -7.450195926347907616 ) ) ;
#49289 = ORIENTED_EDGE ( 'NONE', *, *, #106551, .T. ) ;
#49290 = CARTESIAN_POINT ( 'NONE',  ( -7.286132170098562177, 40.29425722237677832, -70.75304762475369103 ) ) ;
#49292 = CARTESIAN_POINT ( 'NONE',  ( 30.44468774519250331, -53.37907340497660869, 35.76283041829702114 ) ) ;
#49291 = CARTESIAN_POINT ( 'NONE',  ( 19.00000000000000711, 5.000000000000000888, -1.500000000000001332 ) ) ;
#49293 = CARTESIAN_POINT ( 'NONE',  ( -4.044731509663068714, 51.90665404057882881, -7.475086770086759813 ) ) ;
#49294 = ORIENTED_EDGE ( 'NONE', *, *, #5978, .F. ) ;
#49295 =( NAMED_UNIT ( * ) SI_UNIT ( $, .STERADIAN. ) SOLID_ANGLE_UNIT ( ) );
#49296 = ORIENTED_EDGE ( 'NONE', *, *, #39084, .T. ) ;
#49298 = CARTESIAN_POINT ( 'NONE',  ( 0.6455896130745356620, 52.10958058375629776, 7.916501336716939896 ) ) ;
#49297 = SURFACE_SIDE_STYLE ('',( #16417 ) ) ;
#49299 = CARTESIAN_POINT ( 'NONE',  ( 64.29999999999999716, 6.915964383211875250E-15, 0.000000000000000000 ) ) ;
#49300 = DIRECTION ( 'NONE',  ( 1.000000000000000000, 1.224606353822377258E-16, 0.000000000000000000 ) ) ;
#49301 = APPLICATION_CONTEXT ( 'automotive_design' ) ;
#49302 = DIRECTION ( 'NONE',  ( 1.224646799147352468E-16, 0.000000000000000000, -1.000000000000000000 ) ) ;
#49303 = CARTESIAN_POINT ( 'NONE',  ( 68.45015997180047407, 4.000000000000013323, 0.000000000000000000 ) ) ;
#49304 = CARTESIAN_POINT ( 'NONE',  ( 0.8352780885855292103, 18.10189008090095797, -49.56687221457461590 ) ) ;
#49305 = ORIENTED_EDGE ( 'NONE', *, *, #95223, .T. ) ;
#49306 = CARTESIAN_POINT ( 'NONE',  ( 89.96949554733780019, -59.99999999999997868, -18.88444619536232594 ) ) ;
#49307 = AXIS2_PLACEMENT_3D ( 'NONE', #92593, #101231, #75881 ) ;
#49308 = CARTESIAN_POINT ( 'NONE',  ( 22.65138445058343208, 26.07323991223989168, -30.83851241702902612 ) ) ;
#49309 = CARTESIAN_POINT ( 'NONE',  ( -14.91858118607497019, 1.255821567010171884E-17, 15.00000000000000000 ) ) ;
#49310 = CARTESIAN_POINT ( 'NONE',  ( -10.47772246152234565, -5.000000000000000000, -91.06170733474810675 ) ) ;
#49311 = LINE ( 'NONE', #72020, #8840 ) ;
#49312 = ORIENTED_EDGE ( 'NONE', *, *, #84019, .T. ) ;
#49313 = EDGE_CURVE ( 'NONE', #29960, #9249, #58394, .T. ) ;
#49314 = CIRCLE ( 'NONE', #2819, 12.00000000000000000 ) ;
#49315 = B_SPLINE_CURVE_WITH_KNOTS ( 'NONE', 3,
 ( #106255, #65816, #64243, #23257, #105734, #22737, #6503, #46969, #5974, #39440, #22203, #14589, #41012, #55576, #57178, #38906, #71768, #90092 ),
 .UNSPECIFIED., .F., .F.,
 ( 4, 2, 2, 2, 2, 2, 2, 2, 4 ),
 ( 0.000000000000000000, 0.06250000000000000000, 0.1250000000000000000, 0.1875000000000000000, 0.2500000000000000000, 0.3125000000000000000, 0.3750000000000000000, 0.4375000000000000000, 0.5000000000000000000 ),
 .UNSPECIFIED. ) ;
#49316 = ADVANCED_FACE ( 'NONE', ( #98401 ), #79318, .T. ) ;
#49317 = LINE ( 'NONE', #90325, #91827 ) ;
#49318 = ORIENTED_EDGE ( 'NONE', *, *, #50786, .F. ) ;
#49319 = ORIENTED_EDGE ( 'NONE', *, *, #90395, .T. ) ;
#49320 = CARTESIAN_POINT ( 'NONE',  ( 0.9512138561578256102, 54.12926960197279413, 8.184984789997367116 ) ) ;
#49321 = CARTESIAN_POINT ( 'NONE',  ( 34.10284876471455817, 1.482358050883964840E-15, 0.000000000000000000 ) ) ;
#49322 = AXIS2_PLACEMENT_3D ( 'NONE', #99382, #57868, #74056 ) ;
#49323 = CARTESIAN_POINT ( 'NONE',  ( -40.74567133769577509, 318.5959897825344456, 3.761255434899160033 ) ) ;
#49324 = CARTESIAN_POINT ( 'NONE',  ( -4.755599198601705879, -66.38001295931699985, 13.81229897532385564 ) ) ;
#49325 = CARTESIAN_POINT ( 'NONE',  ( 1.238781280703658005, -50.00000000000000000, 101.3451024322821894 ) ) ;
#49326 = CARTESIAN_POINT ( 'NONE',  ( 12.50000000000000355, 34.83311936966315869, -54.12527282038643506 ) ) ;
#49327 = ORIENTED_EDGE ( 'NONE', *, *, #43257, .F. ) ;
#49329 = ADVANCED_FACE ( 'NONE', ( #1275 ), #50370, .T. ) ;
#49328 = CARTESIAN_POINT ( 'NONE',  ( -10.28624191511820207, 43.99263840937192782, 12.90779740156163768 ) ) ;
#49330 = VERTEX_POINT ( 'NONE', #49303 ) ;
#49331 = DIRECTION ( 'NONE',  ( -1.000000000000000000, 0.000000000000000000, 0.000000000000000000 ) ) ;
#49332 = CARTESIAN_POINT ( 'NONE',  ( 4.551587301587296075, -48.79941684889506348, 104.4018401814738155 ) ) ;
#49333 = PRESENTATION_LAYER_ASSIGNMENT (  '', '', ( #51021 ) ) ;
#49334 = AXIS2_PLACEMENT_3D ( 'NONE', #42980, #85578, #76388 ) ;
#49335 = VECTOR ( 'NONE', #71657, 999.9999999999998863 ) ;
#49337 = ORIENTED_EDGE ( 'NONE', *, *, #59356, .F. ) ;
#49336 = CARTESIAN_POINT ( 'NONE',  ( -75.38507137031108130, -60.00000000000003553, 138.7214457628266473 ) ) ;
#49338 = CARTESIAN_POINT ( 'NONE',  ( 67.30723638396268882, -39.48332017755057421, 93.17411211822772543 ) ) ;
#49339 = VECTOR ( 'NONE', #87466, 1000.000000000000114 ) ;
#49340 = VERTEX_POINT ( 'NONE', #83281 ) ;
#49341 = EDGE_CURVE ( 'NONE', #8913, #57315, #41229, .T. ) ;
#49342 = CARTESIAN_POINT ( 'NONE',  ( 4.999999999999996447, -45.99999999999997868, 40.27905619136139137 ) ) ;
#49343 = CIRCLE ( 'NONE', #97607, 8.000000000000000000 ) ;
#49344 = DIRECTION ( 'NONE',  ( 0.5735764363510470476, -0.8191520442889911324, 1.003171929053524007E-16 ) ) ;
#49345 = CARTESIAN_POINT ( 'NONE',  ( 6.394337469123806628, -3.776351736504768741, -6.540833074877208553 ) ) ;
#49346 = ORIENTED_EDGE ( 'NONE', *, *, #14637, .T. ) ;
#49347 = SURFACE_SIDE_STYLE ('',( #65016 ) ) ;
#49348 = LINE ( 'NONE', #42326, #64410 ) ;
#49349 = CARTESIAN_POINT ( 'NONE',  ( -36.94051212422546371, 491.4300504572172485, 12.31983948577911647 ) ) ;
#49350 = DIRECTION ( 'NONE',  ( 0.000000000000000000, 1.000000000000000000, 0.000000000000000000 ) ) ;
#49351 = CARTESIAN_POINT ( 'NONE',  ( 4.898587196589412829E-16, -24.31250000409677270, -8.000000000000000000 ) ) ;
#49352 = DIRECTION ( 'NONE',  ( 0.5735764363510490460, 0.8191520442889896891, 0.000000000000000000 ) ) ;
#49353 =( NAMED_UNIT ( * ) SI_UNIT ( $, .STERADIAN. ) SOLID_ANGLE_UNIT ( ) );
#49354 = DIRECTION ( 'NONE',  ( 0.000000000000000000, -1.000000000000000000, 0.000000000000000000 ) ) ;
#49355 = CIRCLE ( 'NONE', #2859, 4.000000000000000888 ) ;
#49356 = CARTESIAN_POINT ( 'NONE',  ( -6.220663814092025845, 4.180217462607255463, 5.000000000000000888 ) ) ;
#49357 = CARTESIAN_POINT ( 'NONE',  ( -18.41162169223098033, 304.6294254666754568, 9.889731659030220001 ) ) ;
#49358 =( NAMED_UNIT ( * ) PLANE_ANGLE_UNIT ( ) SI_UNIT ( $, .RADIAN. ) );
#49359 = ORIENTED_EDGE ( 'NONE', *, *, #26249, .F. ) ;
#49360 = DIRECTION ( 'NONE',  ( -1.000000000000000000, -0.000000000000000000, -0.000000000000000000 ) ) ;
#49361 = DIRECTION ( 'NONE',  ( -1.000000000000000000, -1.224606353822377258E-16, -0.000000000000000000 ) ) ;
#49362 = DIRECTION ( 'NONE',  ( -0.000000000000000000, 1.000000000000000000, 0.000000000000000000 ) ) ;
#49363 = CARTESIAN_POINT ( 'NONE',  ( -93.39911556732610620, -30.00000000000000711, 191.1953737942166924 ) ) ;
#49364 = EDGE_CURVE ( 'NONE', #17049, #73038, #97870, .T. ) ;
#49365 = CARTESIAN_POINT ( 'NONE',  ( -38.92806086102961416, 485.1409375601101601, -4.243407870181493458 ) ) ;
#49366 = CARTESIAN_POINT ( 'NONE',  ( 63.99273081836761889, -57.67907566170010369, 122.4759172911383303 ) ) ;
#49368 = CARTESIAN_POINT ( 'NONE',  ( 2.499999999999997335, -30.00000000000000000, 30.00000000000000000 ) ) ;
#49367 = CARTESIAN_POINT ( 'NONE',  ( -0.6416280306071847628, 26.01284353103483227, -38.42409783453992844 ) ) ;
#49369 = EDGE_CURVE ( 'NONE', #34458, #84319, #81000, .T. ) ;
#49370 = EDGE_CURVE ( 'NONE', #29485, #5037, #10393, .T. ) ;
#49371 = CARTESIAN_POINT ( 'NONE',  ( 5.476207722142115486, -21.71875361764507062, -38.54698999943882853 ) ) ;
#49372 = CARTESIAN_POINT ( 'NONE',  ( -7.500000000000000888, -0.7512838658081425480, 2.510605655661746205E-15 ) ) ;
#49373 = DIRECTION ( 'NONE',  ( 0.000000000000000000, -1.000000000000000000, 0.000000000000000000 ) ) ;
#49374 = CARTESIAN_POINT ( 'NONE',  ( -4.190096357442898878, -60.00000000000000711, 39.63091782826867160 ) ) ;
#49375 = AXIS2_PLACEMENT_3D ( 'NONE', #37485, #88648, #39051 ) ;
#49376 = CARTESIAN_POINT ( 'NONE',  ( 13.71930391805453553, 20.41463764547162896, 6.718748382517820694 ) ) ;
#49377 = CARTESIAN_POINT ( 'NONE',  ( 35.22245897681152371, 463.4774333389169101, 19.78759537333438345 ) ) ;
#49378 = CIRCLE ( 'NONE', #99343, 7.999999999999986677 ) ;
#49379 = CARTESIAN_POINT ( 'NONE',  ( -86.99319857952023938, -28.01872268044905923, 186.8509686606727200 ) ) ;
#49380 = ORIENTED_EDGE ( 'NONE', *, *, #103768, .T. ) ;
#49381 = DIRECTION ( 'NONE',  ( 0.000000000000000000, -1.000000000000000000, 0.000000000000000000 ) ) ;
#49382 = DIRECTION ( 'NONE',  ( 0.000000000000000000, 1.000000000000000000, 0.000000000000000000 ) ) ;
#49383 = CARTESIAN_POINT ( 'NONE',  ( -8.225604079535896673, -46.43935024322556160, 31.62298990380002550 ) ) ;
#49384 = CARTESIAN_POINT ( 'NONE',  ( 0.000000000000000000, 0.000000000000000000, 0.000000000000000000 ) ) ;
#49386 = CARTESIAN_POINT ( 'NONE',  ( 4.692764267120560717, -68.34565006887950744, 13.80912607275098658 ) ) ;
#49385 = FACE_OUTER_BOUND ( 'NONE', #46514, .T. ) ;
#49387 = ORIENTED_EDGE ( 'NONE', *, *, #42349, .T. ) ;
#49388 = ADVANCED_FACE ( 'NONE', ( #18039 ), #101851, .F. ) ;
#49389 = FILL_AREA_STYLE_COLOUR ( '', #52421 ) ;
#49390 = B_SPLINE_CURVE_WITH_KNOTS ( 'NONE', 3,
 ( #55286, #70958, #21909, #94184, #6204, #46680 ),
 .UNSPECIFIED., .F., .F.,
 ( 4, 2, 4 ),
 ( 0.005511122051665473358, 0.007432374760074465445, 0.009353627468483458399 ),
 .UNSPECIFIED. ) ;
#49391 = CARTESIAN_POINT ( 'NONE',  ( -7.731157688197621169, -5.000000000014319212, -17.87147387707815582 ) ) ;
#49392 = CARTESIAN_POINT ( 'NONE',  ( -7.045965687440314262, 31.30392463786035151, 3.790395326974318913 ) ) ;
#49393 = CARTESIAN_POINT ( 'NONE',  ( 26.74014876403748175, 304.8529031102725639, -9.560831669777455133 ) ) ;
#49394 = CARTESIAN_POINT ( 'NONE',  ( 0.000000000000000000, -15.00000000000000000, 0.000000000000000000 ) ) ;
#49395 = SHAPE_REPRESENTATION ( '3. Bracket', ( #10728 ), #7340 ) ;
#49396 = FACE_BOUND ( 'NONE', #1139, .T. ) ;
#49397 = DIRECTION ( 'NONE',  ( 0.000000000000000000, 0.000000000000000000, 1.000000000000000000 ) ) ;
#49398 = CARTESIAN_POINT ( 'NONE',  ( 113.5291039388664700, -60.00000000000007105, 153.5981272189337403 ) ) ;
#49399 = CARTESIAN_POINT ( 'NONE',  ( -45.33180403702434091, 464.4945808635454227, 2.178908857919817699 ) ) ;
#49400 = VERTEX_POINT ( 'NONE', #77857 ) ;
#49401 = CARTESIAN_POINT ( 'NONE',  ( 30.00000000000000000, 450.0000000000002274, 18.20242257375371153 ) ) ;
#49402 = CARTESIAN_POINT ( 'NONE',  ( 0.4969600502617449456, -4.995646404165267285, 7.347286611336970807 ) ) ;
#49403 = AXIS2_PLACEMENT_3D ( 'NONE', #76136, #68052, #99886 ) ;
#49404 = VECTOR ( 'NONE', #36044, 1000.000000000000000 ) ;
#49405 = CONICAL_SURFACE ( 'NONE', #75205, 6.500000000000000000, 1.047197551196600296 ) ;
#49406 = CIRCLE ( 'NONE', #106224, 8.750000000000023093 ) ;
#49407 = CARTESIAN_POINT ( 'NONE',  ( -35.37498230280494482, 485.2520700389512740, -2.749549059026963338 ) ) ;
#49408 = ADVANCED_FACE ( 'NONE', ( #68167 ), #24225, .T. ) ;
#49409 = CARTESIAN_POINT ( 'NONE',  ( 4.561148568382323631, 8.777942558635560388, -5.000000000000000000 ) ) ;
#49410 = DIRECTION ( 'NONE',  ( 0.000000000000000000, -1.000000000000000000, 0.000000000000000000 ) ) ;
#49411 = ORIENTED_EDGE ( 'NONE', *, *, #45393, .F. ) ;
#49412 = UNCERTAINTY_MEASURE_WITH_UNIT (LENGTH_MEASURE( 1.000000000000000082E-05 ), #95760, 'distance_accuracy_value', 'NONE');
#49413 = AXIS2_PLACEMENT_3D ( 'NONE', #35402, #68270, #75279 ) ;
#49415 = AXIS2_PLACEMENT_3D ( 'NONE', #95577, #103660, #4975 ) ;
#49414 = CARTESIAN_POINT ( 'NONE',  ( -22.33139259354657469, 304.3259814047488589, 10.03910396366137192 ) ) ;
#49416 = ORIENTED_EDGE ( 'NONE', *, *, #26263, .F. ) ;
#49417 = CARTESIAN_POINT ( 'NONE',  ( 88.20199406385988539, -5.000000000000000000, 6.123233995736778115E-16 ) ) ;
#49418 = CARTESIAN_POINT ( 'NONE',  ( 3.997425403568278579, 15.99999999372935022, 9.168149550320896068 ) ) ;
#49419 = CARTESIAN_POINT ( 'NONE',  ( 32.94539137534165718, 488.0149952105424518, 9.145905951749512042 ) ) ;
#49420 = VERTEX_POINT ( 'NONE', #44432 ) ;
#49421 = CARTESIAN_POINT ( 'NONE',  ( 58.90678327789231616, 48.00000000000000000, -28.11551192221969941 ) ) ;
#49422 = CARTESIAN_POINT ( 'NONE',  ( 5.000000000000000000, -14.90207541444466166, 12.47233211435964506 ) ) ;
#49423 = CARTESIAN_POINT ( 'NONE',  ( -71.03131189882361696, -60.00000000001953282, 166.0686979362143347 ) ) ;
#49424 = CARTESIAN_POINT ( 'NONE',  ( -10.38582326156070046, 145.0440906288519898, 0.000000000000000000 ) ) ;
#49425 = ORIENTED_EDGE ( 'NONE', *, *, #29370, .T. ) ;
#49426 = CARTESIAN_POINT ( 'NONE',  ( 106.1038126249908231, -60.00000000000002132, 198.1916009746322231 ) ) ;
#49428 = CARTESIAN_POINT ( 'NONE',  ( 15.42399563816537622, -25.54935048520918528, 28.31163924845273883 ) ) ;
#49427 = CARTESIAN_POINT ( 'NONE',  ( -114.4010969832937121, -60.00000000000006395, 179.2248356726699399 ) ) ;
#49429 = SURFACE_SIDE_STYLE ('',( #49964 ) ) ;
#49430 = CARTESIAN_POINT ( 'NONE',  ( -43.84331470278493725, -36.07451146886668880, 41.44895103270090431 ) ) ;
#49431 = CARTESIAN_POINT ( 'NONE',  ( 5.901338098438385416, -64.37119818154236839, 14.30438978747334033 ) ) ;
#49432 = EDGE_LOOP ( 'NONE', ( #80848, #53542, #63244, #42790 ) ) ;
#49433 = CARTESIAN_POINT ( 'NONE',  ( 89.99999999999997158, -38.00000000001091394, 196.0238439516549818 ) ) ;
#49434 = CARTESIAN_POINT ( 'NONE',  ( 16.10535093526683070, 21.79478144880583557, 1.090471457032648583 ) ) ;
#49435 = CARTESIAN_POINT ( 'NONE',  ( 31.03867016165222026, 468.3124986733989772, 18.90871194958903345 ) ) ;
#49436 = DIRECTION ( 'NONE',  ( 0.000000000000000000, -1.000000000000000000, 0.000000000000000000 ) ) ;
#49437 = CARTESIAN_POINT ( 'NONE',  ( -8.000000000000001776, -28.34375000409677270, 3.313708498984759387 ) ) ;
#49438 = CARTESIAN_POINT ( 'NONE',  ( 10.00200699113076652, -0.6430754150849513628, 20.04989093843450121 ) ) ;
#49440 = ORIENTED_EDGE ( 'NONE', *, *, #97547, .T. ) ;
#49439 = PRESENTATION_LAYER_ASSIGNMENT (  '', '', ( #87431 ) ) ;
#49441 = SURFACE_STYLE_USAGE ( .BOTH. , #88857 ) ;
#49442 = VERTEX_POINT ( 'NONE', #92971 ) ;
#49443 = CARTESIAN_POINT ( 'NONE',  ( 53.17600322138483904, -30.00000000000000000, 72.57813921009470448 ) ) ;
#49444 = CARTESIAN_POINT ( 'NONE',  ( 47.03691741412936267, 13.53106325772396268, 14.84138715777531381 ) ) ;
#49445 = CARTESIAN_POINT ( 'NONE',  ( 33.00000000000000000, 450.0000000000002274, -1.797577426246301568 ) ) ;
#49446 = CONICAL_SURFACE ( 'NONE', #37491, 5.000000000000010658, 0.9599310885968697082 ) ;
#49447 = CARTESIAN_POINT ( 'NONE',  ( 8.000000000000000000, 9.797174393178825657E-16, -1.875285714285714445 ) ) ;
#49448 = CARTESIAN_POINT ( 'NONE',  ( 90.99536718434406168, -29.99999999999998934, 94.30297898937882906 ) ) ;
#49449 = CARTESIAN_POINT ( 'NONE',  ( -21.29078873992701659, 304.0464254837385170, 9.978592173037190705 ) ) ;
#49450 = ORIENTED_EDGE ( 'NONE', *, *, #28060, .T. ) ;
#49451 = EDGE_CURVE ( 'NONE', #57919, #4171, #87875, .T. ) ;
#49452 = VERTEX_POINT ( 'NONE', #83808 ) ;
#49453 = ORIENTED_EDGE ( 'NONE', *, *, #61367, .F. ) ;
#49454 = DIRECTION ( 'NONE',  ( 0.000000000000000000, -1.000000000000000000, 0.000000000000000000 ) ) ;
#49455 = CARTESIAN_POINT ( 'NONE',  ( -6.057904167604424295, 41.61856606222242760, -70.65344123333893833 ) ) ;
#49456 = FACE_OUTER_BOUND ( 'NONE', #19617, .T. ) ;
#49457 = CARTESIAN_POINT ( 'NONE',  ( -31.39122502990187513, 374.8582828950688963, 22.89686894917594273 ) ) ;
#49458 = ADVANCED_FACE ( 'NONE', ( #3439 ), #77326, .T. ) ;
#49459 = VECTOR ( 'NONE', #92674, 1000.000000000000000 ) ;
#49460 = ORIENTED_EDGE ( 'NONE', *, *, #55231, .F. ) ;
#49462 = EDGE_CURVE ( 'NONE', #63533, #96201, #105116, .T. ) ;
#49461 = DIRECTION ( 'NONE',  ( -1.000000000000000000, -1.224606353822377258E-16, -0.000000000000000000 ) ) ;
#49463 = ORIENTED_EDGE ( 'NONE', *, *, #33907, .T. ) ;
#49464 = DIRECTION ( 'NONE',  ( 1.000000000000000000, 0.000000000000000000, -0.000000000000000000 ) ) ;
#49465 = CARTESIAN_POINT ( 'NONE',  ( 79.84856180006062232, -38.77050156954319959, 192.7098517259555308 ) ) ;
#49466 = DIRECTION ( 'NONE',  ( 0.000000000000000000, 0.000000000000000000, 1.000000000000000000 ) ) ;
#49467 = CARTESIAN_POINT ( 'NONE',  ( 32.67437147574466394, 300.1844539814272821, 3.135089118897082638 ) ) ;
#49468 = LINE ( 'NONE', #106642, #33309 ) ;
#49469 = AXIS2_PLACEMENT_3D ( 'NONE', #81072, #56793, #105879 ) ;
#49470 = EDGE_CURVE ( 'NONE', #40845, #57762, #91344, .T. ) ;
#49471 = DIRECTION ( 'NONE',  ( -1.000000000000000000, -1.224606353822377258E-16, -0.000000000000000000 ) ) ;
#49472 = ADVANCED_FACE ( 'NONE', ( #76251 ), #3971, .T. ) ;
#49473 = ADVANCED_FACE ( 'NONE', ( #10973 ), #13796, .F. ) ;
#49474 = DIRECTION ( 'NONE',  ( 0.000000000000000000, -1.000000000000000000, 0.000000000000000000 ) ) ;
#49475 = CARTESIAN_POINT ( 'NONE',  ( -4.211261491276468760, -48.41319459706108574, 103.7733746176733689 ) ) ;
#49476 = CARTESIAN_POINT ( 'NONE',  ( 0.000000000000000000, 0.000000000000000000, -0.01269999999999786924 ) ) ;
#49477 = ORIENTED_EDGE ( 'NONE', *, *, #69142, .F. ) ;
#49478 = FACE_OUTER_BOUND ( 'NONE', #38311, .T. ) ;
#49479 = CARTESIAN_POINT ( 'NONE',  ( -24.18257333278238264, 295.4930867534158665, 10.07449787404065233 ) ) ;
#49480 = CARTESIAN_POINT ( 'NONE',  ( 7.311243580803559183, 54.26735737584581187, -2.887849316459860205 ) ) ;
#49481 = UNCERTAINTY_MEASURE_WITH_UNIT (LENGTH_MEASURE( 1.000000000000000082E-05 ), #1970, 'distance_accuracy_value', 'NONE');
#49482 = DIRECTION ( 'NONE',  ( 1.000000000000000000, 1.224606353822377258E-16, 0.000000000000000000 ) ) ;
#49483 = CARTESIAN_POINT ( 'NONE',  ( 7.999999999999998224, -11.09374999999999289, 3.313708498984766493 ) ) ;
#49484 = STYLED_ITEM ( 'NONE', ( #90528 ), #25990 ) ;
#49486 = DIRECTION ( 'NONE',  ( 0.000000000000000000, -1.000000000000000000, 0.000000000000000000 ) ) ;
#49485 = AXIS2_PLACEMENT_3D ( 'NONE', #88556, #47544, #64803 ) ;
#49487 = LINE ( 'NONE', #65681, #27118 ) ;
#49488 = CIRCLE ( 'NONE', #56322, 10.00000000000000178 ) ;
#49489 = CIRCLE ( 'NONE', #52964, 1.000000000000000888 ) ;
#49490 = FACE_OUTER_BOUND ( 'NONE', #101354, .T. ) ;
#49491 = AXIS2_PLACEMENT_3D ( 'NONE', #7636, #98776, #32495 ) ;
#49492 = CARTESIAN_POINT ( 'NONE',  ( 83.91935083234469062, -61.03361821168092405, 192.1967390494019696 ) ) ;
#49493 = CARTESIAN_POINT ( 'NONE',  ( 1.128077836147720614, 302.8478239976497548, 9.936168295454386623 ) ) ;
#49494 = CARTESIAN_POINT ( 'NONE',  ( -4.313246244820144959, 141.0138720982649829, 5.000000000000002665 ) ) ;
#49495 = VERTEX_POINT ( 'NONE', #26686 ) ;
#49496 = CARTESIAN_POINT ( 'NONE',  ( 91.47756376649307697, -57.66240114371687042, -20.19489575921430102 ) ) ;
#49497 = CARTESIAN_POINT ( 'NONE',  ( 41.46910480218704009, 484.7338956289814860, -3.418960549715446717 ) ) ;
#49498 = CIRCLE ( 'NONE', #16778, 1.000000000000000888 ) ;
#49499 = CARTESIAN_POINT ( 'NONE',  ( 28.56337834059337055, 13.37291324415828875, 40.29174292248561784 ) ) ;
#49500 = CONICAL_SURFACE ( 'NONE', #28934, 3.309500000000001663, 0.9599310885968770357 ) ;
#49501 = CARTESIAN_POINT ( 'NONE',  ( -81.58524466189544455, -30.00000000000001421, -7.583927274541655272 ) ) ;
#49502 = CARTESIAN_POINT ( 'NONE',  ( -82.22606752459770973, -38.00000000000003553, 160.2907289571271860 ) ) ;
#49503 = DIRECTION ( 'NONE',  ( -1.000000000000000000, -0.000000000000000000, -0.000000000000000000 ) ) ;
#49504 = DIRECTION ( 'NONE',  ( 1.000000000000000000, 1.224606353822377258E-16, 0.000000000000000000 ) ) ;
#49506 = DIRECTION ( 'NONE',  ( 0.000000000000000000, -1.000000000000000000, 0.000000000000000000 ) ) ;
#49505 = CARTESIAN_POINT ( 'NONE',  ( 3.352941176470589646, -48.79941684889505638, 104.5794940929807524 ) ) ;
#49507 = EDGE_CURVE ( 'NONE', #97345, #30914, #36260, .T. ) ;
#49508 = CONICAL_SURFACE ( 'NONE', #6465, 3.309500000000001663, 0.9599310885968770357 ) ;
#49509 = DIRECTION ( 'NONE',  ( -1.000000000000000000, -1.224606353822377258E-16, -0.000000000000000000 ) ) ;
#49510 = CARTESIAN_POINT ( 'NONE',  ( 85.31310517497098544, 5.000000000000021316, 0.000000000000000000 ) ) ;
#49511 = CYLINDRICAL_SURFACE ( 'NONE', #94557, 4.000000000000000000 ) ;
#49512 = DIRECTION ( 'NONE',  ( 0.6181567188933647650, -0.3028222199719650121, 0.7253833289911206794 ) ) ;
#49513 = DIRECTION ( 'NONE',  ( 0.000000000000000000, 0.000000000000000000, -1.000000000000000000 ) ) ;
#49514 = CARTESIAN_POINT ( 'NONE',  ( 33.75766768374546700, 485.0582975308568621, 1.699565690043864707 ) ) ;
#49515 = EDGE_LOOP ( 'NONE', ( #80368, #40518, #74379, #99611, #24050 ) ) ;
#49516 = CARTESIAN_POINT ( 'NONE',  ( 5.819846122303832914, -6.321060697775078729, -2.051601713726796561 ) ) ;
#49517 = AXIS2_PLACEMENT_3D ( 'NONE', #98744, #1644, #27045 ) ;
#49518 = CARTESIAN_POINT ( 'NONE',  ( -7.801777176595949825, 81.41172014187367267, -1.786991866639916715 ) ) ;
#49519 = CARTESIAN_POINT ( 'NONE',  ( 43.02661387979727436, 465.7449615347604208, 11.43319743843670544 ) ) ;
#49521 = CARTESIAN_POINT ( 'NONE',  ( -67.74125374443480041, -34.58950197393470916, -22.71994573540199625 ) ) ;
#49520 = DIRECTION ( 'NONE',  ( 0.000000000000000000, 0.4999999999999999445, -0.8660254037844387076 ) ) ;
#49522 = VERTEX_POINT ( 'NONE', #84357 ) ;
#49523 = B_SPLINE_CURVE_WITH_KNOTS ( 'NONE', 3,
 ( #12336, #86791, #12862, #78140, #37190, #37732, #78654, #70052, #4792, #102958, #29122, #70591, #103483, #84649, #10733, #97490, #31223, #87308, #71112, #32263, #80787, #73216, #96985, #63575, #88373, #55961, #104533 ),
 .UNSPECIFIED., .F., .F.,
 ( 4, 2, 2, 2, 2, 2, 1, 2, 2, 2, 2, 2, 2, 4 ),
 ( 0.000000000000000000, 0.1250000000000165701, 0.2500000000000331402, 0.3750000000000497380, 0.4375000000000578426, 0.4687500000000607847, 0.4843750000000630607, 0.4921875000000641154, 0.5000000000000651701, 0.6250000000000489608, 0.7500000000000326406, 0.8750000000000164313, 0.9375000000000082157, 1.000000000000000000 ),
 .UNSPECIFIED. ) ;
#49524 = ORIENTED_EDGE ( 'NONE', *, *, #41679, .F. ) ;
#49525 = CARTESIAN_POINT ( 'NONE',  ( -2.683400376901624263E-15, -5.469921996229798467, 3.525817189091414949 ) ) ;
#49526 = MECHANICAL_DESIGN_GEOMETRIC_PRESENTATION_REPRESENTATION (  '', ( #101220 ), #54680 ) ;
#49527 = ADVANCED_FACE ( 'NONE', ( #10450 ), #27221, .F. ) ;
#49528 = CARTESIAN_POINT ( 'NONE',  ( 10.28624191511773844, 43.25714326066793092, -15.40779740156427202 ) ) ;
#49529 = CARTESIAN_POINT ( 'NONE',  ( -0.8333261453522353701, -30.00000000000001421, 28.88964995960238369 ) ) ;
#49530 = CARTESIAN_POINT ( 'NONE',  ( -82.02569044098642337, -60.00000000000000000, -26.68448968580177905 ) ) ;
#49531 = ORIENTED_EDGE ( 'NONE', *, *, #77389, .F. ) ;
#49532 = CARTESIAN_POINT ( 'NONE',  ( 48.18879443871838930, -35.41177168222470328, -28.23099784303214577 ) ) ;
#49533 = CARTESIAN_POINT ( 'NONE',  ( -6.752503985042242363, 294.7360527384791453, -7.398079589859515970 ) ) ;
#49534 = CARTESIAN_POINT ( 'NONE',  ( 99.46726541099765484, -52.78227579418069837, 194.5120875942841394 ) ) ;
#49536 = CARTESIAN_POINT ( 'NONE',  ( -47.55643143940722695, 10.90089820249354879, 16.76894861493079603 ) ) ;
#49535 = LINE ( 'NONE', #39869, #66352 ) ;
#49537 = EDGE_CURVE ( 'NONE', #81845, #53956, #3497, .T. ) ;
#49538 = AXIS2_PLACEMENT_3D ( 'NONE', #61192, #2401, #43934 ) ;
#49539 = ORIENTED_EDGE ( 'NONE', *, *, #78440, .T. ) ;
#49540 = ORIENTED_EDGE ( 'NONE', *, *, #46196, .T. ) ;
#49541 = VERTEX_POINT ( 'NONE', #35842 ) ;
#49543 =( BOUNDED_SURFACE ( )  B_SPLINE_SURFACE ( 3, 2, ( 
 ( #85846, #18454, #91796 ),
 ( #43762, #44848, #84231 ),
 ( #11379, #28155, #43241 ),
 ( #20075, #100935, #2223 ) ),
 .UNSPECIFIED., .F., .F., .F. ) 
 B_SPLINE_SURFACE_WITH_KNOTS ( ( 4, 4 ),
 ( 3, 3 ),
 ( -2.775557561562891351E-17, 0.001861785345366372352 ),
 ( 0.000000000000000000, 1.000000000000000000 ),
 .UNSPECIFIED. ) 
 GEOMETRIC_REPRESENTATION_ITEM ( )  RATIONAL_B_SPLINE_SURFACE ( (
 ( 1.000000000000000000, 0.7560596356357111025, 1.000000000000000000),
 ( 1.000000000000000000, 0.7634190799318307796, 1.000000000000000000),
 ( 1.000000000000000000, 0.7696912645870118697, 1.000000000000000000),
 ( 1.000000000000000000, 0.7737149417968429699, 1.000000000000000000) ) ) 
 REPRESENTATION_ITEM ( '' )  SURFACE ( )  );
#49542 = CARTESIAN_POINT ( 'NONE',  ( 29.85428238372634269, 328.3168341217437387, 14.69675115712503910 ) ) ;
#49544 = CARTESIAN_POINT ( 'NONE',  ( -4.999999999999999112, -12.61682532715667904, 11.58371340991526921 ) ) ;
#49545 = CARTESIAN_POINT ( 'NONE',  ( 9.539861337244017747, 53.58159379677093170, 1.989136213324401492 ) ) ;
#49546 = EDGE_LOOP ( 'NONE', ( #93088, #28712 ) ) ;
#49547 = CARTESIAN_POINT ( 'NONE',  ( 30.00000000000000000, 450.0000000000002274, 25.20242257375371864 ) ) ;
#49548 = CARTESIAN_POINT ( 'NONE',  ( -8.331345277524542681, 1.033251829022860324E-15, -8.000000000000000000 ) ) ;
#49549 = CARTESIAN_POINT ( 'NONE',  ( 11.36650669486618881, 4.898587196589413815E-16, -4.000000000000000888 ) ) ;
#49550 = CARTESIAN_POINT ( 'NONE',  ( -2.832004189415751050, -57.67120204282113605, 41.61186672541032294 ) ) ;
#49551 = CARTESIAN_POINT ( 'NONE',  ( -7.188101187500000044, -28.90625000204838813, -8.802885111219163269E-16 ) ) ;
#49552 = CARTESIAN_POINT ( 'NONE',  ( -30.93146042459081002, 14.42085588385339712, 40.69811146320443385 ) ) ;
#49553 = COLOUR_RGB ( '', 0.66274510, 0.83137255, 0.94901961) ;
#49554 = CARTESIAN_POINT ( 'NONE',  ( -16.05785784214673484, 4.775831776474317891, -3.710403933782548513 ) ) ;
#49555 = CONICAL_SURFACE ( 'NONE', #63369, 4.000000000000001776, 0.9599310885968808105 ) ;
#49556 = CARTESIAN_POINT ( 'NONE',  ( 41.39111156191358276, -30.00000000000003908, -36.78675873448672462 ) ) ;
#49557 = CARTESIAN_POINT ( 'NONE',  ( -12.46506237085073110, -30.00000000000006395, 37.03826559298295251 ) ) ;
#49558 = CARTESIAN_POINT ( 'NONE',  ( -50.37523485278211410, -32.58700810942853110, 49.03711277103302280 ) ) ;
#49559 = FACE_OUTER_BOUND ( 'NONE', #57132, .T. ) ;
#49560 = PRODUCT_RELATED_PRODUCT_CATEGORY ( 'part', '', ( #36449 ) ) ;
#49562 = EDGE_LOOP ( 'NONE', ( #88723, #78345, #5444, #24228, #36910 ) ) ;
#49561 = PRESENTATION_LAYER_ASSIGNMENT (  '', '', ( #27215 ) ) ;
#49563 = VECTOR ( 'NONE', #37781, 999.9999999999998863 ) ;
#49564 = CARTESIAN_POINT ( 'NONE',  ( -101.2893714159135925, -60.24741957559085392, 194.9011525870544972 ) ) ;
#49565 = DIRECTION ( 'NONE',  ( 0.000000000000000000, -0.9109553866901075603, 0.4125048890137871238 ) ) ;
#49566 = CARTESIAN_POINT ( 'NONE',  ( 15.66776169706031396, -1.217559620640022100, 14.95230841597768290 ) ) ;
#49567 = ORIENTED_EDGE ( 'NONE', *, *, #2403, .F. ) ;
#49568 = CARTESIAN_POINT ( 'NONE',  ( -17.83068241833874623, 34.57775873570747649, -22.40589842973222900 ) ) ;
#49569 = CARTESIAN_POINT ( 'NONE',  ( 99.79593632746312437, -38.46925667693373185, 200.5817790329920456 ) ) ;
#49570 = CARTESIAN_POINT ( 'NONE',  ( 21.84999999999999787, 1.533819458162526451E-15, 0.000000000000000000 ) ) ;
#49571 = CARTESIAN_POINT ( 'NONE',  ( -5.689124116752916294, 51.96569795582090734, -6.093860943101484295 ) ) ;
#49572 = DIRECTION ( 'NONE',  ( 0.000000000000000000, -1.000000000000000000, 0.000000000000000000 ) ) ;
#49573 = CARTESIAN_POINT ( 'NONE',  ( -45.60838156036751201, 42.00000000000000000, -79.13121736029046360 ) ) ;
#49574 = CARTESIAN_POINT ( 'NONE',  ( 82.58295863708946172, -30.00000000000000711, 149.9139447893771262 ) ) ;
#49575 = CIRCLE ( 'NONE', #59924, 15.00000000000000000 ) ;
#49576 = CARTESIAN_POINT ( 'NONE',  ( 35.15824258293613980, 491.5080798214766560, 12.36499586377719062 ) ) ;
#49577 = CARTESIAN_POINT ( 'NONE',  ( -34.86930528710281862, 472.8495416016138506, 16.94467871989038343 ) ) ;
#49578 = TOROIDAL_SURFACE ( 'NONE', #106392, 7.500000000000000888, 5.000000000000000000 ) ;
#49579 = ORIENTED_EDGE ( 'NONE', *, *, #14168, .F. ) ;
#49580 = EDGE_LOOP ( 'NONE', ( #75295, #66320, #103062, #71745, #49097 ) ) ;
#49581 = CARTESIAN_POINT ( 'NONE',  ( 52.40275982922914011, -22.17845676421043422, 48.78481890060238868 ) ) ;
#49582 = CARTESIAN_POINT ( 'NONE',  ( 6.635365873752379962, 41.60399788275461219, -58.75656668935356919 ) ) ;
#49583 = CARTESIAN_POINT ( 'NONE',  ( 2.500000000000002665, -30.00000000000000000, -14.79019945774903810 ) ) ;
#49584 = EDGE_CURVE ( 'NONE', #50075, #92851, #60633, .T. ) ;
#49585 = ORIENTED_EDGE ( 'NONE', *, *, #85240, .F. ) ;
#49586 = CARTESIAN_POINT ( 'NONE',  ( -91.77192237904225181, -38.35461803959927352, 32.56391333383364639 ) ) ;
#49587 = VECTOR ( 'NONE', #56725, 1000.000000000000000 ) ;
#49588 = ORIENTED_EDGE ( 'NONE', *, *, #99878, .T. ) ;
#49589 = CARTESIAN_POINT ( 'NONE',  ( 7.999999999999998224, -29.28125000409677270, 3.313708498984766049 ) ) ;
#49590 = CARTESIAN_POINT ( 'NONE',  ( 91.15118748837623741, -38.35268490642818762, 25.35169414273645216 ) ) ;
#49591 = CARTESIAN_POINT ( 'NONE',  ( 14.98940227155761384, 22.23241460859703267, 3.884032814068775874 ) ) ;
#49592 = CARTESIAN_POINT ( 'NONE',  ( 97.20070980819903639, -52.71699338941720470, 105.9753043912546673 ) ) ;
#49593 = FILL_AREA_STYLE_COLOUR ( '', #53831 ) ;
#49594 = CARTESIAN_POINT ( 'NONE',  ( -33.82200258925038838, 329.9395885283731218, -2.846730487787179520 ) ) ;
#49595 = CARTESIAN_POINT ( 'NONE',  ( 4.699999999999999289, 6.499999999999999112, 0.000000000000000000 ) ) ;
#49596 = AXIS2_PLACEMENT_3D ( 'NONE', #77596, #68985, #101339 ) ;
#49597 = CARTESIAN_POINT ( 'NONE',  ( 74.84184181931864543, -59.99999999999998579, 180.0432328657729784 ) ) ;
#49598 = EDGE_CURVE ( 'NONE', #41885, #62849, #100784, .T. ) ;
#49599 = CARTESIAN_POINT ( 'NONE',  ( 18.06487379447606756, 45.00000000000000711, 62.52595132501897979 ) ) ;
#49600 = VERTEX_POINT ( 'NONE', #95638 ) ;
#49601 = CARTESIAN_POINT ( 'NONE',  ( 61.73071043583632900, -18.64118289587166899, 66.86164523920359670 ) ) ;
#49602 = EDGE_CURVE ( 'NONE', #89572, #13768, #80488, .T. ) ;
#49603 = CARTESIAN_POINT ( 'NONE',  ( -25.97041880520462698, 295.9150275961153511, -1.771067803760172366 ) ) ;
#49604 = CARTESIAN_POINT ( 'NONE',  ( 0.000000000000000000, 0.000000000000000000, 0.000000000000000000 ) ) ;
#49605 = CARTESIAN_POINT ( 'NONE',  ( -8.292751449259418095, -5.000000000000000888, -16.13133567586304906 ) ) ;
#49607 = CARTESIAN_POINT ( 'NONE',  ( -36.06936872001291761, 485.1953429453741364, -2.471779398547188311 ) ) ;
#49606 = CARTESIAN_POINT ( 'NONE',  ( -80.31910585633404764, -38.35622671115012139, -26.31299467937850523 ) ) ;
#49608 = CARTESIAN_POINT ( 'NONE',  ( -40.35637509736679363, 344.7269692263602110, 21.61016027867152900 ) ) ;
#49609 = CARTESIAN_POINT ( 'NONE',  ( 12.34835181856063002, -4.332967528434596538, -12.86601580078908214 ) ) ;
#49610 = CARTESIAN_POINT ( 'NONE',  ( -37.88504238421052861, 463.4171042825119002, 19.90923349044181379 ) ) ;
#49611 = CARTESIAN_POINT ( 'NONE',  ( -1.469576158976823947E-15, -24.87499999999999289, 8.000000000000000000 ) ) ;
#49612 = CARTESIAN_POINT ( 'NONE',  ( -18.91791044776116237, 47.99999999999999289, 62.18611311450883505 ) ) ;
#49613 = AXIS2_PLACEMENT_3D ( 'NONE', #12302, #20469, #28534 ) ;
#49614 = LINE ( 'NONE', #89558, #63877 ) ;
#49615 = CONICAL_SURFACE ( 'NONE', #106426, 4.000000000000007105, 0.9599310885968835860 ) ;
#49616 = VERTEX_POINT ( 'NONE', #105316 ) ;
#49617 = CARTESIAN_POINT ( 'NONE',  ( 83.43530994757759345, -42.97836967012928966, 178.5296786636865534 ) ) ;
#49618 = CARTESIAN_POINT ( 'NONE',  ( 43.47770857297100378, 484.8227827122626081, 4.253339224814538078 ) ) ;
#49619 = STYLED_ITEM ( 'NONE', ( #20527 ), #68261 ) ;
#49620 = CARTESIAN_POINT ( 'NONE',  ( -8.000000000000000000, -8.937500004096769146, -9.797174393178825657E-16 ) ) ;
#49621 = VERTEX_POINT ( 'NONE', #4498 ) ;
#49622 = CARTESIAN_POINT ( 'NONE',  ( 19.34999999999999787, 1.533819458162526451E-15, 0.000000000000000000 ) ) ;
#49623 = DIRECTION ( 'NONE',  ( 0.5735764363510470476, -0.8191520442889911324, 1.003171929053524007E-16 ) ) ;
#49624 = DIRECTION ( 'NONE',  ( 0.000000000000000000, 1.000000000000000000, 0.000000000000000000 ) ) ;
#49625 = CARTESIAN_POINT ( 'NONE',  ( 1.912569619637256418E-15, -1.500000000000000000, -15.43455230191221261 ) ) ;
#49626 = CARTESIAN_POINT ( 'NONE',  ( -49.86794645319100994, 40.83866221574536581, -41.94290818787430908 ) ) ;
#49627 = FACE_OUTER_BOUND ( 'NONE', #75238, .T. ) ;
#49628 = AXIS2_PLACEMENT_3D ( 'NONE', #66267, #50593, #99154 ) ;
#49629 = MECHANICAL_DESIGN_GEOMETRIC_PRESENTATION_REPRESENTATION (  '', ( #85862 ), #80658 ) ;
#49630 = AXIS2_PLACEMENT_3D ( 'NONE', #36990, #35395, #94127 ) ;
#49631 = CARTESIAN_POINT ( 'NONE',  ( -6.750000000000015099, -11.69134295108991495, 0.000000000000000000 ) ) ;
#49632 = CARTESIAN_POINT ( 'NONE',  ( 0.6448156900331544206, 25.22696244642840924, 40.58375750131497028 ) ) ;
#49634 = CARTESIAN_POINT ( 'NONE',  ( -14.09421869355620593, 20.98092464764351561, -6.031492443631700340 ) ) ;
#49633 = CARTESIAN_POINT ( 'NONE',  ( -21.81185593177036353, -26.89099996095279366, 37.28562843958906114 ) ) ;
#49635 = ADVANCED_FACE ( 'NONE', ( #22305 ), #46547, .T. ) ;
#49636 = CARTESIAN_POINT ( 'NONE',  ( 2.977408999572651815, -11.93750000204838457, 7.188101187500000933 ) ) ;
#49637 = CARTESIAN_POINT ( 'NONE',  ( 22.86660670453057165, 295.1252011229040590, -1.941278114811820110 ) ) ;
#49638 = AXIS2_PLACEMENT_3D ( 'NONE', #61595, #63714, #86408 ) ;
#49639 = FACE_OUTER_BOUND ( 'NONE', #55375, .T. ) ;
#49640 = VERTEX_POINT ( 'NONE', #79964 ) ;
#49641 = CARTESIAN_POINT ( 'NONE',  ( -19.49880643229725408, 49.99998348590659702, 59.93398820730007515 ) ) ;
#49642 = CARTESIAN_POINT ( 'NONE',  ( 23.29962249077899727, 25.97067266342275715, 30.70617127781015654 ) ) ;
#49643 = CARTESIAN_POINT ( 'NONE',  ( -38.54489124932221955, 464.3862832426350451, 18.94817373525692261 ) ) ;
#49646 = CARTESIAN_POINT ( 'NONE',  ( 56.96794851135737048, -21.77000581858095174, -23.90161939876400865 ) ) ;
#49645 = CARTESIAN_POINT ( 'NONE',  ( 5.290067270632397012, 54.20842449845690680, 6.031152949374294359 ) ) ;
#49644 = B_SPLINE_CURVE_WITH_KNOTS ( 'NONE', 3,
 ( #8084, #58228, #91157, #17263, #89547, #31856, #82511, #56625, #6485, #80907, #64736, #106773, #33451, #105198, #97613, #48000, #32922, #15642, #39416, #98675, #65265, #40988, #16715, #74401, #49062, #65798, #64224, #8613, #39935, #24829, #7538, #40454, #481, #90605 ),
 .UNSPECIFIED., .F., .F.,
 ( 4, 2, 2, 2, 2, 2, 2, 2, 2, 2, 2, 2, 2, 2, 2, 2, 4 ),
 ( 6.938893903907228378E-18, 0.0007899780065504824781, 0.001579956013100958017, 0.002369934019651433448, 0.003159912026201909096, 0.003949890032752384310, 0.004739868039302859958, 0.005529846045853335605, 0.006319824052403811253, 0.007109802058954286900, 0.007899780065504761681, 0.008689758072055237328, 0.009479736078605712976, 0.01026971408515618862, 0.01105969209170666427, 0.01184967009825713992, 0.01263964810480761557 ),
 .UNSPECIFIED. ) ;
#49647 = ORIENTED_EDGE ( 'NONE', *, *, #82026, .F. ) ;
#49648 = PRESENTATION_LAYER_ASSIGNMENT (  '', '', ( #96184 ) ) ;
#49649 = CARTESIAN_POINT ( 'NONE',  ( -4.472135954999578722, -85.27411850998325349, -4.000000000000003553 ) ) ;
#49650 = CARTESIAN_POINT ( 'NONE',  ( -4.038444544431111893, 51.98515651805179516, 7.232149228015535947 ) ) ;
#49651 = EDGE_LOOP ( 'NONE', ( #72080, #79703, #101931, #104677, #93800 ) ) ;
#49652 = CARTESIAN_POINT ( 'NONE',  ( 22.61650669486618526, -3.851859888774471706E-31, 4.000000000000000888 ) ) ;
#49653 = SURFACE_STYLE_USAGE ( .BOTH. , #90123 ) ;
#49654 = CONICAL_SURFACE ( 'NONE', #63474, 5.000000000000001776, 0.9599310885968803664 ) ;
#49655 = CARTESIAN_POINT ( 'NONE',  ( -21.89416662624832099, 41.75480087786124272, -77.14963689140114411 ) ) ;
#49656 = CARTESIAN_POINT ( 'NONE',  ( -95.56678818837158929, -59.99999999999998579, 53.06396543177949354 ) ) ;
#49657 = CARTESIAN_POINT ( 'NONE',  ( 28.61312531052607255, 18.65874454358747769, -40.19656138064517137 ) ) ;
#49658 = CARTESIAN_POINT ( 'NONE',  ( 6.936184427528457874, 0.000000000000000000, -8.605212085995399107 ) ) ;
#49659 = CARTESIAN_POINT ( 'NONE',  ( 35.74363442581862671, 380.1068966271811860, 4.951945592532029927 ) ) ;
#49661 = FACE_OUTER_BOUND ( 'NONE', #59464, .T. ) ;
#49660 = CARTESIAN_POINT ( 'NONE',  ( -3.140974613990812792, -5.000000000000002665, -96.68767211932356531 ) ) ;
#49662 = AXIS2_PLACEMENT_3D ( 'NONE', #55009, #15092, #88472 ) ;
#49663 = EDGE_CURVE ( 'NONE', #89014, #10653, #78380, .T. ) ;
#49664 = CARTESIAN_POINT ( 'NONE',  ( -84.54716333029104192, -28.99156628927957158, 167.9126512817154264 ) ) ;
#49665 = ORIENTED_EDGE ( 'NONE', *, *, #40254, .F. ) ;
#49666 =( LENGTH_UNIT ( ) NAMED_UNIT ( * ) SI_UNIT ( .MILLI., .METRE. ) );
#49667 = ORIENTED_EDGE ( 'NONE', *, *, #12325, .F. ) ;
#49668 = ORIENTED_EDGE ( 'NONE', *, *, #93067, .F. ) ;
#49669 = FACE_BOUND ( 'NONE', #5288, .T. ) ;
#49670 = EDGE_CURVE ( 'NONE', #3656, #74698, #27634, .T. ) ;
#49671 = DIRECTION ( 'NONE',  ( -0.5735764363510512664, 0.8191520442889881348, 1.003171929053520309E-16 ) ) ;
#49672 = ORIENTED_EDGE ( 'NONE', *, *, #46061, .F. ) ;
#49673 = DIRECTION ( 'NONE',  ( -1.000000000000000000, -1.224606353822377258E-16, -0.000000000000000000 ) ) ;
#49674 = DIRECTION ( 'NONE',  ( -1.000000000000000000, -1.224606353822377258E-16, -0.000000000000000000 ) ) ;
#49675 = DIRECTION ( 'NONE',  ( 0.000000000000000000, -1.000000000000000000, 0.000000000000000000 ) ) ;
#49676 = CARTESIAN_POINT ( 'NONE',  ( -4.000000000000000000, 17.85270131633358304, 5.744562646538042827 ) ) ;
#49677 = FACE_OUTER_BOUND ( 'NONE', #43392, .T. ) ;
#49678 = CARTESIAN_POINT ( 'NONE',  ( 12.12965108312117479, -5.000000000000000000, -89.82640756711197128 ) ) ;
#49679 = CARTESIAN_POINT ( 'NONE',  ( -17.49999999999997513, 50.00000000000000000, 100.0000000000000000 ) ) ;
#49680 = CARTESIAN_POINT ( 'NONE',  ( 114.4011996162234510, -59.99999999999997158, 179.2244502532067827 ) ) ;
#49681 = CARTESIAN_POINT ( 'NONE',  ( -114.0148073962512854, -59.99999999999994316, 183.4850465800912218 ) ) ;
#49682 = EDGE_CURVE ( 'NONE', #52131, #9396, #37435, .T. ) ;
#49683 = CARTESIAN_POINT ( 'NONE',  ( -62.14394237747171701, -53.39298685405226053, 85.00033226795140706 ) ) ;
#49684 = ORIENTED_EDGE ( 'NONE', *, *, #31393, .F. ) ;
#49685 = CARTESIAN_POINT ( 'NONE',  ( -5.800528474434197612, 38.95336917065268523, 63.47065297900079628 ) ) ;
#49686 = CARTESIAN_POINT ( 'NONE',  ( 94.78037765028581418, -59.99999999999025846, -12.41180976829698857 ) ) ;
#49687 = ORIENTED_EDGE ( 'NONE', *, *, #56945, .T. ) ;
#49688 = CARTESIAN_POINT ( 'NONE',  ( 6.014821585911270141, -25.54826201030574495, 28.13812934727146953 ) ) ;
#49689 = CARTESIAN_POINT ( 'NONE',  ( -102.7041175444934709, -45.26540032460502516, 151.6231392685371020 ) ) ;
#49690 = CARTESIAN_POINT ( 'NONE',  ( 7.188101187499999156, -15.12500000204838457, 2.977408999572654924 ) ) ;
#49691 = STYLED_ITEM ( 'NONE', ( #10562 ), #1263 ) ;
#49692 = FACE_OUTER_BOUND ( 'NONE', #21453, .T. ) ;
#49693 = ORIENTED_EDGE ( 'NONE', *, *, #91217, .T. ) ;
#49695 = CARTESIAN_POINT ( 'NONE',  ( 36.67849848893011000, 463.9785128198733446, 19.62079535019029564 ) ) ;
#49694 = AXIS2_PLACEMENT_3D ( 'NONE', #22077, #9566, #17689 ) ;
#49696 = VERTEX_POINT ( 'NONE', #87029 ) ;
#49697 = CARTESIAN_POINT ( 'NONE',  ( 0.000000000000000000, 57.12835554495183032, 0.000000000000000000 ) ) ;
#49698 = EDGE_CURVE ( 'NONE', #13321, #73863, #70829, .T. ) ;
#49699 = CARTESIAN_POINT ( 'NONE',  ( -58.09773888555076837, -59.99999999999998579, 94.39131198705021575 ) ) ;
#49700 = CARTESIAN_POINT ( 'NONE',  ( 9.612665144396085992, -57.01130939352533744, 29.76292019730385618 ) ) ;
#49701 = CARTESIAN_POINT ( 'NONE',  ( -5.082755093536325042, -21.96875000204838457, -5.082755093536325930 ) ) ;
#49702 = CARTESIAN_POINT ( 'NONE',  ( 44.22093662635627709, 464.1457359768089077, 8.759819298992027825 ) ) ;
#49703 = CARTESIAN_POINT ( 'NONE',  ( -5.000000000000000888, -4.000000000000003553, 40.07669683062201926 ) ) ;
#49704 = CARTESIAN_POINT ( 'NONE',  ( -3.867509348774311739, 18.90767212923780249, -5.834931863125392582 ) ) ;
#49705 = DIRECTION ( 'NONE',  ( 0.000000000000000000, 0.000000000000000000, 1.000000000000000000 ) ) ;
#49706 = CARTESIAN_POINT ( 'NONE',  ( 0.000000000000000000, 0.1588408748199928722, 0.000000000000000000 ) ) ;
#49707 =( NAMED_UNIT ( * ) SI_UNIT ( $, .STERADIAN. ) SOLID_ANGLE_UNIT ( ) );
#49708 = CARTESIAN_POINT ( 'NONE',  ( -23.97799606807676298, 27.87796489320411197, 30.95132209396226486 ) ) ;
#49709 = LINE ( 'NONE', #77720, #91403 ) ;
#49710 = CARTESIAN_POINT ( 'NONE',  ( -32.48576253217986931, -32.55615044963190030, 32.82149560294217139 ) ) ;
#49711 = CARTESIAN_POINT ( 'NONE',  ( 8.572527594031473190E-16, -6.938893903907228378E-15, -7.000000000000000000 ) ) ;
#49712 = CARTESIAN_POINT ( 'NONE',  ( 40.33137201940245831, -18.77755698846380028, 34.22384520775455030 ) ) ;
#49713 = CIRCLE ( 'NONE', #39425, 8.000000000000000000 ) ;
#49714 = ORIENTED_EDGE ( 'NONE', *, *, #18724, .F. ) ;
#49715 = FACE_OUTER_BOUND ( 'NONE', #61863, .T. ) ;
#49716 = CARTESIAN_POINT ( 'NONE',  ( -78.45547098499037020, -38.62875648362158643, 189.5571983322416827 ) ) ;
#49717 = ORIENTED_EDGE ( 'NONE', *, *, #10775, .F. ) ;
#49719 = CARTESIAN_POINT ( 'NONE',  ( 39.84233570596349949, 333.3323931548420660, 19.23895789620553032 ) ) ;
#49718 = CARTESIAN_POINT ( 'NONE',  ( 7.770228158362351145, 1.340359594676612611E-15, 0.000000000000000000 ) ) ;
#49720 = CARTESIAN_POINT ( 'NONE',  ( 72.90321207859628316, -60.00000000000000711, 126.5507789543278108 ) ) ;
#49721 = CARTESIAN_POINT ( 'NONE',  ( 16.42611686831694939, 36.46285186709819470, 24.26654634025072355 ) ) ;
#49722 = FACE_OUTER_BOUND ( 'NONE', #13979, .T. ) ;
#49723 = AXIS2_PLACEMENT_3D ( 'NONE', #1038, #45148, #25939 ) ;
#49724 = CARTESIAN_POINT ( 'NONE',  ( 6.890281281981907924, 41.03680257675737408, -70.85895802599645776 ) ) ;
#49725 = DIRECTION ( 'NONE',  ( 0.5735764363510462704, 0.8191520442889915765, 0.000000000000000000 ) ) ;
#49726 = CARTESIAN_POINT ( 'NONE',  ( -31.44899729243502051, 391.8699891364225891, 24.19055939260229238 ) ) ;
#49727 = CARTESIAN_POINT ( 'NONE',  ( 28.86650669486618881, 4.898587196589413815E-16, -4.000000000000000888 ) ) ;
#49728 = CARTESIAN_POINT ( 'NONE',  ( 103.4784459831494559, -59.99999999999999289, 101.3822661864015231 ) ) ;
#49729 = CARTESIAN_POINT ( 'NONE',  ( 4.999999999999995559, -46.00000000000000000, 42.58845726811989607 ) ) ;
#49730 = EDGE_CURVE ( 'NONE', #101817, #84992, #87813, .T. ) ;
#49731 = CARTESIAN_POINT ( 'NONE',  ( -34.78087296571919751, 461.0374007115530617, 3.662433066614679156 ) ) ;
#49732 = ORIENTED_EDGE ( 'NONE', *, *, #85097, .F. ) ;
#49733 = EDGE_CURVE ( 'NONE', #47334, #76051, #5261, .T. ) ;
#49734 = CARTESIAN_POINT ( 'NONE',  ( -92.10385064345778972, -29.99999999999979039, 190.9054133797868928 ) ) ;
#49735 = EDGE_LOOP ( 'NONE', ( #18730, #12859, #47582, #11567, #84081 ) ) ;
#49736 = CARTESIAN_POINT ( 'NONE',  ( 5.354260712552314949, 36.72665595308956199, -54.26279534929282278 ) ) ;
#49737 = CARTESIAN_POINT ( 'NONE',  ( 7.869432500664373720, 87.30546385994320246, 5.000000000000000888 ) ) ;
#49738 = CARTESIAN_POINT ( 'NONE',  ( 32.13416664219985108, 374.4073344487368331, 24.05703695877565096 ) ) ;
#49739 = CARTESIAN_POINT ( 'NONE',  ( 9.698972129396510766, 26.82370287258062191, -2.445345647270328993 ) ) ;
#49740 = CARTESIAN_POINT ( 'NONE',  ( -1.320432766682874540E-15, -21.40625000204838457, 7.188101187500000044 ) ) ;
#49742 = ADVANCED_FACE ( 'NONE', ( #24438 ), #15236, .T. ) ;
#49741 = CARTESIAN_POINT ( 'NONE',  ( -3.857142857142850989, -1.200583151104938517, 103.1763305333244318 ) ) ;
#49743 = CARTESIAN_POINT ( 'NONE',  ( 6.941422757283499223, 41.41225026875491722, -70.44081393238894861 ) ) ;
#49744 = AXIS2_PLACEMENT_3D ( 'NONE', #32774, #65647, #57530 ) ;
#49745 = AXIS2_PLACEMENT_3D ( 'NONE', #64911, #23413, #32030 ) ;
#49746 = CONICAL_SURFACE ( 'NONE', #3255, 4.000000000000001776, 0.9599310885968774798 ) ;
#49748 = ORIENTED_EDGE ( 'NONE', *, *, #71487, .F. ) ;
#49747 = PRESENTATION_STYLE_ASSIGNMENT (( #8755 ) ) ;
#49749 = CARTESIAN_POINT ( 'NONE',  ( 81.76547146975626390, -29.09233618002616950, 145.4551964297468487 ) ) ;
#49750 = FILL_AREA_STYLE ('',( #91819 ) ) ;
#49751 =( NAMED_UNIT ( * ) PLANE_ANGLE_UNIT ( ) SI_UNIT ( $, .RADIAN. ) );
#49752 = ORIENTED_EDGE ( 'NONE', *, *, #38224, .T. ) ;
#49753 = DIRECTION ( 'NONE',  ( 0.000000000000000000, -1.000000000000000000, 0.000000000000000000 ) ) ;
#49754 = FACE_OUTER_BOUND ( 'NONE', #28970, .T. ) ;
#49755 = CARTESIAN_POINT ( 'NONE',  ( 38.66172427885771157, 27.30186337571333155, -12.83265428641589523 ) ) ;
#49756 = CARTESIAN_POINT ( 'NONE',  ( 7.896571385775229324, 26.21002000654247155, 1.305932416347440173 ) ) ;
#49757 = CARTESIAN_POINT ( 'NONE',  ( -59.00131487267276498, -60.00000000000000711, -29.97991402113869697 ) ) ;
#49758 = CARTESIAN_POINT ( 'NONE',  ( 10.28624191511840280, 46.12099395432375104, 12.90779740156148847 ) ) ;
#49759 = CARTESIAN_POINT ( 'NONE',  ( -33.97359119245066239, 434.1099241184709285, 11.80501937577158778 ) ) ;
#49760 = ORIENTED_EDGE ( 'NONE', *, *, #14359, .T. ) ;
#49761 = B_SPLINE_CURVE_WITH_KNOTS ( 'NONE', 3,
 ( #68670, #3921, #61101, #77808, #67065, #101550, #93470, #99946, #19620, #26119, #88553, #29295, #70775, #79913, #22250, #62181 ),
 .UNSPECIFIED., .F., .F.,
 ( 4, 2, 2, 2, 2, 2, 2, 4 ),
 ( 0.000000000000000000, 0.01751496934764543850, 0.03502993869529087700, 0.04378742336911359279, 0.05254490804293632245, 0.06130239271675903823, 0.06568113505367038918, 0.07005987739058174013 ),
 .UNSPECIFIED. ) ;
#49762 = VECTOR ( 'NONE', #42728, 1000.000000000000000 ) ;
#49763 = DIRECTION ( 'NONE',  ( -1.000000000000000000, -1.224606353822377258E-16, -0.000000000000000000 ) ) ;
#49764 = CLOSED_SHELL ( 'NONE', ( #90473, #51356, #43134, #53837, #62095, #15031, #29072, #92333, #21281, #35622, #20165, #63755, #24749, #9030, #59048, #88275, #84085, #22551, #32687, #87467, #57307, #58251, #13666, #99986, #294, #15981, #72054, #56899, #105596, #33418, #34323, #24828, #16090, #65779, #50507, #48794, #101128, #62036, #62029, #88989, #104789, #22472, #103125, #102191, #59938, #88677, #23143, #70074, #83493, #68560, #25636, #54358, #32235, #19126, #101514, #92267, #32056, #99909, #106523, #36729, #17273, #104955, #102932, #19443, #7207, #73745, #65843, #2927, #85640, #11011, #15334, #10793, #71726, #82791, #33014, #47180, #58021, #26118, #58664, #7675, #81324, #40893, #669, #18149, #11487, #86398, #96655, #66769, #50872, #92599, #26303, #16408, #40572, #92721, #69230, #92335, #87883, #79701, #61354, #86532, #79726, #76459, #81664, #14193, #68623, #34075, #78793, #7947, #3243, #104801, #42514, #13023, #67967, #56187, #43983, #23331, #49458, #49316, #52676, #70744, #52029, #51534, #25085, #53850, #14698, #83289, #32777, #79909, #19805, #13643, #92190, #62340, #62358, #11484, #37707, #97543, #49742 ) ) ;
#49765 = CARTESIAN_POINT ( 'NONE',  ( 38.12216208879490864, 18.64284798592648329, -4.860317469366568055 ) ) ;
#49766 = CARTESIAN_POINT ( 'NONE',  ( 86.75287041639032282, -24.36799545327036043, 185.3761312858067640 ) ) ;
#49767 = DIRECTION ( 'NONE',  ( -0.000000000000000000, 1.000000000000000000, -0.000000000000000000 ) ) ;
#49768 = EDGE_CURVE ( 'NONE', #89019, #78525, #105744, .T. ) ;
#49769 = CARTESIAN_POINT ( 'NONE',  ( -7.188101187500001821, -30.50000000204838813, -2.977408999572651371 ) ) ;
#49770 = CARTESIAN_POINT ( 'NONE',  ( 21.50886870662808903, -26.69092517108576956, 37.20578707323234369 ) ) ;
#49771 = CARTESIAN_POINT ( 'NONE',  ( -38.42841492633962730, 491.4186471570457115, 12.30549038569188269 ) ) ;
#49772 = LINE ( 'NONE', #9299, #74036 ) ;
#49773 = EDGE_CURVE ( 'NONE', #36517, #13469, #61031, .T. ) ;
#49774 = CARTESIAN_POINT ( 'NONE',  ( 39.46660235664349159, 438.4151231452425463, 22.74768781139262330 ) ) ;
#49775 = CARTESIAN_POINT ( 'NONE',  ( 49.02741474918247633, 7.901513937033938895, 16.35941288907570623 ) ) ;
#49776 = ORIENTED_EDGE ( 'NONE', *, *, #61176, .F. ) ;
#49777 = CARTESIAN_POINT ( 'NONE',  ( -36.16847030042355016, 438.2414514106959018, 3.889105687734305317 ) ) ;
#49778 = CARTESIAN_POINT ( 'NONE',  ( 0.000000000000000000, 0.000000000000000000, 4.000000000000000000 ) ) ;
#49779 = ADVANCED_FACE ( 'NONE', ( #92303 ), #49543, .F. ) ;
#49780 = DIRECTION ( 'NONE',  ( -0.6175266994149452016, -0.6213472858387197872, -0.4822741190345386508 ) ) ;
#49781 = VERTEX_POINT ( 'NONE', #19542 ) ;
#49782 = CARTESIAN_POINT ( 'NONE',  ( -8.559508646656381003, 51.83514083332404709, -1.531152949374265049 ) ) ;
#49783 = CARTESIAN_POINT ( 'NONE',  ( -43.03357534758841041, 463.2291678140047679, 4.675918524149428990 ) ) ;
#49784 = CARTESIAN_POINT ( 'NONE',  ( 112.0245006668171186, -57.67108255664081184, 191.2454414640604625 ) ) ;
#49785 = CIRCLE ( 'NONE', #11911, 15.80007993603364724 ) ;
#49786 = CARTESIAN_POINT ( 'NONE',  ( 37.13212445136079509, 463.5388707510517747, 19.67708231430621879 ) ) ;
#49787 = DIRECTION ( 'NONE',  ( 0.000000000000000000, -0.8660254037844383745, -0.5000000000000004441 ) ) ;
#49788 = CARTESIAN_POINT ( 'NONE',  ( -2.850063997753378597, -5.000000000000000000, -72.23558523188754066 ) ) ;
#49789 = CARTESIAN_POINT ( 'NONE',  ( -89.99999999999997158, -60.00000000000000000, 188.5238439516623146 ) ) ;
#49790 = CARTESIAN_POINT ( 'NONE',  ( -80.97052878467144410, -60.00000000000000711, 197.1200735740363257 ) ) ;
#49791 = CIRCLE ( 'NONE', #89222, 12.00000000000000000 ) ;
#49792 =( GEOMETRIC_REPRESENTATION_CONTEXT ( 3 ) GLOBAL_UNCERTAINTY_ASSIGNED_CONTEXT ( ( #95211 ) ) GLOBAL_UNIT_ASSIGNED_CONTEXT ( ( #21106, #44822, #3819 ) ) REPRESENTATION_CONTEXT ( 'NONE', 'WORKASPACE' ) );
#49793 = CARTESIAN_POINT ( 'NONE',  ( -3.220999722221654600E-16, 7.895640089090876224, -6.564402953523721607 ) ) ;
#49794 = CARTESIAN_POINT ( 'NONE',  ( -62.91825180719953892, 50.00000000000000000, 6.605622457240398759 ) ) ;
#49795 = CARTESIAN_POINT ( 'NONE',  ( -85.48315206928592147, -35.70362574039081238, 183.4287206597788895 ) ) ;
#49796 = ORIENTED_EDGE ( 'NONE', *, *, #53898, .F. ) ;
#49797 = CARTESIAN_POINT ( 'NONE',  ( 28.20173342337447409, 307.2982505937521864, -9.226824045861857115 ) ) ;
#49798 = VERTEX_POINT ( 'NONE', #52921 ) ;
#49799 = CARTESIAN_POINT ( 'NONE',  ( -7.618844049274132502, -13.17235898929460802, 2.450177051822845620 ) ) ;
#49800 = EDGE_CURVE ( 'NONE', #54339, #60761, #77554, .T. ) ;
#49801 = PRESENTATION_STYLE_ASSIGNMENT (( #58437 ) ) ;
#49802 = CARTESIAN_POINT ( 'NONE',  ( -85.63635423108523526, -52.74933567132664791, -9.611642272926120611 ) ) ;
#49803 = AXIS2_PLACEMENT_3D ( 'NONE', #12787, #20427, #95322 ) ;
#49804 = CARTESIAN_POINT ( 'NONE',  ( -4.805888432417104283, -14.59013712844724786, -7.778733730875007524 ) ) ;
#49805 = CARTESIAN_POINT ( 'NONE',  ( -4.403431911294753753, 10.10497258083900363, -5.000000000000000000 ) ) ;
#49806 = LINE ( 'NONE', #91351, #106698 ) ;
#49807 =( NAMED_UNIT ( * ) PLANE_ANGLE_UNIT ( ) SI_UNIT ( $, .RADIAN. ) );
#49808 = CARTESIAN_POINT ( 'NONE',  ( 6.991644890290505288, 41.20407774039003357, -58.47941669199799009 ) ) ;
#49809 = EDGE_CURVE ( 'NONE', #55752, #32781, #92842, .T. ) ;
#49810 = CARTESIAN_POINT ( 'NONE',  ( -2.399209547574901823E-15, 57.18445727710329862, 19.59103268995865221 ) ) ;
#49811 = COLOUR_RGB ( '', 0.08235294, 0.09019608, 0.10196078) ;
#49812 = CARTESIAN_POINT ( 'NONE',  ( -36.74148664940361186, 437.9559008978175143, 4.252305828303462043 ) ) ;
#49813 = CARTESIAN_POINT ( 'NONE',  ( 16.35077622672217146, -14.21045842199431064, -36.83539407110947650 ) ) ;
#49814 = CARTESIAN_POINT ( 'NONE',  ( -78.75458884624195832, -29.08646686470842369, 129.2280381913504357 ) ) ;
#49815 = ORIENTED_EDGE ( 'NONE', *, *, #100102, .F. ) ;
#49816 = CARTESIAN_POINT ( 'NONE',  ( 71.37437158690347871, -14.21045842199427156, 121.5198118854055451 ) ) ;
#49817 = CARTESIAN_POINT ( 'NONE',  ( 7.934996450857311423, 88.86862456472529459, -1.050865690281773901 ) ) ;
#49818 = CARTESIAN_POINT ( 'NONE',  ( 114.2239807911121829, -57.67113939738325712, 171.8931019229777064 ) ) ;
#49819 = EDGE_LOOP ( 'NONE', ( #48067, #24038, #87975, #99834, #24163 ) ) ;
#49820 = DIRECTION ( 'NONE',  ( -1.000000000000000000, -1.224606353822377258E-16, -0.000000000000000000 ) ) ;
#49821 = MECHANICAL_DESIGN_GEOMETRIC_PRESENTATION_REPRESENTATION (  '', ( #96353 ), #103200 ) ;
#49822 = CARTESIAN_POINT ( 'NONE',  ( 9.349999999999997868, 1.533819458162526451E-15, 0.000000000000000000 ) ) ;
#49823 = ORIENTED_EDGE ( 'NONE', *, *, #51335, .F. ) ;
#49824 = EDGE_CURVE ( 'NONE', #63286, #4234, #94817, .T. ) ;
#49825 = CARTESIAN_POINT ( 'NONE',  ( -12.50000000000000000, -3.000000000000003109, -14.34180675897363599 ) ) ;
#49826 = CARTESIAN_POINT ( 'NONE',  ( 1.347111479062088207E-15, -50.00000000000000000, 100.9999999999999858 ) ) ;
#49827 = CARTESIAN_POINT ( 'NONE',  ( -5.082755093536326818, -10.71875000204838457, 5.082755093536325042 ) ) ;
#49828 = CARTESIAN_POINT ( 'NONE',  ( 6.439685834476087223, -4.942299687812549358, -7.659344964962875757 ) ) ;
#49829 =( LENGTH_UNIT ( ) NAMED_UNIT ( * ) SI_UNIT ( .MILLI., .METRE. ) );
#49830 = CARTESIAN_POINT ( 'NONE',  ( 7.898269865231975828, 11.02838903529590908, -12.97150009825809924 ) ) ;
#49831 = DIRECTION ( 'NONE',  ( 1.000000000000000000, 0.000000000000000000, 0.000000000000000000 ) ) ;
#49832 = DIRECTION ( 'NONE',  ( -0.000000000000000000, -1.000000000000000000, -0.000000000000000000 ) ) ;
#49833 = ORIENTED_EDGE ( 'NONE', *, *, #68108, .F. ) ;
#49834 = CARTESIAN_POINT ( 'NONE',  ( -7.278899862585794800, 40.56071481047660399, -70.70219261697603486 ) ) ;
#49836 = CARTESIAN_POINT ( 'NONE',  ( 27.77284297229067178, -22.10363696659563360, 29.38272422889403401 ) ) ;
#49835 = PRESENTATION_STYLE_ASSIGNMENT (( #50358 ) ) ;
#49837 = CARTESIAN_POINT ( 'NONE',  ( 20.21880305278369150, 304.8280059657581660, -9.005058168222337400 ) ) ;
#49838 = VERTEX_POINT ( 'NONE', #76654 ) ;
#49839 = CARTESIAN_POINT ( 'NONE',  ( -1.168166114424086244, 14.76304312983176104, 50.96139025757861418 ) ) ;
#49840 = COLOUR_RGB ( '', 0.09019608, 0.27058824, 0.51372549) ;
#49841 = ORIENTED_EDGE ( 'NONE', *, *, #82355, .F. ) ;
#49843 = CARTESIAN_POINT ( 'NONE',  ( 0.000000000000000000, -5.000000000000000000, 10.00000000000000000 ) ) ;
#49842 = DIRECTION ( 'NONE',  ( -1.000000000000000000, -1.224606353822377258E-16, -0.000000000000000000 ) ) ;
#49844 = CARTESIAN_POINT ( 'NONE',  ( -2.500000000000001776, -30.00000000000000000, 30.00000000000000000 ) ) ;
#49845 = CARTESIAN_POINT ( 'NONE',  ( -16.26028350797723832, 302.5670365178829684, -10.06049214740963293 ) ) ;
#49846 = CARTESIAN_POINT ( 'NONE',  ( -33.74271564777242816, 484.1802673187708592, 2.058285076122308155 ) ) ;
#49847 = CARTESIAN_POINT ( 'NONE',  ( 1.944839216437187431E-15, 45.30391365246044444, 18.75000000000001066 ) ) ;
#49848 = CARTESIAN_POINT ( 'NONE',  ( -35.51382444471699529, 463.4141161792284720, 19.91564417027156253 ) ) ;
#49849 = ORIENTED_EDGE ( 'NONE', *, *, #3927, .T. ) ;
#49850 =( GEOMETRIC_REPRESENTATION_CONTEXT ( 3 ) GLOBAL_UNCERTAINTY_ASSIGNED_CONTEXT ( ( #67742 ) ) GLOBAL_UNIT_ASSIGNED_CONTEXT ( ( #44110, #67848, #60315 ) ) REPRESENTATION_CONTEXT ( 'NONE', 'WORKASPACE' ) );
#49851 = CARTESIAN_POINT ( 'NONE',  ( 92.40875900179753444, -60.00000000000000711, -11.92294509418752213 ) ) ;
#49852 = CARTESIAN_POINT ( 'NONE',  ( -10.92801675053744148, 45.30201443972634934, -15.24347305256524088 ) ) ;
#49853 = CARTESIAN_POINT ( 'NONE',  ( 30.00000000000000355, 461.9652624853973748, 12.11314247086045803 ) ) ;
#49854 = SURFACE_STYLE_FILL_AREA ( #97339 ) ;
#49855 = DIRECTION ( 'NONE',  ( 1.000000000000000000, 0.000000000000000000, 0.000000000000000000 ) ) ;
#49856 = ORIENTED_EDGE ( 'NONE', *, *, #83486, .T. ) ;
#49857 = EDGE_CURVE ( 'NONE', #40596, #71589, #1765, .T. ) ;
#49858 = CARTESIAN_POINT ( 'NONE',  ( -36.32210038707830790, 28.19822729005272421, 12.06285977509587859 ) ) ;
#49859 = ORIENTED_EDGE ( 'NONE', *, *, #57291, .T. ) ;
#49860 = VERTEX_POINT ( 'NONE', #85289 ) ;
#49861 = CARTESIAN_POINT ( 'NONE',  ( 7.212408192734267587, 82.98482910679631175, -3.465038817813880456 ) ) ;
#49862 = CARTESIAN_POINT ( 'NONE',  ( 6.333820801331254913, -4.275724398228172518, -5.594228103109054828 ) ) ;
#49863 = CARTESIAN_POINT ( 'NONE',  ( 0.5805565836007602343, 3.752776749732561257, -6.499999999999999112 ) ) ;
#49864 = DIRECTION ( 'NONE',  ( 0.000000000000000000, -1.000000000000000000, 0.000000000000000000 ) ) ;
#49865 = CARTESIAN_POINT ( 'NONE',  ( 83.06461413968138174, -37.84181084904789572, -1.854778334287288999 ) ) ;
#49866 = CARTESIAN_POINT ( 'NONE',  ( -42.43985862560405309, 333.9176701535965890, 7.447030561597399512 ) ) ;
#49867 = CARTESIAN_POINT ( 'NONE',  ( -3.757130767675045835, -69.58003094729899374, 13.51214695925444609 ) ) ;
#49869 = EDGE_CURVE ( 'NONE', #66555, #104368, #53037, .T. ) ;
#49868 = CARTESIAN_POINT ( 'NONE',  ( 12.50000000000000355, 27.89883036488820167, -45.48774139817316353 ) ) ;
#49870 = ORIENTED_EDGE ( 'NONE', *, *, #81900, .T. ) ;
#49871 = CARTESIAN_POINT ( 'NONE',  ( 30.93386089603002986, 8.839832930400802979, 40.91297150549235084 ) ) ;
#49872 = ORIENTED_EDGE ( 'NONE', *, *, #101208, .T. ) ;
#49873 = DIRECTION ( 'NONE',  ( 1.776356839400250465E-15, 0.000000000000000000, 1.000000000000000000 ) ) ;
#49874 = CARTESIAN_POINT ( 'NONE',  ( -91.97836648421129269, -38.50002395389604715, 200.9810570860146299 ) ) ;
#49875 = CARTESIAN_POINT ( 'NONE',  ( 4.334722950428502308, -48.88070975476235702, 104.3859289939585864 ) ) ;
#49876 = AXIS2_PLACEMENT_3D ( 'NONE', #18331, #68464, #9662 ) ;
#49878 = ORIENTED_EDGE ( 'NONE', *, *, #58949, .F. ) ;
#49877 = CARTESIAN_POINT ( 'NONE',  ( -78.44352337963121613, -59.99999999999999289, 159.1831049015135875 ) ) ;
#49879 = CARTESIAN_POINT ( 'NONE',  ( 64.80880146042169088, -32.53003655438431707, 82.02282776973038381 ) ) ;
#49880 = ORIENTED_EDGE ( 'NONE', *, *, #23809, .T. ) ;
#49881 = CARTESIAN_POINT ( 'NONE',  ( -16.51907061138353683, 42.00139744608745218, -87.79003255390433935 ) ) ;
#49882 = CARTESIAN_POINT ( 'NONE',  ( -5.082755093536326818, -28.71875000204838813, 5.082755093536325042 ) ) ;
#49883 =( BOUNDED_SURFACE ( )  B_SPLINE_SURFACE ( 2, 3, ( 
 ( #87841, #52803, #46834, #85729 ),
 ( #11801, #44733, #102425, #94345 ),
 ( #20507, #24713, #82387, #16593 ) ),
 .UNSPECIFIED., .F., .F., .F. ) 
 B_SPLINE_SURFACE_WITH_KNOTS ( ( 3, 3 ),
 ( 4, 4 ),
 ( 0.000000000000000000, 1.000000000000000000 ),
 ( -0.02264331519860533423, -0.01818793032683159450 ),
 .UNSPECIFIED. ) 
 GEOMETRIC_REPRESENTATION_ITEM ( )  RATIONAL_B_SPLINE_SURFACE ( (
 ( 1.000000000000000000, 1.000000000000000000, 1.000000000000000000, 1.000000000000000000),
 ( 1.857142857142858317, 1.857142857142858317, 1.857142857142858317, 1.857142857142858317),
 ( 1.000000000000000000, 1.000000000000000000, 1.000000000000000000, 1.000000000000000000) ) ) 
 REPRESENTATION_ITEM ( '' )  SURFACE ( )  );
#49884 = CARTESIAN_POINT ( 'NONE',  ( -92.43439519788523739, -57.65869811958181401, -18.51275992931142156 ) ) ;
#49885 = ADVANCED_FACE ( 'NONE', ( #14034 ), #6086, .F. ) ;
#49886 = EDGE_LOOP ( 'NONE', ( #11600, #13752, #45862, #76180, #17247, #94051 ) ) ;
#49887 = CARTESIAN_POINT ( 'NONE',  ( -37.50843646915485152, 482.0142436422872834, 15.15300368821568000 ) ) ;
#49888 = CIRCLE ( 'NONE', #63704, 7.500000000000000888 ) ;
#49889 = CARTESIAN_POINT ( 'NONE',  ( -37.38602481899999219, 490.8442832704672014, 12.40593855172241611 ) ) ;
#49890 = FACE_OUTER_BOUND ( 'NONE', #89924, .T. ) ;
#49891 = CARTESIAN_POINT ( 'NONE',  ( 8.000000000000000000, -24.59375000409677270, -3.313708498984761608 ) ) ;
#49892 = CARTESIAN_POINT ( 'NONE',  ( 13.69330508143927538, 1.340359594676612611E-15, 0.000000000000000000 ) ) ;
#49893 = CARTESIAN_POINT ( 'NONE',  ( 33.21459943997680853, 487.8270262909274493, 10.08789160141814278 ) ) ;
#49894 = CARTESIAN_POINT ( 'NONE',  ( -7.493944919676032157, 40.57567429012536309, -59.86116873889386625 ) ) ;
#49895 = CARTESIAN_POINT ( 'NONE',  ( 9.253500431420430772, 31.29771549917707674, 3.792688295761954098 ) ) ;
#49896 = CARTESIAN_POINT ( 'NONE',  ( -16.96954359408614366, 304.5683848806726814, 9.876757081930351845 ) ) ;
#49897 = DIRECTION ( 'NONE',  ( 0.000000000000000000, 0.000000000000000000, 1.000000000000000000 ) ) ;
#49898 = CARTESIAN_POINT ( 'NONE',  ( -0.6976587266869073156, -30.00000000000001066, -7.793936262885737598 ) ) ;
#49899 = VERTEX_POINT ( 'NONE', #13504 ) ;
#49900 = CARTESIAN_POINT ( 'NONE',  ( 4.999999999999998224, -5.773502691896267969, -7.063244554130005071 ) ) ;
#49901 = LINE ( 'NONE', #25683, #6044 ) ;
#49902 = CARTESIAN_POINT ( 'NONE',  ( 4.356282367766563191, -60.00000000000000711, 39.63058553034037601 ) ) ;
#49903 = CARTESIAN_POINT ( 'NONE',  ( -90.94143197032809667, -30.00000000000000355, 190.4644691013067472 ) ) ;
#49904 = EDGE_CURVE ( 'NONE', #90401, #54423, #62110, .T. ) ;
#49905 = AXIS2_PLACEMENT_3D ( 'NONE', #94635, #68766, #93561 ) ;
#49906 = CARTESIAN_POINT ( 'NONE',  ( 38.77611916830803551, 25.24244599302587844, -11.84947842017332320 ) ) ;
#49907 = CARTESIAN_POINT ( 'NONE',  ( 70.45866099340145183, -57.68246761816307355, 157.7518986473937161 ) ) ;
#49909 = DIRECTION ( 'NONE',  ( -0.000000000000000000, 1.000000000000000000, -0.000000000000000000 ) ) ;
#49908 = CARTESIAN_POINT ( 'NONE',  ( 14.91858118607497374, 2.271260765197548532E-16, 15.00000000000000000 ) ) ;
#49911 = CARTESIAN_POINT ( 'NONE',  ( 23.84453580884438395, -27.27310615191336396, -38.40431109410636168 ) ) ;
#49910 = VECTOR ( 'NONE', #42138, 1000.000000000000000 ) ;
#49912 = FACE_OUTER_BOUND ( 'NONE', #59250, .T. ) ;
#49913 = CARTESIAN_POINT ( 'NONE',  ( 0.000000000000000000, 0.000000000000000000, 0.000000000000000000 ) ) ;
#49914 = CARTESIAN_POINT ( 'NONE',  ( -38.97755016977858844, -60.00000000000000000, 50.71592569719196320 ) ) ;
#49915 = CARTESIAN_POINT ( 'NONE',  ( 11.41228817278395091, 13.87733114462658257, 9.968491662189933322 ) ) ;
#49916 = AXIS2_PLACEMENT_3D ( 'NONE', #1363, #93061, #67725 ) ;
#49917 = CARTESIAN_POINT ( 'NONE',  ( 0.000000000000000000, 0.000000000000000000, -3.393184225085859929 ) ) ;
#49918 = CARTESIAN_POINT ( 'NONE',  ( -86.89680602446821922, -28.03361883784057795, 186.5272980465382489 ) ) ;
#49919 = ORIENTED_EDGE ( 'NONE', *, *, #29410, .F. ) ;
#49920 = CARTESIAN_POINT ( 'NONE',  ( 19.31075363035184012, 49.87050359945839517, 61.31541196677274996 ) ) ;
#49921 = CARTESIAN_POINT ( 'NONE',  ( -0.9999999999999943379, -50.00000000000000000, 101.0455488498966758 ) ) ;
#49922 = CARTESIAN_POINT ( 'NONE',  ( -7.997530052830874148, -18.58626440210924002, 26.97989019616458961 ) ) ;
#49923 = SURFACE_STYLE_FILL_AREA ( #43444 ) ;
#49924 = CARTESIAN_POINT ( 'NONE',  ( 24.63846153846153797, 1.411358822780289120E-15, 0.000000000000000000 ) ) ;
#49926 = CARTESIAN_POINT ( 'NONE',  ( 6.075632316336291971, -62.90659182483985745, 14.38622881700373490 ) ) ;
#49925 = DIRECTION ( 'NONE',  ( 0.000000000000000000, 1.000000000000000000, 0.000000000000000000 ) ) ;
#49927 = EDGE_CURVE ( 'NONE', #103221, #11237, #71599, .T. ) ;
#49928 = ORIENTED_EDGE ( 'NONE', *, *, #58682, .T. ) ;
#49929 =( NAMED_UNIT ( * ) PLANE_ANGLE_UNIT ( ) SI_UNIT ( $, .RADIAN. ) );
#49930 = CARTESIAN_POINT ( 'NONE',  ( -6.904524730080175310, -4.999999999998975930, -16.27804637755029304 ) ) ;
#49931 = CARTESIAN_POINT ( 'NONE',  ( -7.896165657598945842, 33.78911131371973653, -1.307894402814547385 ) ) ;
#49932 = AXIS2_PLACEMENT_3D ( 'NONE', #50299, #83202, #99915 ) ;
#49933 = CARTESIAN_POINT ( 'NONE',  ( 35.18962234169666203, 301.6382339994959239, -8.468528340524796860 ) ) ;
#49934 = DIRECTION ( 'NONE',  ( -1.000000000000000000, -0.000000000000000000, -0.000000000000000000 ) ) ;
#49935 = EDGE_CURVE ( 'NONE', #22614, #32012, #44065, .T. ) ;
#49936 = CARTESIAN_POINT ( 'NONE',  ( -7.003653396366579464, -83.94293794440324064, -3.866846144092870308 ) ) ;
#49937 = DIRECTION ( 'NONE',  ( -1.000000000000000000, -0.000000000000000000, -0.000000000000000000 ) ) ;
#49938 = CARTESIAN_POINT ( 'NONE',  ( 113.8520663817495233, -59.99999999999995026, 157.1483003829898450 ) ) ;
#49939 = FACE_BOUND ( 'NONE', #77657, .T. ) ;
#49940 = ORIENTED_EDGE ( 'NONE', *, *, #78143, .T. ) ;
#49941 = LINE ( 'NONE', #21869, #56728 ) ;
#49942 = CARTESIAN_POINT ( 'NONE',  ( -9.165151389911704527, 250.2629551091633573, 4.000000000000000888 ) ) ;
#49943 = CARTESIAN_POINT ( 'NONE',  ( 4.744389013293893065, -1.372925465831636327, 104.3204960233004357 ) ) ;
#49944 = CARTESIAN_POINT ( 'NONE',  ( 43.58191376438443143, 439.3922052527890401, 13.97025970319826982 ) ) ;
#49945 = DIRECTION ( 'NONE',  ( 0.000000000000000000, 0.000000000000000000, 1.000000000000000000 ) ) ;
#49946 = ORIENTED_EDGE ( 'NONE', *, *, #55813, .T. ) ;
#49947 = EDGE_CURVE ( 'NONE', #39480, #56970, #70989, .T. ) ;
#49948 = CARTESIAN_POINT ( 'NONE',  ( -23.65461719027016230, 304.8910927077299107, 10.16394219231294294 ) ) ;
#49949 = ORIENTED_EDGE ( 'NONE', *, *, #5622, .T. ) ;
#49950 = CARTESIAN_POINT ( 'NONE',  ( 34.40251038080555190, 484.1263118519839850, 0.1376245346420501836 ) ) ;
#49951 = FACE_OUTER_BOUND ( 'NONE', #36556, .T. ) ;
#49952 = CARTESIAN_POINT ( 'NONE',  ( 32.62376965138175677, 486.1221409277114276, 7.511474791660580408 ) ) ;
#49953 = CARTESIAN_POINT ( 'NONE',  ( -51.78317192862404994, 48.00000000000000000, 39.73656039225668479 ) ) ;
#49954 = CARTESIAN_POINT ( 'NONE',  ( 5.000000000000000000, -14.73708290046165281, 12.39211607765093426 ) ) ;
#49955 = TOROIDAL_SURFACE ( 'NONE', #22446, 13.99700487351915612, 1.000000000000000000 ) ;
#49956 = CARTESIAN_POINT ( 'NONE',  ( -67.57337042125921300, -59.99999999999997868, 141.1407361875824051 ) ) ;
#49957 = B_SPLINE_CURVE_WITH_KNOTS ( 'NONE', 3,
 ( #75259, #98477, #41840, #7869, #106029, #67200, #24629, #8408 ),
 .UNSPECIFIED., .F., .F.,
 ( 4, 2, 2, 4 ),
 ( 0.000000000000000000, 0.5000000000000000000, 0.7500000000000000000, 1.000000000000000000 ),
 .UNSPECIFIED. ) ;
#49958 = CARTESIAN_POINT ( 'NONE',  ( 46.00000000000000000, 438.3644743593593489, 10.24495404210296989 ) ) ;
#49959 = ORIENTED_EDGE ( 'NONE', *, *, #50775, .F. ) ;
#49960 = CARTESIAN_POINT ( 'NONE',  ( 101.0978150197463492, -59.99999999999998579, 201.5160938181417407 ) ) ;
#49962 = CARTESIAN_POINT ( 'NONE',  ( 14.28806202503381684, -22.06801482742367071, 27.67556484836572039 ) ) ;
#49961 = CARTESIAN_POINT ( 'NONE',  ( -77.87378252178784521, -14.21045842199420228, 157.7502635463301317 ) ) ;
#49964 = SURFACE_STYLE_FILL_AREA ( #33815 ) ;
#49963 = UNCERTAINTY_MEASURE_WITH_UNIT (LENGTH_MEASURE( 1.000000000000000082E-05 ), #69815, 'distance_accuracy_value', 'NONE');
#49965 = CARTESIAN_POINT ( 'NONE',  ( 0.000000000000000000, 4.898587196589413815E-16, -4.000000000000000888 ) ) ;
#49966 = CIRCLE ( 'NONE', #77539, 4.000000000000001776 ) ;
#49967 = CARTESIAN_POINT ( 'NONE',  ( -42.62392613728367508, -25.70309449447480432, 37.69303809212602374 ) ) ;
#49968 = DIRECTION ( 'NONE',  ( 0.000000000000000000, 0.000000000000000000, 1.000000000000000000 ) ) ;
#49969 = VERTEX_POINT ( 'NONE', #104648 ) ;
#49970 = CARTESIAN_POINT ( 'NONE',  ( 26.08349330513380693, 1.593028355512270962E-15, 0.000000000000000000 ) ) ;
#49971 = CARTESIAN_POINT ( 'NONE',  ( 6.125000000000095923, -15.62228920881129390, 14.41094225130415651 ) ) ;
#49972 = FACE_OUTER_BOUND ( 'NONE', #104548, .T. ) ;
#49973 = CARTESIAN_POINT ( 'NONE',  ( 16.94034599462699830, 304.5648770741773887, -9.060986067200369476 ) ) ;
#49974 = CARTESIAN_POINT ( 'NONE',  ( -32.13503062639005492, 486.0946171966414795, 5.282847667695663496 ) ) ;
#49975 = VERTEX_POINT ( 'NONE', #22708 ) ;
#49976 = CARTESIAN_POINT ( 'NONE',  ( 5.000000000093224095, -46.22753318115157128, 103.2791840072271015 ) ) ;
#49977 = DIRECTION ( 'NONE',  ( 0.000000000000000000, -1.000000000000000000, 0.000000000000000000 ) ) ;
#49978 = ORIENTED_EDGE ( 'NONE', *, *, #65428, .F. ) ;
#49979 = CARTESIAN_POINT ( 'NONE',  ( 78.63367630571566735, -29.99999999999999289, -15.31311550526425691 ) ) ;
#49980 = CARTESIAN_POINT ( 'NONE',  ( 19.39114753129161173, 41.87392969580012902, -80.53546452172405168 ) ) ;
#49982 = CARTESIAN_POINT ( 'NONE',  ( 24.23033468520214484, 25.18874691648631270, -32.69349562522533859 ) ) ;
#49981 = AXIS2_PLACEMENT_3D ( 'NONE', #84571, #12251, #36053 ) ;
#49983 = CARTESIAN_POINT ( 'NONE',  ( 0.000000000000000000, 79.50000000000000000, 0.000000000000000000 ) ) ;
#49984 = CARTESIAN_POINT ( 'NONE',  ( 83.29267879008702380, -30.00000000000001421, 45.23466661269899447 ) ) ;
#49985 = DIRECTION ( 'NONE',  ( 1.000000000000000000, -0.000000000000000000, -0.000000000000000000 ) ) ;
#49986 = ORIENTED_EDGE ( 'NONE', *, *, #85143, .T. ) ;
#49987 = ADVANCED_FACE ( 'NONE', ( #47466 ), #62104, .F. ) ;
#49988 = AXIS2_PLACEMENT_3D ( 'NONE', #38273, #87862, #71132 ) ;
#49989 = ORIENTED_EDGE ( 'NONE', *, *, #68521, .F. ) ;
#49990 = ORIENTED_EDGE ( 'NONE', *, *, #8935, .F. ) ;
#49991 = DIRECTION ( 'NONE',  ( 0.5735764363510468256, 0.8191520442889913545, 0.000000000000000000 ) ) ;
#49992 = CARTESIAN_POINT ( 'NONE',  ( -6.138854265193438131, -12.09086120632721872, -8.896243454972955433 ) ) ;
#49993 = CARTESIAN_POINT ( 'NONE',  ( -19.45221650979668837, 49.97868703238423649, 60.60569223047880172 ) ) ;
#49994 = CARTESIAN_POINT ( 'NONE',  ( -42.09158233638503788, 465.7816406625424861, 14.79318349169994562 ) ) ;
#49995 = EDGE_CURVE ( 'NONE', #45750, #31200, #66724, .T. ) ;
#49996 = CARTESIAN_POINT ( 'NONE',  ( -31.44885420705449164, 398.4269215821768171, 24.43068901296845752 ) ) ;
#49998 = ADVANCED_FACE ( 'NONE', ( #99063, #59174 ), #25229, .F. ) ;
#49997 = DIRECTION ( 'NONE',  ( 0.000000000000000000, -1.000000000000000000, 0.000000000000000000 ) ) ;
#49999 = ORIENTED_EDGE ( 'NONE', *, *, #31655, .F. ) ;
#50000 = CARTESIAN_POINT ( 'NONE',  ( 9.482945380845297478, 107.4433305877892764, 3.177595346755246464 ) ) ;
#50001 = CIRCLE ( 'NONE', #91356, 5.000000000000011546 ) ;
#50002 = VERTEX_POINT ( 'NONE', #100146 ) ;
#50003 = SURFACE_STYLE_FILL_AREA ( #17125 ) ;
#50004 = CARTESIAN_POINT ( 'NONE',  ( 81.77512476957420517, -38.84160798149201810, 195.6174134348494533 ) ) ;
#50005 = CARTESIAN_POINT ( 'NONE',  ( 33.84761347220318584, 488.7471039746334895, 11.01988148152525504 ) ) ;
#50006 = CARTESIAN_POINT ( 'NONE',  ( 35.50538377702518744, 304.0193673134525056, 4.053817158089760397 ) ) ;
#50007 =( NAMED_UNIT ( * ) SI_UNIT ( $, .STERADIAN. ) SOLID_ANGLE_UNIT ( ) );
#50008 =( GEOMETRIC_REPRESENTATION_CONTEXT ( 3 ) GLOBAL_UNCERTAINTY_ASSIGNED_CONTEXT ( ( #93618 ) ) GLOBAL_UNIT_ASSIGNED_CONTEXT ( ( #68278, #18145, #36487 ) ) REPRESENTATION_CONTEXT ( 'NONE', 'WORKASPACE' ) );
#50009 = CARTESIAN_POINT ( 'NONE',  ( -40.76154164607882535, 460.9888869747143758, 2.282783108351643886 ) ) ;
#50010 = CARTESIAN_POINT ( 'NONE',  ( 42.59003199992548616, 362.8236097783378682, 16.78898391992328243 ) ) ;
#50011 = FACE_OUTER_BOUND ( 'NONE', #6992, .T. ) ;
#50012 = EDGE_CURVE ( 'NONE', #8869, #73621, #24306, .T. ) ;
#50013 = CARTESIAN_POINT ( 'NONE',  ( 31.84999999999999787, 3.309500000000003439, 0.000000000000000000 ) ) ;
#50014 = ORIENTED_EDGE ( 'NONE', *, *, #21402, .T. ) ;
#50015 = CARTESIAN_POINT ( 'NONE',  ( -21.31378532129378556, 303.0151486721171636, 9.972274757840462911 ) ) ;
#50016 = DIRECTION ( 'NONE',  ( -0.1659550938513554008, -0.9861333108788019608, 5.358985056532664480E-15 ) ) ;
#50017 = FACE_OUTER_BOUND ( 'NONE', #18595, .T. ) ;
#50018 = CARTESIAN_POINT ( 'NONE',  ( 33.64224579327841980, -34.75806849055473435, 43.05022256185317531 ) ) ;
#50019 = EDGE_CURVE ( 'NONE', #75420, #33265, #34391, .T. ) ;
#50020 = CARTESIAN_POINT ( 'NONE',  ( -7.414580834929599185, 102.3534371971851726, 3.010264818013836940 ) ) ;
#50021 = AXIS2_PLACEMENT_3D ( 'NONE', #30125, #77059, #3175 ) ;
#50022 = CYLINDRICAL_SURFACE ( 'NONE', #31246, 4.000000000000000000 ) ;
#50023 = CARTESIAN_POINT ( 'NONE',  ( 85.78132872117437557, -35.63418972109697336, 184.6297816553372400 ) ) ;
#50024 = CARTESIAN_POINT ( 'NONE',  ( 8.572527594031501786E-16, 2.999999999999992450, 7.000000000000023981 ) ) ;
#50025 = DIRECTION ( 'NONE',  ( 1.000000000000000000, 0.000000000000000000, 0.000000000000000000 ) ) ;
#50026 = VERTEX_POINT ( 'NONE', #83963 ) ;
#50027 = CARTESIAN_POINT ( 'NONE',  ( 94.55070737517196733, -57.65490497192584485, -10.62783235369682799 ) ) ;
#50028 = FACE_OUTER_BOUND ( 'NONE', #23315, .T. ) ;
#50029 = DIRECTION ( 'NONE',  ( -1.000000000000000000, -1.224606353822377258E-16, -0.000000000000000000 ) ) ;
#50030 = CARTESIAN_POINT ( 'NONE',  ( 3.313708498984761608, -18.21874999999999645, -8.000000000000000000 ) ) ;
#50031 = CARTESIAN_POINT ( 'NONE',  ( -81.02929317658217201, -29.99999999999999645, 3.510823643410445172 ) ) ;
#50032 = CIRCLE ( 'NONE', #27685, 2.000000000000000444 ) ;
#50033 = PRESENTATION_STYLE_ASSIGNMENT (( #36035 ) ) ;
#50034 = CARTESIAN_POINT ( 'NONE',  ( 22.00868112945000021, 27.89883671455867287, -32.31191507115346440 ) ) ;
#50035 = CARTESIAN_POINT ( 'NONE',  ( 97.73333333333333428, 4.172000000000019249, 5.109226446042768454E-16 ) ) ;
#50037 = DIRECTION ( 'NONE',  ( 0.000000000000000000, -0.9887960631535436251, 0.1492727218618769280 ) ) ;
#50036 = CARTESIAN_POINT ( 'NONE',  ( 0.2573354458087814822, 4.368923434677189022, 5.432802636760777126 ) ) ;
#50038 = ADVANCED_FACE ( 'NONE', ( #91541 ), #23229, .F. ) ;
#50039 = CARTESIAN_POINT ( 'NONE',  ( -17.49999999999997513, 49.17184032807011107, 64.03033582390544609 ) ) ;
#50040 = CARTESIAN_POINT ( 'NONE',  ( -32.02495471002953309, 438.9490378437291156, 23.64594461092559996 ) ) ;
#50041 = CARTESIAN_POINT ( 'NONE',  ( 4.478476647430158941, -84.72647920817956901, 3.992942460563208229 ) ) ;
#50042 = CARTESIAN_POINT ( 'NONE',  ( 29.66054107240687543, 1.482358050883964840E-15, 0.000000000000000000 ) ) ;
#50043 = CARTESIAN_POINT ( 'NONE',  ( 6.249999999999998224, -6.928203230275509661, -4.000000000000000000 ) ) ;
#50044 = CARTESIAN_POINT ( 'NONE',  ( 33.74271564777237842, 484.1802673187710297, 2.058285076122392532 ) ) ;
#50045 = AXIS2_PLACEMENT_3D ( 'NONE', #43383, #25642, #2373 ) ;
#50046 = ORIENTED_EDGE ( 'NONE', *, *, #38218, .T. ) ;
#50047 = DIRECTION ( 'NONE',  ( -1.000000000000000000, -1.224606353822377258E-16, -0.000000000000000000 ) ) ;
#50048 = DIRECTION ( 'NONE',  ( 0.000000000000000000, 0.000000000000000000, 1.000000000000000000 ) ) ;
#50049 = CARTESIAN_POINT ( 'NONE',  ( -7.045755811259134305, 83.69658396986446292, 3.790843699961853552 ) ) ;
#50050 = CARTESIAN_POINT ( 'NONE',  ( -45.60865816377937421, -26.43209940392021906, -29.05745762912890484 ) ) ;
#50051 = AXIS2_PLACEMENT_3D ( 'NONE', #1431, #33312, #66184 ) ;
#50053 = CARTESIAN_POINT ( 'NONE',  ( 37.50059943756144776, 490.7879993827856993, 12.38039871356534505 ) ) ;
#50052 = DIRECTION ( 'NONE',  ( -1.000000000000000000, -0.000000000000000000, -0.000000000000000000 ) ) ;
#50054 = EDGE_CURVE ( 'NONE', #4234, #22906, #63868, .T. ) ;
#50055 = ORIENTED_EDGE ( 'NONE', *, *, #21526, .T. ) ;
#50056 = EDGE_CURVE ( 'NONE', #17114, #93530, #22536, .T. ) ;
#50057 = ORIENTED_EDGE ( 'NONE', *, *, #14073, .T. ) ;
#50058 = CARTESIAN_POINT ( 'NONE',  ( -26.78645834884456178, 34.58995912366707159, 10.02611660484962819 ) ) ;
#50059 = EDGE_CURVE ( 'NONE', #75948, #101891, #34632, .T. ) ;
#50060 = ADVANCED_FACE ( 'NONE', ( #82904 ), #84569, .T. ) ;
#50061 = CARTESIAN_POINT ( 'NONE',  ( 38.17475322892877898, 491.0341113493716421, 12.03733759146246740 ) ) ;
#50062 = AXIS2_PLACEMENT_3D ( 'NONE', #8625, #15654, #96595 ) ;
#50063 = DIRECTION ( 'NONE',  ( -1.000000000000000000, -0.000000000000000000, -0.000000000000000000 ) ) ;
#50064 = CARTESIAN_POINT ( 'NONE',  ( -59.89870783239705077, -60.00000000000000000, -35.70476153864051838 ) ) ;
#50065 = VERTEX_POINT ( 'NONE', #84508 ) ;
#50066 = DIRECTION ( 'NONE',  ( -1.000000000000000000, -0.000000000000000000, -0.000000000000000000 ) ) ;
#50067 = CARTESIAN_POINT ( 'NONE',  ( 15.50036553200073719, 2.628019270337233149, 0.8101929630272969307 ) ) ;
#50068 = CARTESIAN_POINT ( 'NONE',  ( 100.3141319396906823, -45.27614848971162331, 192.2799094378773361 ) ) ;
#50070 = CARTESIAN_POINT ( 'NONE',  ( -48.02835407290516656, 9.771516447483513446, 16.85535821593516559 ) ) ;
#50069 = CARTESIAN_POINT ( 'NONE',  ( 4.404194502973587610, 294.7962568506322327, -8.995744148930016948 ) ) ;
#50071 = AXIS2_PLACEMENT_3D ( 'NONE', #70803, #96146, #13075 ) ;
#50072 = ORIENTED_EDGE ( 'NONE', *, *, #104867, .T. ) ;
#50073 = EDGE_CURVE ( 'NONE', #54290, #83253, #31156, .T. ) ;
#50074 = ORIENTED_EDGE ( 'NONE', *, *, #89227, .F. ) ;
#50075 = VERTEX_POINT ( 'NONE', #85037 ) ;
#50076 = CARTESIAN_POINT ( 'NONE',  ( 31.16745676550236510, 425.0786795845950792, 24.76594861758827193 ) ) ;
#50077 = DIRECTION ( 'NONE',  ( -1.000000000000000000, -1.224606353822377258E-16, -0.000000000000000000 ) ) ;
#50078 = CARTESIAN_POINT ( 'NONE',  ( 0.000000000000000000, 0.000000000000000000, 4.000000000000000000 ) ) ;
#50079 = ORIENTED_EDGE ( 'NONE', *, *, #44524, .T. ) ;
#50080 = CARTESIAN_POINT ( 'NONE',  ( -42.08762648273147988, 487.0030674539048618, 9.106351919857871735 ) ) ;
#50081 = CARTESIAN_POINT ( 'NONE',  ( -32.42646496125482969, 485.5066083816486753, 3.829258843079225816 ) ) ;
#50082 = B_SPLINE_CURVE_WITH_KNOTS ( 'NONE', 3,
 ( #91308, #26079, #33606, #92342, #42740, #1734 ),
 .UNSPECIFIED., .F., .F.,
 ( 4, 2, 4 ),
 ( 0.005511122051665461215, 0.007432374760074458506, 0.009353627468483456664 ),
 .UNSPECIFIED. ) ;
#50083 = DIRECTION ( 'NONE',  ( -1.000000000000000000, -0.000000000000000000, -0.000000000000000000 ) ) ;
#50084 = CARTESIAN_POINT ( 'NONE',  ( -35.73279548032036956, -57.69589661319782437, 49.90756511973714282 ) ) ;
#50085 = CARTESIAN_POINT ( 'NONE',  ( 5.082755093536325930, -30.96875000204838813, -5.082755093536325042 ) ) ;
#50086 = CARTESIAN_POINT ( 'NONE',  ( -30.92872287337569048, 13.87446774603009558, 40.98770496732624480 ) ) ;
#50087 = DIRECTION ( 'NONE',  ( -1.000000000000000000, -1.224606353822377258E-16, -0.000000000000000000 ) ) ;
#50088 = CARTESIAN_POINT ( 'NONE',  ( 6.400000000000000355, 9.237604307034020579, -1.850927914596627675E-15 ) ) ;
#50089 = AXIS2_PLACEMENT_3D ( 'NONE', #61680, #101578, #77302 ) ;
#50090 = CARTESIAN_POINT ( 'NONE',  ( -94.21198422502472170, -59.99999999999998579, 13.85022971857252649 ) ) ;
#50091 = DIRECTION ( 'NONE',  ( -1.000000000000000000, -0.000000000000000000, -0.000000000000000000 ) ) ;
#50092 = CARTESIAN_POINT ( 'NONE',  ( -50.33888081872743214, -56.83758401715910225, 57.28329760184606556 ) ) ;
#50093 = VECTOR ( 'NONE', #75876, 1000.000000000000000 ) ;
#50094 = DIRECTION ( 'NONE',  ( 0.000000000000000000, 1.000000000000000000, 0.000000000000000000 ) ) ;
#50095 = B_SPLINE_CURVE_WITH_KNOTS ( 'NONE', 3,
 ( #86731, #11736, #12805, #78601, #94279, #53285, #86206, #12278, #24133, #16004, #14926, #65621, #65082, #38704, #73152, #7897, #31161, #105540, #55897, #106599 ),
 .UNSPECIFIED., .F., .F.,
 ( 4, 2, 2, 2, 2, 2, 2, 2, 2, 4 ),
 ( -6.890858614811975829E-05, 0.0009161940774506751629, 0.001901296741049470071, 0.002886399404648264978, 0.003871502068247059669, 0.004856604731845854360, 0.005841707395444649918, 0.006334258727244045963, 0.006826810059043442007, 0.007811912722642235830 ),
 .UNSPECIFIED. ) ;
#50096 = ORIENTED_EDGE ( 'NONE', *, *, #135, .T. ) ;
#50097 = CARTESIAN_POINT ( 'NONE',  ( -96.88649155114819678, -45.25226034781319839, 194.0198334961624482 ) ) ;
#50098 = CARTESIAN_POINT ( 'NONE',  ( -4.055648887808908754, 294.8040761930253666, -9.158006418688662720 ) ) ;
#50099 = CARTESIAN_POINT ( 'NONE',  ( 14.24611712352057857, 0.6929283341933295537, 14.98501566461477985 ) ) ;
#50100 = VERTEX_POINT ( 'NONE', #102275 ) ;
#50101 = CARTESIAN_POINT ( 'NONE',  ( -17.84561098364271459, 43.24919059263760346, 5.055340749336767026 ) ) ;
#50102 = CARTESIAN_POINT ( 'NONE',  ( 105.6520087378447528, -38.38240529042644766, 196.7784137681985612 ) ) ;
#50103 = DIRECTION ( 'NONE',  ( -1.000000000000000000, -0.000000000000000000, -0.000000000000000000 ) ) ;
#50104 = CARTESIAN_POINT ( 'NONE',  ( -5.454857745093078414, 51.31478691690154648, -8.531152949374575911 ) ) ;
#50105 = DIRECTION ( 'NONE',  ( 0.000000000000000000, -1.000000000000000000, 0.000000000000000000 ) ) ;
#50106 = SURFACE_SIDE_STYLE ('',( #90572 ) ) ;
#50107 = CARTESIAN_POINT ( 'NONE',  ( 85.25636826630055509, -30.00000000000000000, 172.6984853744677082 ) ) ;
#50108 = CARTESIAN_POINT ( 'NONE',  ( 36.28158941437224883, 490.9587137816808422, 12.45622313965986905 ) ) ;
#50109 = CARTESIAN_POINT ( 'NONE',  ( -32.02016918911336774, 464.7988659274551537, 11.81876822792606774 ) ) ;
#50110 = FILL_AREA_STYLE_COLOUR ( '', #94877 ) ;
#50111 = EDGE_CURVE ( 'NONE', #72013, #64557, #20890, .T. ) ;
#50112 = AXIS2_PLACEMENT_3D ( 'NONE', #46283, #95899, #13887 ) ;
#50113 = ORIENTED_EDGE ( 'NONE', *, *, #4682, .T. ) ;
#50114 = ORIENTED_EDGE ( 'NONE', *, *, #78523, .T. ) ;
#50115 = CARTESIAN_POINT ( 'NONE',  ( 51.77002234501873090, -42.97291842264748141, 55.07874347774893664 ) ) ;
#50116 = CARTESIAN_POINT ( 'NONE',  ( -33.33990657616918440, 464.2315420232590100, 17.97851960990337972 ) ) ;
#50117 = CARTESIAN_POINT ( 'NONE',  ( 9.812372088291331451, 51.27357729035378497, 2.926662531446465820 ) ) ;
#50118 = EDGE_CURVE ( 'NONE', #43310, #6068, #82789, .T. ) ;
#50119 = ORIENTED_EDGE ( 'NONE', *, *, #29783, .F. ) ;
#50120 = CARTESIAN_POINT ( 'NONE',  ( -108.0788720051916414, -38.35628241340692313, 138.4083630056905747 ) ) ;
#50121 = ORIENTED_EDGE ( 'NONE', *, *, #90337, .F. ) ;
#50122 = CARTESIAN_POINT ( 'NONE',  ( 106.6080917448352778, -38.35597051698264437, 127.9552692107341301 ) ) ;
#50123 = CARTESIAN_POINT ( 'NONE',  ( 13.30664220163338207, 22.17912454110582487, -4.025023027331216419 ) ) ;
#50124 = CARTESIAN_POINT ( 'NONE',  ( 82.71878536663017201, -37.85263159083670104, 22.06153483090329104 ) ) ;
#50125 = FACE_OUTER_BOUND ( 'NONE', #48793, .T. ) ;
#50126 = CARTESIAN_POINT ( 'NONE',  ( -1.630169624183789523, -5.000000000000000000, -16.56347947976414403 ) ) ;
#50127 = CARTESIAN_POINT ( 'NONE',  ( -31.78833566326770566, 317.3161387333121297, -5.990659203738045058 ) ) ;
#50128 = CARTESIAN_POINT ( 'NONE',  ( 74.36184181517107561, -60.00000000000000711, 175.8036861163617743 ) ) ;
#50129 = PRESENTATION_LAYER_ASSIGNMENT (  '', '', ( #7081 ) ) ;
#50130 = PRESENTATION_LAYER_ASSIGNMENT (  '', '', ( #41510 ) ) ;
#50131 = CARTESIAN_POINT ( 'NONE',  ( 17.58497575071690022, 45.00000000000000711, 63.15110831394576962 ) ) ;
#50132 = ORIENTED_EDGE ( 'NONE', *, *, #60282, .T. ) ;
#50133 = CARTESIAN_POINT ( 'NONE',  ( 62.23191167537439838, -46.43536929189312445, 81.72875552745274774 ) ) ;
#50134 = CARTESIAN_POINT ( 'NONE',  ( -22.25540596620007605, 295.0193264978564684, -1.964391734705814629 ) ) ;
#50135 = CARTESIAN_POINT ( 'NONE',  ( 0.000000000000000000, 0.000000000000000000, -1.971869939371574620 ) ) ;
#50136 = CARTESIAN_POINT ( 'NONE',  ( 12.21253585067004543, 1.340359594676612611E-15, 0.000000000000000000 ) ) ;
#50137 = MECHANICAL_DESIGN_GEOMETRIC_PRESENTATION_REPRESENTATION (  '', ( #69108 ), #86366 ) ;
#50139 = CARTESIAN_POINT ( 'NONE',  ( -37.21896735870636519, 485.5897823164965530, -4.183926505970648080 ) ) ;
#50138 = CARTESIAN_POINT ( 'NONE',  ( -76.84754332433912793, -29.99999999997301359, 173.7522665578053704 ) ) ;
#50140 = CARTESIAN_POINT ( 'NONE',  ( -42.74137506439731737, 379.1533860022373119, 18.72083839136980643 ) ) ;
#50141 = CARTESIAN_POINT ( 'NONE',  ( -37.56673239365863282, 25.47613764497371847, -13.45617127781024891 ) ) ;
#50142 = LINE ( 'NONE', #83050, #83422 ) ;
#50143 = CARTESIAN_POINT ( 'NONE',  ( 8.000000000000000000, -28.99999999999999289, 0.000000000000000000 ) ) ;
#50144 = CARTESIAN_POINT ( 'NONE',  ( -5.036189802311206165, -3.000000000000002665, -76.26213611587844809 ) ) ;
#50145 = PRESENTATION_LAYER_ASSIGNMENT (  '', '', ( #24320 ) ) ;
#50146 = ADVANCED_FACE ( 'NONE', ( #68869 ), #95261, .F. ) ;
#50147 = AXIS2_PLACEMENT_3D ( 'NONE', #50539, #76421, #59733 ) ;
#50149 = B_SPLINE_CURVE_WITH_KNOTS ( 'NONE', 3,
 ( #48914, #56480, #48391, #99057 ),
 .UNSPECIFIED., .F., .F.,
 ( 4, 4 ),
 ( 0.000000000000000000, 1.000000000000000000 ),
 .UNSPECIFIED. ) ;
#50148 = CARTESIAN_POINT ( 'NONE',  ( 16.64348903516496492, 43.47556584774762456, -6.657797401562562278 ) ) ;
#50150 = ORIENTED_EDGE ( 'NONE', *, *, #92693, .T. ) ;
#50151 = CARTESIAN_POINT ( 'NONE',  ( 83.18190987619777843, -46.51210091988467354, 180.8283602554456877 ) ) ;
#50152 = EDGE_CURVE ( 'NONE', #80922, #90030, #87958, .T. ) ;
#50153 = CARTESIAN_POINT ( 'NONE',  ( 43.94956565205495735, 434.7294131184629009, 8.824837262785111491 ) ) ;
#50154 = CARTESIAN_POINT ( 'NONE',  ( 38.09999999999998721, 4.052968581778165278E-16, -3.309499999999999886 ) ) ;
#50155 = VERTEX_POINT ( 'NONE', #10597 ) ;
#50156 = DIRECTION ( 'NONE',  ( -1.000000000000000000, -0.000000000000000000, -0.000000000000000000 ) ) ;
#50157 = CARTESIAN_POINT ( 'NONE',  ( 41.08349330513380693, 4.000000000000002665, 0.000000000000000000 ) ) ;
#50158 = CARTESIAN_POINT ( 'NONE',  ( 0.000000000000000000, 0.000000000000000000, -2.716724522925831220 ) ) ;
#50159 = FILL_AREA_STYLE_COLOUR ( '', #16110 ) ;
#50160 = CARTESIAN_POINT ( 'NONE',  ( -27.36171982050201024, -28.59563504858160599, -38.29070100074284966 ) ) ;
#50161 = CARTESIAN_POINT ( 'NONE',  ( -11.96518466135214886, -2.129975200491694753, 20.65966393205720664 ) ) ;
#50162 = B_SPLINE_CURVE_WITH_KNOTS ( 'NONE', 3,
 ( #67669, #98940, #67135, #90881, #59049, #7812, #33720, #73609, #75202, #66596, #58514, #50394, #9397, #100549, #32668, #42313, #26712, #91933, #83835, #48797, #65539, #36925 ),
 .UNSPECIFIED., .F., .F.,
 ( 4, 2, 2, 2, 2, 2, 2, 2, 2, 2, 4 ),
 ( 0.003168291407922112484, 0.003670795193784145982, 0.004173298979646179047, 0.004675802765508212111, 0.004927054658439226908, 0.005178306551370240839, 0.005680810337232268699, 0.005932062230163284364, 0.006183314123094299161, 0.006685817908956327021, 0.007188321694818354882 ),
 .UNSPECIFIED. ) ;
#50163 =( NAMED_UNIT ( * ) SI_UNIT ( $, .STERADIAN. ) SOLID_ANGLE_UNIT ( ) );
#50164 = AXIS2_PLACEMENT_3D ( 'NONE', #93324, #4308, #3252 ) ;
#50165 = CARTESIAN_POINT ( 'NONE',  ( 54.03418529048751395, -60.00000000000000000, 82.52390411942170090 ) ) ;
#50166 = CARTESIAN_POINT ( 'NONE',  ( 0.000000000000000000, 0.000000000000000000, 1.734723475976807094E-15 ) ) ;
#50167 = CARTESIAN_POINT ( 'NONE',  ( 6.808966170647585692, -13.13057375426282825, 32.04009476704212034 ) ) ;
#50169 = CARTESIAN_POINT ( 'NONE',  ( -13.75359951688389160, 20.47115004747033851, -6.669194425414865179 ) ) ;
#50168 = CARTESIAN_POINT ( 'NONE',  ( -24.00273426019377965, -28.36012771311524361, 37.92953909826832870 ) ) ;
#50170 = CONICAL_SURFACE ( 'NONE', #20979, 7.000000000000000000, 0.9599310885968753704 ) ;
#50171 = CARTESIAN_POINT ( 'NONE',  ( -2.977408999572654480, -15.12500000204838457, 7.188101187499999156 ) ) ;
#50172 =( LENGTH_UNIT ( ) NAMED_UNIT ( * ) SI_UNIT ( .MILLI., .METRE. ) );
#50173 = LINE ( 'NONE', #34566, #56924 ) ;
#50174 = ORIENTED_EDGE ( 'NONE', *, *, #32198, .T. ) ;
#50175 = CARTESIAN_POINT ( 'NONE',  ( -19.09326099321248549, 49.66527553187732025, 61.75128748409861856 ) ) ;
#50176 = DIRECTION ( 'NONE',  ( 0.000000000000000000, -1.000000000000000000, 0.000000000000000000 ) ) ;
#50177 = PRESENTATION_STYLE_ASSIGNMENT (( #17305 ) ) ;
#50178 =( BOUNDED_SURFACE ( )  B_SPLINE_SURFACE ( 3, 2, ( 
 ( #93309, #42083, #59357 ),
 ( #74971, #17836, #83601 ),
 ( #67444, #35095, #51224 ),
 ( #9706, #87348, #93837 ),
 ( #69569, #21054, #29152 ),
 ( #45295, #78174, #52839 ),
 ( #12369, #53892, #79235 ),
 ( #38792, #4293, #37760 ),
 ( #36704, #5363, #19996 ),
 ( #12893, #70624, #102992 ),
 ( #86823, #54401, #61488 ),
 ( #53380, #71662, #62023 ),
 ( #3772, #102458, #60948 ),
 ( #38281, #37225, #71144 ),
 ( #28606, #103514, #94381 ),
 ( #85764, #45821, #21562 ),
 ( #11838, #20542, #86299 ),
 ( #29667, #4825, #78691 ),
 ( #70089, #44768, #13423 ),
 ( #94918, #54944, #62537 ),
 ( #95424, #46346, #104034 ),
 ( #30174, #77658, #63066 ),
 ( #95965, #22090, #79762 ),
 ( #87872, #13956, #46866 ),
 ( #5868, #28077, #48448 ),
 ( #82427, #7994, #57070 ),
 ( #65714, #41430, #39331 ),
 ( #40366, #89465, #15558 ) ),
 .UNSPECIFIED., .F., .F., .F. ) 
 B_SPLINE_SURFACE_WITH_KNOTS ( ( 4, 2, 2, 2, 2, 2, 2, 2, 2, 2, 2, 2, 2, 4 ),
 ( 3, 3 ),
 ( 0.008123433161209985681, 0.009051127437186799740, 0.009978821713163612064, 0.01090651598914042439, 0.01183421026511723845, 0.01276190454109405077, 0.01368959881707086310, 0.01461729309304767715, 0.01554498736902448948, 0.01647268164500130180, 0.01740037592097811586, 0.01925576447293174051, 0.02111115302488536516, 0.02296654157683899328 ),
 ( 0.000000000000000000, 1.000000000000000000 ),
 .UNSPECIFIED. ) 
 GEOMETRIC_REPRESENTATION_ITEM ( )  RATIONAL_B_SPLINE_SURFACE ( (
 ( 1.000000000000000000, 0.5207636911093219689, 1.000000000000000000),
 ( 1.000000000000000000, 0.5178187716629953918, 1.000000000000000000),
 ( 1.000000000000000000, 0.5159244862375357288, 1.000000000000000000),
 ( 1.000000000000000000, 0.5142886050002780651, 1.000000000000000000),
 ( 1.000000000000000000, 0.5145473390822793425, 1.000000000000000000),
 ( 1.000000000000000000, 0.5172493923475872668, 1.000000000000000000),
 ( 1.000000000000000000, 0.5196793001234910614, 1.000000000000000000),
 ( 1.000000000000000000, 0.5263251517290957748, 1.000000000000000000),
 ( 1.000000000000000000, 0.5305477076593381192, 1.000000000000000000),
 ( 1.000000000000000000, 0.5405083355075952500, 1.000000000000000000),
 ( 1.000000000000000000, 0.5462226599306142516, 1.000000000000000000),
 ( 1.000000000000000000, 0.5585066026749704315, 1.000000000000000000),
 ( 1.000000000000000000, 0.5651105631668802420, 1.000000000000000000),
 ( 1.000000000000000000, 0.5789734458161401864, 1.000000000000000000),
 ( 1.000000000000000000, 0.5862399530452739871, 1.000000000000000000),
 ( 1.000000000000000000, 0.6008664520152333655, 1.000000000000000000),
 ( 1.000000000000000000, 0.6082721003052478093, 1.000000000000000000),
 ( 1.000000000000000000, 0.6231433865265936234, 1.000000000000000000),
 ( 1.000000000000000000, 0.6306097951832441151, 1.000000000000000000),
 ( 1.000000000000000000, 0.6455317574246466350, 1.000000000000000000),
 ( 1.000000000000000000, 0.6530101251172123478, 1.000000000000000000),
 ( 1.000000000000000000, 0.6749576138080563004, 1.000000000000000000),
 ( 1.000000000000000000, 0.6890737998548138732, 1.000000000000000000),
 ( 1.000000000000000000, 0.7163646493011636140, 1.000000000000000000),
 ( 1.000000000000000000, 0.7295941717914107283, 1.000000000000000000),
 ( 1.000000000000000000, 0.7548878312893493314, 1.000000000000000000),
 ( 1.000000000000000000, 0.7668601322836052780, 1.000000000000000000),
 ( 1.000000000000000000, 0.7779866052154993383, 1.000000000000000000) ) ) 
 REPRESENTATION_ITEM ( '' )  SURFACE ( )  );
#50180 = CARTESIAN_POINT ( 'NONE',  ( 28.77839882463454657, -47.40898664704774035, -33.14052421978329477 ) ) ;
#50179 = CARTESIAN_POINT ( 'NONE',  ( 2.499999999999984457, -21.99834388059804269, -30.53959902372158908 ) ) ;
#50182 = EDGE_CURVE ( 'NONE', #76051, #47334, #51825, .T. ) ;
#50181 = CIRCLE ( 'NONE', #13986, 2.999999999999988010 ) ;
#50183 = EDGE_LOOP ( 'NONE', ( #42696, #28361, #78651, #75013 ) ) ;
#50184 = CARTESIAN_POINT ( 'NONE',  ( -4.472135954999579610, -85.00000000000000000, -4.000000000000001776 ) ) ;
#50185 =( LENGTH_UNIT ( ) NAMED_UNIT ( * ) SI_UNIT ( .MILLI., .METRE. ) );
#50186 = VERTEX_POINT ( 'NONE', #53203 ) ;
#50187 = EDGE_CURVE ( 'NONE', #77405, #93124, #62370, .T. ) ;
#50188 = DIRECTION ( 'NONE',  ( -1.000000000000000000, -1.224606353822377258E-16, -0.000000000000000000 ) ) ;
#50189 = ADVANCED_FACE ( 'NONE', ( #3590 ), #72845, .T. ) ;
#50190 = DIRECTION ( 'NONE',  ( -0.000000000000000000, -0.000000000000000000, -1.000000000000000000 ) ) ;
#50191 = CARTESIAN_POINT ( 'NONE',  ( -20.77102041147630729, 41.81346959299248311, -78.66739485428914236 ) ) ;
#50192 = CARTESIAN_POINT ( 'NONE',  ( -98.09066009260625663, -60.00000000000000711, 69.48659794401923762 ) ) ;
#50193 = DIRECTION ( 'NONE',  ( -0.000000000000000000, -0.000000000000000000, -1.000000000000000000 ) ) ;
#50194 = CARTESIAN_POINT ( 'NONE',  ( -44.03570364123616798, 435.3116947630537084, 15.43179346459665524 ) ) ;
#50195 = CARTESIAN_POINT ( 'NONE',  ( -30.00000000000000000, -54.00000000000000711, 23.11721482942554928 ) ) ;
#50197 = CARTESIAN_POINT ( 'NONE',  ( -6.315918965248128458, 41.33387153033192618, -58.37026290468334366 ) ) ;
#50196 = CARTESIAN_POINT ( 'NONE',  ( -34.10808184343350291, 434.1697022380918156, 11.22013956023728909 ) ) ;
#50198 = CARTESIAN_POINT ( 'NONE',  ( -82.28169001980204200, -46.46948612797371680, 174.1992972938939772 ) ) ;
#50199 = ORIENTED_EDGE ( 'NONE', *, *, #23380, .T. ) ;
#50200 = CIRCLE ( 'NONE', #96727, 9.000000000000000000 ) ;
#50201 = EDGE_CURVE ( 'NONE', #23441, #2917, #12181, .T. ) ;
#50202 = ORIENTED_EDGE ( 'NONE', *, *, #9204, .T. ) ;
#50203 = AXIS2_PLACEMENT_3D ( 'NONE', #72180, #98042, #81836 ) ;
#50204 = ORIENTED_EDGE ( 'NONE', *, *, #38286, .F. ) ;
#50205 = DIRECTION ( 'NONE',  ( 0.000000000000000000, 1.000000000000000000, 0.000000000000000000 ) ) ;
#50206 = FACE_OUTER_BOUND ( 'NONE', #97232, .T. ) ;
#50207 = ORIENTED_EDGE ( 'NONE', *, *, #52997, .T. ) ;
#50208 = DIRECTION ( 'NONE',  ( -1.000000000000000000, -1.224606353822377258E-16, -0.000000000000000000 ) ) ;
#50209 = CARTESIAN_POINT ( 'NONE',  ( -47.47329288218261922, -57.67116814553164517, -40.40967777935767202 ) ) ;
#50210 = LINE ( 'NONE', #24382, #90382 ) ;
#50211 = CARTESIAN_POINT ( 'NONE',  ( -7.619753052866895082, -61.82548497192825465, -2.447276542590449910 ) ) ;
#50212 = CARTESIAN_POINT ( 'NONE',  ( 43.03357534759661718, 463.2291678140137492, 4.675918524166122303 ) ) ;
#50213 = DIRECTION ( 'NONE',  ( 0.000000000000000000, 0.000000000000000000, 1.000000000000000000 ) ) ;
#50214 = CARTESIAN_POINT ( 'NONE',  ( 43.66729043033832625, 435.6676719292337907, 17.39374879622096159 ) ) ;
#50215 = AXIS2_PLACEMENT_3D ( 'NONE', #62442, #86202, #69994 ) ;
#50216 = CARTESIAN_POINT ( 'NONE',  ( 108.0662294780436383, -29.99999999999999645, 149.4678247624379708 ) ) ;
#50217 = AXIS2_PLACEMENT_3D ( 'NONE', #76295, #2405, #18083 ) ;
#50218 = CARTESIAN_POINT ( 'NONE',  ( -114.4010969832937121, -60.00000000000006395, 179.2248356726699399 ) ) ;
#50219 = CARTESIAN_POINT ( 'NONE',  ( -57.65532094949794839, -49.91396688608944743, 71.01409991697076407 ) ) ;
#50220 = ORIENTED_EDGE ( 'NONE', *, *, #60882, .F. ) ;
#50221 = CARTESIAN_POINT ( 'NONE',  ( 60.72168482585779259, 38.95312673567827488, -19.36417048051057677 ) ) ;
#50222 = CARTESIAN_POINT ( 'NONE',  ( 113.4579317004694445, -59.99999999998775024, 187.0486580085058961 ) ) ;
#50223 = ORIENTED_EDGE ( 'NONE', *, *, #71883, .T. ) ;
#50224 = CARTESIAN_POINT ( 'NONE',  ( 6.036068601854779558, -29.02932134256533203, 28.71825046550461380 ) ) ;
#50225 = CARTESIAN_POINT ( 'NONE',  ( -100.3227765610642734, -37.82072275983777843, 142.2249858778365876 ) ) ;
#50226 = CARTESIAN_POINT ( 'NONE',  ( 7.188101187500000933, -14.93750000204838457, -2.977408999572650483 ) ) ;
#50227 = DIRECTION ( 'NONE',  ( 0.9915366780650388678, -0.1269898409407509698, -0.02699252395738872823 ) ) ;
#50228 = CARTESIAN_POINT ( 'NONE',  ( 37.31633518135760141, 464.0415485246131198, 19.53686901080153149 ) ) ;
#50229 = ORIENTED_EDGE ( 'NONE', *, *, #17367, .F. ) ;
#50230 = CARTESIAN_POINT ( 'NONE',  ( -6.499999999999999112, -3.752776749732595452, -0.7999999999999977129 ) ) ;
#50231 = CARTESIAN_POINT ( 'NONE',  ( -29.92534626571542944, -60.00000000000000000, 42.99766300317948975 ) ) ;
#50232 = SURFACE_STYLE_USAGE ( .BOTH. , #57776 ) ;
#50233 = CARTESIAN_POINT ( 'NONE',  ( -5.082755093536326818, -23.09375000204838457, 5.082755093536325042 ) ) ;
#50234 = DIRECTION ( 'NONE',  ( 0.000000000000000000, -1.000000000000000000, 0.000000000000000000 ) ) ;
#50235 = CARTESIAN_POINT ( 'NONE',  ( -89.99999999999997158, -60.00000000000000000, 196.0238439516549818 ) ) ;
#50236 = CARTESIAN_POINT ( 'NONE',  ( -1.344569080228518650E-17, 21.85270131633358304, -7.000000000000011546 ) ) ;
#50237 = CARTESIAN_POINT ( 'NONE',  ( 5.000000000000000000, -3.274104202382571494, -10.50969124766998952 ) ) ;
#50238 = CARTESIAN_POINT ( 'NONE',  ( 32.87816783969756784, 464.9425048721737994, 11.07737551929927022 ) ) ;
#50239 =( LENGTH_UNIT ( ) NAMED_UNIT ( * ) SI_UNIT ( .MILLI., .METRE. ) );
#50240 = DIRECTION ( 'NONE',  ( -1.000000000000000000, -1.224606353822377258E-16, -0.000000000000000000 ) ) ;
#50241 = CARTESIAN_POINT ( 'NONE',  ( 103.9527125734255861, -59.99999999999999289, 141.3402690312935874 ) ) ;
#50242 = CARTESIAN_POINT ( 'NONE',  ( -32.67571524685207862, -36.02606224958812930, 33.54986086304085546 ) ) ;
#50243 = AXIS2_PLACEMENT_3D ( 'NONE', #44807, #77696, #63101 ) ;
#50244 = CARTESIAN_POINT ( 'NONE',  ( -1.992238869817497093, -49.88365665291251361, 102.1880563748276955 ) ) ;
#50245 = CARTESIAN_POINT ( 'NONE',  ( 44.85640785158575738, -46.43708517621621468, 45.33465009235806065 ) ) ;
#50246 = AXIS2_PLACEMENT_3D ( 'NONE', #20467, #105436, #55788 ) ;
#50247 = CARTESIAN_POINT ( 'NONE',  ( 18.58349330513380693, 1.593028355512270962E-15, 0.000000000000000000 ) ) ;
#50248 = ORIENTED_EDGE ( 'NONE', *, *, #516, .F. ) ;
#50249 = CARTESIAN_POINT ( 'NONE',  ( 43.37695759419762709, 434.6160983767974813, 10.05510951421143595 ) ) ;
#50250 = EDGE_CURVE ( 'NONE', #11128, #87415, #70772, .T. ) ;
#50251 = CARTESIAN_POINT ( 'NONE',  ( -81.54857902955093607, -38.84165332927102554, 195.3365240599568153 ) ) ;
#50252 = ORIENTED_EDGE ( 'NONE', *, *, #60320, .T. ) ;
#50254 = SURFACE_STYLE_FILL_AREA ( #17380 ) ;
#50253 = CARTESIAN_POINT ( 'NONE',  ( 0.000000000000000000, 79.50000000000000000, -66.00000000000000000 ) ) ;
#50255 = CARTESIAN_POINT ( 'NONE',  ( 50.11938532533323354, -59.99999999999997868, 57.93673938823967973 ) ) ;
#50256 = CARTESIAN_POINT ( 'NONE',  ( 0.000000000000000000, -79.93083296558610584, -85.00000000000000000 ) ) ;
#50257 = CARTESIAN_POINT ( 'NONE',  ( -43.34642793437723185, 464.8022470470604048, 10.25621957592192857 ) ) ;
#50258 = DIRECTION ( 'NONE',  ( -1.000000000000000000, -1.224606353822377258E-16, -0.000000000000000000 ) ) ;
#50259 = DIRECTION ( 'NONE',  ( -1.000000000000000000, -1.224606353822377258E-16, -0.000000000000000000 ) ) ;
#50260 = CARTESIAN_POINT ( 'NONE',  ( -29.78543059554420225, 327.5436091316801139, 14.51305068536635012 ) ) ;
#50261 = CARTESIAN_POINT ( 'NONE',  ( 17.71951158999540610, 45.45134770963999671, 4.750929343604541444 ) ) ;
#50262 = CARTESIAN_POINT ( 'NONE',  ( 103.3162346027592804, -59.99999999999999289, 100.4319430175666810 ) ) ;
#50263 = CARTESIAN_POINT ( 'NONE',  ( 15.05785784214677392, 3.824195276769925655, -4.604276673498363337 ) ) ;
#50264 = FACE_OUTER_BOUND ( 'NONE', #6416, .T. ) ;
#50265 = EDGE_CURVE ( 'NONE', #6164, #13541, #31599, .T. ) ;
#50266 = VERTEX_POINT ( 'NONE', #73064 ) ;
#50267 = CARTESIAN_POINT ( 'NONE',  ( -101.1327230100927181, -30.00000000000000355, 173.0889935382795954 ) ) ;
#50268 = EDGE_LOOP ( 'NONE', ( #11582, #68920, #69649, #65122, #44490 ) ) ;
#50269 = CARTESIAN_POINT ( 'NONE',  ( 35.59999999999999432, 1.533819458162526451E-15, 0.000000000000000000 ) ) ;
#50270 = FILL_AREA_STYLE_COLOUR ( '', #23577 ) ;
#50271 = CARTESIAN_POINT ( 'NONE',  ( 20.56658349655994300, 303.9107536853347824, 9.949562365852784751 ) ) ;
#50272 = CARTESIAN_POINT ( 'NONE',  ( -22.19982010036164866, 28.18804608458828653, -31.21118039878593464 ) ) ;
#50273 = CARTESIAN_POINT ( 'NONE',  ( -1.320432766682874540E-15, -18.40625000204838457, 7.188101187500000044 ) ) ;
#50274 = DIRECTION ( 'NONE',  ( 0.000000000000000000, 1.000000000000000000, 0.000000000000000000 ) ) ;
#50276 = EDGE_LOOP ( 'NONE', ( #55802, #96054, #8283, #15336 ) ) ;
#50275 = FILL_AREA_STYLE_COLOUR ( '', #46031 ) ;
#50277 = CARTESIAN_POINT ( 'NONE',  ( 84.58095252641739137, -25.55800566126467999, 162.3696887303881056 ) ) ;
#50278 = EDGE_CURVE ( 'NONE', #38824, #74088, #46679, .T. ) ;
#50279 = CARTESIAN_POINT ( 'NONE',  ( 9.165151389911679658, 85.00000000000000000, 4.000000000000000000 ) ) ;
#50280 = VERTEX_POINT ( 'NONE', #97891 ) ;
#50281 = CIRCLE ( 'NONE', #77863, 3.400000000000000355 ) ;
#50282 = FACE_OUTER_BOUND ( 'NONE', #14260, .T. ) ;
#50283 = DIRECTION ( 'NONE',  ( -1.000000000000000000, 0.000000000000000000, 0.000000000000000000 ) ) ;
#50284 = CARTESIAN_POINT ( 'NONE',  ( -5.000000000000002665, 152.0000000000000000, 5.000000000000000000 ) ) ;
#50285 = CARTESIAN_POINT ( 'NONE',  ( 6.162888688655347558, -3.752776749732574135, -6.500000000000001776 ) ) ;
#50286 = CARTESIAN_POINT ( 'NONE',  ( -4.814352310392307821, 251.7967859410357221, -3.583053941560747191 ) ) ;
#50287 = CARTESIAN_POINT ( 'NONE',  ( -30.15464468665757991, 316.8850315688116552, 13.37365732414975206 ) ) ;
#50288 = EDGE_CURVE ( 'NONE', #94695, #75208, #60492, .T. ) ;
#50289 = EDGE_LOOP ( 'NONE', ( #72841, #55916, #40390, #85741 ) ) ;
#50290 = B_SPLINE_CURVE_WITH_KNOTS ( 'NONE', 3,
 ( #24983, #96348, #22476, #24469, #74030, #90222, #49218, #70991, #81565, #5720, #95809, #41671, #103879, #55319, #73488, #16877, #74559, #8765, #16327, #32548, #88245, #71507, #62913, #90761, #30028, #632, #21938, #47232, #13269, #54788, #82115, #87718, #13802, #104409, #46711, #33600, #65420, #8235, #109, #7695, #41146, #49757, #5204, #82663, #95282, #21410, #54247, #46191 ),
 .UNSPECIFIED., .F., .F.,
 ( 4, 2, 2, 2, 2, 2, 2, 2, 2, 2, 1, 2, 2, 1, 2, 2, 2, 2, 2, 2, 2, 2, 2, 2, 4 ),
 ( 1.003362932294564080, 1.007956983089783654, 1.012551033885003005, 1.021739135475442151, 1.030927237065881075, 1.040115338656319999, 1.049303440246759145, 1.058491541837198069, 1.067679643427636993, 1.076867745018076139, 1.078016257716881032, 1.078303385891582256, 1.078590514066283479, 1.079164770415685926, 1.081461795813295490, 1.086055846608515063, 1.095243948198953987, 1.104432049789393133, 1.113620151379832057, 1.122808252970271203, 1.127402303765490554, 1.131996354560710127, 1.141184456151149273, 1.145778506946368624, 1.150372557741588198 ),
 .UNSPECIFIED. ) ;
#50292 = DIRECTION ( 'NONE',  ( -0.5735764363510494901, -0.8191520442889894671, 0.000000000000000000 ) ) ;
#50291 = CIRCLE ( 'NONE', #19333, 10.00000000000000533 ) ;
#50293 = CARTESIAN_POINT ( 'NONE',  ( -1.000000000000000000, -67.36501624957764989, 11.52273887415191922 ) ) ;
#50294 = CARTESIAN_POINT ( 'NONE',  ( 14.82166267806915094, 22.90614510862747011, 2.002102660500554521 ) ) ;
#50295 = VECTOR ( 'NONE', #80674, 1000.000000000000000 ) ;
#50296 = LINE ( 'NONE', #40613, #65398 ) ;
#50297 = CARTESIAN_POINT ( 'NONE',  ( -2.977408999572650039, -33.68750000204839523, -7.188101187500001821 ) ) ;
#50298 = CARTESIAN_POINT ( 'NONE',  ( -41.74100955526786549, 489.2843990805219505, 10.50852780968136813 ) ) ;
#50299 = CARTESIAN_POINT ( 'NONE',  ( 6.936184427528457874, 0.000000000000000000, 0.000000000000000000 ) ) ;
#50300 = CARTESIAN_POINT ( 'NONE',  ( 48.91516379432449924, 8.057663746602608867, 16.48802948946137548 ) ) ;
#50301 = ORIENTED_EDGE ( 'NONE', *, *, #13090, .T. ) ;
#50302 = CARTESIAN_POINT ( 'NONE',  ( 10.28624191511840458, 45.38549880562042205, 15.40779740156149202 ) ) ;
#50303 = CARTESIAN_POINT ( 'NONE',  ( -33.11890921805862575, 438.9412750689605787, 23.90522689637586140 ) ) ;
#50304 = CARTESIAN_POINT ( 'NONE',  ( -5.832992532897281812, 4.736036812732102419, -5.000000000000000000 ) ) ;
#50305 = DIRECTION ( 'NONE',  ( 0.000000000000000000, 1.000000000000000000, 0.000000000000000000 ) ) ;
#50306 = AXIS2_PLACEMENT_3D ( 'NONE', #8565, #67875, #43597 ) ;
#50307 = ORIENTED_EDGE ( 'NONE', *, *, #47517, .T. ) ;
#50308 =( NAMED_UNIT ( * ) PLANE_ANGLE_UNIT ( ) SI_UNIT ( $, .RADIAN. ) );
#50309 = CARTESIAN_POINT ( 'NONE',  ( -7.500000000000005329, 41.41666666666666430, -68.91429205785459544 ) ) ;
#50310 = CARTESIAN_POINT ( 'NONE',  ( 109.9183362485910749, -57.66822971772113959, 196.2431448240839700 ) ) ;
#50311 = CONICAL_SURFACE ( 'NONE', #29732, 3.309500000000001663, 0.9599310885968770357 ) ;
#50312 = ORIENTED_EDGE ( 'NONE', *, *, #86149, .T. ) ;
#50313 = AXIS2_PLACEMENT_3D ( 'NONE', #73389, #106290, #48058 ) ;
#50314 = CARTESIAN_POINT ( 'NONE',  ( 61.11682663846713837, 6.975173280561618775E-15, 0.000000000000000000 ) ) ;
#50315 = CYLINDRICAL_SURFACE ( 'NONE', #49322, 5.000000000000000888 ) ;
#50316 = DIRECTION ( 'NONE',  ( -0.5735764363510512664, 0.8191520442889881348, 1.003171929053520309E-16 ) ) ;
#50317 = CARTESIAN_POINT ( 'NONE',  ( -76.86091367493919790, -60.00000000000000000, 190.0407920036354597 ) ) ;
#50318 = CARTESIAN_POINT ( 'NONE',  ( 9.293831213271754876, 43.59774867130855824, -14.93437611856834835 ) ) ;
#50319 = CARTESIAN_POINT ( 'NONE',  ( -35.96492786661492858, 302.4488314805894902, -8.278427239160079054 ) ) ;
#50320 = CARTESIAN_POINT ( 'NONE',  ( -84.73889666017791455, -39.38651883830629430, 182.5246982632422714 ) ) ;
#50321 = ORIENTED_EDGE ( 'NONE', *, *, #98491, .F. ) ;
#50322 = CARTESIAN_POINT ( 'NONE',  ( 24.06928029728074492, 304.6542708667294619, -9.827242677062491438 ) ) ;
#50323 = EDGE_CURVE ( 'NONE', #84503, #43166, #81279, .T. ) ;
#50324 = EDGE_LOOP ( 'NONE', ( #34205, #47434, #103067, #75758, #11473 ) ) ;
#50325 = CARTESIAN_POINT ( 'NONE',  ( 71.14984002819953446, 6.856755485862130937E-15, 0.000000000000000000 ) ) ;
#50326 = ADVANCED_FACE ( 'NONE', ( #47737 ), #54229, .T. ) ;
#50327 = CARTESIAN_POINT ( 'NONE',  ( -83.25032691496221560, -37.78210659561245421, -7.769091474988147894 ) ) ;
#50328 = CARTESIAN_POINT ( 'NONE',  ( -4.293150003527051339, -12.96978500885295738, -9.455099716441258906 ) ) ;
#50329 = CARTESIAN_POINT ( 'NONE',  ( -15.88225526726033365, 44.00162778657170293, 4.402143696494996483 ) ) ;
#50330 = CARTESIAN_POINT ( 'NONE',  ( 21.88049162136248071, 294.9920307902382319, 9.966805799653187137 ) ) ;
#50331 = CARTESIAN_POINT ( 'NONE',  ( 32.33349330513379982, 1.593028355512270567E-15, 0.000000000000000000 ) ) ;
#50332 = CARTESIAN_POINT ( 'NONE',  ( -90.56128410203886858, 42.00000000000000000, -11.85444436786843703 ) ) ;
#50333 = CARTESIAN_POINT ( 'NONE',  ( -2.071635198146551927E-15, 58.72416816948006613, 16.91618513671782509 ) ) ;
#50334 = CARTESIAN_POINT ( 'NONE',  ( 0.000000000000000000, 0.000000000000000000, -0.5505556536572887572 ) ) ;
#50335 = CARTESIAN_POINT ( 'NONE',  ( -61.70175965769652748, -30.00000000000001066, -32.45223383460360367 ) ) ;
#50336 = CARTESIAN_POINT ( 'NONE',  ( -66.15153670451748269, -56.86596900142542665, 99.15932261016065752 ) ) ;
#50337 = ORIENTED_EDGE ( 'NONE', *, *, #8991, .T. ) ;
#50338 = CARTESIAN_POINT ( 'NONE',  ( 68.99587917277882809, -30.00000000000005329, 123.4883035811859884 ) ) ;
#50339 = CARTESIAN_POINT ( 'NONE',  ( 94.71841002673514254, -57.66036132024994743, -7.141312747736634492 ) ) ;
#50340 = ORIENTED_EDGE ( 'NONE', *, *, #32601, .T. ) ;
#50341 = DIRECTION ( 'NONE',  ( 0.000000000000000000, -1.000000000000000000, 0.000000000000000000 ) ) ;
#50342 = DIRECTION ( 'NONE',  ( 0.000000000000000000, -1.000000000000000000, 0.000000000000000000 ) ) ;
#50343 = ORIENTED_EDGE ( 'NONE', *, *, #30394, .T. ) ;
#50344 = CARTESIAN_POINT ( 'NONE',  ( 2.448541588119020673, 14.67925956666102572, -6.561650255352408756 ) ) ;
#50345 = DIRECTION ( 'NONE',  ( 1.000000000000000000, 0.000000000000000000, 0.000000000000000000 ) ) ;
#50346 = CARTESIAN_POINT ( 'NONE',  ( 0.000000000000000000, 115.0000000000000000, 0.000000000000000000 ) ) ;
#50347 = CARTESIAN_POINT ( 'NONE',  ( -7.188101187500002709, -15.31250000204838457, 2.977408999572648707 ) ) ;
#50348 = CARTESIAN_POINT ( 'NONE',  ( 44.12472801210888917, 485.7238370326480208, 3.975897585123575606 ) ) ;
#50349 = TOROIDAL_SURFACE ( 'NONE', #36634, 7.999999999999998224, 2.000000000000000000 ) ;
#50350 = CARTESIAN_POINT ( 'NONE',  ( 12.64023069600374960, -4.285714285714294469, -21.88880945939638067 ) ) ;
#50351 = CYLINDRICAL_SURFACE ( 'NONE', #77067, 1.250000000000001110 ) ;
#50352 = DIRECTION ( 'NONE',  ( 0.000000000000000000, -1.000000000000000000, 0.000000000000000000 ) ) ;
#50353 = CARTESIAN_POINT ( 'NONE',  ( 4.898587196589412829E-16, -18.12499999999999645, -8.000000000000000000 ) ) ;
#50354 = DIRECTION ( 'NONE',  ( 0.000000000000000000, 1.000000000000000000, 0.000000000000000000 ) ) ;
#50355 = ORIENTED_EDGE ( 'NONE', *, *, #69207, .F. ) ;
#50356 = CARTESIAN_POINT ( 'NONE',  ( -7.121430446200055719, 40.29466789218744083, -71.00332351295398325 ) ) ;
#50357 = PRESENTATION_LAYER_ASSIGNMENT (  '', '', ( #67560 ) ) ;
#50359 = CARTESIAN_POINT ( 'NONE',  ( 33.11060381627214610, -49.89861181656793576, 36.32314459125598916 ) ) ;
#50358 = SURFACE_STYLE_USAGE ( .BOTH. , #84344 ) ;
#50360 = CARTESIAN_POINT ( 'NONE',  ( 35.48551685587499804, 424.7621062603631685, 6.304300610002332661 ) ) ;
#50361 = VERTEX_POINT ( 'NONE', #38625 ) ;
#50362 = CARTESIAN_POINT ( 'NONE',  ( -0.3597645216197892792, 13.03473291421858704, 51.69869386382899989 ) ) ;
#50364 = EDGE_CURVE ( 'NONE', #69148, #27394, #23445, .T. ) ;
#50363 = B_SPLINE_CURVE_WITH_KNOTS ( 'NONE', 3,
 ( #16855, #49736, #13517, #44315, #94471, #60519, #36268, #95008, #69135, #102008, #52932, #28167, #46437, #12457, #103087, #12983, #3321, #86913, #61043, #103605, #85858, #20087, #93930, #68604, #44860, #21143, #45911, #70181, #62630, #78267, #79327, #61580, #87440, #29756, #77748, #45386, #69657, #4379 ),
 .UNSPECIFIED., .F., .F.,
 ( 4, 2, 2, 2, 1, 1, 1, 1, 1, 1, 1, 2, 2, 2, 2, 1, 1, 1, 1, 1, 1, 1, 2, 2, 2, 4 ),
 ( 0.000000000000000000, 0.2499999999998910316, 0.3749999999998364086, 0.4374999999998089306, 0.4687499999997950528, 0.4843749999997879474, 0.4921874999997842837, 0.4960937499997825628, 0.4980468749997818967, 0.4990234374997816746, 0.4995117187497816746, 0.4997558593747817302, 0.4999999999997817857, 0.6249999999998058220, 0.6874999999998179234, 0.7187499999998239186, 0.7343749999998269162, 0.7421874999998283595, 0.7460937499998292477, 0.7480468749998296918, 0.7490234374998299138, 0.7495117187498299138, 0.7497558593748300249, 0.7499999999998301359, 0.8749999999999150679, 1.000000000000000000 ),
 .UNSPECIFIED. ) ;
#50365 = ORIENTED_EDGE ( 'NONE', *, *, #51014, .F. ) ;
#50367 = CARTESIAN_POINT ( 'NONE',  ( 43.67170302692484540, 434.9885551707870945, 18.57290719901132547 ) ) ;
#50366 = CARTESIAN_POINT ( 'NONE',  ( 0.3194001229792603480, 3.115132258397520282, 7.999999999999996447 ) ) ;
#50368 = DIRECTION ( 'NONE',  ( 0.000000000000000000, -1.000000000000000000, 0.000000000000000000 ) ) ;
#50369 = CARTESIAN_POINT ( 'NONE',  ( -15.65658065573060931, 294.5586797367948861, -2.062307047882345312 ) ) ;
#50370 = CYLINDRICAL_SURFACE ( 'NONE', #98259, 5.000000000000002665 ) ;
#50371 = CARTESIAN_POINT ( 'NONE',  ( -37.40828998626499668, 463.5731143434641695, 19.60478905907894287 ) ) ;
#50372 = ORIENTED_EDGE ( 'NONE', *, *, #43901, .T. ) ;
#50373 = CARTESIAN_POINT ( 'NONE',  ( 92.73990332427236183, -59.99999999999999289, -6.443125037031961710 ) ) ;
#50374 = CARTESIAN_POINT ( 'NONE',  ( 32.89862776688910628, 464.9311084009901833, 10.99515925127345461 ) ) ;
#50375 = CARTESIAN_POINT ( 'NONE',  ( 0.000000000000000000, 300.0000000000000000, 9.936999415352289589 ) ) ;
#50376 = CARTESIAN_POINT ( 'NONE',  ( -47.50596275964301185, 17.89684634806518915, -14.46697959672336609 ) ) ;
#50377 = EDGE_CURVE ( 'NONE', #43629, #85509, #63434, .T. ) ;
#50378 = ORIENTED_EDGE ( 'NONE', *, *, #76130, .T. ) ;
#50379 = DIRECTION ( 'NONE',  ( 0.000000000000000000, 1.000000000000000000, 0.000000000000000000 ) ) ;
#50380 = ORIENTED_EDGE ( 'NONE', *, *, #84367, .F. ) ;
#50381 = VERTEX_POINT ( 'NONE', #56351 ) ;
#50382 = CARTESIAN_POINT ( 'NONE',  ( 7.343637806710344051, 82.55636878099383580, 3.177475076494672646 ) ) ;
#50383 = FACE_OUTER_BOUND ( 'NONE', #35222, .T. ) ;
#50384 = LINE ( 'NONE', #9386, #38553 ) ;
#50385 = DIRECTION ( 'NONE',  ( -0.000000000000000000, 1.000000000000000000, -0.000000000000000000 ) ) ;
#50386 = CARTESIAN_POINT ( 'NONE',  ( 86.98871639540843148, -60.17830634995334549, -5.043400601815899442 ) ) ;
#50387 = CIRCLE ( 'NONE', #59041, 5.000000000000002665 ) ;
#50388 = CARTESIAN_POINT ( 'NONE',  ( -40.84209758864429318, 312.5378719886987255, -5.789410655104530790 ) ) ;
#50389 = CARTESIAN_POINT ( 'NONE',  ( -16.94581198861071769, 304.5649023924335097, -10.06098255995172508 ) ) ;
#50390 = CARTESIAN_POINT ( 'NONE',  ( 12.49989493515518646, 18.64301898209307140, -36.27145154709465658 ) ) ;
#50391 = ORIENTED_EDGE ( 'NONE', *, *, #78918, .F. ) ;
#50392 = CARTESIAN_POINT ( 'NONE',  ( 6.499999999999999112, 2.227636940139142929, -0.2900584647821211615 ) ) ;
#50393 = ORIENTED_EDGE ( 'NONE', *, *, #43257, .T. ) ;
#50394 = CARTESIAN_POINT ( 'NONE',  ( 9.812626099621477138, 51.27376982094347824, -2.923931248734654709 ) ) ;
#50395 = CARTESIAN_POINT ( 'NONE',  ( 14.27307692307692299, 4.172000000000003261, 5.109226446042759579E-16 ) ) ;
#50397 = ORIENTED_EDGE ( 'NONE', *, *, #32887, .T. ) ;
#50396 = CARTESIAN_POINT ( 'NONE',  ( 5.856054662371438901, 51.27348195240095663, 8.398858895281488657 ) ) ;
#50398 = CARTESIAN_POINT ( 'NONE',  ( 76.47493250985364455, -53.37270521551824487, 138.8582642167188794 ) ) ;
#50399 = EDGE_CURVE ( 'NONE', #73528, #20871, #5182, .T. ) ;
#50400 = ORIENTED_EDGE ( 'NONE', *, *, #12497, .T. ) ;
#50401 = CARTESIAN_POINT ( 'NONE',  ( 17.50000000000002842, 50.00000000000000000, 63.82142195508322402 ) ) ;
#50402 = CARTESIAN_POINT ( 'NONE',  ( 7.188101187500000933, -25.06250000204838813, -2.977408999572650483 ) ) ;
#50403 = CARTESIAN_POINT ( 'NONE',  ( -83.13494729127086202, -57.67105474064026538, -28.32277909022158724 ) ) ;
#50404 = EDGE_CURVE ( 'NONE', #40876, #98370, #51898, .T. ) ;
#50405 = EDGE_LOOP ( 'NONE', ( #17405, #98050 ) ) ;
#50406 = DIRECTION ( 'NONE',  ( -0.000000000000000000, 0.000000000000000000, 1.000000000000000000 ) ) ;
#50407 = CARTESIAN_POINT ( 'NONE',  ( 106.4188425553138302, -60.15150696938596298, 177.5013719461561266 ) ) ;
#50408 = EDGE_CURVE ( 'NONE', #21504, #3430, #31238, .T. ) ;
#50409 = CARTESIAN_POINT ( 'NONE',  ( -36.49045618873069685, 28.04599723762765606, -12.86279510840584095 ) ) ;
#50410 = DIRECTION ( 'NONE',  ( -1.000000000000000000, -1.224606353822377258E-16, -0.000000000000000000 ) ) ;
#50411 = EDGE_CURVE ( 'NONE', #8490, #74905, #103858, .T. ) ;
#50412 = CARTESIAN_POINT ( 'NONE',  ( 3.313708498984762052, -25.90625000409676559, -8.000000000000000000 ) ) ;
#50413 = CARTESIAN_POINT ( 'NONE',  ( -2.094395098902661623, -3.000000000000000000, 8.000000000000000000 ) ) ;
#50414 = CARTESIAN_POINT ( 'NONE',  ( 9.989690267985817940, 246.0255558340508628, -0.5238310916885806634 ) ) ;
#50415 = AXIS2_PLACEMENT_3D ( 'NONE', #58184, #34492, #17221 ) ;
#50416 = CARTESIAN_POINT ( 'NONE',  ( -7.500000000000006217, 39.99999999999122480, -59.88032989330939415 ) ) ;
#50417 = LINE ( 'NONE', #9419, #38405 ) ;
#50418 = CARTESIAN_POINT ( 'NONE',  ( 9.999999999999998224, -15.00000000000000000, -9.999999999999998224 ) ) ;
#50420 = EDGE_CURVE ( 'NONE', #49600, #16458, #28613, .T. ) ;
#50419 = CARTESIAN_POINT ( 'NONE',  ( 51.88291765283140933, 153.1183258647170362, 182.1969486012845891 ) ) ;
#50421 = CARTESIAN_POINT ( 'NONE',  ( 0.000000000000000000, 15.00000000000000000, -9.999999999999998224 ) ) ;
#50422 = ORIENTED_EDGE ( 'NONE', *, *, #35288, .T. ) ;
#50423 = CARTESIAN_POINT ( 'NONE',  ( -13.00000000000003730, -65.00000000000000000, -4.000000000000002665 ) ) ;
#50424 = AXIS2_PLACEMENT_3D ( 'NONE', #76192, #10913, #70769 ) ;
#50425 = CARTESIAN_POINT ( 'NONE',  ( 4.268270791835775846, -59.99999999999998579, 39.63076618222462599 ) ) ;
#50426 = CARTESIAN_POINT ( 'NONE',  ( -84.52869890352867799, -29.99999999999999289, 165.8509777010769426 ) ) ;
#50427 = ORIENTED_EDGE ( 'NONE', *, *, #66363, .T. ) ;
#50428 = CARTESIAN_POINT ( 'NONE',  ( 37.56673239365841255, 25.47613764497371136, -13.45617127781092215 ) ) ;
#50429 =( GEOMETRIC_REPRESENTATION_CONTEXT ( 3 ) GLOBAL_UNCERTAINTY_ASSIGNED_CONTEXT ( ( #83800 ) ) GLOBAL_UNIT_ASSIGNED_CONTEXT ( ( #3972, #43889, #70304 ) ) REPRESENTATION_CONTEXT ( 'NONE', 'WORKASPACE' ) );
#50430 = CARTESIAN_POINT ( 'NONE',  ( 71.20881682316100125, -57.68098021455711688, 164.2442580483489962 ) ) ;
#50432 = CARTESIAN_POINT ( 'NONE',  ( 7.000000000000000000, 0.000000000000000000, -13.00000000000000000 ) ) ;
#50431 = DIRECTION ( 'NONE',  ( -1.000000000000000000, 0.000000000000000000, 0.000000000000000000 ) ) ;
#50433 = B_SPLINE_CURVE_WITH_KNOTS ( 'NONE', 3,
 ( #66287, #74891, #58194, #33958, #66829, #69491, #19391, #2070, #61409, #67886, #93763, #59277, #2608, #34500, #43608, #100246, #85134, #26411, #76500, #28528, #94300, #9629, #52223, #60874, #93229, #19920, #26938, #101843, #10694, #27476, #59811, #11224, #18297, #35558, #44151, #92152 ),
 .UNSPECIFIED., .F., .F.,
 ( 4, 2, 2, 2, 2, 2, 2, 2, 2, 2, 2, 2, 2, 2, 2, 2, 2, 4 ),
 ( 0.01291936762762757943, 0.01372441420841338973, 0.01452946078919920003, 0.01533450736998500860, 0.01613955395077081717, 0.01694460053155662921, 0.01774964711234243778, 0.01855469369312824635, 0.01935974027391405838, 0.02016478685469987042, 0.02096983343548567899, 0.02177488001627148756, 0.02257992659705729960, 0.02338497317784310817, 0.02419001975862891674, 0.02459254304902182275, 0.02499506633941472877, 0.02580011292020053734 ),
 .UNSPECIFIED. ) ;
#50434 = CARTESIAN_POINT ( 'NONE',  ( 12.43520736934317483, -23.27680199471840439, -38.53969105432245357 ) ) ;
#50435 = CARTESIAN_POINT ( 'NONE',  ( 84.15356149169568312, 1.016364837396684119E-14, 0.000000000000000000 ) ) ;
#50436 = CYLINDRICAL_SURFACE ( 'NONE', #51238, 1.250000000000001110 ) ;
#50437 = CARTESIAN_POINT ( 'NONE',  ( -47.25096821319525731, -60.00000000000000711, 65.33942938962390201 ) ) ;
#50438 = CARTESIAN_POINT ( 'NONE',  ( -31.71529466845016998, 439.7354232657903594, 23.74396842416312836 ) ) ;
#50439 = CARTESIAN_POINT ( 'NONE',  ( 11.08349330513380515, -4.000000000000000888, 4.898587196589416773E-16 ) ) ;
#50440 = CARTESIAN_POINT ( 'NONE',  ( -85.55236343420649803, -61.06994240337794366, 193.9676891635616585 ) ) ;
#50441 = VERTEX_POINT ( 'NONE', #6216 ) ;
#50442 = FACE_OUTER_BOUND ( 'NONE', #96301, .T. ) ;
#50443 = CARTESIAN_POINT ( 'NONE',  ( -6.142256572465674580, -46.43922209401467427, 31.61959343549931845 ) ) ;
#50444 = FACE_OUTER_BOUND ( 'NONE', #89464, .T. ) ;
#50445 = FILL_AREA_STYLE_COLOUR ( '', #61456 ) ;
#50446 = AXIS2_PLACEMENT_3D ( 'NONE', #86556, #12614, #87598 ) ;
#50448 = CARTESIAN_POINT ( 'NONE',  ( 2.760661874148076844, -69.15507977559171593, 12.98220749377402683 ) ) ;
#50447 = CARTESIAN_POINT ( 'NONE',  ( -37.51894975547678968, 308.4495690710303961, 5.152636288847776136 ) ) ;
#50449 = EDGE_CURVE ( 'NONE', #96436, #91320, #72033, .T. ) ;
#50450 = EDGE_LOOP ( 'NONE', ( #92055, #11538, #80828, #21119, #33770 ) ) ;
#50451 = DIRECTION ( 'NONE',  ( 0.000000000000000000, 0.000000000000000000, -1.000000000000000000 ) ) ;
#50452 = CARTESIAN_POINT ( 'NONE',  ( -9.313960278265176029, -5.000000000000103029, -17.95852857499287225 ) ) ;
#50453 = CARTESIAN_POINT ( 'NONE',  ( 15.67156894839903991, 34.65681240932962481, 23.70584078379189563 ) ) ;
#50454 = AXIS2_PLACEMENT_3D ( 'NONE', #7952, #24185, #83978 ) ;
#50455 = CARTESIAN_POINT ( 'NONE',  ( 34.83065384313196944, 301.2489324959578880, -8.560106014107077499 ) ) ;
#50456 = EDGE_CURVE ( 'NONE', #45240, #103131, #40186, .T. ) ;
#50457 = FACE_OUTER_BOUND ( 'NONE', #86721, .T. ) ;
#50458 = SURFACE_STYLE_USAGE ( .BOTH. , #84977 ) ;
#50459 = CARTESIAN_POINT ( 'NONE',  ( 10.59999999999999609, 1.533819458162526451E-15, 0.000000000000000000 ) ) ;
#50460 = CARTESIAN_POINT ( 'NONE',  ( 109.0466504562702141, -30.00000000000000355, 159.8086616330221830 ) ) ;
#50461 = CARTESIAN_POINT ( 'NONE',  ( -81.74677077760871668, -42.97261976273406958, 163.6235584250746058 ) ) ;
#50462 = ORIENTED_EDGE ( 'NONE', *, *, #69210, .T. ) ;
#50463 = DIRECTION ( 'NONE',  ( -1.000000000000000000, -0.000000000000000000, -0.000000000000000000 ) ) ;
#50464 = CARTESIAN_POINT ( 'NONE',  ( -9.333555687487638863, 251.7810269660895699, 3.591168747312683429 ) ) ;
#50465 = FACE_OUTER_BOUND ( 'NONE', #37786, .T. ) ;
#50466 = LINE ( 'NONE', #59655, #75116 ) ;
#50467 = DIRECTION ( 'NONE',  ( 0.000000000000000000, -1.000000000000000000, 0.000000000000000000 ) ) ;
#50468 = ORIENTED_EDGE ( 'NONE', *, *, #66784, .T. ) ;
#50469 = UNCERTAINTY_MEASURE_WITH_UNIT (LENGTH_MEASURE( 1.000000000000000082E-05 ), #4783, 'distance_accuracy_value', 'NONE');
#50470 = CARTESIAN_POINT ( 'NONE',  ( -20.08590916391416314, 304.8421219133190903, 8.934941684170844667 ) ) ;
#50471 = ORIENTED_EDGE ( 'NONE', *, *, #23404, .T. ) ;
#50473 = DIRECTION ( 'NONE',  ( 1.000000000000000000, 0.000000000000000000, 0.000000000000000000 ) ) ;
#50472 =( BOUNDED_CURVE ( )  B_SPLINE_CURVE ( 2, ( #19111, #26144, #58999, #84864, #75698, #26661, #100504, #59540, #51949 ),
 .UNSPECIFIED., .F., .F. ) 
 B_SPLINE_CURVE_WITH_KNOTS ( ( 3, 2, 2, 2, 3 ),
 ( 0.6029411764705882026, 0.6102941176470588758, 0.6176470588235294379, 0.6250000000000000000, 0.6323529411764705621 ),
 .UNSPECIFIED. ) 
 CURVE ( )  GEOMETRIC_REPRESENTATION_ITEM ( )  RATIONAL_B_SPLINE_CURVE ( ( 1.000000000000000000, 0.9238795325112867385, 1.000000000000000000, 0.9238795325112867385, 1.000000000000000000, 0.9238795325112867385, 1.000000000000000000, 0.9238795325112867385, 1.000000000000000000 ) ) 
 REPRESENTATION_ITEM ( '' )  );
#50474 = CARTESIAN_POINT ( 'NONE',  ( -13.50000000000000000, 7.794228634059985339, -11.79422863405993382 ) ) ;
#50475 = CARTESIAN_POINT ( 'NONE',  ( 12.33349330513380693, -3.851859888774471706E-31, 4.000000000000001776 ) ) ;
#50476 = CARTESIAN_POINT ( 'NONE',  ( -52.56483885390515809, 48.00000000000000000, -38.23529411764715036 ) ) ;
#50477 = DIRECTION ( 'NONE',  ( 0.000000000000000000, -1.000000000000000000, 0.000000000000000000 ) ) ;
#50478 = CARTESIAN_POINT ( 'NONE',  ( 0.000000000000000000, 4.898587196589412829E-16, -4.000000000000000000 ) ) ;
#50479 = ORIENTED_EDGE ( 'NONE', *, *, #106183, .F. ) ;
#50480 = CARTESIAN_POINT ( 'NONE',  ( 111.0015139017943540, -60.00000000000001421, 187.3024812079267463 ) ) ;
#50482 = CARTESIAN_POINT ( 'NONE',  ( 16.95927991814305003, -49.91546993179999703, 32.46382548788433553 ) ) ;
#50481 = CARTESIAN_POINT ( 'NONE',  ( -71.28683113122063730, -60.00000000000007816, 168.6212938583825292 ) ) ;
#50483 = CARTESIAN_POINT ( 'NONE',  ( 83.17034439044972771, -37.99999999999994316, -9.670047016417147034 ) ) ;
#50484 = DIRECTION ( 'NONE',  ( -1.000000000000000000, -0.000000000000000000, -0.000000000000000000 ) ) ;
#50485 = CARTESIAN_POINT ( 'NONE',  ( -40.48299353324593852, -22.23726300500976194, 35.13222277374845248 ) ) ;
#50486 = ADVANCED_FACE ( 'NONE', ( #55812 ), #98422, .F. ) ;
#50487 = CARTESIAN_POINT ( 'NONE',  ( 82.42421628608209971, 1.030564683017419500E-14, 0.000000000000000000 ) ) ;
#50488 = ORIENTED_EDGE ( 'NONE', *, *, #4535, .F. ) ;
#50489 = CARTESIAN_POINT ( 'NONE',  ( 8.929771841637641927, 1.482358050883964840E-15, 0.000000000000000000 ) ) ;
#50490 = CARTESIAN_POINT ( 'NONE',  ( 8.239113808047395793, 53.79488085724082680, 3.999741343929974935 ) ) ;
#50491 = CARTESIAN_POINT ( 'NONE',  ( 39.84233570596349949, 333.3323931548420660, 19.23895789620553032 ) ) ;
#50492 = AXIS2_PLACEMENT_3D ( 'NONE', #9308, #101919, #66498 ) ;
#50493 = SURFACE_STYLE_FILL_AREA ( #33827 ) ;
#50494 = CARTESIAN_POINT ( 'NONE',  ( 6.585468679846621320, 3.617797563910810865, 6.733790807807553236 ) ) ;
#50495 = CARTESIAN_POINT ( 'NONE',  ( 8.559508646656407649, 53.68473964988125857, 4.031152949374444461 ) ) ;
#50496 = ORIENTED_EDGE ( 'NONE', *, *, #4287, .F. ) ;
#50497 = EDGE_CURVE ( 'NONE', #60656, #24664, #67175, .T. ) ;
#50498 = ORIENTED_EDGE ( 'NONE', *, *, #42157, .T. ) ;
#50499 = CARTESIAN_POINT ( 'NONE',  ( 81.49414201415379466, -30.00000000000006040, -9.315152446787697826 ) ) ;
#50500 = CARTESIAN_POINT ( 'NONE',  ( 18.56873304867848162, 41.90421603127634853, -81.65074648123847112 ) ) ;
#50501 = UNCERTAINTY_MEASURE_WITH_UNIT (LENGTH_MEASURE( 1.000000000000000082E-05 ), #65367, 'distance_accuracy_value', 'NONE');
#50502 = DIRECTION ( 'NONE',  ( 0.8191520442889900222, 0.000000000000000000, 0.5735764363510486019 ) ) ;
#50503 = CARTESIAN_POINT ( 'NONE',  ( 4.999999999999999112, 5.773502691896258199, -7.063244554130000630 ) ) ;
#50504 = CARTESIAN_POINT ( 'NONE',  ( 80.95415150621239775, -30.00000000000000000, 4.843109486027489474 ) ) ;
#50505 = AXIS2_PLACEMENT_3D ( 'NONE', #21199, #86972, #62689 ) ;
#50506 = SURFACE_SIDE_STYLE ('',( #76382 ) ) ;
#50507 = ADVANCED_FACE ( 'NONE', ( #83302 ), #85441, .T. ) ;
#50508 = ORIENTED_EDGE ( 'NONE', *, *, #90266, .T. ) ;
#50509 = VERTEX_POINT ( 'NONE', #2905 ) ;
#50510 = EDGE_LOOP ( 'NONE', ( #58088, #62543, #93313, #7517 ) ) ;
#50511 = CARTESIAN_POINT ( 'NONE',  ( -31.99602169361977388, 464.8336097802194331, 12.51960734453166957 ) ) ;
#50512 = LINE ( 'NONE', #25779, #56155 ) ;
#50513 = AXIS2_PLACEMENT_3D ( 'NONE', #33320, #7410, #106102 ) ;
#50514 = CARTESIAN_POINT ( 'NONE',  ( 5.475947152006327201, -13.16217730109125306, 2.462898245435121591 ) ) ;
#50515 = CARTESIAN_POINT ( 'NONE',  ( -31.13164573599167184, 436.9142555170884066, 23.68610392534201736 ) ) ;
#50516 = ORIENTED_EDGE ( 'NONE', *, *, #73604, .F. ) ;
#50517 = ORIENTED_EDGE ( 'NONE', *, *, #48161, .T. ) ;
#50518 = PLANE ( 'NONE',  #79433 ) ;
#50519 = CARTESIAN_POINT ( 'NONE',  ( 74.67842920201081824, -38.33200830287892558, 166.4539110603844279 ) ) ;
#50520 = CARTESIAN_POINT ( 'NONE',  ( 33.21583695390473423, 487.8294359878499336, 10.09122741357699304 ) ) ;
#50521 = CARTESIAN_POINT ( 'NONE',  ( 27.27586408842989130, 307.4943522527414075, 11.01523124013777100 ) ) ;
#50522 = CARTESIAN_POINT ( 'NONE',  ( -5.855777637195783925, 246.2189350324153736, -1.331220292256674043 ) ) ;
#50523 = AXIS2_PLACEMENT_3D ( 'NONE', #34939, #59729, #1451 ) ;
#50524 = ORIENTED_EDGE ( 'NONE', *, *, #22418, .T. ) ;
#50525 = CARTESIAN_POINT ( 'NONE',  ( -27.42597638825734663, 34.37175190012616355, -10.02588870074117366 ) ) ;
#50526 = DIRECTION ( 'NONE',  ( 1.000000000000000000, -0.000000000000000000, -0.000000000000000000 ) ) ;
#50527 = CARTESIAN_POINT ( 'NONE',  ( 40.02592568779148507, 1.482358050883964840E-15, 0.000000000000000000 ) ) ;
#50528 = ADVANCED_FACE ( 'NONE', ( #61172 ), #10994, .T. ) ;
#50529 = MECHANICAL_DESIGN_GEOMETRIC_PRESENTATION_REPRESENTATION (  '', ( #9175 ), #74631 ) ;
#50530 = CARTESIAN_POINT ( 'NONE',  ( 14.97192734824148808, 2.056257465146328567, 0.8331214207672043015 ) ) ;
#50532 = EDGE_LOOP ( 'NONE', ( #14670, #17349, #36936, #14727 ) ) ;
#50531 =( GEOMETRIC_REPRESENTATION_CONTEXT ( 3 ) GLOBAL_UNCERTAINTY_ASSIGNED_CONTEXT ( ( #65645 ) ) GLOBAL_UNIT_ASSIGNED_CONTEXT ( ( #94094, #85479, #86561 ) ) REPRESENTATION_CONTEXT ( 'NONE', 'WORKASPACE' ) );
#50533 = CARTESIAN_POINT ( 'NONE',  ( -24.05303310288100604, 295.4586947108799109, 10.06705650746367375 ) ) ;
#50534 = LINE ( 'NONE', #19316, #86755 ) ;
#50535 = CARTESIAN_POINT ( 'NONE',  ( -5.335963852939137553, -6.035591050534815594, -7.593821156097424918 ) ) ;
#50536 = CARTESIAN_POINT ( 'NONE',  ( 33.84761347220244687, 488.7471039746337738, 11.01988148152553748 ) ) ;
#50537 = EDGE_CURVE ( 'NONE', #12701, #11751, #69104, .T. ) ;
#50538 = CARTESIAN_POINT ( 'NONE',  ( 1.917245519677769350, 301.4538546725594870, 9.817117674984364939 ) ) ;
#50539 = CARTESIAN_POINT ( 'NONE',  ( 89.93133926947346879, 1.016364837396684119E-14, 0.000000000000000000 ) ) ;
#50540 = CARTESIAN_POINT ( 'NONE',  ( 86.30666900314933798, -21.08433947227320360, 179.9884049068863305 ) ) ;
#50541 = CARTESIAN_POINT ( 'NONE',  ( 16.83415698846517117, 37.10146012410931604, -21.80698433968623817 ) ) ;
#50542 = SURFACE_SIDE_STYLE ('',( #40878 ) ) ;
#50543 = ORIENTED_EDGE ( 'NONE', *, *, #103826, .F. ) ;
#50544 = CARTESIAN_POINT ( 'NONE',  ( 83.09486208724929668, -57.67107040063709888, -28.34176565233813250 ) ) ;
#50545 = EDGE_CURVE ( 'NONE', #33697, #21252, #96782, .T. ) ;
#50546 = DIRECTION ( 'NONE',  ( 0.000000000000000000, -1.000000000000000000, 0.000000000000000000 ) ) ;
#50547 = CARTESIAN_POINT ( 'NONE',  ( -0.5219667817988858927, 7.204195837485517728, -0.5602453477493318790 ) ) ;
#50548 = CARTESIAN_POINT ( 'NONE',  ( 0.2573354458087814822, 4.368923434677189022, 5.432802636760777126 ) ) ;
#50549 = CARTESIAN_POINT ( 'NONE',  ( -81.40926587446145390, -30.00000000000000000, -9.992568410953589719 ) ) ;
#50550 = CARTESIAN_POINT ( 'NONE',  ( 40.11650669486618881, -3.851859888774471706E-31, 4.000000000000000888 ) ) ;
#50551 = LINE ( 'NONE', #42477, #85915 ) ;
#50552 = DIRECTION ( 'NONE',  ( 0.000000000000000000, 1.000000000000000000, 0.000000000000000000 ) ) ;
#50553 = CARTESIAN_POINT ( 'NONE',  ( -9.220915120640610141, 248.9554511356789988, -3.870126578504832437 ) ) ;
#50554 = CARTESIAN_POINT ( 'NONE',  ( -17.49999999999996803, 47.99999999999997868, 64.09949417230998847 ) ) ;
#50555 = LINE ( 'NONE', #49510, #71169 ) ;
#50556 = CARTESIAN_POINT ( 'NONE',  ( -30.00000000000000000, 1.347111479062088405E-15, 11.00000000000000000 ) ) ;
#50557 = CARTESIAN_POINT ( 'NONE',  ( 4.521127550501229386, -84.32389759472334845, 3.944701057164354818 ) ) ;
#50558 = DIRECTION ( 'NONE',  ( 0.9230641662213218135, 0.000000000000000000, 0.3846459996388055247 ) ) ;
#50559 = CARTESIAN_POINT ( 'NONE',  ( 26.11923076923076792, -4.171999999999999709, 5.616230220889763424E-16 ) ) ;
#50560 = AXIS2_PLACEMENT_3D ( 'NONE', #46611, #79507, #30996 ) ;
#50561 = CARTESIAN_POINT ( 'NONE',  ( -98.86074489839170099, -37.99999999999991473, 192.0568120749455829 ) ) ;
#50562 = ORIENTED_EDGE ( 'NONE', *, *, #87114, .T. ) ;
#50563 = CARTESIAN_POINT ( 'NONE',  ( 6.879475648205856331, 9.213907405080439261, -1.316666052250857977 ) ) ;
#50564 = PRESENTATION_STYLE_ASSIGNMENT (( #17705 ) ) ;
#50565 = FACE_OUTER_BOUND ( 'NONE', #5880, .T. ) ;
#50566 = CARTESIAN_POINT ( 'NONE',  ( -38.67654687014966441, -24.46767789941978677, -30.56595494665695512 ) ) ;
#50568 = CARTESIAN_POINT ( 'NONE',  ( -43.00000000000000000, 500.0000000000002274, 0.000000000000000000 ) ) ;
#50567 = DIRECTION ( 'NONE',  ( 0.8191520442889974607, 1.003171929053531649E-16, -0.5735764363510380548 ) ) ;
#50569 = EDGE_CURVE ( 'NONE', #33011, #288, #103280, .T. ) ;
#50570 = ORIENTED_EDGE ( 'NONE', *, *, #62176, .F. ) ;
#50571 = CARTESIAN_POINT ( 'NONE',  ( -14.62196857730996946, 42.00000000000000711, -88.48477568205504440 ) ) ;
#50572 = ORIENTED_EDGE ( 'NONE', *, *, #95294, .T. ) ;
#50573 = CYLINDRICAL_SURFACE ( 'NONE', #79247, 4.000000000000000000 ) ;
#50574 = ADVANCED_FACE ( 'NONE', ( #96716 ), #105333, .F. ) ;
#50575 = CARTESIAN_POINT ( 'NONE',  ( 16.02742720722318026, 4.186773460852821316, 2.547561848287669850 ) ) ;
#50576 = CARTESIAN_POINT ( 'NONE',  ( -51.17622358944377936, -60.00000000000000000, -37.67033473011792211 ) ) ;
#50577 = ORIENTED_EDGE ( 'NONE', *, *, #37314, .T. ) ;
#50578 =( LENGTH_UNIT ( ) NAMED_UNIT ( * ) SI_UNIT ( .MILLI., .METRE. ) );
#50579 = CARTESIAN_POINT ( 'NONE',  ( 15.46209624076536038, 2.722175477912782249, 1.608330402076072474 ) ) ;
#50580 = CARTESIAN_POINT ( 'NONE',  ( 103.0186286448298745, -60.16906176935165007, 192.8004402776240340 ) ) ;
#50582 = CARTESIAN_POINT ( 'NONE',  ( -46.81343110146983122, 13.24251555485282239, 15.91224400466310307 ) ) ;
#50581 = DIRECTION ( 'NONE',  ( -0.000000000000000000, 1.000000000000000000, -0.000000000000000000 ) ) ;
#50583 = ORIENTED_EDGE ( 'NONE', *, *, #32011, .F. ) ;
#50584 = CIRCLE ( 'NONE', #91959, 4.250000000000000000 ) ;
#50585 = ORIENTED_EDGE ( 'NONE', *, *, #55931, .F. ) ;
#50586 = ORIENTED_EDGE ( 'NONE', *, *, #76568, .F. ) ;
#50587 = CARTESIAN_POINT ( 'NONE',  ( 31.36030843854360128, 339.5225620909950521, 18.44549848323119434 ) ) ;
#50588 = AXIS2_PLACEMENT_3D ( 'NONE', #87712, #4669, #104403 ) ;
#50589 = DIRECTION ( 'NONE',  ( 0.000000000000000000, -1.000000000000000000, 0.000000000000000000 ) ) ;
#50590 = CARTESIAN_POINT ( 'NONE',  ( 15.39661048887591299, 46.16593794825683261, 5.596966726905939105 ) ) ;
#50591 = EDGE_LOOP ( 'NONE', ( #72662, #97293, #89883, #5127 ) ) ;
#50592 = STYLED_ITEM ( 'NONE', ( #65289 ), #48600 ) ;
#50593 = DIRECTION ( 'NONE',  ( -1.000000000000000000, 0.000000000000000000, 0.000000000000000000 ) ) ;
#50594 = CARTESIAN_POINT ( 'NONE',  ( 6.289812543865802574, 6.246946743711088601, 2.837966828325882318 ) ) ;
#50595 = AXIS2_PLACEMENT_3D ( 'NONE', #8620, #39943, #72298 ) ;
#50596 = DIRECTION ( 'NONE',  ( 0.000000000000000000, 0.000000000000000000, -1.000000000000000000 ) ) ;
#50597 = CARTESIAN_POINT ( 'NONE',  ( -69.31411742845799040, -57.68241165371757262, 149.3509116208381329 ) ) ;
#50598 = CARTESIAN_POINT ( 'NONE',  ( 4.401442555609581635E-16, -32.28125000204838813, -7.188101187500000044 ) ) ;
#50599 = CARTESIAN_POINT ( 'NONE',  ( -30.06732394248810536, 17.62925877149443821, 39.66393268825138563 ) ) ;
#50600 = CARTESIAN_POINT ( 'NONE',  ( -31.19652432992544888, 378.3327707670021027, 24.28948218791313707 ) ) ;
#50601 = CARTESIAN_POINT ( 'NONE',  ( -6.955654383127702012, 41.30888465058240655, -58.54627983348873244 ) ) ;
#50602 = CARTESIAN_POINT ( 'NONE',  ( -89.36642547188127139, -29.99999999999995381, 5.438168021589780743 ) ) ;
#50603 = CARTESIAN_POINT ( 'NONE',  ( -49.32002684479864740, -39.51885134585224080, 49.64505812268525631 ) ) ;
#50604 = DIRECTION ( 'NONE',  ( 0.000000000000000000, 0.000000000000000000, -1.000000000000000000 ) ) ;
#50605 = ORIENTED_EDGE ( 'NONE', *, *, #29997, .T. ) ;
#50606 = CARTESIAN_POINT ( 'NONE',  ( -97.07210653995934990, -60.35970870470556093, 196.7639714328392415 ) ) ;
#50607 = CARTESIAN_POINT ( 'NONE',  ( -8.849035312365487016, 302.6218124189194896, -10.03679229143247476 ) ) ;
#50608 = CARTESIAN_POINT ( 'NONE',  ( 11.81783007639908334, -1.930264526412683868, 20.62761066482512717 ) ) ;
#50609 = EDGE_LOOP ( 'NONE', ( #68328, #532, #78571, #102092, #60976, #76999 ) ) ;
#50610 = CARTESIAN_POINT ( 'NONE',  ( 44.14911905790283697, 464.3766534542007207, 9.623404994951284763 ) ) ;
#50611 = CARTESIAN_POINT ( 'NONE',  ( 100.5869678965343610, -38.46297986693701887, 200.3470908674215707 ) ) ;
#50612 = SURFACE_STYLE_USAGE ( .BOTH. , #17756 ) ;
#50613 = CARTESIAN_POINT ( 'NONE',  ( -6.510243396850508901, 51.36750486090217294, -7.564727007839853634 ) ) ;
#50614 = CARTESIAN_POINT ( 'NONE',  ( -16.93833563167039458, 302.5835715773326910, 9.880235389495441112 ) ) ;
#50615 = CARTESIAN_POINT ( 'NONE',  ( -23.70422451874885184, 42.00000000000000000, -88.20421627933662023 ) ) ;
#50616 = CARTESIAN_POINT ( 'NONE',  ( 87.06605025660013553, -30.00000000000000000, 183.9618747148463740 ) ) ;
#50617 = B_SPLINE_SURFACE_WITH_KNOTS ( 'NONE', 1, 3, ( 
 ( #41236, #42294, #66045, #98922, #737, #25081, #90861, #33701 ),
 ( #99459, #34246, #58496, #1280, #88481, #19672, #6474, #46938 ) ),
 .UNSPECIFIED., .F., .F., .F.,
 ( 2, 2 ),
 ( 4, 2, 2, 4 ),
 ( 0.000000000000000000, 1.000000000000000000 ),
 ( 0.000000000000000000, 0.04450745600790868145, 0.06676118401186306728, 0.08901491201581737678 ),
 .UNSPECIFIED. ) ;
#50618 = LINE ( 'NONE', #9637, #64812 ) ;
#50619 = CARTESIAN_POINT ( 'NONE',  ( -29.08094203968506974, 13.68582110885884440, 39.75724343093563107 ) ) ;
#50620 = CARTESIAN_POINT ( 'NONE',  ( 0.000000000000000000, 0.000000000000000000, -10.00000000000000000 ) ) ;
#50621 = CONICAL_SURFACE ( 'NONE', #4159, 6.500000000000000000, 1.047197551196600296 ) ;
#50622 = VERTEX_POINT ( 'NONE', #39553 ) ;
#50623 = EDGE_LOOP ( 'NONE', ( #16052, #73006, #96094, #61878, #7722 ) ) ;
#50624 = CARTESIAN_POINT ( 'NONE',  ( 51.52558495347906131, -32.57909100336876662, 50.96452728205734672 ) ) ;
#50625 = CARTESIAN_POINT ( 'NONE',  ( 7.126148245860624009, 41.12758397993106030, -58.55282951229288102 ) ) ;
#50626 = CARTESIAN_POINT ( 'NONE',  ( 37.40728451038606295, 27.65912829610039125, -13.45617127781095590 ) ) ;
#50627 = ORIENTED_EDGE ( 'NONE', *, *, #36258, .T. ) ;
#50628 = CARTESIAN_POINT ( 'NONE',  ( -110.5377068114738108, -38.35610058096415287, 161.0159699682552343 ) ) ;
#50629 = ORIENTED_EDGE ( 'NONE', *, *, #100634, .T. ) ;
#50630 = CARTESIAN_POINT ( 'NONE',  ( 5.656854249492380582, -29.00000000409677270, -5.656854249492379694 ) ) ;
#50631 = CARTESIAN_POINT ( 'NONE',  ( 110.2494631951638127, -38.35601185217798559, 184.3351315308087806 ) ) ;
#50632 = CARTESIAN_POINT ( 'NONE',  ( 14.98461734045173088, 22.22601645454860986, -3.898224806824892141 ) ) ;
#50633 = CARTESIAN_POINT ( 'NONE',  ( 86.15997024733299270, -37.84900569248561908, 53.97426573764452229 ) ) ;
#50634 = CARTESIAN_POINT ( 'NONE',  ( 0.000000000000000000, -30.00000000000000000, 0.000000000000000000 ) ) ;
#50635 = CARTESIAN_POINT ( 'NONE',  ( -21.67644693109840048, 305.0488537841421248, -8.958167403557810715 ) ) ;
#50636 = CARTESIAN_POINT ( 'NONE',  ( 76.19063985184907040, -60.00000000000000000, 187.7640617696651191 ) ) ;
#50637 = CARTESIAN_POINT ( 'NONE',  ( 5.902907888931476776, -4.999999999999999112, -73.20788160635341058 ) ) ;
#50638 = CARTESIAN_POINT ( 'NONE',  ( -44.19123973042153608, 435.3640897803193184, 10.85603094147129788 ) ) ;
#50639 = ORIENTED_EDGE ( 'NONE', *, *, #95545, .F. ) ;
#50640 = CARTESIAN_POINT ( 'NONE',  ( 59.90236492691475689, -49.91050096998650076, 76.94228515587644779 ) ) ;
#50641 = DIRECTION ( 'NONE',  ( 0.000000000000000000, -1.000000000000000000, 0.000000000000000000 ) ) ;
#50642 = EDGE_CURVE ( 'NONE', #103416, #40845, #34700, .T. ) ;
#50643 = CARTESIAN_POINT ( 'NONE',  ( -8.584127441494805666, -5.000000000000000000, -16.50953036925850981 ) ) ;
#50644 = B_SPLINE_CURVE_WITH_KNOTS ( 'NONE', 3,
 ( #15799, #24981, #39568, #63839, #104814, #30963 ),
 .UNSPECIFIED., .F., .F.,
 ( 4, 2, 4 ),
 ( 2.380731629579044207E-07, 0.002336973833157560739, 0.004673709593152165255 ),
 .UNSPECIFIED. ) ;
#50645 = CARTESIAN_POINT ( 'NONE',  ( -35.33914081917379946, 485.2455454566305093, -2.714404708513355580 ) ) ;
#50646 = CARTESIAN_POINT ( 'NONE',  ( -33.15386418467154073, 409.3216133033088227, 25.87705685211801310 ) ) ;
#50647 = FACE_OUTER_BOUND ( 'NONE', #89629, .T. ) ;
#50648 = CARTESIAN_POINT ( 'NONE',  ( 24.34999999999999787, -3.309499999999999886, 4.475777889183790779E-16 ) ) ;
#50649 = CARTESIAN_POINT ( 'NONE',  ( -5.656854249492379694, -29.93749999999999645, -5.656854249492380582 ) ) ;
#50650 = CARTESIAN_POINT ( 'NONE',  ( -22.24914325797420389, -18.02156853467999653, 31.43918858065762478 ) ) ;
#50651 = ADVANCED_FACE ( 'NONE', ( #62251 ), #63827, .T. ) ;
#50652 = CARTESIAN_POINT ( 'NONE',  ( 15.56598648174122346, 43.92012149713269054, -6.062017361296271112 ) ) ;
#50653 = ORIENTED_EDGE ( 'NONE', *, *, #77329, .T. ) ;
#50654 = CARTESIAN_POINT ( 'NONE',  ( 84.85119566129066015, -32.34994737913991258, 176.2922552301222936 ) ) ;
#50655 = CARTESIAN_POINT ( 'NONE',  ( -37.72538228492555135, 27.83011398562653227, 10.95617127781058464 ) ) ;
#50656 = CARTESIAN_POINT ( 'NONE',  ( -42.10086803841213765, 435.6552064019005570, 19.95582312411059789 ) ) ;
#50657 = EDGE_LOOP ( 'NONE', ( #43506, #56733, #87360, #87814 ) ) ;
#50658 = CARTESIAN_POINT ( 'NONE',  ( -21.04247164025376193, 37.86482112153537116, -10.52123582012687564 ) ) ;
#50659 = CONICAL_SURFACE ( 'NONE', #95506, 3.309500000000001663, 0.9599310885968770357 ) ;
#50660 = EDGE_CURVE ( 'NONE', #8292, #32226, #47850, .T. ) ;
#50661 = DIRECTION ( 'NONE',  ( 1.000000000000000000, 0.000000000000000000, 0.000000000000000000 ) ) ;
#50662 = FACE_OUTER_BOUND ( 'NONE', #40685, .T. ) ;
#50663 = CARTESIAN_POINT ( 'NONE',  ( -6.544091414552472230, -3.000000000000003109, -98.56434427383338459 ) ) ;
#50664 = CARTESIAN_POINT ( 'NONE',  ( -21.95063819072343492, -26.56093263958899087, -38.44887722113407591 ) ) ;
#50665 = CARTESIAN_POINT ( 'NONE',  ( -10.52454070266728792, -0.8718843809977038228, 20.23127905671319837 ) ) ;
#50666 = AXIS2_PLACEMENT_3D ( 'NONE', #90759, #83186, #75078 ) ;
#50667 = AXIS2_PLACEMENT_3D ( 'NONE', #59073, #44487, #18088 ) ;
#50669 = VECTOR ( 'NONE', #3198, 1000.000000000000000 ) ;
#50668 = SURFACE_STYLE_FILL_AREA ( #2125 ) ;
#50670 = CARTESIAN_POINT ( 'NONE',  ( 50.71755735396195774, -60.00000000000000711, 73.61387294642976542 ) ) ;
#50671 = DIRECTION ( 'NONE',  ( 1.000000000000000000, -0.000000000000000000, -0.000000000000000000 ) ) ;
#50672 = CARTESIAN_POINT ( 'NONE',  ( 1.787493240145907603, -12.60618723787961315, 32.17814028491976330 ) ) ;
#50674 = CARTESIAN_POINT ( 'NONE',  ( -13.08561955852094627, 23.85450803358479988, -4.082908960275540622 ) ) ;
#50673 = CARTESIAN_POINT ( 'NONE',  ( -20.54080512885244048, -26.05094486570658319, 36.94806580626582360 ) ) ;
#50675 = FACE_OUTER_BOUND ( 'NONE', #31830, .T. ) ;
#50676 = CARTESIAN_POINT ( 'NONE',  ( 45.29905483860081716, 480.9466865490944656, -2.171671249451534003 ) ) ;
#50677 = B_SPLINE_CURVE_WITH_KNOTS ( 'NONE', 3,
 ( #60860, #70001, #53806, #53290, #86735, #45213, #3681, #38197, #85668, #95879, #13869, #12810, #103429, #77566, #71057, #95341, #44679, #30094, #62450, #4206, #45724, #79677, #36086, #93750, #19902, #37135, #102902, #52745, #69478, #61936, #21477, #102363, #29066, #20972 ),
 .UNSPECIFIED., .F., .F.,
 ( 4, 2, 2, 2, 2, 2, 2, 2, 2, 2, 2, 2, 2, 2, 2, 2, 4 ),
 ( 0.000000000000000000, 0.06250000000000002776, 0.1250000000000000555, 0.1875000000000000555, 0.2500000000000000555, 0.3125000000000000000, 0.3750000000000000000, 0.4374999999999999445, 0.4999999999999999445, 0.5624999999999998890, 0.6249999999999997780, 0.6874999999999998890, 0.7499999999999998890, 0.8124999999999998890, 0.8749999999999998890, 0.9375000000000000000, 1.000000000000000000 ),
 .UNSPECIFIED. ) ;
#50678 = CARTESIAN_POINT ( 'NONE',  ( -1.000000000000000000, -69.59657292933731298, 12.76848391598547394 ) ) ;
#50679 = CARTESIAN_POINT ( 'NONE',  ( 4.324913936355947008, -1.111773959251803445, 104.4044995709989934 ) ) ;
#50680 = ORIENTED_EDGE ( 'NONE', *, *, #8120, .F. ) ;
#50681 = CARTESIAN_POINT ( 'NONE',  ( 4.540089413576434474, -21.58519901417236042, -38.54822756895638491 ) ) ;
#50682 = B_SPLINE_CURVE_WITH_KNOTS ( 'NONE', 3,
 ( #17827, #26476, #99788, #76039, #33481, #2136, #83595, #9701, #98707, #8113 ),
 .UNSPECIFIED., .F., .F.,
 ( 4, 2, 2, 2, 4 ),
 ( 0.000000000000000000, 0.002305503304226491201, 0.004611006608452982401, 0.006916509912679473168, 0.009222013216905966537 ),
 .UNSPECIFIED. ) ;
#50683 = CARTESIAN_POINT ( 'NONE',  ( -19.49662282918389877, 49.99981527065391873, 59.98277621002914373 ) ) ;
#50684 = CARTESIAN_POINT ( 'NONE',  ( -38.06522774901652184, 464.2393341908695561, 19.21804507436417353 ) ) ;
#50686 = CARTESIAN_POINT ( 'NONE',  ( 35.14719567999821948, -47.40883101621029994, -32.39563694789472237 ) ) ;
#50685 = CARTESIAN_POINT ( 'NONE',  ( -34.92499999999994742, 0.000000000000000000, 0.000000000000000000 ) ) ;
#50687 = EDGE_CURVE ( 'NONE', #17308, #21504, #5052, .T. ) ;
#50688 = AXIS2_PLACEMENT_3D ( 'NONE', #47708, #38592, #56860 ) ;
#50689 = EDGE_LOOP ( 'NONE', ( #58953, #27120, #31145, #66595 ) ) ;
#50690 = CARTESIAN_POINT ( 'NONE',  ( -5.650483388624518710, -88.45566596850385110, 2.031129859422142303 ) ) ;
#50691 = CARTESIAN_POINT ( 'NONE',  ( -4.884983410653892300, 51.44234778147703935, 8.466500073338718124 ) ) ;
#50692 = ORIENTED_EDGE ( 'NONE', *, *, #92792, .F. ) ;
#50693 = EDGE_CURVE ( 'NONE', #3187, #66199, #32989, .T. ) ;
#50694 = DIRECTION ( 'NONE',  ( -1.000000000000000000, -1.224606353822377258E-16, -0.000000000000000000 ) ) ;
#50695 = EDGE_CURVE ( 'NONE', #70219, #85144, #97227, .T. ) ;
#50696 = CARTESIAN_POINT ( 'NONE',  ( 30.00229752355648571, 12.60065794652348359, -39.63915577993689965 ) ) ;
#50697 = CARTESIAN_POINT ( 'NONE',  ( -19.44876292489749758, 41.87164991014802951, -80.45734961732209456 ) ) ;
#50698 = AXIS2_PLACEMENT_3D ( 'NONE', #58515, #81690, #24579 ) ;
#50699 = CARTESIAN_POINT ( 'NONE',  ( -95.01606930152259167, -59.99999999999999289, 49.16530457434027568 ) ) ;
#50700 = DIRECTION ( 'NONE',  ( -0.000000000000000000, 1.000000000000000000, -0.000000000000000000 ) ) ;
#50701 = DIRECTION ( 'NONE',  ( 0.000000000000000000, -1.000000000000000000, 0.000000000000000000 ) ) ;
#50702 = COLOUR_RGB ( '', 0.08235294, 0.09019608, 0.10196078) ;
#50703 = CARTESIAN_POINT ( 'NONE',  ( 31.19792890532719198, 414.2215770364159084, 25.44228638033458623 ) ) ;
#50705 = CARTESIAN_POINT ( 'NONE',  ( 40.87544524660111733, 460.0150911311816344, 2.035358705196582463 ) ) ;
#50704 = APPLICATION_CONTEXT ( 'automotive_design' ) ;
#50707 = CARTESIAN_POINT ( 'NONE',  ( -15.50036553200112444, 2.628019270336301449, -0.8101929630158405393 ) ) ;
#50706 = CARTESIAN_POINT ( 'NONE',  ( -2.617478844990611897, -3.000000000000002665, -75.26027323389583046 ) ) ;
#50708 = CARTESIAN_POINT ( 'NONE',  ( -80.87069194252994464, -60.49237983335919466, 182.4063684378278651 ) ) ;
#50709 = ORIENTED_EDGE ( 'NONE', *, *, #61966, .T. ) ;
#50710 = FILL_AREA_STYLE_COLOUR ( '', #47119 ) ;
#50711 = ORIENTED_EDGE ( 'NONE', *, *, #94630, .F. ) ;
#50712 = COLOUR_RGB ( '', 0.40784314, 0.44705882, 0.49803922) ;
#50713 = EDGE_LOOP ( 'NONE', ( #101531, #81544, #22298, #59834 ) ) ;
#50714 = CARTESIAN_POINT ( 'NONE',  ( -4.302760725356050919, -1.102344419738585879, 104.4121068519184945 ) ) ;
#50715 = CARTESIAN_POINT ( 'NONE',  ( 0.000000000000000000, 5.629165124598848102, 3.250000000000005329 ) ) ;
#50716 = ORIENTED_EDGE ( 'NONE', *, *, #31519, .T. ) ;
#50717 = EDGE_CURVE ( 'NONE', #91205, #81976, #103740, .T. ) ;
#50718 = CARTESIAN_POINT ( 'NONE',  ( 8.929771841637641927, 5.000000000000002665, 0.000000000000000000 ) ) ;
#50719 = SURFACE_STYLE_USAGE ( .BOTH. , #16787 ) ;
#50720 = DIRECTION ( 'NONE',  ( 0.000000000000000000, -1.000000000000000000, 0.000000000000000000 ) ) ;
#50721 = CARTESIAN_POINT ( 'NONE',  ( -7.801777176595948937, -61.41172014187367267, -1.786991866639924043 ) ) ;
#50722 = CARTESIAN_POINT ( 'NONE',  ( -0.4142949201392615577, 54.27908600331601718, 7.817690266341844385 ) ) ;
#50723 = CARTESIAN_POINT ( 'NONE',  ( -13.87268571384243465, -50.40938940377537847, 28.89968788215285755 ) ) ;
#50724 = CARTESIAN_POINT ( 'NONE',  ( -97.47674776263787066, -60.00000000000000000, 196.6139650356533934 ) ) ;
#50725 = CARTESIAN_POINT ( 'NONE',  ( 88.56622727954015772, -14.21045842199445630, 40.39835639566682346 ) ) ;
#50726 = ADVANCED_FACE ( 'NONE', ( #29883 ), #71897, .F. ) ;
#50727 = CARTESIAN_POINT ( 'NONE',  ( -77.57376394631657490, -29.99999999999998934, 180.9696502640093172 ) ) ;
#50728 = CARTESIAN_POINT ( 'NONE',  ( -56.87924109845976517, -49.91323546493563157, 69.03781967801916153 ) ) ;
#50729 = EDGE_LOOP ( 'NONE', ( #1614, #84281, #47163, #83955 ) ) ;
#50730 = CARTESIAN_POINT ( 'NONE',  ( -0.3760805828550403684, 300.0000000000000000, 9.936999415321508877 ) ) ;
#50731 = CARTESIAN_POINT ( 'NONE',  ( 19.87093931444394102, -60.00000000000000000, 40.18337028875610883 ) ) ;
#50732 = VERTEX_POINT ( 'NONE', #96193 ) ;
#50733 = CARTESIAN_POINT ( 'NONE',  ( 5.051333850944835113, -35.99138616323499207, 29.87840771616124869 ) ) ;
#50734 = CARTESIAN_POINT ( 'NONE',  ( -102.2537717332236440, -37.82053749917956509, 182.3686263342081588 ) ) ;
#50735 = CARTESIAN_POINT ( 'NONE',  ( -5.082755093536326818, -9.593750002048384573, 5.082755093536325042 ) ) ;
#50736 = EDGE_CURVE ( 'NONE', #61254, #94186, #3649, .T. ) ;
#50737 = CARTESIAN_POINT ( 'NONE',  ( 3.313708498984761608, -18.40625000409676915, -8.000000000000000000 ) ) ;
#50738 = DIRECTION ( 'NONE',  ( 0.000000000000000000, -1.000000000000000000, 0.000000000000000000 ) ) ;
#50739 = EDGE_LOOP ( 'NONE', ( #32329, #103790, #41214, #27508, #48637 ) ) ;
#50740 = CARTESIAN_POINT ( 'NONE',  ( -45.99999999999998579, 488.0052860040137830, 1.469193544622068526 ) ) ;
#50741 = CARTESIAN_POINT ( 'NONE',  ( -49.50947049896235086, -59.99999999999998579, 70.55260509993409812 ) ) ;
#50742 = CARTESIAN_POINT ( 'NONE',  ( -3.460324465708875863, -1.165480915299198728, 104.5902739981059426 ) ) ;
#50743 = CARTESIAN_POINT ( 'NONE',  ( 2.977408999572650927, -20.75000000204839523, -7.188101187500001821 ) ) ;
#50744 = CARTESIAN_POINT ( 'NONE',  ( -0.6458512730941106117, 36.35850673702802283, -29.58327430845546147 ) ) ;
#50745 =( NAMED_UNIT ( * ) PLANE_ANGLE_UNIT ( ) SI_UNIT ( $, .RADIAN. ) );
#50746 = AXIS2_PLACEMENT_3D ( 'NONE', #9417, #11021, #44480 ) ;
#50747 = CARTESIAN_POINT ( 'NONE',  ( -0.01431428620034891179, -57.67120202577072519, -44.61186648040676772 ) ) ;
#50748 = CARTESIAN_POINT ( 'NONE',  ( 25.11650669486618881, 4.000000000000003553, 4.898587196589414801E-16 ) ) ;
#50749 = CARTESIAN_POINT ( 'NONE',  ( 23.96375140441108442, 306.3052962357393199, 10.25885168886986243 ) ) ;
#50750 = CARTESIAN_POINT ( 'NONE',  ( 9.241147685141145374, -13.39842114471960066, 16.48049835958764575 ) ) ;
#50751 = CARTESIAN_POINT ( 'NONE',  ( 102.9313392694734688, 5.000000000000023093, 6.123233995736781074E-16 ) ) ;
#50752 = DIRECTION ( 'NONE',  ( -1.000000000000000000, -1.224606353822377258E-16, -0.000000000000000000 ) ) ;
#50753 = PRODUCT_DEFINITION_FORMATION_WITH_SPECIFIED_SOURCE ( 'ANY', '', #38205, .NOT_KNOWN. ) ;
#50754 = CARTESIAN_POINT ( 'NONE',  ( -31.39360692306285117, -29.07856664448081219, 31.74873827322397091 ) ) ;
#50755 = CARTESIAN_POINT ( 'NONE',  ( -1.468752096361391368, -49.97154544718587488, 101.6458968146044697 ) ) ;
#50756 = CARTESIAN_POINT ( 'NONE',  ( 44.07113633205571546, -46.43536708221260056, 44.37285927327917534 ) ) ;
#50757 = CYLINDRICAL_SURFACE ( 'NONE', #81649, 5.000000000000000888 ) ;
#50758 = ORIENTED_EDGE ( 'NONE', *, *, #80243, .T. ) ;
#50759 = CARTESIAN_POINT ( 'NONE',  ( 43.77364510076557735, 434.9303853138975455, 13.50475697610904824 ) ) ;
#50760 = CARTESIAN_POINT ( 'NONE',  ( -80.08513989354706553, -38.78833375829605501, 193.1411605214941005 ) ) ;
#50761 = ORIENTED_EDGE ( 'NONE', *, *, #53045, .T. ) ;
#50763 = CARTESIAN_POINT ( 'NONE',  ( -6.837824896291513355, -3.947820044545450102, -6.564402953523720718 ) ) ;
#50762 = DIRECTION ( 'NONE',  ( 0.000000000000000000, 0.000000000000000000, 1.000000000000000000 ) ) ;
#50764 = CARTESIAN_POINT ( 'NONE',  ( 4.175852187281085648, -59.99999999999998579, 33.87838816770964456 ) ) ;
#50765 = CARTESIAN_POINT ( 'NONE',  ( 0.000000000000000000, 0.000000000000000000, 0.000000000000000000 ) ) ;
#50766 = CARTESIAN_POINT ( 'NONE',  ( -7.302672345405872179, 41.33022796407946942, -59.14964389299829151 ) ) ;
#50767 = DIRECTION ( 'NONE',  ( -0.000000000000000000, 1.000000000000000000, -0.000000000000000000 ) ) ;
#50768 = DIRECTION ( 'NONE',  ( -0.000000000000000000, -1.000000000000000000, -0.000000000000000000 ) ) ;
#50769 = CARTESIAN_POINT ( 'NONE',  ( -23.52494306516553380, 305.9412313528462164, 9.175829795430782809 ) ) ;
#50770 = DIRECTION ( 'NONE',  ( 0.000000000000000000, 0.000000000000000000, 1.000000000000000000 ) ) ;
#50771 = CARTESIAN_POINT ( 'NONE',  ( 103.5882826872034457, -60.00000000000000711, 102.0264544966379106 ) ) ;
#50772 = CARTESIAN_POINT ( 'NONE',  ( 14.34999999999999787, 1.533819458162526451E-15, 0.000000000000000000 ) ) ;
#50773 = CARTESIAN_POINT ( 'NONE',  ( -34.76127857255404052, 469.3282716276013389, 1.881874431123442548 ) ) ;
#50774 = ORIENTED_EDGE ( 'NONE', *, *, #88212, .T. ) ;
#50775 = EDGE_CURVE ( 'NONE', #95821, #25469, #105261, .T. ) ;
#50776 = CONICAL_SURFACE ( 'NONE', #83508, 4.000000000000007105, 0.9599310885968835860 ) ;
#50777 = CARTESIAN_POINT ( 'NONE',  ( -90.96836049887622266, -29.99999999999996447, 190.4758564127751583 ) ) ;
#50778 = EDGE_LOOP ( 'NONE', ( #62755, #98557, #2277, #26902 ) ) ;
#50779 = EDGE_CURVE ( 'NONE', #87625, #36600, #31477, .T. ) ;
#50780 = CARTESIAN_POINT ( 'NONE',  ( 25.89579718936635544, 37.13050443889593311, -9.162997211423999033 ) ) ;
#50781 = CARTESIAN_POINT ( 'NONE',  ( 42.19180677453719142, 462.2931784592651070, 3.389262873192026682 ) ) ;
#50782 = CARTESIAN_POINT ( 'NONE',  ( 20.20152979676450400, 303.8530952710909787, 9.937276093638269359 ) ) ;
#50783 = FACE_OUTER_BOUND ( 'NONE', #93195, .T. ) ;
#50784 = CARTESIAN_POINT ( 'NONE',  ( -2.977408999572650039, -22.06250000204838813, -7.188101187500001821 ) ) ;
#50785 = DIRECTION ( 'NONE',  ( -1.000000000000000000, 0.000000000000000000, -0.000000000000000000 ) ) ;
#50786 = EDGE_CURVE ( 'NONE', #57410, #43420, #95656, .T. ) ;
#50787 = EDGE_CURVE ( 'NONE', #24472, #73965, #39838, .T. ) ;
#50788 =( GEOMETRIC_REPRESENTATION_CONTEXT ( 3 ) GLOBAL_UNCERTAINTY_ASSIGNED_CONTEXT ( ( #51955 ) ) GLOBAL_UNIT_ASSIGNED_CONTEXT ( ( #52994, #52442, #76190 ) ) REPRESENTATION_CONTEXT ( 'NONE', 'WORKASPACE' ) );
#50789 = AXIS2_PLACEMENT_3D ( 'NONE', #19790, #11632, #85555 ) ;
#50790 = PLANE ( 'NONE',  #55142 ) ;
#50791 = CIRCLE ( 'NONE', #69770, 4.000000000000000888 ) ;
#50793 = ORIENTED_EDGE ( 'NONE', *, *, #24209, .T. ) ;
#50792 =( NAMED_UNIT ( * ) PLANE_ANGLE_UNIT ( ) SI_UNIT ( $, .RADIAN. ) );
#50794 = CARTESIAN_POINT ( 'NONE',  ( 79.60221368316047119, -60.33621870816789823, 171.0006651665154607 ) ) ;
#50795 = CARTESIAN_POINT ( 'NONE',  ( 0.000000000000000000, 0.000000000000000000, 0.000000000000000000 ) ) ;
#50796 = TOROIDAL_SURFACE ( 'NONE', #80064, 8.400000000000000355, 0.5999999999999978684 ) ;
#50797 = FILL_AREA_STYLE_COLOUR ( '', #103976 ) ;
#50798 = ORIENTED_EDGE ( 'NONE', *, *, #6916, .F. ) ;
#50799 = FACE_OUTER_BOUND ( 'NONE', #78803, .T. ) ;
#50800 = EDGE_CURVE ( 'NONE', #53314, #13515, #71360, .T. ) ;
#50802 = ADVANCED_FACE ( 'NONE', ( #81038 ), #7153, .F. ) ;
#50801 = DIRECTION ( 'NONE',  ( 0.000000000000000000, 0.000000000000000000, 1.000000000000000000 ) ) ;
#50803 = CARTESIAN_POINT ( 'NONE',  ( 40.92692307692308162, 4.172000000000003261, 5.109226446042759579E-16 ) ) ;
#50804 = CARTESIAN_POINT ( 'NONE',  ( 30.00000000000000355, 488.6481008951276408, 3.890293910849272230 ) ) ;
#50805 = FILL_AREA_STYLE_COLOUR ( '', #50712 ) ;
#50806 =( BOUNDED_SURFACE ( )  B_SPLINE_SURFACE ( 3, 2, ( 
 ( #79295, #86882, #45876 ),
 ( #97068, #63668, #80342 ),
 ( #103058, #70685, #71718 ),
 ( #94979, #38854, #103576 ) ),
 .UNSPECIFIED., .F., .F., .F. ) 
 B_SPLINE_SURFACE_WITH_KNOTS ( ( 4, 4 ),
 ( 3, 3 ),
 ( -4.770489558936219510E-18, 0.0008582108274411621215 ),
 ( 0.000000000000000000, 1.000000000000000000 ),
 .UNSPECIFIED. ) 
 GEOMETRIC_REPRESENTATION_ITEM ( )  RATIONAL_B_SPLINE_SURFACE ( (
 ( 1.000000000000000000, 0.7409272757993125014, 1.000000000000000000),
 ( 1.000000000000000000, 0.7386644886093398643, 1.000000000000000000),
 ( 1.000000000000000000, 0.7359402037277221753, 1.000000000000000000),
 ( 1.000000000000000000, 0.7328671738315111206, 1.000000000000000000) ) ) 
 REPRESENTATION_ITEM ( '' )  SURFACE ( )  );
#50807 = CARTESIAN_POINT ( 'NONE',  ( -28.58275984112454537, 310.5877163737961837, 11.78456586285337870 ) ) ;
#50808 = DIRECTION ( 'NONE',  ( 0.000000000000000000, 0.000000000000000000, -1.000000000000000000 ) ) ;
#50809 = ORIENTED_EDGE ( 'NONE', *, *, #82271, .T. ) ;
#50810 = SURFACE_STYLE_FILL_AREA ( #100440 ) ;
#50811 = DIRECTION ( 'NONE',  ( 1.000000000000000000, 0.000000000000000000, 0.000000000000000000 ) ) ;
#50812 = CARTESIAN_POINT ( 'NONE',  ( -4.999999999997459810, -63.35894816178143429, 9.450637109162125071 ) ) ;
#50813 = CARTESIAN_POINT ( 'NONE',  ( 86.94938139748957440, -20.65577565933631732, 186.2948166322831867 ) ) ;
#50814 = DIRECTION ( 'NONE',  ( -1.000000000000000000, -0.000000000000000000, -0.000000000000000000 ) ) ;
#50815 = CARTESIAN_POINT ( 'NONE',  ( 2.977408999572650927, -32.37500000204838813, -7.188101187500001821 ) ) ;
#50816 = CARTESIAN_POINT ( 'NONE',  ( -30.00000000000000000, 500.0000000000002274, 5.000000000000001776 ) ) ;
#50817 = DIRECTION ( 'NONE',  ( -0.5735764363510461594, 0.8191520442889916875, 1.003171929053524870E-16 ) ) ;
#50818 = CARTESIAN_POINT ( 'NONE',  ( -7.703920929261755646, -4.447860822324870789, -7.917989418073283048 ) ) ;
#50819 = CONTEXT_DEPENDENT_SHAPE_REPRESENTATION ( #24615, #83599 ) ;
#50820 = ORIENTED_EDGE ( 'NONE', *, *, #93977, .F. ) ;
#50821 = CARTESIAN_POINT ( 'NONE',  ( 0.000000000000000000, 3.500000000000000000, 0.000000000000000000 ) ) ;
#50822 = DIRECTION ( 'NONE',  ( 1.000000000000000000, 1.224606353822377258E-16, 0.000000000000000000 ) ) ;
#50823 = PRESENTATION_LAYER_ASSIGNMENT (  '', '', ( #4348 ) ) ;
#50824 = CARTESIAN_POINT ( 'NONE',  ( -10.32854822922020332, 7.030784501320459512, 0.000000000000000000 ) ) ;
#50825 = CARTESIAN_POINT ( 'NONE',  ( 0.000000000000000000, 0.000000000000000000, 0.000000000000000000 ) ) ;
#50826 = ORIENTED_EDGE ( 'NONE', *, *, #56516, .F. ) ;
#50827 = CARTESIAN_POINT ( 'NONE',  ( -29.99999999998877698, 464.1630077738784621, 12.90488033688509795 ) ) ;
#50828 = CARTESIAN_POINT ( 'NONE',  ( -7.500000000000004441, 41.41666666666666430, -71.71180648257555390 ) ) ;
#50829 = CARTESIAN_POINT ( 'NONE',  ( 109.2576472045765428, -57.67135000464508465, 124.2156221577730975 ) ) ;
#50830 = ORIENTED_EDGE ( 'NONE', *, *, #45147, .F. ) ;
#50831 = EDGE_CURVE ( 'NONE', #28736, #90523, #33583, .T. ) ;
#50832 = CARTESIAN_POINT ( 'NONE',  ( 31.53900113926844639, 437.3650476817602453, 21.86274588273925090 ) ) ;
#50833 = B_SPLINE_CURVE_WITH_KNOTS ( 'NONE', 3,
 ( #39956, #6502, #15137, #96605, #88512, #90091, #89035, #49082, #48019, #65284, #105733, #15662, #31876, #48555, #71248, #97634, #96071, #73355, #106254, #32415 ),
 .UNSPECIFIED., .F., .F.,
 ( 4, 2, 2, 2, 2, 2, 2, 2, 2, 4 ),
 ( 0.007218903764951243446, 0.007723284340237460133, 0.008227664915523676820, 0.008732045490809895241, 0.009236426066096111928, 0.009488616353739223741, 0.009740806641382337289, 0.01024518721666855745, 0.01074956779195477760, 0.01125394836724099949 ),
 .UNSPECIFIED. ) ;
#50834 = CARTESIAN_POINT ( 'NONE',  ( -1.231305719443886781, 11.27890317915398022, -50.25262848319923847 ) ) ;
#50835 = DIRECTION ( 'NONE',  ( 1.000000000000000000, 0.000000000000000000, 0.000000000000000000 ) ) ;
#50836 = CARTESIAN_POINT ( 'NONE',  ( 7.500000000000000000, 4.330127018922203419, -0.9999999999999974465 ) ) ;
#50837 = CARTESIAN_POINT ( 'NONE',  ( -82.60176852780435297, -60.00000000000000711, 198.5318555412940214 ) ) ;
#50838 = DIRECTION ( 'NONE',  ( -1.000000000000000000, -1.224606353822377258E-16, -0.000000000000000000 ) ) ;
#50839 = FILL_AREA_STYLE_COLOUR ( '', #70148 ) ;
#50840 = DIRECTION ( 'NONE',  ( -1.000000000000000000, -0.000000000000000000, -0.000000000000000000 ) ) ;
#50841 = B_SPLINE_CURVE_WITH_KNOTS ( 'NONE', 3,
 ( #77727, #69636, #10313, #61557, #3839, #35705, #94453, #59426, #20610, #53449, #93382, #12435, #18994, #44293, #45363, #92290, #35162, #84220, #43231, #2212, #68028, #100921 ),
 .UNSPECIFIED., .F., .F.,
 ( 4, 2, 2, 2, 2, 2, 2, 2, 2, 2, 4 ),
 ( 0.007250106599135532071, 0.007754025997590315369, 0.008257945396045098668, 0.008761864794499881967, 0.009265784192954665266, 0.009769703591409448565, 0.01002166329063684802, 0.01027362298986424748, 0.01052558268909164693, 0.01077754238831904639, 0.01128146178677384009 ),
 .UNSPECIFIED. ) ;
#50842 = CARTESIAN_POINT ( 'NONE',  ( -84.63742604999939090, -42.97016984000447337, 184.5374066289867585 ) ) ;
#50843 = ORIENTED_EDGE ( 'NONE', *, *, #63845, .T. ) ;
#50844 = FILL_AREA_STYLE ('',( #92911 ) ) ;
#50845 = EDGE_LOOP ( 'NONE', ( #7825, #34251, #29127, #62386 ) ) ;
#50847 = EDGE_CURVE ( 'NONE', #104380, #74005, #55285, .T. ) ;
#50846 = CARTESIAN_POINT ( 'NONE',  ( 16.02336867590681990, 4.077607736802333349, -2.243736929340127695 ) ) ;
#50849 = CARTESIAN_POINT ( 'NONE',  ( 3.685905252136449928, -1.041089327947708032, 104.2837900504744510 ) ) ;
#50848 =( GEOMETRIC_REPRESENTATION_CONTEXT ( 3 ) GLOBAL_UNCERTAINTY_ASSIGNED_CONTEXT ( ( #102229 ) ) GLOBAL_UNIT_ASSIGNED_CONTEXT ( ( #7662, #91801, #32521 ) ) REPRESENTATION_CONTEXT ( 'NONE', 'WORKASPACE' ) );
#50850 = CARTESIAN_POINT ( 'NONE',  ( -85.70201354400094829, -52.74627078913300693, -8.673989746495539777 ) ) ;
#50851 = DIRECTION ( 'NONE',  ( -1.000000000000000000, -1.224606353822377258E-16, -0.000000000000000000 ) ) ;
#50852 = DIRECTION ( 'NONE',  ( -1.000000000000000000, -0.000000000000000000, -0.000000000000000000 ) ) ;
#50853 = PRESENTATION_LAYER_ASSIGNMENT (  '', '', ( #97371 ) ) ;
#50854 = CARTESIAN_POINT ( 'NONE',  ( 21.19348424345033521, 294.8901562694577478, 1.945151701991103321 ) ) ;
#50855 = CARTESIAN_POINT ( 'NONE',  ( -1.000000000000000888, -4.000000000000000000, 42.58845726811989607 ) ) ;
#50856 = CARTESIAN_POINT ( 'NONE',  ( -79.13121736037271603, 42.00000000000000000, 45.60838156032633606 ) ) ;
#50857 = CARTESIAN_POINT ( 'NONE',  ( -23.21751746555244722, 28.11705169068991594, 30.70617127781060418 ) ) ;
#50858 = CARTESIAN_POINT ( 'NONE',  ( 76.70261674817732001, -29.99999999999993250, 172.7038044719299990 ) ) ;
#50859 = CARTESIAN_POINT ( 'NONE',  ( -35.32911723019367400, 437.0667969981783472, 5.602639083905333273 ) ) ;
#50860 = CARTESIAN_POINT ( 'NONE',  ( 8.555192725956649369, -60.00000000000006395, -44.87746236044966253 ) ) ;
#50861 = CARTESIAN_POINT ( 'NONE',  ( -74.51172177323695678, -22.12478468806351017, 106.6322136500146627 ) ) ;
#50862 = COLOUR_RGB ( '', 0.72549020, 0.75294118, 0.79215686) ;
#50863 = EDGE_LOOP ( 'NONE', ( #17982, #69568 ) ) ;
#50864 = CARTESIAN_POINT ( 'NONE',  ( 76.70261674817732001, -29.99999999999993250, 172.7038044719299990 ) ) ;
#50865 = CARTESIAN_POINT ( 'NONE',  ( -63.17580323280985510, 40.83918043368394990, 15.57597231978257213 ) ) ;
#50866 = CARTESIAN_POINT ( 'NONE',  ( 111.2848894786437342, -57.67078734050053868, 193.4929494032239745 ) ) ;
#50867 = CIRCLE ( 'NONE', #69836, 12.00000000000001066 ) ;
#50869 = VERTEX_POINT ( 'NONE', #34135 ) ;
#50868 = CIRCLE ( 'NONE', #26847, 4.000000000000000888 ) ;
#50870 = CARTESIAN_POINT ( 'NONE',  ( 11.39273938773877326, -10.91116184185876037, 10.30307882325512558 ) ) ;
#50871 = AXIS2_PLACEMENT_3D ( 'NONE', #99266, #57217, #48068 ) ;
#50872 = ADVANCED_FACE ( 'NONE', ( #49201 ), #100099, .T. ) ;
#50873 = CARTESIAN_POINT ( 'NONE',  ( 6.249999999999998224, 4.618802153517001408, -8.000000000000000000 ) ) ;
#50874 = ORIENTED_EDGE ( 'NONE', *, *, #67008, .F. ) ;
#50875 = DIRECTION ( 'NONE',  ( -1.000000000000000000, -1.224606353822377258E-16, -0.000000000000000000 ) ) ;
#50876 = CARTESIAN_POINT ( 'NONE',  ( 4.000000000000002665, 17.58193670394227937, -5.744562646538072137 ) ) ;
#50877 = CARTESIAN_POINT ( 'NONE',  ( 30.43016653122454329, 310.3809086888959996, -8.487237336552468037 ) ) ;
#50878 = CARTESIAN_POINT ( 'NONE',  ( 5.082755093536325930, -12.96875000204838280, -5.082755093536325042 ) ) ;
#50879 = DIRECTION ( 'NONE',  ( -1.000000000000000000, 0.000000000000000000, 8.673617379884035472E-17 ) ) ;
#50880 = CIRCLE ( 'NONE', #16563, 3.309500000000001663 ) ;
#50881 = CARTESIAN_POINT ( 'NONE',  ( 2.505816879450918577, -0.4130341807012217203, 103.1328224996094747 ) ) ;
#50882 = SURFACE_SIDE_STYLE ('',( #18016 ) ) ;
#50883 = CARTESIAN_POINT ( 'NONE',  ( 16.84999999999999787, 3.309500000000003439, 4.052968581778167743E-16 ) ) ;
#50884 = CARTESIAN_POINT ( 'NONE',  ( -1.469576158976823947E-15, -14.37499999999999112, 8.000000000000000000 ) ) ;
#50885 = DIRECTION ( 'NONE',  ( 0.000000000000000000, 1.000000000000000000, 0.000000000000000000 ) ) ;
#50886 = EDGE_LOOP ( 'NONE', ( #8407, #90888, #94426, #74270 ) ) ;
#50887 = CARTESIAN_POINT ( 'NONE',  ( -6.965116046117190152, 41.61856606226410094, -70.00485699691064667 ) ) ;
#50888 = CARTESIAN_POINT ( 'NONE',  ( 34.27415957760879195, -60.29897218423202077, 38.86718388344454667 ) ) ;
#50889 = CARTESIAN_POINT ( 'NONE',  ( -4.080371711542015056, 51.84956781351371546, -7.633648114451180966 ) ) ;
#50890 = EDGE_LOOP ( 'NONE', ( #2509, #35645, #42955, #47243, #3700 ) ) ;
#50891 = FILL_AREA_STYLE_COLOUR ( '', #54748 ) ;
#50892 = PRODUCT_DEFINITION ( 'UNKNOWN', '', #66242, #89899 ) ;
#50893 = ORIENTED_EDGE ( 'NONE', *, *, #34477, .T. ) ;
#50895 = CARTESIAN_POINT ( 'NONE',  ( 73.33904886068935980, 6.975173280561618775E-15, 0.000000000000000000 ) ) ;
#50894 = DIRECTION ( 'NONE',  ( -1.000000000000000000, -1.224606353822377258E-16, -0.000000000000000000 ) ) ;
#50896 = DIRECTION ( 'NONE',  ( 0.000000000000000000, 0.000000000000000000, -1.000000000000000000 ) ) ;
#50897 = CARTESIAN_POINT ( 'NONE',  ( -43.65008909229012346, 485.2536725492916503, 3.136905111446141259 ) ) ;
#50898 = DIRECTION ( 'NONE',  ( 0.000000000000000000, -1.000000000000000000, 0.000000000000000000 ) ) ;
#50899 = CARTESIAN_POINT ( 'NONE',  ( 32.72541600403675233, 465.0324911293816967, 11.87889517178029841 ) ) ;
#50900 = CARTESIAN_POINT ( 'NONE',  ( -37.88504238421005965, 463.4171042825123550, 19.90923349044087942 ) ) ;
#50901 = EDGE_LOOP ( 'NONE', ( #81400, #12619, #35022, #36888, #2387, #4227, #91616, #42432 ) ) ;
#50902 = CARTESIAN_POINT ( 'NONE',  ( 68.98189563180189054, -60.00000000000000711, -32.94317599190360113 ) ) ;
#50903 = CARTESIAN_POINT ( 'NONE',  ( -9.032223969890592841, 46.05502784614109402, 14.03066199895137345 ) ) ;
#50904 = CARTESIAN_POINT ( 'NONE',  ( 29.99999999999957723, 464.1603955069842300, 12.55952670045058284 ) ) ;
#50905 = CARTESIAN_POINT ( 'NONE',  ( 39.83572194810514588, 489.3931820501625793, 11.44122026685077564 ) ) ;
#50906 = AXIS2_PLACEMENT_3D ( 'NONE', #41953, #17171, #10121 ) ;
#50907 = DIRECTION ( 'NONE',  ( -1.000000000000000000, -1.224606353822377258E-16, -0.000000000000000000 ) ) ;
#50908 = VERTEX_POINT ( 'NONE', #41130 ) ;
#50909 = DIRECTION ( 'NONE',  ( -0.4165977904505306917, 0.000000000000000000, 0.9090909090909092827 ) ) ;
#50910 = ORIENTED_EDGE ( 'NONE', *, *, #19561, .T. ) ;
#50911 = ORIENTED_EDGE ( 'NONE', *, *, #53219, .F. ) ;
#50912 = CARTESIAN_POINT ( 'NONE',  ( 7.344505440741524893, 82.55381072701295864, -3.175463080953001782 ) ) ;
#50913 = CARTESIAN_POINT ( 'NONE',  ( 6.289692432696772251, -6.589071317540681427, -2.245373559998993684 ) ) ;
#50914 = CARTESIAN_POINT ( 'NONE',  ( -15.49777008014214275, 34.92648659974615555, -22.93096364591211866 ) ) ;
#50915 = FACE_OUTER_BOUND ( 'NONE', #84250, .T. ) ;
#50916 = CARTESIAN_POINT ( 'NONE',  ( 83.12214618901758456, -45.27717091314015363, -14.26087837487842869 ) ) ;
#50917 = CARTESIAN_POINT ( 'NONE',  ( -40.60927779514467773, 317.8171704805693025, 3.565600996951467927 ) ) ;
#50918 = DIRECTION ( 'NONE',  ( 0.000000000000000000, -0.5000000000000011102, -0.8660254037844379305 ) ) ;
#50919 = CARTESIAN_POINT ( 'NONE',  ( 12.50000000000001421, 34.82001026956950085, -54.10527893612417216 ) ) ;
#50920 = ORIENTED_EDGE ( 'NONE', *, *, #25136, .T. ) ;
#50921 = DIRECTION ( 'NONE',  ( -1.000000000000000000, -1.224606353822377258E-16, -0.000000000000000000 ) ) ;
#50922 = ADVANCED_FACE ( 'NONE', ( #40592 ), #46749, .T. ) ;
#50923 = ORIENTED_EDGE ( 'NONE', *, *, #34599, .T. ) ;
#50924 = CARTESIAN_POINT ( 'NONE',  ( -6.256238905932293370, -3.000000000000353495, -71.20382035666706599 ) ) ;
#50925 = CARTESIAN_POINT ( 'NONE',  ( 37.88504238421471371, 463.4171042825133213, 19.90923349043903556 ) ) ;
#50927 = EDGE_LOOP ( 'NONE', ( #19366, #72168, #46285, #78199 ) ) ;
#50926 = CARTESIAN_POINT ( 'NONE',  ( 6.308322377852634055, 51.28511537930989306, 8.025364867616824327 ) ) ;
#50928 = CARTESIAN_POINT ( 'NONE',  ( 73.44948613080914868, -36.01487196046611672, 111.7734220330967361 ) ) ;
#50929 = CIRCLE ( 'NONE', #23407, 12.00000000000001066 ) ;
#50930 = EDGE_LOOP ( 'NONE', ( #57171, #42816, #50680, #96839, #101945, #101701 ) ) ;
#50931 = EDGE_CURVE ( 'NONE', #99036, #62818, #105542, .T. ) ;
#50932 = CARTESIAN_POINT ( 'NONE',  ( -5.082755093536325042, -27.59375000204838457, -5.082755093536325930 ) ) ;
#50933 = EDGE_CURVE ( 'NONE', #99558, #64598, #15710, .T. ) ;
#50934 = CARTESIAN_POINT ( 'NONE',  ( -91.04381008827128596, -57.66401771476134996, -20.86613467659797649 ) ) ;
#50935 = VERTEX_POINT ( 'NONE', #16309 ) ;
#50936 = DIRECTION ( 'NONE',  ( -0.000000000000000000, -0.000000000000000000, 1.000000000000000000 ) ) ;
#50937 = VECTOR ( 'NONE', #43493, 1000.000000000000000 ) ;
#50938 = CARTESIAN_POINT ( 'NONE',  ( 105.5033247266267438, -60.15119772182732305, 185.5882202471690618 ) ) ;
#50939 = CARTESIAN_POINT ( 'NONE',  ( 5.619944455633341995, 51.29440671850761646, -8.489742679686163029 ) ) ;
#50940 = CARTESIAN_POINT ( 'NONE',  ( 41.08349330513380693, 4.898587196589405926E-16, -4.000000000000001776 ) ) ;
#50941 = CARTESIAN_POINT ( 'NONE',  ( 5.656854249492378806, -26.37500000409677270, 5.656854249492381470 ) ) ;
#50942 = AXIS2_PLACEMENT_3D ( 'NONE', #98277, #7134, #13628 ) ;
#50943 = CARTESIAN_POINT ( 'NONE',  ( -7.999999999999996447, -3.000000000000000000, 2.094395098902548824 ) ) ;
#50944 = CARTESIAN_POINT ( 'NONE',  ( 12.33349330513380693, 1.593028355512270962E-15, 0.000000000000000000 ) ) ;
#50945 = STYLED_ITEM ( 'NONE', ( #54169 ), #36583 ) ;
#50946 = LINE ( 'NONE', #68771, #6819 ) ;
#50947 = FACE_OUTER_BOUND ( 'NONE', #40928, .T. ) ;
#50948 = CARTESIAN_POINT ( 'NONE',  ( 97.47675437802963927, -60.00000000000000000, 196.6138812136176739 ) ) ;
#50949 = DIRECTION ( 'NONE',  ( -1.000000000000000000, -6.895525817007803270E-17, -2.692290834716004216E-15 ) ) ;
#50950 = CARTESIAN_POINT ( 'NONE',  ( -4.165977904505307805, 16.00000000000000000, -9.090909090909091717 ) ) ;
#50951 = EDGE_LOOP ( 'NONE', ( #12854, #19157, #35790, #52001, #40431 ) ) ;
#50952 = CARTESIAN_POINT ( 'NONE',  ( -5.500000000000006217, 42.00000000000000000, -59.88032989329961708 ) ) ;
#50953 = FACE_OUTER_BOUND ( 'NONE', #51272, .T. ) ;
#50954 = AXIS2_PLACEMENT_3D ( 'NONE', #44230, #52842, #78694 ) ;
#50955 = DIRECTION ( 'NONE',  ( -1.000000000000000000, -1.224606353822377258E-16, -0.000000000000000000 ) ) ;
#50956 = CARTESIAN_POINT ( 'NONE',  ( -84.25785865898413363, -30.00000000000000000, 163.3270934916272097 ) ) ;
#50957 = ORIENTED_EDGE ( 'NONE', *, *, #58917, .F. ) ;
#50958 = ORIENTED_EDGE ( 'NONE', *, *, #76890, .F. ) ;
#50959 = AXIS2_PLACEMENT_3D ( 'NONE', #54911, #87838, #72695 ) ;
#50960 = CARTESIAN_POINT ( 'NONE',  ( 37.88407777523421061, 25.64317711490430085, -10.98674666298723324 ) ) ;
#50961 = CARTESIAN_POINT ( 'NONE',  ( 70.98554509634433884, -57.68173086340836164, 162.1951512261919675 ) ) ;
#50963 = PLANE ( 'NONE',  #75842 ) ;
#50962 = CARTESIAN_POINT ( 'NONE',  ( 0.000000000000000000, 0.000000000000000000, -3.725171428571429022 ) ) ;
#50964 = ADVANCED_FACE ( 'NONE', ( #15784 ), #89801, .T. ) ;
#50965 = CARTESIAN_POINT ( 'NONE',  ( 40.50854106486515605, -33.09212884851145731, -37.39549675235985404 ) ) ;
#50966 = CARTESIAN_POINT ( 'NONE',  ( -39.19378338566357911, 489.8656698032278882, 11.78649807965604346 ) ) ;
#50967 = PRODUCT_DEFINITION_SHAPE ( 'NONE', 'NONE',  #54175 ) ;
#50968 = CARTESIAN_POINT ( 'NONE',  ( -43.22294892181861314, -59.99999999999999289, 57.26282192755943612 ) ) ;
#50969 = PRESENTATION_STYLE_ASSIGNMENT (( #4039 ) ) ;
#50970 = CARTESIAN_POINT ( 'NONE',  ( -86.74237309757550918, -39.12072068744619457, 188.5955380950024960 ) ) ;
#50971 = ORIENTED_EDGE ( 'NONE', *, *, #96594, .T. ) ;
#50972 = DIRECTION ( 'NONE',  ( 1.150791560227848297E-16, -0.3420201433256725987, 0.9396926207859068736 ) ) ;
#50973 = CARTESIAN_POINT ( 'NONE',  ( -4.005429499995301512, -29.03095694028940343, 28.72119633659973204 ) ) ;
#50974 = VECTOR ( 'NONE', #84858, 1000.000000000000000 ) ;
#50975 = DIRECTION ( 'NONE',  ( -1.000000000000000000, -0.000000000000000000, -0.000000000000000000 ) ) ;
#50976 = CARTESIAN_POINT ( 'NONE',  ( -37.50105686171508523, 463.9558322285216150, 19.48687368954042398 ) ) ;
#50979 = ADVANCED_FACE ( 'NONE', ( #91812 ), #41670, .T. ) ;
#50978 = CARTESIAN_POINT ( 'NONE',  ( 5.560201442585154474, -66.10109771767969278, 14.15124469594628387 ) ) ;
#50977 = CARTESIAN_POINT ( 'NONE',  ( -33.94524946120131403, 301.6549615082749369, 3.482976818372956362 ) ) ;
#50980 = ORIENTED_EDGE ( 'NONE', *, *, #3822, .T. ) ;
#50981 = CARTESIAN_POINT ( 'NONE',  ( 0.000000000000000000, 0.5000000000000000000, -3.500000000000000000 ) ) ;
#50982 = CARTESIAN_POINT ( 'NONE',  ( 0.6419155526175454041, 28.14113459593094291, 38.42427017686829060 ) ) ;
#50983 = CARTESIAN_POINT ( 'NONE',  ( -30.00061906993008876, 12.59382690271829652, -39.64398720750899230 ) ) ;
#50984 = CARTESIAN_POINT ( 'NONE',  ( 17.82557447769810821, 50.00000000000000000, 62.13990790720372104 ) ) ;
#50985 = CARTESIAN_POINT ( 'NONE',  ( 24.80105969489321893, 306.0237540681346218, -9.745911707962003234 ) ) ;
#50986 = CARTESIAN_POINT ( 'NONE',  ( -32.93513049338658760, 465.6726574193328361, 10.66039033145138326 ) ) ;
#50987 = DIRECTION ( 'NONE',  ( 0.000000000000000000, 0.9180702648391416698, -0.3964176948853171401 ) ) ;
#50988 = CARTESIAN_POINT ( 'NONE',  ( 106.9311160729171917, -14.21045842199435860, 169.9238089813113390 ) ) ;
#50989 = CARTESIAN_POINT ( 'NONE',  ( -79.39540201253396390, -56.85378631388855553, 163.2853465063474232 ) ) ;
#50990 = VERTEX_POINT ( 'NONE', #64868 ) ;
#50991 = CARTESIAN_POINT ( 'NONE',  ( 32.78741055188847042, 485.3331003366707819, 5.977022408747033388 ) ) ;
#50992 = CARTESIAN_POINT ( 'NONE',  ( 14.85284876471456350, 1.482358050883964840E-15, 0.000000000000000000 ) ) ;
#50993 = CARTESIAN_POINT ( 'NONE',  ( -1.469576158976823947E-15, -20.56250000409676915, 8.000000000000000000 ) ) ;
#50994 = CARTESIAN_POINT ( 'NONE',  ( -6.618366600633001084, -4.380080200176828420, -16.79229307443615582 ) ) ;
#50995 = CARTESIAN_POINT ( 'NONE',  ( 37.68709909070376796, 382.9750476856748378, 5.555079075619126172 ) ) ;
#50996 = EDGE_CURVE ( 'NONE', #93158, #61487, #62325, .T. ) ;
#50997 = CARTESIAN_POINT ( 'NONE',  ( 6.326445470157510798, -6.578717624163891387, 2.268395195563515099 ) ) ;
#50998 = ORIENTED_EDGE ( 'NONE', *, *, #63676, .F. ) ;
#50999 =( GEOMETRIC_REPRESENTATION_CONTEXT ( 3 ) GLOBAL_UNCERTAINTY_ASSIGNED_CONTEXT ( ( #81764 ) ) GLOBAL_UNIT_ASSIGNED_CONTEXT ( ( #56235, #5068, #32013 ) ) REPRESENTATION_CONTEXT ( 'NONE', 'WORKASPACE' ) );
#51000 = CARTESIAN_POINT ( 'NONE',  ( 4.898587196589412829E-16, -22.62499999999999289, -8.000000000000000000 ) ) ;
#51001 = ORIENTED_EDGE ( 'NONE', *, *, #100888, .F. ) ;
#51003 = EDGE_CURVE ( 'NONE', #28378, #83974, #17932, .T. ) ;
#51002 = CARTESIAN_POINT ( 'NONE',  ( 2.802461721337127898, 15.83563386295778308, 9.606080321247342013 ) ) ;
#51004 = CARTESIAN_POINT ( 'NONE',  ( 32.62920465536820558, 486.5749440413383127, 6.880070463956039717 ) ) ;
#51005 = STYLED_ITEM ( 'NONE', ( #18778 ), #64164 ) ;
#51006 = CARTESIAN_POINT ( 'NONE',  ( -11.91432047182436094, 49.99999999999999289, 64.17585289259305625 ) ) ;
#51007 = CARTESIAN_POINT ( 'NONE',  ( 5.000000000000041744, -12.81882114895618052, 11.98449427368572451 ) ) ;
#51008 = CARTESIAN_POINT ( 'NONE',  ( 0.000000000000000000, 50.00000000000000000, 0.000000000000000000 ) ) ;
#51009 = VERTEX_POINT ( 'NONE', #65934 ) ;
#51010 = CARTESIAN_POINT ( 'NONE',  ( 100.0806260828529162, -60.00000000000001421, 201.8633356714223339 ) ) ;
#51011 = AXIS2_PLACEMENT_3D ( 'NONE', #91177, #26462, #99225 ) ;
#51013 = CARTESIAN_POINT ( 'NONE',  ( 20.58328600930757801, -56.87559710208555686, 33.96513392023969402 ) ) ;
#51012 = CARTESIAN_POINT ( 'NONE',  ( -97.75001763179835734, -59.99999999999991473, 204.9118596629033675 ) ) ;
#51014 = EDGE_CURVE ( 'NONE', #27128, #87652, #83757, .T. ) ;
#51016 = FACE_OUTER_BOUND ( 'NONE', #92169, .T. ) ;
#51015 = PRODUCT_DEFINITION_CONTEXT ( 'detailed design', #93438, 'design' ) ;
#51017 = DIRECTION ( 'NONE',  ( 0.000000000000000000, 0.3241911592375312789, 0.9459915920726916783 ) ) ;
#51018 = CARTESIAN_POINT ( 'NONE',  ( -43.67735976744434367, -29.16186524003355274, 39.50783654124030164 ) ) ;
#51019 = CARTESIAN_POINT ( 'NONE',  ( 28.50099738913158376, 6.123233995736770227E-16, -5.000000000000002665 ) ) ;
#51020 = UNCERTAINTY_MEASURE_WITH_UNIT (LENGTH_MEASURE( 1.000000000000000082E-05 ), #22106, 'distance_accuracy_value', 'NONE');
#51021 = STYLED_ITEM ( 'NONE', ( #64483 ), #88996 ) ;
#51022 = CONICAL_SURFACE ( 'NONE', #91120, 4.000000000000000000, 0.9599310885968912466 ) ;
#51023 = VERTEX_POINT ( 'NONE', #92321 ) ;
#51024 = AXIS2_PLACEMENT_3D ( 'NONE', #97885, #6753, #80106 ) ;
#51025 = SURFACE_STYLE_USAGE ( .BOTH. , #91514 ) ;
#51026 = CARTESIAN_POINT ( 'NONE',  ( 7.945173694731215264, 53.90995037661843270, 3.881245261317305406 ) ) ;
#51027 = CARTESIAN_POINT ( 'NONE',  ( 23.96375140441108442, 306.3052962357393199, 10.25885168886986243 ) ) ;
#51028 = CARTESIAN_POINT ( 'NONE',  ( 29.83349330513380693, -4.000000000000000888, 4.898587196589416773E-16 ) ) ;
#51029 = CARTESIAN_POINT ( 'NONE',  ( -33.22299792462370505, 463.2507813292579044, 6.141559824023456571 ) ) ;
#51030 = ORIENTED_EDGE ( 'NONE', *, *, #20025, .T. ) ;
#51031 = CARTESIAN_POINT ( 'NONE',  ( -15.50560966020059617, 37.05331456527880363, -22.93063681418762911 ) ) ;
#51032 = ORIENTED_EDGE ( 'NONE', *, *, #76974, .T. ) ;
#51033 = CARTESIAN_POINT ( 'NONE',  ( 81.29237555794308889, -30.00000000000015987, -10.77076475157867463 ) ) ;
#51034 = CARTESIAN_POINT ( 'NONE',  ( 47.90468627969811166, 11.89467801380305545, 14.35535821593427919 ) ) ;
#51035 = EDGE_CURVE ( 'NONE', #14360, #24961, #78603, .T. ) ;
#51036 = CARTESIAN_POINT ( 'NONE',  ( -41.50820411079202188, 461.5963371455320612, 2.703439750996428081 ) ) ;
#51037 = CARTESIAN_POINT ( 'NONE',  ( -2.352990130084491319E-16, 8.660254037844390851, -7.422398894150036064 ) ) ;
#51038 = CARTESIAN_POINT ( 'NONE',  ( 80.94845987451680003, -30.00000000000001066, 4.951624427427304909 ) ) ;
#51039 = CARTESIAN_POINT ( 'NONE',  ( -27.25085409960445659, 309.8132056794035520, 11.34972795043210247 ) ) ;
#51040 = ORIENTED_EDGE ( 'NONE', *, *, #82674, .T. ) ;
#51041 = ORIENTED_EDGE ( 'NONE', *, *, #51124, .T. ) ;
#51042 = ORIENTED_EDGE ( 'NONE', *, *, #88247, .T. ) ;
#51043 = CARTESIAN_POINT ( 'NONE',  ( -47.18533784750982107, 13.30762177597462781, -14.68117529621423145 ) ) ;
#51044 = CARTESIAN_POINT ( 'NONE',  ( -36.35681509222002461, 25.99976016919919886, -12.56101700226311024 ) ) ;
#51045 = DIRECTION ( 'NONE',  ( -0.000000000000000000, 1.000000000000000000, -0.000000000000000000 ) ) ;
#51046 = CARTESIAN_POINT ( 'NONE',  ( -31.27232363897158152, 363.0966317728114063, 21.44374338523576640 ) ) ;
#51047 = CARTESIAN_POINT ( 'NONE',  ( 0.000000000000000000, 0.000000000000000000, 0.000000000000000000 ) ) ;
#51048 = ORIENTED_EDGE ( 'NONE', *, *, #102935, .T. ) ;
#51049 = CARTESIAN_POINT ( 'NONE',  ( 6.145467200814584530, 50.00000000000543565, -92.99666842292452884 ) ) ;
#51050 = ORIENTED_EDGE ( 'NONE', *, *, #27558, .T. ) ;
#51051 = DIRECTION ( 'NONE',  ( -1.000000000000000000, -1.224606353822377258E-16, -0.000000000000000000 ) ) ;
#51052 = CARTESIAN_POINT ( 'NONE',  ( 66.27348762673410931, -38.33599680880077187, 118.2887617752395784 ) ) ;
#51053 = CARTESIAN_POINT ( 'NONE',  ( 0.000000000000000000, 0.000000000000000000, 0.000000000000000000 ) ) ;
#51054 = CARTESIAN_POINT ( 'NONE',  ( 25.39130259153011693, 304.9315442971644643, 10.40036917033271635 ) ) ;
#51055 = VECTOR ( 'NONE', #30056, 1000.000000000000114 ) ;
#51056 = CYLINDRICAL_SURFACE ( 'NONE', #83725, 7.000000000000000000 ) ;
#51057 = EDGE_LOOP ( 'NONE', ( #60925, #12333, #100392, #44116, #26868 ) ) ;
#51058 = MECHANICAL_DESIGN_GEOMETRIC_PRESENTATION_REPRESENTATION (  '', ( #95896 ), #2868 ) ;
#51059 = DIRECTION ( 'NONE',  ( -0.5735764363510494901, -0.8191520442889894671, 0.000000000000000000 ) ) ;
#51060 = DIRECTION ( 'NONE',  ( 0.000000000000000000, -1.000000000000000000, 0.000000000000000000 ) ) ;
#51061 = EDGE_CURVE ( 'NONE', #71083, #1485, #92856, .T. ) ;
#51062 = DIRECTION ( 'NONE',  ( -1.000000000000000000, -0.000000000000000000, -0.000000000000000000 ) ) ;
#51063 = CARTESIAN_POINT ( 'NONE',  ( 14.85111941933868884, 2.241372557329905479, 2.058092574385571361 ) ) ;
#51064 = ORIENTED_EDGE ( 'NONE', *, *, #11707, .F. ) ;
#51065 = CARTESIAN_POINT ( 'NONE',  ( 0.000000000000000000, 0.000000000000000000, 0.000000000000000000 ) ) ;
#51066 = DIRECTION ( 'NONE',  ( -1.000000000000000000, 0.000000000000000000, -0.000000000000000000 ) ) ;
#51067 = FACE_OUTER_BOUND ( 'NONE', #35194, .T. ) ;
#51068 = CARTESIAN_POINT ( 'NONE',  ( -2.621328321947687723, -7.606199919103087126, -7.633618187056816495 ) ) ;
#51069 = DIRECTION ( 'NONE',  ( 0.000000000000000000, 0.000000000000000000, -1.000000000000000000 ) ) ;
#51070 = ADVANCED_FACE ( 'NONE', ( #10341 ), #83890, .T. ) ;
#51071 = LINE ( 'NONE', #85607, #22017 ) ;
#51072 = DIRECTION ( 'NONE',  ( -0.5735764363510497121, 0.8191520442889892450, 1.003171929053521665E-16 ) ) ;
#51073 = CARTESIAN_POINT ( 'NONE',  ( 86.04703566227567535, -31.95183572172941666, 184.0160242643544279 ) ) ;
#51074 =( GEOMETRIC_REPRESENTATION_CONTEXT ( 3 ) GLOBAL_UNCERTAINTY_ASSIGNED_CONTEXT ( ( #99855 ) ) GLOBAL_UNIT_ASSIGNED_CONTEXT ( ( #5081, #79491, #47112 ) ) REPRESENTATION_CONTEXT ( 'NONE', 'WORKASPACE' ) );
#51075 = CIRCLE ( 'NONE', #70111, 1.999999999999999778 ) ;
#51076 = CARTESIAN_POINT ( 'NONE',  ( -8.474746145538347264, 26.96279221873305332, 4.999999999998729017 ) ) ;
#51077 = ORIENTED_EDGE ( 'NONE', *, *, #63608, .T. ) ;
#51078 = CARTESIAN_POINT ( 'NONE',  ( 94.69864826002789471, -57.66440398302673032, -5.036685645262155120 ) ) ;
#51079 = CYLINDRICAL_SURFACE ( 'NONE', #89940, 8.000000000000000000 ) ;
#51080 = CARTESIAN_POINT ( 'NONE',  ( 15.97317602965549277, 35.08246898966388727, -22.07552446507282795 ) ) ;
#51081 = FACE_OUTER_BOUND ( 'NONE', #46286, .T. ) ;
#51082 = CARTESIAN_POINT ( 'NONE',  ( -81.89555708626969022, -30.00000000000000355, 32.87881983670175856 ) ) ;
#51083 = ADVANCED_FACE ( 'NONE', ( #106242, #40998, #8622, #58237, #64747 ), #45082, .F. ) ;
#51084 = ADVANCED_BREP_SHAPE_REPRESENTATION ( '', ( #55083, #10728 ), #2257 ) ;
#51085 = COLOUR_RGB ( '', 0.09019608, 0.27058824, 0.51372549) ;
#51086 = VECTOR ( 'NONE', #53658, 1000.000000000000000 ) ;
#51087 = CARTESIAN_POINT ( 'NONE',  ( 23.05268216894187105, 28.15323590773658324, -30.70617127781077471 ) ) ;
#51088 = CARTESIAN_POINT ( 'NONE',  ( 0.000000000000000000, 0.000000000000000000, 1.734723475976807094E-15 ) ) ;
#51089 = CARTESIAN_POINT ( 'NONE',  ( -9.999945253488261798, 246.0001368662946390, -0.2662901834230864684 ) ) ;
#51090 = EDGE_CURVE ( 'NONE', #5652, #74471, #70930, .T. ) ;
#51091 = CARTESIAN_POINT ( 'NONE',  ( 5.687306430306777294, -50.94086591487122462, 39.79591033833035141 ) ) ;
#51092 = CARTESIAN_POINT ( 'NONE',  ( -39.28066024253707411, -34.89573333781912368, 37.03216938462795582 ) ) ;
#51093 = DIRECTION ( 'NONE',  ( 0.000000000000000000, 0.000000000000000000, -1.000000000000000000 ) ) ;
#51094 = DIRECTION ( 'NONE',  ( 0.000000000000000000, 0.000000000000000000, -1.000000000000000000 ) ) ;
#51095 = CARTESIAN_POINT ( 'NONE',  ( -22.59034450229749424, 25.42945400995673921, 33.04942977596110154 ) ) ;
#51096 = CARTESIAN_POINT ( 'NONE',  ( 40.02592568779148507, 5.000000000000003553, 0.000000000000000000 ) ) ;
#51097 = B_SPLINE_CURVE_WITH_KNOTS ( 'NONE', 3,
 ( #92921, #84839, #84309, #99951, #59512, #27711, #10404, #68120, #75672, #35796, #9331, #67602, #76733, #2304, #58443, #76201, #35252, #101016, #43842, #68674, #17466, #1773 ),
 .UNSPECIFIED., .F., .F.,
 ( 4, 2, 2, 2, 2, 2, 2, 2, 2, 2, 4 ),
 ( 0.002104729445818187550, 0.004038629005729561100, 0.005972528565640933783, 0.007906428125552308200, 0.009840327685463680016, 0.01177422724537505357, 0.01274117702533074208, 0.01370812680528642885, 0.01467507658524211736, 0.01564202636519780587, 0.01757592592510918289 ),
 .UNSPECIFIED. ) ;
#51098 = CIRCLE ( 'NONE', #85557, 3.309500000000007880 ) ;
#51099 = CIRCLE ( 'NONE', #97521, 57.50357696970299770 ) ;
#51100 = CARTESIAN_POINT ( 'NONE',  ( 47.72628330118641315, -26.96252987353755159, -28.54815866115082912 ) ) ;
#51101 = CARTESIAN_POINT ( 'NONE',  ( -22.90482800453732537, -53.39944789579089246, 33.72992494732504554 ) ) ;
#51102 = CONICAL_SURFACE ( 'NONE', #49413, 3.309500000000001663, 0.9599310885968770357 ) ;
#51103 = ORIENTED_EDGE ( 'NONE', *, *, #102184, .T. ) ;
#51104 = CARTESIAN_POINT ( 'NONE',  ( 6.445370176742730273, -7.262437273741192634, -1.101027156350390390 ) ) ;
#51105 = CARTESIAN_POINT ( 'NONE',  ( -9.176855344542985904, 105.5296042697740972, -3.973472207155928970 ) ) ;
#51106 = AXIS2_PLACEMENT_3D ( 'NONE', #37509, #21316, #71954 ) ;
#51107 = CARTESIAN_POINT ( 'NONE',  ( 7.500000000000006217, 39.99999999999942446, -59.88032989331673406 ) ) ;
#51108 = CARTESIAN_POINT ( 'NONE',  ( -40.31725178085623185, -24.96478901505654591, -30.23181082201408998 ) ) ;
#51109 =( BOUNDED_SURFACE ( )  B_SPLINE_SURFACE ( 2, 3, ( 
 ( #48291, #95814, #88250, #7832, #71513, #63457, #96351, #104414, #81189, #40742, #23001, #73627, #7299, #89836, #22482, #81709, #55837, #21941 ),
 ( #56374, #15937, #87724, #15404, #13805, #54793, #46717, #30559, #79609, #39702, #24066, #5724, #105995, #55323, #32143, #48815, #97915, #14330 ),
 ( #47236, #80135, #6238, #56911, #88774, #39174, #31104, #63988, #47758, #80661, #72578, #105480, #41274, #50943, #74165, #245, #50413, #34822 ) ),
 .UNSPECIFIED., .F., .T., .T. ) 
 B_SPLINE_SURFACE_WITH_KNOTS ( ( 3, 3 ),
 ( 4, 2, 2, 2, 2, 2, 2, 2, 4 ),
 ( 0.000000000000000000, 1.000000000000000000 ),
 ( 0.000000000000000000, 0.7853981633974482790, 1.570796326794896558, 2.356194490192344837, 3.141592653589793116, 3.926990816987241395, 4.712388980384689674, 5.497787143782137953, 6.283185307179586232 ),
 .UNSPECIFIED. ) 
 GEOMETRIC_REPRESENTATION_ITEM ( )  RATIONAL_B_SPLINE_SURFACE ( (
 ( 1.000000000000000000, 1.000000000000000000, 1.000000000000000000, 1.000000000000000000, 1.000000000000000000, 1.000000000000000000, 1.000000000000000000, 1.000000000000000000, 1.000000000000000000, 1.000000000000000000, 1.000000000000000000, 1.000000000000000000, 1.000000000000000000, 1.000000000000000000, 1.000000000000000000, 1.000000000000000000, 1.000000000000000000, 1.000000000000000000),
 ( 1.857142857142858317, 1.857142857142858317, 1.857142857142858317, 1.857142857142858317, 1.857142857142858317, 1.857142857142858317, 1.857142857142858317, 1.857142857142858317, 1.857142857142858317, 1.857142857142858317, 1.857142857142858317, 1.857142857142858317, 1.857142857142858317, 1.857142857142858317, 1.857142857142858317, 1.857142857142858317, 1.857142857142858317, 1.857142857142858317),
 ( 1.000000000000000000, 1.000000000000000000, 1.000000000000000000, 1.000000000000000000, 1.000000000000000000, 1.000000000000000000, 1.000000000000000000, 1.000000000000000000, 1.000000000000000000, 1.000000000000000000, 1.000000000000000000, 1.000000000000000000, 1.000000000000000000, 1.000000000000000000, 1.000000000000000000, 1.000000000000000000, 1.000000000000000000, 1.000000000000000000) ) ) 
 REPRESENTATION_ITEM ( '' )  SURFACE ( )  );
#51112 = EDGE_CURVE ( 'NONE', #79502, #50622, #66875, .T. ) ;
#51111 = DIRECTION ( 'NONE',  ( 0.000000000000000000, -1.000000000000000000, 0.000000000000000000 ) ) ;
#51110 =( NAMED_UNIT ( * ) SI_UNIT ( $, .STERADIAN. ) SOLID_ANGLE_UNIT ( ) );
#51113 = ORIENTED_EDGE ( 'NONE', *, *, #17089, .T. ) ;
#51114 = CARTESIAN_POINT ( 'NONE',  ( -35.68341320044621057, 437.0253618188252744, 4.635368180647969183 ) ) ;
#51115 = ORIENTED_EDGE ( 'NONE', *, *, #99714, .F. ) ;
#51116 = DIRECTION ( 'NONE',  ( -1.000000000000000000, -0.000000000000000000, -0.000000000000000000 ) ) ;
#51117 = CARTESIAN_POINT ( 'NONE',  ( -43.75401118688380819, 486.3173572309548263, 5.908089951475163915 ) ) ;
#51118 = ORIENTED_EDGE ( 'NONE', *, *, #54093, .T. ) ;
#51119 =( LENGTH_UNIT ( ) NAMED_UNIT ( * ) SI_UNIT ( .MILLI., .METRE. ) );
#51120 = CARTESIAN_POINT ( 'NONE',  ( -8.398759976699373908, 53.73767103463583084, -4.031152949374835259 ) ) ;
#51121 = CARTESIAN_POINT ( 'NONE',  ( 99.09806703519338100, -37.80934666507823749, 191.7968710950989646 ) ) ;
#51123 = CARTESIAN_POINT ( 'NONE',  ( -7.999885325681428405, -6.000229348700641729, 0.2682325777720040438 ) ) ;
#51122 = CARTESIAN_POINT ( 'NONE',  ( 9.659821686343899927, 294.6522965669146856, -2.601680433888549970 ) ) ;
#51124 = EDGE_CURVE ( 'NONE', #21525, #60365, #17271, .T. ) ;
#51125 = AXIS2_PLACEMENT_3D ( 'NONE', #33141, #41734, #89767 ) ;
#51126 = ORIENTED_EDGE ( 'NONE', *, *, #30704, .F. ) ;
#51127 = ORIENTED_EDGE ( 'NONE', *, *, #19932, .T. ) ;
#51128 = AXIS2_PLACEMENT_3D ( 'NONE', #29610, #88352, #54346 ) ;
#51129 = VERTEX_POINT ( 'NONE', #24319 ) ;
#51130 = CARTESIAN_POINT ( 'NONE',  ( 32.19453407377343979, 398.3930569349155917, 25.63217955030058803 ) ) ;
#51131 = ADVANCED_FACE ( 'NONE', ( #72816 ), #23440, .T. ) ;
#51132 = CARTESIAN_POINT ( 'NONE',  ( -39.08699041849552458, 460.7998460666116216, 2.161775044689049796 ) ) ;
#51133 = CARTESIAN_POINT ( 'NONE',  ( 8.875371311763096571, 53.84840360445480911, 1.561291615688902956 ) ) ;
#51134 = ORIENTED_EDGE ( 'NONE', *, *, #15787, .T. ) ;
#51135 = DIRECTION ( 'NONE',  ( 0.000000000000000000, 0.000000000000000000, 1.000000000000000000 ) ) ;
#51136 = CARTESIAN_POINT ( 'NONE',  ( -32.62730128615267944, 485.2399689022751659, 2.794144060392764750 ) ) ;
#51137 = CARTESIAN_POINT ( 'NONE',  ( -32.70807617001331380, 465.7746982375695666, 13.85399747859611885 ) ) ;
#51138 = CARTESIAN_POINT ( 'NONE',  ( -29.91071955673133687, -57.68399870184025247, 45.22199076326395328 ) ) ;
#51139 = CARTESIAN_POINT ( 'NONE',  ( 6.928203230275507885, -65.00000000000000000, 4.000000000000002665 ) ) ;
#51140 = CARTESIAN_POINT ( 'NONE',  ( -24.93816302196866275, 307.4233949143036284, 10.52291764336465008 ) ) ;
#51141 = DIRECTION ( 'NONE',  ( -1.000000000000000000, -1.224606353822377258E-16, -0.000000000000000000 ) ) ;
#51142 = CARTESIAN_POINT ( 'NONE',  ( -90.08857655234534434, -29.99999999999997158, -9.079940112750868764 ) ) ;
#51143 = EDGE_CURVE ( 'NONE', #47418, #9380, #81434, .T. ) ;
#51144 = CARTESIAN_POINT ( 'NONE',  ( -44.12590681760964628, 464.4133046726178691, 9.755964702276591183 ) ) ;
#51145 = CARTESIAN_POINT ( 'NONE',  ( -50.70036326620968481, -42.97893239173847491, 53.12086675882575548 ) ) ;
#51146 = CARTESIAN_POINT ( 'NONE',  ( 101.2019940638598854, 1.030564683017419500E-14, 0.000000000000000000 ) ) ;
#51147 = VERTEX_POINT ( 'NONE', #16185 ) ;
#51148 = CARTESIAN_POINT ( 'NONE',  ( 35.51071014494291234, 436.6042799465416238, 4.950281864158008638 ) ) ;
#51149 = CIRCLE ( 'NONE', #82182, 1.000000000000000000 ) ;
#51150 = CARTESIAN_POINT ( 'NONE',  ( -9.675290556387215801, 294.8809879903923843, -10.04271151416090291 ) ) ;
#51151 = CARTESIAN_POINT ( 'NONE',  ( 9.285924700174383872, -2.939022340138890410, 14.74017746627012571 ) ) ;
#51152 = ORIENTED_EDGE ( 'NONE', *, *, #8740, .T. ) ;
#51153 = CARTESIAN_POINT ( 'NONE',  ( 90.40984625334591840, -38.51012991717329470, 200.6755570011027885 ) ) ;
#51154 = CARTESIAN_POINT ( 'NONE',  ( 48.80488232270386106, 14.82891652079634426, 14.61828285348437007 ) ) ;
#51155 = DIRECTION ( 'NONE',  ( 1.000000000000000000, 0.000000000000000000, 0.000000000000000000 ) ) ;
#51156 = ADVANCED_FACE ( 'NONE', ( #49071 ), #103419, .T. ) ;
#51157 = CARTESIAN_POINT ( 'NONE',  ( 42.61650669486618881, 1.474610560812782335E-15, 0.000000000000000000 ) ) ;
#51158 = CARTESIAN_POINT ( 'NONE',  ( 94.46887059736158676, -30.00000000000000355, 191.3163273378258964 ) ) ;
#51159 = CARTESIAN_POINT ( 'NONE',  ( 43.77569424703103351, 434.3726356145342606, 11.96512969950840244 ) ) ;
#51160 = CARTESIAN_POINT ( 'NONE',  ( 0.000000000000000000, 0.000000000000000000, 0.000000000000000000 ) ) ;
#51161 = ORIENTED_EDGE ( 'NONE', *, *, #51329, .T. ) ;
#51162 = ORIENTED_EDGE ( 'NONE', *, *, #14040, .T. ) ;
#51163 = CARTESIAN_POINT ( 'NONE',  ( 51.33347871815171004, -56.83565511434251505, 59.27340484389767283 ) ) ;
#51164 = AXIS2_PLACEMENT_3D ( 'NONE', #93727, #19881, #27438 ) ;
#51165 = CARTESIAN_POINT ( 'NONE',  ( 6.894536717076869436, 41.40765062553401776, -58.61755662071193029 ) ) ;
#51166 = CARTESIAN_POINT ( 'NONE',  ( -7.500000000000007994, 40.00000000000000000, -70.16688272716517361 ) ) ;
#51167 = EDGE_LOOP ( 'NONE', ( #61541, #26989 ) ) ;
#51168 = CARTESIAN_POINT ( 'NONE',  ( -90.37015026637372728, -38.40145438430572966, -14.97427795305133458 ) ) ;
#51169 = VERTEX_POINT ( 'NONE', #55965 ) ;
#51170 = CARTESIAN_POINT ( 'NONE',  ( 108.3039360038514332, -38.35759540363747533, 192.1380689804155111 ) ) ;
#51171 = CARTESIAN_POINT ( 'NONE',  ( 13.33593371540757033, 24.31301558282364539, 2.945959972171505292 ) ) ;
#51173 = CARTESIAN_POINT ( 'NONE',  ( 86.85184780015545414, -37.84892900490719825, 58.81766505457247973 ) ) ;
#51172 = AXIS2_PLACEMENT_3D ( 'NONE', #91823, #2796, #50283 ) ;
#51174 = MECHANICAL_DESIGN_GEOMETRIC_PRESENTATION_REPRESENTATION (  '', ( #40790 ), #4630 ) ;
#51175 = AXIS2_PLACEMENT_3D ( 'NONE', #105776, #39994, #78988 ) ;
#51176 = CARTESIAN_POINT ( 'NONE',  ( 32.81882165182034328, 465.7334778289837800, 14.51165368401601441 ) ) ;
#51178 = CIRCLE ( 'NONE', #78663, 2.000000000000000000 ) ;
#51177 = CARTESIAN_POINT ( 'NONE',  ( -8.737863883542573262, -3.000000000000003109, -79.96381019629100706 ) ) ;
#51179 = CARTESIAN_POINT ( 'NONE',  ( 5.000000000000000000, -15.63336956925477672, -6.409577599286647498 ) ) ;
#51180 = CARTESIAN_POINT ( 'NONE',  ( -23.84258101729975365, 25.80558521616085699, -30.86173856011716055 ) ) ;
#51181 = AXIS2_PLACEMENT_3D ( 'NONE', #16772, #64279, #33504 ) ;
#51182 = CARTESIAN_POINT ( 'NONE',  ( -43.78405977007513883, 434.9821340022087384, 12.01170688374028828 ) ) ;
#51183 = CIRCLE ( 'NONE', #96022, 4.000000000000000000 ) ;
#51184 = ORIENTED_EDGE ( 'NONE', *, *, #54602, .T. ) ;
#51185 = CARTESIAN_POINT ( 'NONE',  ( 62.49820474788960922, -18.63632920802682946, 68.77955571764800879 ) ) ;
#51186 = ADVANCED_FACE ( 'NONE', ( #106115 ), #65769, .T. ) ;
#51187 = DIRECTION ( 'NONE',  ( 0.000000000000000000, 1.000000000000000000, 0.000000000000000000 ) ) ;
#51188 = FACE_OUTER_BOUND ( 'NONE', #79924, .T. ) ;
#51189 = ORIENTED_EDGE ( 'NONE', *, *, #91480, .T. ) ;
#51190 = CARTESIAN_POINT ( 'NONE',  ( 26.84999999999999787, -3.309499999999999886, 4.475777889183790779E-16 ) ) ;
#51191 = CARTESIAN_POINT ( 'NONE',  ( -42.77250796224285523, 406.2445966473596854, 19.93629092197699748 ) ) ;
#51192 = CARTESIAN_POINT ( 'NONE',  ( 0.000000000000000000, 3.500000000000000000, 0.000000000000000000 ) ) ;
#51193 = DIRECTION ( 'NONE',  ( 1.000000000000000000, -0.000000000000000000, -0.000000000000000000 ) ) ;
#51194 = CARTESIAN_POINT ( 'NONE',  ( 3.313708498984762496, -29.28124999999999645, 7.999999999999998224 ) ) ;
#51195 = CARTESIAN_POINT ( 'NONE',  ( -39.00146644722711642, -25.89668121096503128, 35.32705130283117256 ) ) ;
#51196 = EDGE_CURVE ( 'NONE', #70568, #72013, #97907, .T. ) ;
#51197 = AXIS2_PLACEMENT_3D ( 'NONE', #68729, #67116, #26171 ) ;
#51198 = CARTESIAN_POINT ( 'NONE',  ( 9.830769230769229594, -4.171999999999999709, 5.616230220889763424E-16 ) ) ;
#51199 = ORIENTED_EDGE ( 'NONE', *, *, #77867, .T. ) ;
#51200 = CARTESIAN_POINT ( 'NONE',  ( 83.13910501099707062, -50.07829878328394102, 183.9083247637312013 ) ) ;
#51201 = CARTESIAN_POINT ( 'NONE',  ( -85.08119784002818164, -52.74728882239156036, 190.3170911141409363 ) ) ;
#51202 = ORIENTED_EDGE ( 'NONE', *, *, #61215, .T. ) ;
#51203 = FACE_OUTER_BOUND ( 'NONE', #31869, .T. ) ;
#51204 = CARTESIAN_POINT ( 'NONE',  ( 8.447961717367675760, -4.999999999999968914, -16.27270454675222666 ) ) ;
#51205 = CARTESIAN_POINT ( 'NONE',  ( 34.12349128637390550, 490.8027302422246407, 11.84948222508928062 ) ) ;
#51206 = CARTESIAN_POINT ( 'NONE',  ( 10.71924530989373103, -3.000000000000002665, -74.44967652504091404 ) ) ;
#51207 = CARTESIAN_POINT ( 'NONE',  ( -15.04647843581905420, -3.000000000000003109, -85.64811627161152785 ) ) ;
#51208 = VECTOR ( 'NONE', #42651, 1000.000000000000000 ) ;
#51209 = CARTESIAN_POINT ( 'NONE',  ( -33.64427641176231276, -30.86707006437501377, -37.96572353344528494 ) ) ;
#51210 = EDGE_CURVE ( 'NONE', #10713, #97033, #98472, .T. ) ;
#51211 = CARTESIAN_POINT ( 'NONE',  ( 43.66925938860883605, -60.00000000000000711, 58.07216833024137514 ) ) ;
#51212 = DIRECTION ( 'NONE',  ( -1.000000000000000000, -1.224606353822377258E-16, -0.000000000000000000 ) ) ;
#51213 = CARTESIAN_POINT ( 'NONE',  ( 0.8955584045642486224, -12.57757061814721311, 32.18682162422354054 ) ) ;
#51215 = CARTESIAN_POINT ( 'NONE',  ( -13.33398839547953152, 24.30949496516709019, 2.956257427454192843 ) ) ;
#51214 = CARTESIAN_POINT ( 'NONE',  ( -30.07121567580392352, -32.49802967840809487, 40.61539330391480718 ) ) ;
#51216 = DIRECTION ( 'NONE',  ( 0.000000000000000000, 1.000000000000000000, 0.000000000000000000 ) ) ;
#51217 = B_SPLINE_CURVE_WITH_KNOTS ( 'NONE', 3,
 ( #90577, #50109, #16147, #49035, #81932, #8050 ),
 .UNSPECIFIED., .F., .F.,
 ( 4, 2, 4 ),
 ( 0.000000000000000000, 0.002094584110640377531, 0.004189168221280755063 ),
 .UNSPECIFIED. ) ;
#51218 = CARTESIAN_POINT ( 'NONE',  ( 7.188101187499999156, -10.25000000204838813, 2.977408999572654924 ) ) ;
#51219 = DIRECTION ( 'NONE',  ( -0.000000000000000000, -1.000000000000000000, -0.000000000000000000 ) ) ;
#51220 = EDGE_LOOP ( 'NONE', ( #26459, #70159, #67045, #54326 ) ) ;
#51221 = DIRECTION ( 'NONE',  ( -1.000000000000000000, -1.224606353822377258E-16, -0.000000000000000000 ) ) ;
#51222 = CONICAL_SURFACE ( 'NONE', #70192, 5.000000000000010658, 0.9599310885968697082 ) ;
#51223 = CARTESIAN_POINT ( 'NONE',  ( -17.49999999999995737, 51.99999999999994316, 59.71562975593252531 ) ) ;
#51224 = CARTESIAN_POINT ( 'NONE',  ( -12.41115067335719147, -3.692203772662941752, 20.54117717663471510 ) ) ;
#51225 = DIRECTION ( 'NONE',  ( -1.000000000000000000, -1.224606353822377258E-16, -0.000000000000000000 ) ) ;
#51227 = CARTESIAN_POINT ( 'NONE',  ( 56.20992259933385782, -34.58943827994583131, -26.29397140020956058 ) ) ;
#51226 = CARTESIAN_POINT ( 'NONE',  ( 19.00000000000001066, -4.000000000000000000, 25.00000000000000000 ) ) ;
#51228 = ORIENTED_EDGE ( 'NONE', *, *, #47123, .T. ) ;
#51229 = CARTESIAN_POINT ( 'NONE',  ( 16.33361799548379523, 6.123233995736772199E-16, -5.000000000000001776 ) ) ;
#51230 = DIRECTION ( 'NONE',  ( 0.000000000000000000, 1.000000000000000000, 0.000000000000000000 ) ) ;
#51231 = AXIS2_PLACEMENT_3D ( 'NONE', #7346, #1908, #43458 ) ;
#51232 = CIRCLE ( 'NONE', #35829, 6.500000000000000888 ) ;
#51233 = ORIENTED_EDGE ( 'NONE', *, *, #16782, .F. ) ;
#51234 = CARTESIAN_POINT ( 'NONE',  ( 5.299999999999999822, 3.752776749732553263, -6.499999999999999112 ) ) ;
#51235 = DIRECTION ( 'NONE',  ( -0.000000000000000000, -1.000000000000000000, -0.000000000000000000 ) ) ;
#51236 = CARTESIAN_POINT ( 'NONE',  ( 2.845670519300376476E-15, 38.67090180175566871, 23.23666318551310539 ) ) ;
#51237 = CARTESIAN_POINT ( 'NONE',  ( -103.7318945818505682, -60.00000000000000000, 102.8686475082603948 ) ) ;
#51238 = AXIS2_PLACEMENT_3D ( 'NONE', #100064, #33764, #34840 ) ;
#51239 = DIRECTION ( 'NONE',  ( 1.000000000000000000, 0.000000000000000000, 0.000000000000000000 ) ) ;
#51240 = CARTESIAN_POINT ( 'NONE',  ( 3.288228914120473245, -7.217643567644816294, -7.591235721156639471 ) ) ;
#51241 = CIRCLE ( 'NONE', #4780, 2.000000000000001776 ) ;
#51242 = CARTESIAN_POINT ( 'NONE',  ( 30.95643954367146833, 313.8918926584737505, -7.857037206977866006 ) ) ;
#51243 = CARTESIAN_POINT ( 'NONE',  ( 41.54789589621260859, 460.8787123354391611, 2.862784844377739724 ) ) ;
#51245 = PRESENTATION_STYLE_ASSIGNMENT (( #10784 ) ) ;
#51244 = CARTESIAN_POINT ( 'NONE',  ( 5.036189802311931807, -3.000000000000002665, -76.26213611587876073 ) ) ;
#51246 = CARTESIAN_POINT ( 'NONE',  ( -85.58036756573783066, -21.94021760482315742, 167.0675817319834664 ) ) ;
#51247 = EDGE_LOOP ( 'NONE', ( #41751, #102433, #20463, #20478 ) ) ;
#51248 = ORIENTED_EDGE ( 'NONE', *, *, #28162, .T. ) ;
#51249 = EDGE_LOOP ( 'NONE', ( #96010, #94520, #24114, #66213 ) ) ;
#51250 = AXIS2_PLACEMENT_3D ( 'NONE', #23071, #47312, #81265 ) ;
#51251 = LINE ( 'NONE', #67992, #71659 ) ;
#51252 = DIRECTION ( 'NONE',  ( -1.000000000000000000, -1.224606353822377258E-16, -0.000000000000000000 ) ) ;
#51253 = ADVANCED_FACE ( 'NONE', ( #7960 ), #86433, .T. ) ;
#51254 = CARTESIAN_POINT ( 'NONE',  ( 0.5805565836007658964, 7.505553499465141165, -3.996997974842411264E-16 ) ) ;
#51255 = VERTEX_POINT ( 'NONE', #64627 ) ;
#51256 = B_SPLINE_CURVE_WITH_KNOTS ( 'NONE', 3,
 ( #51811, #93356, #77165, #10809, #91757, #42662, #26527, #75561, #1656, #27595, #76617, #59400, #92261, #101442, #51273, #3279, #84194, #10290, #104079, #94427, #53427, #87916, #102506, #38838, #29198, #79281, #45342, #12411, #69612, #95467, #86865, #53933, #54444, #70134 ),
 .UNSPECIFIED., .F., .F.,
 ( 4, 2, 2, 2, 2, 2, 2, 2, 2, 2, 2, 2, 2, 2, 2, 2, 4 ),
 ( 0.01279395524623341482, 0.01359199989167121127, 0.01439004453710900772, 0.01518808918254680243, 0.01598613382798460061, 0.01678417847342239533, 0.01758222311886019351, 0.01838026776429798823, 0.01917831240973578294, 0.01997635705517358112, 0.02077440170061137584, 0.02157244634604917055, 0.02237049099148696873, 0.02316853563692476692, 0.02396658028236256163, 0.02476462492780035635, 0.02556266957323815453 ),
 .UNSPECIFIED. ) ;
#51257 = CIRCLE ( 'NONE', #30685, 12.00000000000000711 ) ;
#51258 = DIRECTION ( 'NONE',  ( 0.000000000000000000, -1.000000000000000000, 0.000000000000000000 ) ) ;
#51259 = EDGE_CURVE ( 'NONE', #98861, #21000, #29622, .T. ) ;
#51260 = DIRECTION ( 'NONE',  ( 0.000000000000000000, -1.000000000000000000, 0.000000000000000000 ) ) ;
#51261 = DIRECTION ( 'NONE',  ( -1.000000000000000000, -1.224606353822377258E-16, -0.000000000000000000 ) ) ;
#51262 = DIRECTION ( 'NONE',  ( 1.000000000000000000, 1.224606353822377258E-16, 0.000000000000000000 ) ) ;
#51263 = CARTESIAN_POINT ( 'NONE',  ( -0.3343798466136014835, 53.41130560517088810, 10.20736967772077186 ) ) ;
#51264 = LINE ( 'NONE', #19500, #4543 ) ;
#51265 = CARTESIAN_POINT ( 'NONE',  ( -97.05546387255228069, -41.67764191913797589, 193.4168471130767841 ) ) ;
#51266 = EDGE_CURVE ( 'NONE', #13401, #105963, #69176, .T. ) ;
#51267 = CARTESIAN_POINT ( 'NONE',  ( 106.1195120942077494, -59.99999999999999289, 102.8136370513695397 ) ) ;
#51268 = EDGE_CURVE ( 'NONE', #70795, #57621, #53680, .T. ) ;
#51269 = CARTESIAN_POINT ( 'NONE',  ( -78.42710814205257464, -14.21045842199423070, 185.4825180806740548 ) ) ;
#51270 = CARTESIAN_POINT ( 'NONE',  ( -59.97371036787195209, -22.12477874294765812, 64.13592450898646291 ) ) ;
#51271 = CONICAL_SURFACE ( 'NONE', #3094, 4.172000000000001485, 0.9599310885968750373 ) ;
#51272 = EDGE_LOOP ( 'NONE', ( #26076, #17327, #43328, #37555, #30315, #48318, #15888 ) ) ;
#51273 = CARTESIAN_POINT ( 'NONE',  ( 6.924577185163239612, 16.86673950156980339, 1.057577261889345754 ) ) ;
#51274 = EDGE_LOOP ( 'NONE', ( #425, #5404, #87519, #56905 ) ) ;
#51275 = CARTESIAN_POINT ( 'NONE',  ( -100.3409567365024770, -37.81725092391206289, 189.9219167037537375 ) ) ;
#51276 = DIRECTION ( 'NONE',  ( -0.000000000000000000, 1.000000000000000000, -0.000000000000000000 ) ) ;
#51277 = CARTESIAN_POINT ( 'NONE',  ( -43.58492305596168137, 465.9553058690736407, 13.43507729846633758 ) ) ;
#51278 = FILL_AREA_STYLE ('',( #93361 ) ) ;
#51279 = ORIENTED_EDGE ( 'NONE', *, *, #24838, .T. ) ;
#51280 = CARTESIAN_POINT ( 'NONE',  ( 8.641101172573151246, -5.000000000000001776, -72.37542516944607485 ) ) ;
#51281 = CARTESIAN_POINT ( 'NONE',  ( -72.75504568474596567, -59.99999999999998579, 160.2259072040645265 ) ) ;
#51282 = CARTESIAN_POINT ( 'NONE',  ( 36.95318979654836511, 25.70470319923920854, -13.30662917248846178 ) ) ;
#51283 = CARTESIAN_POINT ( 'NONE',  ( 2.977408999572651815, -19.81250000204838813, 7.188101187500000933 ) ) ;
#51284 = EDGE_CURVE ( 'NONE', #74653, #25041, #7167, .T. ) ;
#51285 = CARTESIAN_POINT ( 'NONE',  ( -0.4138703915521824706, 37.18449757264020406, -27.31749840197732127 ) ) ;
#51286 = DIRECTION ( 'NONE',  ( -1.096832036894112098E-16, -0.000000000000000000, -1.000000000000000000 ) ) ;
#51287 = CARTESIAN_POINT ( 'NONE',  ( 4.418225343310108855, -0.000000000000000000, 16.46939662769216994 ) ) ;
#51288 = CARTESIAN_POINT ( 'NONE',  ( 0.000000000000000000, 49.50000000000000000, 60.00000000000000000 ) ) ;
#51289 = CARTESIAN_POINT ( 'NONE',  ( 37.33349330513379982, 1.593028355512270567E-15, 0.000000000000000000 ) ) ;
#51290 = CARTESIAN_POINT ( 'NONE',  ( 7.824046388961988896, -14.69261508678956929, 15.37861778814678537 ) ) ;
#51291 = CARTESIAN_POINT ( 'NONE',  ( -15.51806636169574993, 46.21009754484515497, -4.857304170327880755 ) ) ;
#51292 = DIRECTION ( 'NONE',  ( -1.000000000000000000, -0.000000000000000000, -0.000000000000000000 ) ) ;
#51293 = UNCERTAINTY_MEASURE_WITH_UNIT (LENGTH_MEASURE( 1.000000000000000082E-05 ), #29240, 'distance_accuracy_value', 'NONE');
#51294 = CARTESIAN_POINT ( 'NONE',  ( -29.36599388881087691, -18.64463543894338926, 29.18619376988382541 ) ) ;
#51295 = B_SPLINE_CURVE_WITH_KNOTS ( 'NONE', 3,
 ( #63475, #71013, #103904, #78565 ),
 .UNSPECIFIED., .F., .F.,
 ( 4, 4 ),
 ( 0.0005621349429477124748, 0.02562325005156303875 ),
 .UNSPECIFIED. ) ;
#51296 = CARTESIAN_POINT ( 'NONE',  ( 3.787807677591960687, 19.16435582558940709, 5.887840124967178568 ) ) ;
#51297 = CARTESIAN_POINT ( 'NONE',  ( 44.14039507018947717, -49.88908620783357861, 45.35107315698084562 ) ) ;
#51298 = CARTESIAN_POINT ( 'NONE',  ( -32.73605680493314196, 486.1418706179324545, 5.972480793507408237 ) ) ;
#51299 = DIRECTION ( 'NONE',  ( 0.000000000000000000, 0.000000000000000000, 1.000000000000000000 ) ) ;
#51300 = CARTESIAN_POINT ( 'NONE',  ( -76.27725968842102588, -38.39574923406762252, 180.3589007190480231 ) ) ;
#51301 = ORIENTED_EDGE ( 'NONE', *, *, #31116, .F. ) ;
#51302 = CARTESIAN_POINT ( 'NONE',  ( -16.14595037822624946, 20.73037563562378338, -4.193214079430573449 ) ) ;
#51303 = CARTESIAN_POINT ( 'NONE',  ( 80.72320425233836261, -59.99999999999997868, 180.7930442462130998 ) ) ;
#51304 = DIRECTION ( 'NONE',  ( -1.000000000000000000, -0.000000000000000000, -0.000000000000000000 ) ) ;
#51305 = CARTESIAN_POINT ( 'NONE',  ( -7.484956994628422677, 40.70736991036710606, -59.65999153245496700 ) ) ;
#51306 = CARTESIAN_POINT ( 'NONE',  ( 6.806778131844891000, 41.25019534418786549, -70.74215739200818120 ) ) ;
#51307 = CARTESIAN_POINT ( 'NONE',  ( 0.000000000000000000, 43.50000000000000711, 61.00000000000000000 ) ) ;
#51308 = CARTESIAN_POINT ( 'NONE',  ( -25.05029448812380721, 307.4428306656531618, 9.526979722917090498 ) ) ;
#51309 = FACE_OUTER_BOUND ( 'NONE', #26003, .T. ) ;
#51310 = COLOUR_RGB ( '', 0.40784314, 0.44705882, 0.49803922) ;
#51311 = CARTESIAN_POINT ( 'NONE',  ( 106.3919580027218359, -60.00000000000000000, 118.8438529489762772 ) ) ;
#51312 = AXIS2_PLACEMENT_3D ( 'NONE', #63455, #63983, #22478 ) ;
#51313 = CARTESIAN_POINT ( 'NONE',  ( 0.000000000000000000, 0.000000000000000000, 0.000000000000000000 ) ) ;
#51314 = DIRECTION ( 'NONE',  ( 0.000000000000000000, -1.000000000000000000, 0.000000000000000000 ) ) ;
#51315 = ORIENTED_EDGE ( 'NONE', *, *, #100472, .T. ) ;
#51316 = EDGE_CURVE ( 'NONE', #51548, #106028, #9060, .T. ) ;
#51317 =( NAMED_UNIT ( * ) SI_UNIT ( $, .STERADIAN. ) SOLID_ANGLE_UNIT ( ) );
#51318 = CARTESIAN_POINT ( 'NONE',  ( 4.472135954999578722, -65.00000000000000000, 4.000000000000002665 ) ) ;
#51319 = ORIENTED_EDGE ( 'NONE', *, *, #82674, .F. ) ;
#51320 = DIRECTION ( 'NONE',  ( 0.000000000000000000, 0.000000000000000000, -1.000000000000000000 ) ) ;
#51321 = FILL_AREA_STYLE ('',( #50270 ) ) ;
#51322 = PRESENTATION_STYLE_ASSIGNMENT (( #43778 ) ) ;
#51324 = DIRECTION ( 'NONE',  ( -1.000000000000000000, -0.000000000000000000, -0.000000000000000000 ) ) ;
#51323 = AXIS2_PLACEMENT_3D ( 'NONE', #18280, #51135, #77560 ) ;
#51325 = CIRCLE ( 'NONE', #91007, 5.000000000000010658 ) ;
#51326 = CARTESIAN_POINT ( 'NONE',  ( 5.082755093536324154, -19.71875000204838457, 5.082755093536326818 ) ) ;
#51327 = AXIS2_PLACEMENT_3D ( 'NONE', #26252, #42922, #34862 ) ;
#51328 = CARTESIAN_POINT ( 'NONE',  ( -43.62593301837079451, 434.3202385713651097, 14.43474084663357893 ) ) ;
#51329 = EDGE_CURVE ( 'NONE', #93530, #30792, #17671, .T. ) ;
#51330 = ADVANCED_FACE ( 'NONE', ( #27932 ), #34475, .F. ) ;
#51331 = CONICAL_SURFACE ( 'NONE', #20385, 3.309500000000007880, 0.9599310885968770357 ) ;
#51332 = UNCERTAINTY_MEASURE_WITH_UNIT (LENGTH_MEASURE( 1.000000000000000082E-05 ), #68050, 'distance_accuracy_value', 'NONE');
#51333 = VECTOR ( 'NONE', #105470, 1000.000000000000000 ) ;
#51334 = CARTESIAN_POINT ( 'NONE',  ( -8.000000000000000000, -12.03125000409677270, -3.313708498984762496 ) ) ;
#51335 = EDGE_CURVE ( 'NONE', #85882, #70645, #95046, .T. ) ;
#51337 = ORIENTED_EDGE ( 'NONE', *, *, #11628, .T. ) ;
#51336 =( NAMED_UNIT ( * ) SI_UNIT ( $, .STERADIAN. ) SOLID_ANGLE_UNIT ( ) );
#51338 = CARTESIAN_POINT ( 'NONE',  ( 81.52133577384425678, -42.96784206407738083, 161.5630992417780192 ) ) ;
#51339 = FACE_OUTER_BOUND ( 'NONE', #79663, .T. ) ;
#51340 = DIRECTION ( 'NONE',  ( 0.000000000000000000, 1.000000000000000000, -0.000000000000000000 ) ) ;
#51341 = EDGE_LOOP ( 'NONE', ( #53780, #94647, #18604, #12959, #12540 ) ) ;
#51342 = CARTESIAN_POINT ( 'NONE',  ( 0.000000000000000000, 0.000000000000000000, 0.000000000000000000 ) ) ;
#51343 =( LENGTH_UNIT ( ) NAMED_UNIT ( * ) SI_UNIT ( .MILLI., .METRE. ) );
#51344 = DIRECTION ( 'NONE',  ( 0.000000000000000000, 0.000000000000000000, 1.000000000000000000 ) ) ;
#51345 = LINE ( 'NONE', #74558, #69255 ) ;
#51346 = CARTESIAN_POINT ( 'NONE',  ( -5.646888413699863385, 253.4497415597037389, 2.040714635159906365 ) ) ;
#51347 = CARTESIAN_POINT ( 'NONE',  ( -26.36618118159100632, 306.0239721618610815, 10.65825050287647358 ) ) ;
#51348 = FILL_AREA_STYLE ('',( #27127 ) ) ;
#51349 = EDGE_CURVE ( 'NONE', #27454, #20213, #77868, .T. ) ;
#51350 = EDGE_LOOP ( 'NONE', ( #30966, #88936, #96403, #26165, #92704 ) ) ;
#51351 = UNCERTAINTY_MEASURE_WITH_UNIT (LENGTH_MEASURE( 1.000000000000000082E-05 ), #53090, 'distance_accuracy_value', 'NONE');
#51352 = AXIS2_PLACEMENT_3D ( 'NONE', #31254, #89984, #96495 ) ;
#51353 = CYLINDRICAL_SURFACE ( 'NONE', #953, 4.000000000000000888 ) ;
#51354 = CARTESIAN_POINT ( 'NONE',  ( -1.000000000000000000, -68.69775162920851130, 12.24814655257177343 ) ) ;
#51356 = ADVANCED_FACE ( 'NONE', ( #68348 ), #46886, .T. ) ;
#51355 = CARTESIAN_POINT ( 'NONE',  ( 87.18997347856540614, -27.99825934505209446, 187.4553388889137864 ) ) ;
#51357 = LINE ( 'NONE', #53496, #79172 ) ;
#51358 = CARTESIAN_POINT ( 'NONE',  ( -5.082755093536325042, -23.09375000204838457, -5.082755093536325930 ) ) ;
#51359 = CARTESIAN_POINT ( 'NONE',  ( 0.000000000000000000, 0.000000000000000000, -8.000000000000000000 ) ) ;
#51360 = CARTESIAN_POINT ( 'NONE',  ( 7.306639711237237655, 52.17338899348808212, 2.636058739605869228 ) ) ;
#51361 = EDGE_CURVE ( 'NONE', #97120, #80103, #357, .T. ) ;
#51362 = CONICAL_SURFACE ( 'NONE', #94432, 4.000000000000000000, 0.9599310885968912466 ) ;
#51363 = FACE_OUTER_BOUND ( 'NONE', #7037, .T. ) ;
#51364 = EDGE_LOOP ( 'NONE', ( #87117, #7000, #40842, #95028, #37791, #68518 ) ) ;
#51365 = CARTESIAN_POINT ( 'NONE',  ( -4.237512335919120849E-14, 43.17555810750860701, 18.75000000000000355 ) ) ;
#51366 = CARTESIAN_POINT ( 'NONE',  ( -10.16823181764050688, 7.259740064965972905, -5.000000000000079936 ) ) ;
#51367 = DIRECTION ( 'NONE',  ( 0.7092840680488031735, -0.7049227693954428497, 0.000000000000000000 ) ) ;
#51368 = ORIENTED_EDGE ( 'NONE', *, *, #59875, .T. ) ;
#51369 = CIRCLE ( 'NONE', #20504, 15.00000000000000711 ) ;
#51370 = CARTESIAN_POINT ( 'NONE',  ( -32.03536204142076826, 464.8478167070323934, 12.52449229590025048 ) ) ;
#51371 = CARTESIAN_POINT ( 'NONE',  ( -1.843253007570911225E-16, -9.147862274876562338, -8.047472243342939535 ) ) ;
#51372 = CIRCLE ( 'NONE', #65162, 0.9999999999999930056 ) ;
#51373 = DIRECTION ( 'NONE',  ( 0.000000000000000000, 0.000000000000000000, 1.000000000000000000 ) ) ;
#51374 = CARTESIAN_POINT ( 'NONE',  ( 9.220915120640581719, 103.9554511356791267, -3.870126578504840875 ) ) ;
#51375 = CARTESIAN_POINT ( 'NONE',  ( 7.409683256360576564, 302.7200035818300421, 9.908966834550497538 ) ) ;
#51376 = CARTESIAN_POINT ( 'NONE',  ( -92.26493084220614094, -60.00000000000000711, 202.3836785854439029 ) ) ;
#51377 = CARTESIAN_POINT ( 'NONE',  ( 10.12027680424187714, 44.03028463990052899, -12.90779740156171940 ) ) ;
#51379 = CIRCLE ( 'NONE', #4910, 13.00000000000000000 ) ;
#51378 = CARTESIAN_POINT ( 'NONE',  ( 46.00000000000000000, 500.0000000000002274, -12.00000000000000711 ) ) ;
#51380 = CARTESIAN_POINT ( 'NONE',  ( 0.000000000000000000, 0.000000000000000000, 0.000000000000000000 ) ) ;
#51381 = CIRCLE ( 'NONE', #27275, 4.000000000000000888 ) ;
#51382 = CARTESIAN_POINT ( 'NONE',  ( -85.55559475948190595, -32.12731255185389756, 181.4392504528566690 ) ) ;
#51383 = SURFACE_STYLE_FILL_AREA ( #50844 ) ;
#51384 = ORIENTED_EDGE ( 'NONE', *, *, #5792, .F. ) ;
#51385 = CYLINDRICAL_SURFACE ( 'NONE', #28601, 1.000000000000000888 ) ;
#51386 = EDGE_CURVE ( 'NONE', #24767, #95473, #10702, .T. ) ;
#51387 = CARTESIAN_POINT ( 'NONE',  ( 3.423905177084556328, -0.8279751000742714417, 103.8439100969722375 ) ) ;
#51388 = B_SPLINE_CURVE_WITH_KNOTS ( 'NONE', 3,
 ( #42012, #50104, #90034, #33417, #26414, #99722, #17757, #73847, #92155, #24795, #50613, #35025, #16680, #8045, #83009, #16140, #75444, #49571, #81925, #58197, #1537, #18300 ),
 .UNSPECIFIED., .F., .F.,
 ( 4, 2, 2, 2, 2, 2, 2, 2, 2, 2, 4 ),
 ( 0.006827920940005929341, 0.007331585277004999505, 0.007583417445504535455, 0.007835249614004072272, 0.008338913951003144170, 0.008590746119502681855, 0.008842578288002221273, 0.009849906962000365071, 0.01035357129899943870, 0.01060540346749897986, 0.01085723563599851928 ),
 .UNSPECIFIED. ) ;
#51389 = CARTESIAN_POINT ( 'NONE',  ( -86.51528361792135513, -60.14074312227410246, 2.089646723163113062 ) ) ;
#51390 = CARTESIAN_POINT ( 'NONE',  ( -4.962899348969606272, -12.37352932398175298, -8.506080509220907970 ) ) ;
#51391 = AXIS2_PLACEMENT_3D ( 'NONE', #15345, #48229, #40151 ) ;
#51392 = CARTESIAN_POINT ( 'NONE',  ( 0.000000000000000000, 6.123233995736767268E-16, -5.000000000000000888 ) ) ;
#51393 = CARTESIAN_POINT ( 'NONE',  ( 22.88508939410625942, 295.1610940167444710, 10.00275451425645734 ) ) ;
#51395 = CARTESIAN_POINT ( 'NONE',  ( 28.18083109848378598, 36.45116722329852621, -8.149727080479747698 ) ) ;
#51394 = CONICAL_SURFACE ( 'NONE', #77281, 4.172000000000001485, 0.9599310885968750373 ) ;
#51396 = CARTESIAN_POINT ( 'NONE',  ( -2.912673042965788187E-14, 42.00000000000000000, -90.56128410203886858 ) ) ;
#51397 = AXIS2_PLACEMENT_3D ( 'NONE', #51605, #51062, #92065 ) ;
#51398 = EDGE_CURVE ( 'NONE', #61967, #91723, #22756, .T. ) ;
#51399 = CARTESIAN_POINT ( 'NONE',  ( 0.000000000000000000, 61.50000000000000000, 6.999999999999992895 ) ) ;
#51400 = CARTESIAN_POINT ( 'NONE',  ( 69.92546618954501980, -29.99999999999995026, 127.5380661880360975 ) ) ;
#51401 =( NAMED_UNIT ( * ) SI_UNIT ( $, .STERADIAN. ) SOLID_ANGLE_UNIT ( ) );
#51402 = ADVANCED_FACE ( 'NONE', ( #19318 ), #26862, .T. ) ;
#51403 = CARTESIAN_POINT ( 'NONE',  ( -82.54102867968215662, -60.00000000000007105, -29.20875881225653004 ) ) ;
#51404 = CARTESIAN_POINT ( 'NONE',  ( -72.38508955459566607, -49.91119473924621985, 116.9164654461183659 ) ) ;
#51405 = EDGE_LOOP ( 'NONE', ( #54891, #34480, #105224, #19473 ) ) ;
#51406 = CARTESIAN_POINT ( 'NONE',  ( 64.23331706704713895, -60.00000000000004263, 125.0204823638418361 ) ) ;
#51407 = CARTESIAN_POINT ( 'NONE',  ( -31.42849905601886817, 40.83882027459411290, 56.97537319886429685 ) ) ;
#51408 = CARTESIAN_POINT ( 'NONE',  ( 47.37111856022713141, -57.67116701030797543, -40.42796442818178093 ) ) ;
#51409 = ORIENTED_EDGE ( 'NONE', *, *, #35020, .T. ) ;
#51410 = CARTESIAN_POINT ( 'NONE',  ( 12.74530331293310681, -9.910444218107741676, 11.27135949044345686 ) ) ;
#51411 = CARTESIAN_POINT ( 'NONE',  ( -5.082755093536326818, -24.59375000204838813, 5.082755093536325042 ) ) ;
#51412 = CARTESIAN_POINT ( 'NONE',  ( -5.999787407977319909, -6.000318888155526054, 0.2740427891042984121 ) ) ;
#51413 = ORIENTED_EDGE ( 'NONE', *, *, #100169, .F. ) ;
#51414 = CARTESIAN_POINT ( 'NONE',  ( 33.86650669486618881, -3.851859888774471706E-31, 4.000000000000000888 ) ) ;
#51415 = VERTEX_POINT ( 'NONE', #67288 ) ;
#51416 = CARTESIAN_POINT ( 'NONE',  ( -6.019162162299732444, 41.99999999999999289, -71.20548073449060666 ) ) ;
#51417 = CARTESIAN_POINT ( 'NONE',  ( 46.90314054034891456, 18.02221697236495501, -16.15497048139741665 ) ) ;
#51418 = CARTESIAN_POINT ( 'NONE',  ( 26.36650669486618881, -3.999999999999998224, 0.000000000000000000 ) ) ;
#51419 = CARTESIAN_POINT ( 'NONE',  ( -7.188101187500001821, -12.50000000204838990, -2.977408999572651371 ) ) ;
#51420 = ADVANCED_FACE ( 'NONE', ( #83987 ), #4828, .T. ) ;
#51421 = CARTESIAN_POINT ( 'NONE',  ( -49.15269216906030181, 13.73471152902511072, 15.05374764291914857 ) ) ;
#51422 = CARTESIAN_POINT ( 'NONE',  ( 15.38541618194247995, -4.285714285714296246, -20.05453516056602226 ) ) ;
#51423 =( NAMED_UNIT ( * ) PLANE_ANGLE_UNIT ( ) SI_UNIT ( $, .RADIAN. ) );
#51424 = CARTESIAN_POINT ( 'NONE',  ( -2.617478844992341180, 49.99999999999999289, -75.26027323389158141 ) ) ;
#51425 = DIRECTION ( 'NONE',  ( 0.000000000000000000, -1.000000000000000000, 0.000000000000000000 ) ) ;
#51426 = DIRECTION ( 'NONE',  ( 1.000000000000000000, 1.224606353822377258E-16, 0.000000000000000000 ) ) ;
#51427 = AXIS2_PLACEMENT_3D ( 'NONE', #36721, #70638, #54418 ) ;
#51428 = VERTEX_POINT ( 'NONE', #39571 ) ;
#51429 = CARTESIAN_POINT ( 'NONE',  ( -7.412969763095563103, 41.14559726925956085, -68.91429205793708945 ) ) ;
#51431 = CARTESIAN_POINT ( 'NONE',  ( 33.96413472286053548, -60.30148985827285202, 38.68745865078301449 ) ) ;
#51430 = CARTESIAN_POINT ( 'NONE',  ( -4.284822031655012076, -48.90716638558769347, 104.4267991316944375 ) ) ;
#51432 = CARTESIAN_POINT ( 'NONE',  ( 12.70248734011840597, -4.285714285713678073, -22.03900363279143093 ) ) ;
#51433 = ORIENTED_EDGE ( 'NONE', *, *, #91606, .T. ) ;
#51434 =( NAMED_UNIT ( * ) PLANE_ANGLE_UNIT ( ) SI_UNIT ( $, .RADIAN. ) );
#51435 = CIRCLE ( 'NONE', #85968, 10.12668159690567649 ) ;
#51436 = UNCERTAINTY_MEASURE_WITH_UNIT (LENGTH_MEASURE( 1.000000000000000082E-05 ), #19688, 'distance_accuracy_value', 'NONE');
#51437 = ORIENTED_EDGE ( 'NONE', *, *, #17999, .F. ) ;
#51439 = SURFACE_SIDE_STYLE ('',( #101056 ) ) ;
#51438 = CYLINDRICAL_SURFACE ( 'NONE', #31412, 4.000000000000000000 ) ;
#51440 = CARTESIAN_POINT ( 'NONE',  ( -46.00000000000000000, 450.0000000000002274, 13.20242257375370976 ) ) ;
#51441 = CARTESIAN_POINT ( 'NONE',  ( -43.60560354499889257, 484.6927786829147067, 3.665222855601379504 ) ) ;
#51442 = DIRECTION ( 'NONE',  ( 0.000000000000000000, 0.000000000000000000, 1.000000000000000000 ) ) ;
#51443 = CARTESIAN_POINT ( 'NONE',  ( 31.99602169361446258, 464.8336097802171594, 12.51960734452490875 ) ) ;
#51444 = CARTESIAN_POINT ( 'NONE',  ( -36.55533968308493797, 463.5207292468226115, 19.71490071751487605 ) ) ;
#51446 = ORIENTED_EDGE ( 'NONE', *, *, #69880, .F. ) ;
#51445 = VECTOR ( 'NONE', #71485, 1000.000000000000000 ) ;
#51447 = CARTESIAN_POINT ( 'NONE',  ( 90.03398063620191749, -59.99999999999999289, -18.77590310472173130 ) ) ;
#51448 = CYLINDRICAL_SURFACE ( 'NONE', #104949, 1.250000000000001110 ) ;
#51449 = LINE ( 'NONE', #33172, #58189 ) ;
#51450 =( BOUNDED_CURVE ( )  B_SPLINE_CURVE ( 2, ( #52392, #76666, #87441 ),
 .UNSPECIFIED., .F., .F. ) 
 B_SPLINE_CURVE_WITH_KNOTS ( ( 3, 3 ),
 ( 0.000000000000000000, 1.000000000000000000 ),
 .UNSPECIFIED. ) 
 CURVE ( )  GEOMETRIC_REPRESENTATION_ITEM ( )  RATIONAL_B_SPLINE_CURVE ( ( 1.000000000000000000, 1.857142857142858317, 1.000000000000000000 ) ) 
 REPRESENTATION_ITEM ( '' )  );
#51451 = DIRECTION ( 'NONE',  ( 0.000000000000000000, -1.000000000000000000, 0.000000000000000000 ) ) ;
#51452 = ORIENTED_EDGE ( 'NONE', *, *, #46713, .F. ) ;
#51453 = DIRECTION ( 'NONE',  ( -0.5735764363510461594, 0.8191520442889916875, 1.003171929053524870E-16 ) ) ;
#51454 = EDGE_LOOP ( 'NONE', ( #8016, #11812, #25597, #104704, #80213, #24639 ) ) ;
#51455 = EDGE_LOOP ( 'NONE', ( #89120, #40068, #100344, #4490 ) ) ;
#51456 = CARTESIAN_POINT ( 'NONE',  ( 46.00000000000000000, 438.4646224975062978, 9.895601460515761616 ) ) ;
#51457 = CARTESIAN_POINT ( 'NONE',  ( 6.585468679846627538, -7.640532685286901327, 0.2337908078075560669 ) ) ;
#51458 = CARTESIAN_POINT ( 'NONE',  ( -5.000000000000000888, -46.00000000000000000, 42.58845726811989607 ) ) ;
#51459 = FILL_AREA_STYLE_COLOUR ( '', #70705 ) ;
#51460 = CARTESIAN_POINT ( 'NONE',  ( 85.33315027561728527, -52.75744043830332686, -11.76120068538829422 ) ) ;
#51461 = CARTESIAN_POINT ( 'NONE',  ( -33.20442555830484110, 314.5462679929517549, -7.210101933046130007 ) ) ;
#51462 = CARTESIAN_POINT ( 'NONE',  ( 18.71538461538461462, 4.172000000000003261, 5.109226446042759579E-16 ) ) ;
#51463 = CARTESIAN_POINT ( 'NONE',  ( -18.10250950527013813, 45.00000000000000000, 62.50294572439922547 ) ) ;
#51464 = CLOSED_SHELL ( 'NONE', ( #55595, #45461, #13524, #25018, #6905, #83790, #24559, #32816, #7930, #79129, #93682, #58735, #92572, #96621, #26855, #30588, #13791, #48582, #38349, #82652, #26313, #105614, #91090, #89320, #95172, #20570, #44729, #95319, #23393, #30919, #94217, #102983, #54128, #58959, #69939, #99356, #9762, #75951, #53879, #534, #91150, #86386, #97535, #45906, #8176, #37275, #65038, #5893, #39780, #8012, #1439, #53683, #66635, #40611, #101124, #48028, #43094, #59092, #52690, #11451, #68486, #49473, #10396, #44515, #18065, #104144, #12053, #77489 ) ) ;
#51465 = ORIENTED_EDGE ( 'NONE', *, *, #54274, .F. ) ;
#51467 = EDGE_CURVE ( 'NONE', #51686, #68449, #81298, .T. ) ;
#51466 = CARTESIAN_POINT ( 'NONE',  ( -43.03880698781976832, 435.3545807224047053, 16.83573131045124427 ) ) ;
#51468 = ORIENTED_EDGE ( 'NONE', *, *, #9174, .T. ) ;
#51469 = CARTESIAN_POINT ( 'NONE',  ( 49.24306615471292758, 8.188742177551262102, -15.29695692017807396 ) ) ;
#51470 = CARTESIAN_POINT ( 'NONE',  ( 35.00384615384614762, 1.411358822780289120E-15, 0.000000000000000000 ) ) ;
#51472 = ORIENTED_EDGE ( 'NONE', *, *, #18492, .T. ) ;
#51471 = CARTESIAN_POINT ( 'NONE',  ( 5.799999999999999822, 4.618802153517003184, -8.000000000000000000 ) ) ;
#51473 = CARTESIAN_POINT ( 'NONE',  ( 73.18364344897008777, -39.48763927256371886, 113.0589750438585241 ) ) ;
#51474 = PRESENTATION_LAYER_ASSIGNMENT (  '', '', ( #34266 ) ) ;
#51475 = EDGE_LOOP ( 'NONE', ( #29551, #48611, #1975, #79993, #57678, #73073, #30240 ) ) ;
#51476 = CARTESIAN_POINT ( 'NONE',  ( 3.703334511254893879, -49.04702021385453037, 40.67780616083587120 ) ) ;
#51477 = DIRECTION ( 'NONE',  ( 0.000000000000000000, 1.000000000000000000, 0.000000000000000000 ) ) ;
#51478 = CARTESIAN_POINT ( 'NONE',  ( -7.188101187500000933, -26.00000000204838457, -2.977408999572651371 ) ) ;
#51479 = CARTESIAN_POINT ( 'NONE',  ( -94.31942352638992588, -57.67240272246704791, 24.69011299903190704 ) ) ;
#51480 = ORIENTED_EDGE ( 'NONE', *, *, #11529, .T. ) ;
#51481 = DIRECTION ( 'NONE',  ( 0.000000000000000000, -1.000000000000000000, 0.000000000000000000 ) ) ;
#51482 = CARTESIAN_POINT ( 'NONE',  ( 102.6007214329574140, -37.84836329290174461, 179.2133943646480532 ) ) ;
#51483 = COLOUR_RGB ( '', 0.72549020, 0.75294118, 0.79215686) ;
#51484 = CARTESIAN_POINT ( 'NONE',  ( 5.701517186572424123, 51.28557980447222064, -8.464474017692539931 ) ) ;
#51485 = CARTESIAN_POINT ( 'NONE',  ( 0.000000000000000000, 0.000000000000000000, 0.000000000000000000 ) ) ;
#51486 = CARTESIAN_POINT ( 'NONE',  ( 3.313708498984762496, -17.46875000409676559, 7.999999999999998224 ) ) ;
#51487 = CARTESIAN_POINT ( 'NONE',  ( -7.347880794884119933E-15, 0.000000000000000000, 60.00000000000000000 ) ) ;
#51488 = CONICAL_SURFACE ( 'NONE', #13527, 3.309500000000001663, 0.9599310885968770357 ) ;
#51489 = CARTESIAN_POINT ( 'NONE',  ( -36.45744830273498138, 25.93793769161023022, 12.78814307577592402 ) ) ;
#51490 = B_SPLINE_CURVE_WITH_KNOTS ( 'NONE', 3,
 ( #103855, #45639, #14299, #38107, #21386, #12717 ),
 .UNSPECIFIED., .F., .F.,
 ( 4, 2, 4 ),
 ( 2.380729204614878139E-07, 0.003943479449179625521, 0.007886720825438788343 ),
 .UNSPECIFIED. ) ;
#51491 = EDGE_CURVE ( 'NONE', #32616, #99250, #10400, .T. ) ;
#51492 = SURFACE_SIDE_STYLE ('',( #27276 ) ) ;
#51493 = DIRECTION ( 'NONE',  ( -1.000000000000000000, -1.224606353822377258E-16, -0.000000000000000000 ) ) ;
#51494 = CARTESIAN_POINT ( 'NONE',  ( 29.78291765283140080, 518.1183258647170078, 182.3141634307101526 ) ) ;
#51495 = CARTESIAN_POINT ( 'NONE',  ( 2.909149233950971691, -30.00000000000000711, -7.051612309719152982 ) ) ;
#51496 = ORIENTED_EDGE ( 'NONE', *, *, #22484, .F. ) ;
#51497 = CARTESIAN_POINT ( 'NONE',  ( 7.500000000000000000, -4.330127018922200755, -7.422398894150036064 ) ) ;
#51498 = CARTESIAN_POINT ( 'NONE',  ( -30.00000000000000000, 450.0000000000002274, 13.20242257375370976 ) ) ;
#51499 = CARTESIAN_POINT ( 'NONE',  ( 104.9555555555555486, 1.023464760207051730E-14, 0.000000000000000000 ) ) ;
#51500 = CARTESIAN_POINT ( 'NONE',  ( -85.08044947619957554, -30.00000000000000355, 171.0774529994631905 ) ) ;
#51501 = CIRCLE ( 'NONE', #92849, 5.000000000000001776 ) ;
#51502 = ORIENTED_EDGE ( 'NONE', *, *, #99016, .T. ) ;
#51503 = CARTESIAN_POINT ( 'NONE',  ( 4.969648522638418164, -46.56352935199780774, 42.62389940716953163 ) ) ;
#51504 = CARTESIAN_POINT ( 'NONE',  ( 72.46853216154282507, -57.66608118650142245, 176.6536213893129741 ) ) ;
#51506 = DIRECTION ( 'NONE',  ( 0.000000000000000000, 2.775557561562891351E-13, -1.000000000000000000 ) ) ;
#51505 = CARTESIAN_POINT ( 'NONE',  ( -14.99550388410368207, 1.250601500878925076, -0.4346214790565611774 ) ) ;
#51507 = ORIENTED_EDGE ( 'NONE', *, *, #56637, .F. ) ;
#51508 = VECTOR ( 'NONE', #33839, 1000.000000000000000 ) ;
#51509 = EDGE_CURVE ( 'NONE', #19689, #56343, #74442, .T. ) ;
#51510 = CARTESIAN_POINT ( 'NONE',  ( 25.63403565826709141, -27.94712950634049164, -38.35231772936518979 ) ) ;
#51511 = DIRECTION ( 'NONE',  ( 0.000000000000000000, -0.2521971900443084613, -0.9676758637755490389 ) ) ;
#51512 = FILL_AREA_STYLE ('',( #18652 ) ) ;
#51513 = CARTESIAN_POINT ( 'NONE',  ( -34.35683892909391801, -60.00000000000000711, 45.85838480689532304 ) ) ;
#51514 = CARTESIAN_POINT ( 'NONE',  ( -31.03678703374875880, 438.6650838204938054, 21.86890379898545334 ) ) ;
#51515 = CARTESIAN_POINT ( 'NONE',  ( -86.44470553919718725, -17.06574261455647701, 183.2584459546009157 ) ) ;
#51516 = ORIENTED_EDGE ( 'NONE', *, *, #2080, .T. ) ;
#51517 = CARTESIAN_POINT ( 'NONE',  ( 30.77392345931262341, 15.52887250063909441, 40.23353194602682237 ) ) ;
#51518 = CARTESIAN_POINT ( 'NONE',  ( -5.138880198032813595, -53.40245903056734278, 32.77961879907969234 ) ) ;
#51519 = CARTESIAN_POINT ( 'NONE',  ( -6.641837642500876271, 41.74662713182689089, -59.04567091375639620 ) ) ;
#51520 = CARTESIAN_POINT ( 'NONE',  ( 85.95779223056094054, -47.24568047936485726, 189.6962305527513593 ) ) ;
#51521 = CARTESIAN_POINT ( 'NONE',  ( -41.83706036796058925, 337.9408106068874531, 12.27123674261958897 ) ) ;
#51522 = VERTEX_POINT ( 'NONE', #95669 ) ;
#51523 = CARTESIAN_POINT ( 'NONE',  ( 28.12328997684540610, 24.73290587908618932, 14.06164498842269772 ) ) ;
#51524 = TOROIDAL_SURFACE ( 'NONE', #46381, 8.400000000000000355, 0.5999999999999978684 ) ;
#51525 = CARTESIAN_POINT ( 'NONE',  ( -8.464095510818648194, -5.000000000000260236, -16.25913807934452393 ) ) ;
#51526 = ADVANCED_FACE ( 'NONE', ( #54648 ), #87582, .F. ) ;
#51527 = LINE ( 'NONE', #2976, #5132 ) ;
#51528 = CARTESIAN_POINT ( 'NONE',  ( 17.56618469255510817, 50.00000000000001421, 62.84295761643686262 ) ) ;
#51529 = CARTESIAN_POINT ( 'NONE',  ( 32.54922218626916930, 319.8023524069591303, -6.363686095274232457 ) ) ;
#51530 = AXIS2_PLACEMENT_3D ( 'NONE', #11997, #69203, #60584 ) ;
#51531 = EDGE_CURVE ( 'NONE', #26788, #80415, #99941, .T. ) ;
#51532 = FACE_OUTER_BOUND ( 'NONE', #52320, .T. ) ;
#51533 =( NAMED_UNIT ( * ) PLANE_ANGLE_UNIT ( ) SI_UNIT ( $, .RADIAN. ) );
#51534 = ADVANCED_FACE ( 'NONE', ( #24985 ), #89942, .T. ) ;
#51535 = CARTESIAN_POINT ( 'NONE',  ( 103.3501304845727873, -29.99999999999998579, 116.5671668536019610 ) ) ;
#51536 = CARTESIAN_POINT ( 'NONE',  ( -82.78520545488002824, -25.62296466129009431, 148.0817344972886360 ) ) ;
#51537 = EDGE_LOOP ( 'NONE', ( #65079, #10852, #38389, #98763, #27961 ) ) ;
#51538 = FACE_OUTER_BOUND ( 'NONE', #3171, .T. ) ;
#51539 = CARTESIAN_POINT ( 'NONE',  ( 5.855777637195787477, 253.7810649675844559, -1.331220292256661830 ) ) ;
#51540 = CARTESIAN_POINT ( 'NONE',  ( 48.31638044378208718, -57.67957409234934119, 72.90164476747999345 ) ) ;
#51541 = CARTESIAN_POINT ( 'NONE',  ( -6.738141070038324187, -4.358126490537220121, -16.85492060643100842 ) ) ;
#51542 = CARTESIAN_POINT ( 'NONE',  ( 45.47726348208502145, 415.0353453662364700, 8.193293366016010992 ) ) ;
#51543 = VECTOR ( 'NONE', #57725, 1000.000000000000000 ) ;
#51544 = DIRECTION ( 'NONE',  ( 0.000000000000000000, -1.000000000000000000, 0.000000000000000000 ) ) ;
#51545 = VERTEX_POINT ( 'NONE', #100435 ) ;
#51546 = CARTESIAN_POINT ( 'NONE',  ( 31.23310005892718166, 439.6097802320569485, 23.20956534902767743 ) ) ;
#51547 = EDGE_CURVE ( 'NONE', #85853, #48371, #103726, .T. ) ;
#51548 = VERTEX_POINT ( 'NONE', #91305 ) ;
#51549 = ADVANCED_FACE ( 'NONE', ( #42199 ), #76153, .T. ) ;
#51550 = FACE_OUTER_BOUND ( 'NONE', #15927, .T. ) ;
#51551 = CARTESIAN_POINT ( 'NONE',  ( 6.840797686643921516, 41.85687274158131288, -69.25136110413218660 ) ) ;
#51552 = CARTESIAN_POINT ( 'NONE',  ( 50.18984356158254201, 50.00000000000000000, 38.51389699555568313 ) ) ;
#51553 = CARTESIAN_POINT ( 'NONE',  ( 4.999999999999961808, -13.16121988547497246, 12.48675270919411595 ) ) ;
#51554 = ORIENTED_EDGE ( 'NONE', *, *, #79646, .F. ) ;
#51555 = CARTESIAN_POINT ( 'NONE',  ( 111.8517878722345529, -60.00000000000001421, 162.0410978359878698 ) ) ;
#51557 = CARTESIAN_POINT ( 'NONE',  ( 24.33727547018983017, -60.35103628449270019, 35.15249607386650155 ) ) ;
#51556 = CARTESIAN_POINT ( 'NONE',  ( -83.30586888084981467, -14.21045842199414011, 194.5088339777059332 ) ) ;
#51558 = AXIS2_PLACEMENT_3D ( 'NONE', #27927, #94757, #20905 ) ;
#51559 = CARTESIAN_POINT ( 'NONE',  ( 82.80078431826154883, -37.99999999999994316, -11.83170434587093744 ) ) ;
#51560 = CARTESIAN_POINT ( 'NONE',  ( 6.162888688655347558, -3.752776749732574135, -6.500000000000001776 ) ) ;
#51561 = CARTESIAN_POINT ( 'NONE',  ( -40.76554704193952716, -53.34813757967989289, 42.49434450145254516 ) ) ;
#51562 = CARTESIAN_POINT ( 'NONE',  ( -30.50942973404921332, 18.64284798593271475, -23.36871039511863657 ) ) ;
#51563 = UNCERTAINTY_MEASURE_WITH_UNIT (LENGTH_MEASURE( 1.000000000000000082E-05 ), #92316, 'distance_accuracy_value', 'NONE');
#51564 = ORIENTED_EDGE ( 'NONE', *, *, #27936, .T. ) ;
#51565 = LINE ( 'NONE', #75306, #26834 ) ;
#51566 = VECTOR ( 'NONE', #96625, 1000.000000000000000 ) ;
#51567 = CARTESIAN_POINT ( 'NONE',  ( 0.000000000000000000, 115.0000000000000000, 0.000000000000000000 ) ) ;
#51568 = CARTESIAN_POINT ( 'NONE',  ( -13.76566278825922574, -57.17796501950922305, 29.56014984665260670 ) ) ;
#51569 = DIRECTION ( 'NONE',  ( -0.5735764363510497121, 0.8191520442889892450, 1.003171929053521665E-16 ) ) ;
#51570 = CARTESIAN_POINT ( 'NONE',  ( 6.445370176741849200, 7.262437273738760801, 1.101027156348632685 ) ) ;
#51571 = CARTESIAN_POINT ( 'NONE',  ( 8.011576988516077691, -0.1388693685375959608, 19.36711618773636445 ) ) ;
#51572 = ORIENTED_EDGE ( 'NONE', *, *, #64219, .F. ) ;
#51573 = CARTESIAN_POINT ( 'NONE',  ( -16.12754063828937490, 36.56084451123471979, -24.14283378817831860 ) ) ;
#51574 = ORIENTED_EDGE ( 'NONE', *, *, #476, .F. ) ;
#51575 = CARTESIAN_POINT ( 'NONE',  ( 96.50054790619491030, -30.00000000000008882, 191.2148438178596450 ) ) ;
#51576 = CARTESIAN_POINT ( 'NONE',  ( 28.42041225899258450, 41.23827639480541052, -68.38640372166889847 ) ) ;
#51577 = CARTESIAN_POINT ( 'NONE',  ( -5.477578620271511767, -81.83498560983899495, -2.459398706554656311 ) ) ;
#51578 = CARTESIAN_POINT ( 'NONE',  ( 81.97860939186369933, -30.00000000000000355, 33.72797324346839076 ) ) ;
#51579 = PLANE ( 'NONE',  #5389 ) ;
#51580 = ORIENTED_EDGE ( 'NONE', *, *, #73188, .F. ) ;
#51581 = CIRCLE ( 'NONE', #63696, 1.999999999999998224 ) ;
#51582 = ORIENTED_EDGE ( 'NONE', *, *, #55946, .F. ) ;
#51583 = ORIENTED_EDGE ( 'NONE', *, *, #101021, .F. ) ;
#51585 = ORIENTED_EDGE ( 'NONE', *, *, #37106, .T. ) ;
#51584 = CARTESIAN_POINT ( 'NONE',  ( -46.86466781827400041, 13.70365495135298772, -15.14281811549651913 ) ) ;
#51586 = LINE ( 'NONE', #85032, #99940 ) ;
#51587 = DIRECTION ( 'NONE',  ( 0.000000000000000000, 0.000000000000000000, 1.000000000000000000 ) ) ;
#51588 = CARTESIAN_POINT ( 'NONE',  ( 6.222742520105470021, 3.584500230190541092, -6.791463481567638460 ) ) ;
#51590 = VERTEX_POINT ( 'NONE', #635 ) ;
#51589 = STYLED_ITEM ( 'NONE', ( #97602 ), #33614 ) ;
#51592 = EDGE_CURVE ( 'NONE', #51812, #87574, #52049, .T. ) ;
#51591 = CARTESIAN_POINT ( 'NONE',  ( 9.999999999999989342, 49.99999999999999289, -86.30899693748767731 ) ) ;
#51593 = VERTEX_POINT ( 'NONE', #33602 ) ;
#51594 = FACE_OUTER_BOUND ( 'NONE', #71338, .T. ) ;
#51595 = CARTESIAN_POINT ( 'NONE',  ( 74.26595512671680410, -38.32811518277526375, 162.6728022224276913 ) ) ;
#51596 = CARTESIAN_POINT ( 'NONE',  ( -32.87517070013019094, 485.0717976019059847, 1.466424316699820096 ) ) ;
#51597 = CARTESIAN_POINT ( 'NONE',  ( 25.77264063226874313, 305.3150788826293933, 10.49011161150212068 ) ) ;
#51598 = CIRCLE ( 'NONE', #3408, 4.000000000000001776 ) ;
#51599 = CARTESIAN_POINT ( 'NONE',  ( -43.00000000000000000, 485.2629658518202405, -2.796394914059407100 ) ) ;
#51600 = ORIENTED_EDGE ( 'NONE', *, *, #79954, .F. ) ;
#51601 = CARTESIAN_POINT ( 'NONE',  ( 29.35771261243655061, 8.827287181787172088, -42.06472072717370736 ) ) ;
#51602 = CARTESIAN_POINT ( 'NONE',  ( 17.62428443205140383, 45.49731502040738462, -4.616218165346110958 ) ) ;
#51603 = CARTESIAN_POINT ( 'NONE',  ( 32.97364094493251940, 300.4786680927070392, 3.203698462821897408 ) ) ;
#51604 = EDGE_CURVE ( 'NONE', #47940, #58651, #84793, .T. ) ;
#51605 = CARTESIAN_POINT ( 'NONE',  ( 0.000000000000000000, 0.000000000000000000, 0.000000000000000000 ) ) ;
#51606 = CARTESIAN_POINT ( 'NONE',  ( -8.000000000000000000, -20.74999999999999289, -9.797174393178825657E-16 ) ) ;
#51607 = EDGE_LOOP ( 'NONE', ( #95369, #36851, #31672, #25221 ) ) ;
#51608 = CIRCLE ( 'NONE', #12032, 4.999999999999999112 ) ;
#51609 = PLANE ( 'NONE',  #47778 ) ;
#51610 = FACE_OUTER_BOUND ( 'NONE', #56957, .T. ) ;
#51611 = DIRECTION ( 'NONE',  ( 0.000000000000000000, 0.000000000000000000, 1.000000000000000000 ) ) ;
#51612 = FACE_OUTER_BOUND ( 'NONE', #87247, .T. ) ;
#51613 = CARTESIAN_POINT ( 'NONE',  ( 7.218596499961003055, 294.7245713411965085, 9.909955490001918221 ) ) ;
#51614 = CARTESIAN_POINT ( 'NONE',  ( -7.046357527897571416, 103.6938434939899594, -3.789683693877208270 ) ) ;
#51615 = MECHANICAL_DESIGN_GEOMETRIC_PRESENTATION_REPRESENTATION (  '', ( #67182 ), #24173 ) ;
#51616 = DIRECTION ( 'NONE',  ( -0.000000000000000000, -0.000000000000000000, -1.000000000000000000 ) ) ;
#51617 = CARTESIAN_POINT ( 'NONE',  ( 86.35266085468832387, -20.98688359306337148, 180.9796971926948004 ) ) ;
#51618 = CARTESIAN_POINT ( 'NONE',  ( 17.08200492518409774, 36.32755554593313008, -24.26548702208093999 ) ) ;
#51619 = EDGE_CURVE ( 'NONE', #53610, #89019, #36266, .T. ) ;
#51620 = VECTOR ( 'NONE', #48856, 1000.000000000000000 ) ;
#51621 = CARTESIAN_POINT ( 'NONE',  ( -8.420453562163482175, 123.3148673108831872, 5.000000000001271871 ) ) ;
#51622 = ORIENTED_EDGE ( 'NONE', *, *, #34419, .F. ) ;
#51623 = CARTESIAN_POINT ( 'NONE',  ( 71.90002237152832265, -57.67111777412542040, -33.97088182244272758 ) ) ;
#51624 = DIRECTION ( 'NONE',  ( 0.000000000000000000, 0.000000000000000000, 1.000000000000000000 ) ) ;
#51625 = DIRECTION ( 'NONE',  ( -1.000000000000000000, -1.224606353822377258E-16, -0.000000000000000000 ) ) ;
#51626 = DIRECTION ( 'NONE',  ( -1.000000000000000000, -1.224606353822377258E-16, -0.000000000000000000 ) ) ;
#51627 = ADVANCED_FACE ( 'NONE', ( #34146 ), #25534, .F. ) ;
#51628 = CARTESIAN_POINT ( 'NONE',  ( -86.45155040232437216, -29.99999999999999645, 67.06891508925755829 ) ) ;
#51629 = B_SPLINE_CURVE_WITH_KNOTS ( 'NONE', 3,
 ( #98035, #24187, #57032, #89947, #81829, #7954, #73754, #106650, #34808, #32802 ),
 .UNSPECIFIED., .F., .F.,
 ( 4, 2, 2, 2, 4 ),
 ( -1.267662083617060480E-05, 0.001114285917661883346, 0.002241248456159937019, 0.003368210994657990908, 0.004495173533156045231 ),
 .UNSPECIFIED. ) ;
#51630 = FACE_OUTER_BOUND ( 'NONE', #11258, .T. ) ;
#51631 = CARTESIAN_POINT ( 'NONE',  ( -2.325424218462540882, 7.317669739334965229, -7.030005583190789054 ) ) ;
#51632 = VECTOR ( 'NONE', #33211, 1000.000000000000000 ) ;
#51634 = CARTESIAN_POINT ( 'NONE',  ( 28.50099738913158376, 1.340359594676612611E-15, 0.000000000000000000 ) ) ;
#51633 = DIRECTION ( 'NONE',  ( -0.7071067811865390240, 8.659560562355038861E-17, -0.7071067811865561215 ) ) ;
#51635 = FILL_AREA_STYLE_COLOUR ( '', #36779 ) ;
#51636 = CARTESIAN_POINT ( 'NONE',  ( -35.22237514543125059, -33.10240969494732610, 34.19389076937522276 ) ) ;
#51637 = CARTESIAN_POINT ( 'NONE',  ( -34.34679764914316991, 491.0133751866271723, 12.01297952733263763 ) ) ;
#51638 = CARTESIAN_POINT ( 'NONE',  ( 18.91791044776121211, 46.00000000000000000, 62.18611311450883505 ) ) ;
#51639 = CARTESIAN_POINT ( 'NONE',  ( 44.48219350064427147, 478.0060774381361739, 1.937535957203245562 ) ) ;
#51640 = CARTESIAN_POINT ( 'NONE',  ( 39.38097750404882902, -24.68082471414068380, -30.42226529891207676 ) ) ;
#51641 = EDGE_CURVE ( 'NONE', #68449, #38628, #18485, .T. ) ;
#51642 = CARTESIAN_POINT ( 'NONE',  ( -26.23499765767613212, -42.95978904109873042, 32.63469194111196714 ) ) ;
#51643 = ORIENTED_EDGE ( 'NONE', *, *, #43138, .F. ) ;
#51644 = CARTESIAN_POINT ( 'NONE',  ( 6.560397950766611253, 9.829122060748870737, -2.451970031105678682 ) ) ;
#51645 = CARTESIAN_POINT ( 'NONE',  ( -20.07920920781616658, -35.99626565146032675, 30.40599871804820609 ) ) ;
#51646 = CARTESIAN_POINT ( 'NONE',  ( -55.42315763572941023, -28.56386927801018061, -26.45277240378572259 ) ) ;
#51648 = CARTESIAN_POINT ( 'NONE',  ( -66.60144316463728842, -60.22825214799080129, -27.67180546727933788 ) ) ;
#51647 = FACE_OUTER_BOUND ( 'NONE', #101574, .T. ) ;
#51649 = ORIENTED_EDGE ( 'NONE', *, *, #100243, .F. ) ;
#51650 = COLOUR_RGB ( '', 0.08235294, 0.09019608, 0.10196078) ;
#51651 = CARTESIAN_POINT ( 'NONE',  ( -35.98161575412628821, 437.4062335063961200, 4.370829238943763073 ) ) ;
#51652 = AXIS2_PLACEMENT_3D ( 'NONE', #52024, #86023, #19185 ) ;
#51653 = ORIENTED_EDGE ( 'NONE', *, *, #13119, .F. ) ;
#51654 = VECTOR ( 'NONE', #76435, 1000.000000000000000 ) ;
#51655 = CARTESIAN_POINT ( 'NONE',  ( -15.31761884737777990, -60.00000000000000711, -42.14637892441209033 ) ) ;
#51656 = ORIENTED_EDGE ( 'NONE', *, *, #3409, .F. ) ;
#51657 = FILL_AREA_STYLE ('',( #18263 ) ) ;
#51658 = CARTESIAN_POINT ( 'NONE',  ( -9.659790634495982076, 294.6522974485824875, -2.601814601459285115 ) ) ;
#51659 = CARTESIAN_POINT ( 'NONE',  ( 99.91689189414954342, -45.27234786626318908, 192.6820125696734181 ) ) ;
#51661 = CARTESIAN_POINT ( 'NONE',  ( -7.801777176595949825, -6.411720141873670009, -1.786991866639922932 ) ) ;
#51660 = CARTESIAN_POINT ( 'NONE',  ( 7.160273590795869225, 294.7244959282127184, -7.003631132636504830 ) ) ;
#51662 = VERTEX_POINT ( 'NONE', #92874 ) ;
#51663 = ORIENTED_EDGE ( 'NONE', *, *, #98009, .F. ) ;
#51664 = EDGE_CURVE ( 'NONE', #25507, #39953, #72690, .T. ) ;
#51665 = ORIENTED_EDGE ( 'NONE', *, *, #66250, .F. ) ;
#51666 = CARTESIAN_POINT ( 'NONE',  ( 25.06945282685627774, 307.6499839075243017, 10.57814702769852389 ) ) ;
#51667 = CIRCLE ( 'NONE', #29323, 4.000000000000000888 ) ;
#51668 = EDGE_CURVE ( 'NONE', #97524, #32062, #2255, .T. ) ;
#51669 = CARTESIAN_POINT ( 'NONE',  ( -39.45725925859406402, 460.7192990590703516, 2.112476274834657719 ) ) ;
#51670 = CARTESIAN_POINT ( 'NONE',  ( 15.42241126771897086, 46.21736870922993035, 5.091656527549089262 ) ) ;
#51671 = ORIENTED_EDGE ( 'NONE', *, *, #35001, .T. ) ;
#51672 = CARTESIAN_POINT ( 'NONE',  ( 59.41111111111111143, -3.309500000000000774, 4.475777889183797681E-16 ) ) ;
#51673 = CYLINDRICAL_SURFACE ( 'NONE', #10070, 4.250000000000000000 ) ;
#51674 = CARTESIAN_POINT ( 'NONE',  ( -94.70492387035963588, -59.99999999995124256, 24.66237146002972835 ) ) ;
#51675 = AXIS2_PLACEMENT_3D ( 'NONE', #62664, #39966, #72325 ) ;
#51676 = CARTESIAN_POINT ( 'NONE',  ( -42.23079339798739795, 461.4509360991310700, 2.027626716395849904 ) ) ;
#51677 = CARTESIAN_POINT ( 'NONE',  ( -35.74483125092430669, 413.6409941285803598, 6.029078300230034770 ) ) ;
#51678 = CARTESIAN_POINT ( 'NONE',  ( -7.070595406388543225, 41.16321361949651703, -58.51508551921422452 ) ) ;
#51679 = ADVANCED_FACE ( 'NONE', ( #93425 ), #75056, .F. ) ;
#51680 = CARTESIAN_POINT ( 'NONE',  ( -84.06615883987635129, -30.00000000000009592, -21.85610764691116259 ) ) ;
#51681 = CARTESIAN_POINT ( 'NONE',  ( -44.13785234221902698, 464.3950528659657948, 9.689702101754715358 ) ) ;
#51682 = CARTESIAN_POINT ( 'NONE',  ( -50.43059932419966884, -53.37294702884624087, 56.24277649152521263 ) ) ;
#51683 = AXIS2_PLACEMENT_3D ( 'NONE', #77324, #77854, #76247 ) ;
#51684 = ORIENTED_EDGE ( 'NONE', *, *, #80730, .T. ) ;
#51685 = DIRECTION ( 'NONE',  ( 0.000000000000000000, 1.000000000000000000, 0.000000000000000000 ) ) ;
#51686 = VERTEX_POINT ( 'NONE', #66285 ) ;
#51687 = CARTESIAN_POINT ( 'NONE',  ( 12.50000000000000711, 3.927497522143841291, -21.92086562379284587 ) ) ;
#51688 = CARTESIAN_POINT ( 'NONE',  ( -9.497389752370075655, 295.1492747691260092, -10.04143169208946240 ) ) ;
#51689 = TOROIDAL_SURFACE ( 'NONE', #101606, 12.00000000000000711, 3.000000000000000000 ) ;
#51690 = CARTESIAN_POINT ( 'NONE',  ( 0.000000000000000000, 0.000000000000000000, 5.000000000000000888 ) ) ;
#51691 = ORIENTED_EDGE ( 'NONE', *, *, #60992, .F. ) ;
#51692 = FACE_OUTER_BOUND ( 'NONE', #74581, .T. ) ;
#51693 = CARTESIAN_POINT ( 'NONE',  ( 83.38327456107505498, -38.79623963373321516, 197.2790430537241946 ) ) ;
#51694 = PRESENTATION_STYLE_ASSIGNMENT (( #50612 ) ) ;
#51695 = CARTESIAN_POINT ( 'NONE',  ( 4.073826509763722292, -48.95212347009485399, 104.5376934966453746 ) ) ;
#51696 = CARTESIAN_POINT ( 'NONE',  ( -18.46964424310625930, 302.6549491133945935, 9.895499654730381067 ) ) ;
#51697 = CARTESIAN_POINT ( 'NONE',  ( -72.41885610115939187, 42.00000000000000000, 55.65414010178468374 ) ) ;
#51698 = CARTESIAN_POINT ( 'NONE',  ( 89.15293829421764826, -30.00000000000000711, 188.9274208521591731 ) ) ;
#51699 = CARTESIAN_POINT ( 'NONE',  ( 43.79329400983225185, 434.3557490607465184, 12.18619556048155239 ) ) ;
#51700 = LINE ( 'NONE', #83538, #81135 ) ;
#51701 = EDGE_LOOP ( 'NONE', ( #15371, #11974, #106630 ) ) ;
#51702 = ORIENTED_EDGE ( 'NONE', *, *, #1562, .T. ) ;
#51703 = CARTESIAN_POINT ( 'NONE',  ( 51.87696231258184554, -39.50721492603066309, 54.02982920344263107 ) ) ;
#51704 = CARTESIAN_POINT ( 'NONE',  ( -44.32853450521363925, 435.2015765068597375, 12.56845903945290388 ) ) ;
#51705 = VECTOR ( 'NONE', #50817, 999.9999999999998863 ) ;
#51706 = CARTESIAN_POINT ( 'NONE',  ( 0.000000000000000000, 38.67090180175566871, -23.23666318551310539 ) ) ;
#51707 = ORIENTED_EDGE ( 'NONE', *, *, #36708, .F. ) ;
#51710 = EDGE_CURVE ( 'NONE', #33490, #30956, #71004, .T. ) ;
#51709 = B_SPLINE_CURVE_WITH_KNOTS ( 'NONE', 3,
 ( #33453, #26971, #59855, #66328, #25375, #92725, #18885, #58231, #81961, #66869, #8087, #74934, #40992, #73881, #106776, #32927, #98678, #11797, #78652, #61447 ),
 .UNSPECIFIED., .F., .F.,
 ( 4, 2, 2, 2, 2, 2, 2, 2, 2, 4 ),
 ( 0.003076783614208158761, 0.003581015465326142094, 0.004085247316444126295, 0.004589479167562109628, 0.005093711018680092961, 0.005597942869798077162, 0.005850058795357066660, 0.006102174720916056158, 0.006606406572034035155, 0.007110638423152015018 ),
 .UNSPECIFIED. ) ;
#51708 = CARTESIAN_POINT ( 'NONE',  ( -90.38342445295627670, -38.40159242213010771, -14.93373897757729374 ) ) ;
#51711 = VERTEX_POINT ( 'NONE', #91639 ) ;
#51712 =( NAMED_UNIT ( * ) PLANE_ANGLE_UNIT ( ) SI_UNIT ( $, .RADIAN. ) );
#51713 = CARTESIAN_POINT ( 'NONE',  ( 110.2498375325866107, -38.35601196224923370, 184.3325669443497645 ) ) ;
#51714 = CARTESIAN_POINT ( 'NONE',  ( 15.58050646327639299, 23.00052803995978223, 0.2687008445306368065 ) ) ;
#51715 = CARTESIAN_POINT ( 'NONE',  ( 85.39580779865164573, -52.71438213946019857, 25.13192279552427877 ) ) ;
#51716 = CARTESIAN_POINT ( 'NONE',  ( -13.50000000000000000, -7.794228634059985339, -1.205771365940065953 ) ) ;
#51717 = CARTESIAN_POINT ( 'NONE',  ( -25.91098795542547961, 306.7335490000789946, -8.585778581918489749 ) ) ;
#51718 = SURFACE_STYLE_USAGE ( .BOTH. , #92714 ) ;
#51719 = EDGE_CURVE ( 'NONE', #80223, #3039, #17752, .T. ) ;
#51720 = DIRECTION ( 'NONE',  ( -1.000000000000000000, -1.224606353822377258E-16, -0.000000000000000000 ) ) ;
#51721 = DIRECTION ( 'NONE',  ( 0.000000000000000000, 0.000000000000000000, 1.000000000000000000 ) ) ;
#51722 = CARTESIAN_POINT ( 'NONE',  ( 8.224467148767693914, 115.5412973725991748, 0.000000000000000000 ) ) ;
#51723 = ORIENTED_EDGE ( 'NONE', *, *, #30910, .F. ) ;
#51724 = EDGE_CURVE ( 'NONE', #30465, #59238, #69258, .T. ) ;
#51725 = CARTESIAN_POINT ( 'NONE',  ( 0.3345949520953953593, 37.19393312596059786, 27.29267445124407843 ) ) ;
#51726 = CARTESIAN_POINT ( 'NONE',  ( -33.95156263172580680, 464.5083255208629680, 6.608064661821540398 ) ) ;
#51727 = AXIS2_PLACEMENT_3D ( 'NONE', #32213, #40810, #47828 ) ;
#51728 = CARTESIAN_POINT ( 'NONE',  ( 60.14984002819952025, 6.856755485862130937E-15, 0.000000000000000000 ) ) ;
#51729 = ORIENTED_EDGE ( 'NONE', *, *, #11356, .F. ) ;
#51730 = CARTESIAN_POINT ( 'NONE',  ( -32.98783370188532160, 323.4213243428150690, -4.452354598022544074 ) ) ;
#51731 = CARTESIAN_POINT ( 'NONE',  ( -37.81576683240294301, 309.3149194722910806, 5.368762553532455684 ) ) ;
#51732 = LINE ( 'NONE', #76537, #89797 ) ;
#51733 = CARTESIAN_POINT ( 'NONE',  ( 5.656854249492378806, -23.18749999999999289, 5.656854249492381470 ) ) ;
#51734 = CARTESIAN_POINT ( 'NONE',  ( -1.469576158976823947E-15, -26.37499999999999645, 8.000000000000000000 ) ) ;
#51735 = SURFACE_STYLE_FILL_AREA ( #68475 ) ;
#51736 = MANIFOLD_SOLID_BREP ( 'Thicken1', #53176 ) ;
#51737 = CARTESIAN_POINT ( 'NONE',  ( -7.500000000000007105, -3.000000000000000000, -68.91429205785459544 ) ) ;
#51738 = ORIENTED_EDGE ( 'NONE', *, *, #19524, .T. ) ;
#51739 = CARTESIAN_POINT ( 'NONE',  ( 81.79764319078026347, -60.67315069769534830, 187.1424671695783104 ) ) ;
#51740 =( NAMED_UNIT ( * ) PLANE_ANGLE_UNIT ( ) SI_UNIT ( $, .RADIAN. ) );
#51741 = CARTESIAN_POINT ( 'NONE',  ( 29.66054107240687543, 1.482358050883964840E-15, 0.000000000000000000 ) ) ;
#51742 = ORIENTED_EDGE ( 'NONE', *, *, #50695, .T. ) ;
#51743 = CARTESIAN_POINT ( 'NONE',  ( -101.5804274888581205, -60.15496831279061496, 125.0268949860137155 ) ) ;
#51744 = VECTOR ( 'NONE', #14302, 1000.000000000000000 ) ;
#51745 = CARTESIAN_POINT ( 'NONE',  ( 0.000000000000000000, 0.000000000000000000, -10.00000000000000000 ) ) ;
#51746 = DIRECTION ( 'NONE',  ( 1.000000000000000000, 0.000000000000000000, -1.224646799147353207E-16 ) ) ;
#51747 = CARTESIAN_POINT ( 'NONE',  ( -36.78552755379869410, -31.92457971927218452, -37.73363741030753005 ) ) ;
#51748 =( BOUNDED_SURFACE ( )  B_SPLINE_SURFACE ( 3, 2, ( 
 ( #2807, #68638, #101516 ),
 ( #77239, #27674, #3355 ),
 ( #69166, #96611, #13011 ),
 ( #103632, #38913, #48030 ) ),
 .UNSPECIFIED., .F., .F., .T. ) 
 B_SPLINE_SURFACE_WITH_KNOTS ( ( 4, 4 ),
 ( 3, 3 ),
 ( 4.336808689942017736E-18, 0.001448708294673802226 ),
 ( 0.000000000000000000, 1.000000000000000000 ),
 .UNSPECIFIED. ) 
 GEOMETRIC_REPRESENTATION_ITEM ( )  RATIONAL_B_SPLINE_SURFACE ( (
 ( 1.000000000000000000, 0.7788880963805111524, 1.000000000000000000),
 ( 1.000000000000000000, 0.7852432470598105230, 1.000000000000000000),
 ( 1.000000000000000000, 0.7915643316727953849, 1.000000000000000000),
 ( 1.000000000000000000, 0.7978714159192913380, 1.000000000000000000) ) ) 
 REPRESENTATION_ITEM ( '' )  SURFACE ( )  );
#51749 = VECTOR ( 'NONE', #81147, 1000.000000000000227 ) ;
#51750 = EDGE_CURVE ( 'NONE', #93357, #47288, #104570, .T. ) ;
#51751 = PRESENTATION_LAYER_ASSIGNMENT (  '', '', ( #13866 ) ) ;
#51752 = CARTESIAN_POINT ( 'NONE',  ( 41.61328347345722989, -59.99999999999999289, 54.53347641298491766 ) ) ;
#51753 = CARTESIAN_POINT ( 'NONE',  ( 43.25463156771495221, -38.30615329582972350, 54.80495015273535131 ) ) ;
#51754 = CARTESIAN_POINT ( 'NONE',  ( 7.801642220026312025, 108.5879682614903174, 1.787233835843584417 ) ) ;
#51755 = CARTESIAN_POINT ( 'NONE',  ( 5.516412180249635533, -12.94324287202192991, 32.08767009249079649 ) ) ;
#51756 = ADVANCED_FACE ( 'NONE', ( #105629 ), #60791, .F. ) ;
#51758 = CARTESIAN_POINT ( 'NONE',  ( -13.60252275386366705, 22.67888446432363381, -2.545037732601225233 ) ) ;
#51757 = CARTESIAN_POINT ( 'NONE',  ( -32.60673480809711577, -34.12558338660269186, 42.27298281508674904 ) ) ;
#51759 = VECTOR ( 'NONE', #48011, 999.9999999999998863 ) ;
#51760 = CARTESIAN_POINT ( 'NONE',  ( 6.930002047096925466, 302.1778385079933855, -10.02505617572796659 ) ) ;
#51761 = CARTESIAN_POINT ( 'NONE',  ( 37.04388863813380794, 311.3287000699716032, 13.89786840526617517 ) ) ;
#51762 = EDGE_CURVE ( 'NONE', #101, #66410, #55991, .T. ) ;
#51763 = DIRECTION ( 'NONE',  ( -1.000000000000000000, -1.224606353822377258E-16, -0.000000000000000000 ) ) ;
#51764 = VERTEX_POINT ( 'NONE', #56535 ) ;
#51765 = DIRECTION ( 'NONE',  ( 1.000000000000000000, 0.000000000000000000, 0.000000000000000000 ) ) ;
#51766 = PRODUCT_DEFINITION_SHAPE ( 'NONE', 'NONE',  #73291 ) ;
#51767 = CARTESIAN_POINT ( 'NONE',  ( -1.935861021877891552, -59.99999999999999289, 39.63649550858829684 ) ) ;
#51768 = CARTESIAN_POINT ( 'NONE',  ( -13.50000000000000000, 7.794228634059985339, -11.79422863405993382 ) ) ;
#51769 = CARTESIAN_POINT ( 'NONE',  ( 0.000000000000000000, 0.000000000000000000, -6.724735318933162453 ) ) ;
#51770 = CARTESIAN_POINT ( 'NONE',  ( 12.93241622180732442, -60.22813012449146441, -36.57626181383834307 ) ) ;
#51771 = ORIENTED_EDGE ( 'NONE', *, *, #46495, .T. ) ;
#51772 = FACE_OUTER_BOUND ( 'NONE', #99248, .T. ) ;
#51773 = CARTESIAN_POINT ( 'NONE',  ( -41.43589798206021158, 484.8608140988944797, -3.494610779850012339 ) ) ;
#51774 = ORIENTED_EDGE ( 'NONE', *, *, #82938, .F. ) ;
#51775 = AXIS2_PLACEMENT_3D ( 'NONE', #33622, #74966, #16747 ) ;
#51776 = DIRECTION ( 'NONE',  ( -1.000000000000000000, -0.000000000000000000, -0.000000000000000000 ) ) ;
#51777 = B_SPLINE_CURVE_WITH_KNOTS ( 'NONE', 3,
 ( #31201, #22033, #38739, #5819, #78634, #54890, #70573, #71610, #103981, #61968, #14428, #96962, #94859, #37710, #72153, #47859 ),
 .UNSPECIFIED., .F., .F.,
 ( 4, 2, 2, 2, 2, 2, 2, 4 ),
 ( 0.000000000000000000, 0.0009812749226930392397, 0.001962549845386078479, 0.002943824768079117069, 0.003925099690772156091, 0.005887649536158235872, 0.006868924458851274895, 0.007850199381544313917 ),
 .UNSPECIFIED. ) ;
#51778 = DIRECTION ( 'NONE',  ( 0.000000000000000000, 0.000000000000000000, 1.000000000000000000 ) ) ;
#51779 = STYLED_ITEM ( 'NONE', ( #18319 ), #102887 ) ;
#51780 = FACE_OUTER_BOUND ( 'NONE', #34622, .T. ) ;
#51781 = CARTESIAN_POINT ( 'NONE',  ( -94.39104688558903433, -59.99999999999999289, 44.44594898355327928 ) ) ;
#51782 = DIRECTION ( 'NONE',  ( -1.000000000000000000, -0.000000000000000000, -0.000000000000000000 ) ) ;
#51783 = CARTESIAN_POINT ( 'NONE',  ( 7.922281120364393914, -4.573931137438281169, -8.047472243342934206 ) ) ;
#51784 = CARTESIAN_POINT ( 'NONE',  ( 35.56416567029047116, 496.2909070316903239, -10.19064917708978335 ) ) ;
#51785 = CARTESIAN_POINT ( 'NONE',  ( 39.69724611604618048, 460.7042697230090766, 2.103486822546470680 ) ) ;
#51787 = LINE ( 'NONE', #85229, #80430 ) ;
#51786 = CARTESIAN_POINT ( 'NONE',  ( 9.999999999999994671, -3.000000000000002665, -83.69100306252322241 ) ) ;
#51788 = CARTESIAN_POINT ( 'NONE',  ( -83.84580100612211595, -35.97236730127333715, 172.3106703699040168 ) ) ;
#51789 = VERTEX_POINT ( 'NONE', #47392 ) ;
#51790 = FACE_OUTER_BOUND ( 'NONE', #30706, .T. ) ;
#51791 = EDGE_LOOP ( 'NONE', ( #62059, #84591, #41437, #102429, #81941 ) ) ;
#51792 = ORIENTED_EDGE ( 'NONE', *, *, #101460, .F. ) ;
#51793 = CARTESIAN_POINT ( 'NONE',  ( -10.49999999997808331, -5.000000000000000000, -12.52300748972991506 ) ) ;
#51794 = CARTESIAN_POINT ( 'NONE',  ( -15.51786670351801689, -4.332661967059642016, 9.509450810728861114 ) ) ;
#51795 = ADVANCED_FACE ( 'NONE', ( #104035 ), #46867, .T. ) ;
#51796 = CARTESIAN_POINT ( 'NONE',  ( 7.715274834628325378E-15, 0.000000000000000000, -63.00000000000000000 ) ) ;
#51797 = ORIENTED_EDGE ( 'NONE', *, *, #106403, .F. ) ;
#51798 = VECTOR ( 'NONE', #63003, 1000.000000000000000 ) ;
#51799 = DIRECTION ( 'NONE',  ( -0.000000000000000000, 1.000000000000000000, -0.000000000000000000 ) ) ;
#51800 = CARTESIAN_POINT ( 'NONE',  ( -5.642946032546647395, -57.67118448875083203, -44.55159700680318480 ) ) ;
#51801 = CARTESIAN_POINT ( 'NONE',  ( 8.000113193197771366, -14.00022638645862827, -0.2613481123984672805 ) ) ;
#51802 = FACE_OUTER_BOUND ( 'NONE', #42856, .T. ) ;
#51803 = CARTESIAN_POINT ( 'NONE',  ( 0.000000000000000000, 0.000000000000000000, 0.000000000000000000 ) ) ;
#51804 = CARTESIAN_POINT ( 'NONE',  ( -13.60728112438141402, -51.55816952290514621, 30.29609480636782592 ) ) ;
#51805 = CARTESIAN_POINT ( 'NONE',  ( -5.000000000000000000, -14.73409751812503110, 12.39902340069096098 ) ) ;
#51806 = EDGE_CURVE ( 'NONE', #51764, #88628, #55475, .T. ) ;
#51807 = CARTESIAN_POINT ( 'NONE',  ( 86.99610535363679276, -14.21045842199441012, 24.11248255592787615 ) ) ;
#51808 = CARTESIAN_POINT ( 'NONE',  ( -78.95080019145578376, -30.00000000000002842, 188.4626203831212479 ) ) ;
#51809 = CARTESIAN_POINT ( 'NONE',  ( -60.30957961906158005, -42.96557303354831703, 74.70452531835056220 ) ) ;
#51810 = ORIENTED_EDGE ( 'NONE', *, *, #7193, .F. ) ;
#51811 = CARTESIAN_POINT ( 'NONE',  ( 5.744562646538028616, 12.99999999999999289, 4.000000000000000000 ) ) ;
#51812 = VERTEX_POINT ( 'NONE', #46347 ) ;
#51813 = CARTESIAN_POINT ( 'NONE',  ( -105.4132686368380689, -60.15493453134271817, 186.0986387432675713 ) ) ;
#51814 = CARTESIAN_POINT ( 'NONE',  ( -4.413588872740235480, -9.563952367645422115, 5.751921314332418156 ) ) ;
#51815 = DIRECTION ( 'NONE',  ( 0.000000000000000000, 0.000000000000000000, 1.000000000000000000 ) ) ;
#51816 = VERTEX_POINT ( 'NONE', #54402 ) ;
#51818 = STYLED_ITEM ( 'NONE', ( #85493 ), #7605 ) ;
#51817 = CARTESIAN_POINT ( 'NONE',  ( -81.48333467678395436, -59.99999999999998579, 197.5873724345494509 ) ) ;
#51819 = CARTESIAN_POINT ( 'NONE',  ( 37.40542853975937732, 25.53140870284743613, -13.45617127781092215 ) ) ;
#51820 = CARTESIAN_POINT ( 'NONE',  ( -7.188101187500002709, -21.68750000204838813, 2.977408999572648707 ) ) ;
#51821 = AXIS2_PLACEMENT_3D ( 'NONE', #88615, #6623, #79977 ) ;
#51822 = CARTESIAN_POINT ( 'NONE',  ( 12.61650669486618881, 1.474610560812782335E-15, 0.000000000000000000 ) ) ;
#51823 = CARTESIAN_POINT ( 'NONE',  ( 17.01584901091794322, 0.000000000000000000, 1.113195845613775825 ) ) ;
#51824 = CARTESIAN_POINT ( 'NONE',  ( -12.29798915171474150, -4.463815859614853387, -12.75153713776978037 ) ) ;
#51825 = CIRCLE ( 'NONE', #89725, 9.000000000000000000 ) ;
#51826 = FACE_OUTER_BOUND ( 'NONE', #48996, .T. ) ;
#51827 = CARTESIAN_POINT ( 'NONE',  ( 30.00000000000000000, 0.000000000000000000, 0.000000000000000000 ) ) ;
#51828 = CARTESIAN_POINT ( 'NONE',  ( -16.02154979717254335, 46.08966533359959072, -4.311187973113333349 ) ) ;
#51829 = EDGE_CURVE ( 'NONE', #94251, #21876, #79236, .T. ) ;
#51830 = SURFACE_SIDE_STYLE ('',( #2747 ) ) ;
#51831 = CARTESIAN_POINT ( 'NONE',  ( -29.12107580442651056, -25.58914361729731368, 30.36964868577932819 ) ) ;
#51832 = AXIS2_PLACEMENT_3D ( 'NONE', #52843, #77121, #85767 ) ;
#51833 = CARTESIAN_POINT ( 'NONE',  ( 2.449319673264149344, 21.02564536029728970, 6.561398256599556333 ) ) ;
#51834 = CARTESIAN_POINT ( 'NONE',  ( 43.59138291442800295, -25.70414336249979570, 38.53719198648085609 ) ) ;
#51835 = CARTESIAN_POINT ( 'NONE',  ( -32.62137895416891098, 486.7356100976077187, 7.182248123790627048 ) ) ;
#51836 = AXIS2_PLACEMENT_3D ( 'NONE', #63637, #96526, #22658 ) ;
#51837 = CARTESIAN_POINT ( 'NONE',  ( -5.744562646538029504, 12.99999999999999289, 4.000000000000000000 ) ) ;
#51839 = EDGE_CURVE ( 'NONE', #88140, #60788, #80284, .T. ) ;
#51838 = CARTESIAN_POINT ( 'NONE',  ( -87.07432190745933553, -38.59215479556766581, 199.5759947477305616 ) ) ;
#51840 = ORIENTED_EDGE ( 'NONE', *, *, #56373, .F. ) ;
#51842 = DIRECTION ( 'NONE',  ( 0.000000000000000000, 1.000000000000000000, 0.000000000000000000 ) ) ;
#51841 = CARTESIAN_POINT ( 'NONE',  ( 81.78041284440412539, -38.35659437205359978, -25.37965657400610553 ) ) ;
#51843 = CARTESIAN_POINT ( 'NONE',  ( 78.89378607809999266, -60.00000000000006395, 163.2895204445849799 ) ) ;
#51844 = B_SPLINE_CURVE_WITH_KNOTS ( 'NONE', 3,
 ( #28990, #102288, #85050, #51601, #76403, #94753, #52132, #86135, #84522, #20374, #28434, #77491, #11668, #45137, #35465, #2516, #69930, #36008, #92596, #60268, #12208, #60789, #103360, #11129, #44601, #94205, #10608, #93677, #19830, #43530 ),
 .UNSPECIFIED., .F., .F.,
 ( 4, 2, 2, 2, 2, 2, 2, 2, 2, 2, 2, 2, 2, 2, 4 ),
 ( 0.0004001071830457286088, 0.0008634720163662153516, 0.001326836849686701932, 0.002253566516327680080, 0.003180296182968658011, 0.004107025849609637243, 0.005033755516250615174, 0.005497120349571107609, 0.005960485182891598309, 0.006423850016212089876, 0.006655532432872336528, 0.006887214849532581444, 0.007118897266192828095, 0.007350579682853073012, 0.007813944516173556773 ),
 .UNSPECIFIED. ) ;
#51845 = CARTESIAN_POINT ( 'NONE',  ( -18.98212999821499380, 49.45283421538681523, 61.95133595785922864 ) ) ;
#51846 = CARTESIAN_POINT ( 'NONE',  ( -6.943035977205679998, 41.50417750172036335, -58.81491712266881677 ) ) ;
#51847 = CARTESIAN_POINT ( 'NONE',  ( -48.02835407290533709, 9.771516447483559631, -16.85535821593460426 ) ) ;
#51848 = CARTESIAN_POINT ( 'NONE',  ( 23.73746414932995208, 1.482358050883964840E-15, 0.000000000000000000 ) ) ;
#51849 = CARTESIAN_POINT ( 'NONE',  ( -25.63293091691854286, 308.3345217834615823, 9.742415824227602883 ) ) ;
#51850 = CARTESIAN_POINT ( 'NONE',  ( 7.499999999999999112, -1.443375672974070989, -7.063244554130000630 ) ) ;
#51851 = CARTESIAN_POINT ( 'NONE',  ( 106.7471793853078168, -60.00000000000000000, 197.4229364724118057 ) ) ;
#51852 = FACE_OUTER_BOUND ( 'NONE', #105119, .T. ) ;
#51853 = DIRECTION ( 'NONE',  ( 0.000000000000000000, -1.000000000000000000, 0.000000000000000000 ) ) ;
#51854 = EDGE_LOOP ( 'NONE', ( #73260, #9593 ) ) ;
#51855 = ADVANCED_FACE ( 'NONE', ( #30723 ), #62471, .T. ) ;
#51856 = CARTESIAN_POINT ( 'NONE',  ( 1.468822083365114439, -49.97157980006149103, 101.6459669435612625 ) ) ;
#51857 = CARTESIAN_POINT ( 'NONE',  ( -75.15565943195267096, -30.00000000000000711, -17.90412972589801655 ) ) ;
#51858 = ORIENTED_EDGE ( 'NONE', *, *, #31044, .T. ) ;
#51860 = CARTESIAN_POINT ( 'NONE',  ( 7.000000000000000000, 0.000000000000000000, -6.275264681066861527 ) ) ;
#51859 = CARTESIAN_POINT ( 'NONE',  ( -92.42649569189924819, -38.49805319420887173, 201.0465977874510770 ) ) ;
#51861 = CARTESIAN_POINT ( 'NONE',  ( 7.126148245860624009, 41.12758397993106740, -58.55282951229289523 ) ) ;
#51862 = CARTESIAN_POINT ( 'NONE',  ( 2.977408999572651815, -16.81250000204838457, 7.188101187500000933 ) ) ;
#51863 = CARTESIAN_POINT ( 'NONE',  ( 10.48543666094731996, -5.000000000000002665, -78.95657223723277696 ) ) ;
#51864 = AXIS2_PLACEMENT_3D ( 'NONE', #1435, #82371, #58645 ) ;
#51865 = CARTESIAN_POINT ( 'NONE',  ( -3.313708498984798467, -12.21875000409676915, -7.999999999999961808 ) ) ;
#51867 = ORIENTED_EDGE ( 'NONE', *, *, #72982, .T. ) ;
#51866 = CARTESIAN_POINT ( 'NONE',  ( -40.36578697173862196, 468.8173651557589210, -0.04324207066571782859 ) ) ;
#51868 = CARTESIAN_POINT ( 'NONE',  ( 80.43770127149109328, -56.88658794661572671, 173.6145532136999634 ) ) ;
#51869 = CARTESIAN_POINT ( 'NONE',  ( -41.46910480218704009, 484.7338956289818270, -3.418960549715579500 ) ) ;
#51870 = CARTESIAN_POINT ( 'NONE',  ( 5.193195059372482212E-16, -7.895640089090903757, -6.564402953523731377 ) ) ;
#51871 = ORIENTED_EDGE ( 'NONE', *, *, #68893, .F. ) ;
#51872 = CARTESIAN_POINT ( 'NONE',  ( 34.10284876471455817, 5.000000000000002665, 0.000000000000000000 ) ) ;
#51873 = DIRECTION ( 'NONE',  ( 1.000000000000000000, 1.224606353822377258E-16, 0.000000000000000000 ) ) ;
#51874 = CARTESIAN_POINT ( 'NONE',  ( 38.64245533733815563, 27.44901796531306459, -11.54891632625754028 ) ) ;
#51875 = DIRECTION ( 'NONE',  ( 1.000000000000000000, 0.000000000000000000, 0.000000000000000000 ) ) ;
#51876 = CARTESIAN_POINT ( 'NONE',  ( -5.981691436642410764, 253.9726909919410787, -0.5384679144502781956 ) ) ;
#51877 = CARTESIAN_POINT ( 'NONE',  ( 0.9891189538826573591, 17.70032527776562858, 49.73254565116481984 ) ) ;
#51878 = CARTESIAN_POINT ( 'NONE',  ( 8.593983530299054152, -1.221393525206185826, 15.49134170070576211 ) ) ;
#51879 = EDGE_CURVE ( 'NONE', #94099, #46925, #65923, .T. ) ;
#51880 = ORIENTED_EDGE ( 'NONE', *, *, #61911, .F. ) ;
#51881 = AXIS2_PLACEMENT_3D ( 'NONE', #73723, #88865, #65650 ) ;
#51882 = CARTESIAN_POINT ( 'NONE',  ( 3.400000000000000355, 0.000000000000000000, -0.4455245229258316120 ) ) ;
#51883 = CARTESIAN_POINT ( 'NONE',  ( 4.491425985184478442, 18.64284798592898795, 38.16738163467809386 ) ) ;
#51884 = CARTESIAN_POINT ( 'NONE',  ( 87.07919189661382120, -31.70057368356062000, 187.6106092519108870 ) ) ;
#51885 = ADVANCED_FACE ( 'NONE', ( #58694 ), #65715, .T. ) ;
#51886 = DIRECTION ( 'NONE',  ( -0.5735764363510494901, -0.8191520442889894671, 0.000000000000000000 ) ) ;
#51887 = CARTESIAN_POINT ( 'NONE',  ( -2.977408999572650039, -26.18750000204838813, -7.188101187500001821 ) ) ;
#51888 = DIRECTION ( 'NONE',  ( 0.000000000000000000, 1.000000000000000000, 0.000000000000000000 ) ) ;
#51889 = CARTESIAN_POINT ( 'NONE',  ( 5.290067270632158980, 51.34639538792298197, -8.531152949374604333 ) ) ;
#51890 = B_SPLINE_CURVE_WITH_KNOTS ( 'NONE', 3,
 ( #100045, #73088, #56379, #89313, #7838, #15408, #48296, #81194 ),
 .UNSPECIFIED., .F., .F.,
 ( 4, 2, 2, 4 ),
 ( 0.02179091314793462145, 0.02376333058066962267, 0.02573574801340462737, 0.02968058287887462982 ),
 .UNSPECIFIED. ) ;
#51891 = CARTESIAN_POINT ( 'NONE',  ( 14.58934900096333465, 5.487773041241286620, 6.668063844691364928 ) ) ;
#51892 = CONTEXT_DEPENDENT_SHAPE_REPRESENTATION ( #3968, #6362 ) ;
#51893 = ORIENTED_EDGE ( 'NONE', *, *, #106598, .T. ) ;
#51895 = ADVANCED_FACE ( 'NONE', ( #81341 ), #59000, .T. ) ;
#51894 = CIRCLE ( 'NONE', #55348, 4.000000000000007105 ) ;
#51896 = LINE ( 'NONE', #86430, #26817 ) ;
#51897 = CARTESIAN_POINT ( 'NONE',  ( 14.91858118607497374, 2.271260765197548532E-16, 15.00000000000000000 ) ) ;
#51898 = CIRCLE ( 'NONE', #101797, 4.000000000000001776 ) ;
#51899 = CARTESIAN_POINT ( 'NONE',  ( -10.43542583693917969, 6.878147458890213173, -5.000000000000404121 ) ) ;
#51900 = CARTESIAN_POINT ( 'NONE',  ( 44.35000000000000142, 1.533819458162526451E-15, 0.000000000000000000 ) ) ;
#51901 = ORIENTED_EDGE ( 'NONE', *, *, #41286, .F. ) ;
#51902 = CIRCLE ( 'NONE', #27798, 3.309500000000001663 ) ;
#51903 = CARTESIAN_POINT ( 'NONE',  ( 37.50030914627209455, 491.1170837247063332, 12.27619315344390039 ) ) ;
#51904 = CARTESIAN_POINT ( 'NONE',  ( 10.74465425723776058, 49.99999999999999289, -95.72854256507095272 ) ) ;
#51905 = ORIENTED_EDGE ( 'NONE', *, *, #73333, .F. ) ;
#51906 = MANIFOLD_SOLID_BREP ( 'Fillet1', #60131 ) ;
#51908 = CARTESIAN_POINT ( 'NONE',  ( 6.249999999999998224, 8.000000000000000000, 0.000000000000000000 ) ) ;
#51907 = AXIS2_PLACEMENT_3D ( 'NONE', #12341, #52809, #11805 ) ;
#51909 = CARTESIAN_POINT ( 'NONE',  ( -0.9991018963761647553, 8.903979680119203266, -51.25442813699677913 ) ) ;
#51910 = CARTESIAN_POINT ( 'NONE',  ( 9.165151389911679658, 105.0000000000000142, -4.000000000000001776 ) ) ;
#51911 = CARTESIAN_POINT ( 'NONE',  ( -111.0770631305250902, -59.99999999999998579, 186.8983870106532379 ) ) ;
#51912 = CARTESIAN_POINT ( 'NONE',  ( 9.048917774133558467, 43.82457158262040053, -14.35241448611411919 ) ) ;
#51913 = CARTESIAN_POINT ( 'NONE',  ( 52.56483885390523625, 40.83906611471594061, -38.23529411764706509 ) ) ;
#51914 = FACE_OUTER_BOUND ( 'NONE', #56477, .T. ) ;
#51915 = CARTESIAN_POINT ( 'NONE',  ( -84.21710172597578037, -46.56676066005127268, 185.3566345002555806 ) ) ;
#51916 = ORIENTED_EDGE ( 'NONE', *, *, #21221, .T. ) ;
#51917 = CARTESIAN_POINT ( 'NONE',  ( 3.313708498984761608, -25.71874999999999645, -8.000000000000000000 ) ) ;
#51918 = EDGE_CURVE ( 'NONE', #34061, #92662, #34451, .T. ) ;
#51919 = CARTESIAN_POINT ( 'NONE',  ( 3.769311339735795574, -1.074854658864329959, 104.1674216685381396 ) ) ;
#51920 = CARTESIAN_POINT ( 'NONE',  ( -82.72858650987951989, -37.82906654770548016, 2.983319424909649076 ) ) ;
#51921 = CIRCLE ( 'NONE', #48534, 1.000000000000000666 ) ;
#51922 = DIRECTION ( 'NONE',  ( 0.000000000000000000, 0.000000000000000000, 1.000000000000000000 ) ) ;
#51923 = CARTESIAN_POINT ( 'NONE',  ( -16.48255526477243293, 43.52995101198734318, 6.657797401561652784 ) ) ;
#51924 = AXIS2_PLACEMENT_3D ( 'NONE', #78229, #5919, #28658 ) ;
#51925 = CARTESIAN_POINT ( 'NONE',  ( 22.15188447042185160, 295.0129022001648309, 1.971242154165463223 ) ) ;
#51926 = CARTESIAN_POINT ( 'NONE',  ( 42.40769230769231513, -4.171999999999999709, 5.616230220889763424E-16 ) ) ;
#51927 = CARTESIAN_POINT ( 'NONE',  ( -57.69562748396144514, 41.99999999999999289, -15.50526908263377734 ) ) ;
#51928 = ADVANCED_FACE ( 'NONE', ( #67321 ), #57593, .F. ) ;
#51929 = CARTESIAN_POINT ( 'NONE',  ( 76.85420403038403947, -14.21045842199429288, 149.6289235591555666 ) ) ;
#51930 = CARTESIAN_POINT ( 'NONE',  ( -18.71440884245025060, 61.34242035161803841, -9.357204421225127078 ) ) ;
#51931 = CARTESIAN_POINT ( 'NONE',  ( -86.55941870227799484, -14.21045842199434439, 7.758091717749037386 ) ) ;
#51932 = CIRCLE ( 'NONE', #3689, 4.000000000000001776 ) ;
#51933 = CARTESIAN_POINT ( 'NONE',  ( -68.76518295970697636, -36.01231797821088776, 95.92058326348774244 ) ) ;
#51934 = ORIENTED_EDGE ( 'NONE', *, *, #100170, .T. ) ;
#51935 = CARTESIAN_POINT ( 'NONE',  ( 103.1541778469752160, -29.99999999999992184, 197.4146557462016176 ) ) ;
#51936 = CARTESIAN_POINT ( 'NONE',  ( 26.06643700053798796, -59.99999999999019451, 43.91432386791814935 ) ) ;
#51937 = EDGE_LOOP ( 'NONE', ( #95735, #67112 ) ) ;
#51938 = CARTESIAN_POINT ( 'NONE',  ( 8.559508646656349029, 51.83514083332403999, -1.531152949374623873 ) ) ;
#51939 = CARTESIAN_POINT ( 'NONE',  ( 7.188101187500000933, -23.93750000204838457, -2.977408999572650483 ) ) ;
#51940 = CARTESIAN_POINT ( 'NONE',  ( -5.094000037296078531, -7.553658762287765782, -3.174960020027659535 ) ) ;
#51941 = ORIENTED_EDGE ( 'NONE', *, *, #90598, .F. ) ;
#51942 = CARTESIAN_POINT ( 'NONE',  ( 43.88846153846154152, 1.411358822780289120E-15, 0.000000000000000000 ) ) ;
#51943 = ORIENTED_EDGE ( 'NONE', *, *, #97953, .T. ) ;
#51944 = CARTESIAN_POINT ( 'NONE',  ( 7.135888613855538409, 41.99999999999999289, -71.74865085751123672 ) ) ;
#51945 =( NAMED_UNIT ( * ) SI_UNIT ( $, .STERADIAN. ) SOLID_ANGLE_UNIT ( ) );
#51946 = CARTESIAN_POINT ( 'NONE',  ( -71.84928664377656560, -60.00000000002933831, 174.4758671435405404 ) ) ;
#51947 = DIRECTION ( 'NONE',  ( 0.000000000000000000, 1.000000000000000000, 0.000000000000000000 ) ) ;
#51948 = CARTESIAN_POINT ( 'NONE',  ( 2.977408999572650927, -11.37500000204838813, -7.188101187500001821 ) ) ;
#51949 = CARTESIAN_POINT ( 'NONE',  ( -1.469576158976823947E-15, -17.56250000409676915, 8.000000000000000000 ) ) ;
#51950 = DIRECTION ( 'NONE',  ( 0.000000000000000000, 0.000000000000000000, 1.000000000000000000 ) ) ;
#51951 = CARTESIAN_POINT ( 'NONE',  ( -1.308996937483428491, 49.99999999999999289, -95.00000000000001421 ) ) ;
#51952 = CARTESIAN_POINT ( 'NONE',  ( 7.500000000000001776, -4.330127018922199866, -0.9999999999999974465 ) ) ;
#51953 = DIRECTION ( 'NONE',  ( -0.8191520442889974607, 0.000000000000000000, -0.5735764363510380548 ) ) ;
#51954 = EDGE_CURVE ( 'NONE', #92559, #96331, #67627, .T. ) ;
#51955 = UNCERTAINTY_MEASURE_WITH_UNIT (LENGTH_MEASURE( 1.000000000000000082E-05 ), #52994, 'distance_accuracy_value', 'NONE');
#51956 = ORIENTED_EDGE ( 'NONE', *, *, #75469, .F. ) ;
#51957 = CARTESIAN_POINT ( 'NONE',  ( 4.211261491277978664, -1.586805402942760068, 103.7733746176805880 ) ) ;
#51959 = CARTESIAN_POINT ( 'NONE',  ( 31.90715827978913310, -22.14410705931457457, 30.64563635488976701 ) ) ;
#51958 = CARTESIAN_POINT ( 'NONE',  ( 43.50377727019363050, 435.9167426301696082, 18.24083946424737590 ) ) ;
#51960 = CARTESIAN_POINT ( 'NONE',  ( -11.19959342721765694, -8.673617379884035472E-16, 19.43146043914803300 ) ) ;
#51961 = VERTEX_POINT ( 'NONE', #98071 ) ;
#51962 = ADVANCED_FACE ( 'NONE', ( #82958 ), #24222, .F. ) ;
#51963 = CARTESIAN_POINT ( 'NONE',  ( -5.036189803708991164, 47.99999999999998579, -93.73786388354257326 ) ) ;
#51964 = VERTEX_POINT ( 'NONE', #94253 ) ;
#51965 = CARTESIAN_POINT ( 'NONE',  ( -25.85238267732653128, 35.07671371647713698, -8.660559307860188127 ) ) ;
#51966 = CARTESIAN_POINT ( 'NONE',  ( 18.86650669486618881, -3.999999999999998224, 0.000000000000000000 ) ) ;
#51967 = CARTESIAN_POINT ( 'NONE',  ( -43.52075891743670866, 484.7805561108188499, 4.063293749114545328 ) ) ;
#51968 =( NAMED_UNIT ( * ) PLANE_ANGLE_UNIT ( ) SI_UNIT ( $, .RADIAN. ) );
#51969 = CARTESIAN_POINT ( 'NONE',  ( 31.99294114632900232, 464.8457910465707528, 12.87241426108012732 ) ) ;
#51970 = CARTESIAN_POINT ( 'NONE',  ( 33.00000000000000000, 435.0774731480752280, 11.67986145722084501 ) ) ;
#51971 = ORIENTED_EDGE ( 'NONE', *, *, #44167, .F. ) ;
#51972 = CARTESIAN_POINT ( 'NONE',  ( 92.39395720610478691, -60.00000000000000000, 0.2350603988867105976 ) ) ;
#51973 = FILL_AREA_STYLE_COLOUR ( '', #84294 ) ;
#51975 =( LENGTH_UNIT ( ) NAMED_UNIT ( * ) SI_UNIT ( .MILLI., .METRE. ) );
#51974 = PRESENTATION_LAYER_ASSIGNMENT (  '', '', ( #36557 ) ) ;
#51976 =( NAMED_UNIT ( * ) PLANE_ANGLE_UNIT ( ) SI_UNIT ( $, .RADIAN. ) );
#51977 =( GEOMETRIC_REPRESENTATION_CONTEXT ( 3 ) GLOBAL_UNCERTAINTY_ASSIGNED_CONTEXT ( ( #63576 ) ) GLOBAL_UNIT_ASSIGNED_CONTEXT ( ( #57167, #89556, #24837 ) ) REPRESENTATION_CONTEXT ( 'NONE', 'WORKASPACE' ) );
#51978 = CARTESIAN_POINT ( 'NONE',  ( -6.952098965573305200, 40.29466765805469919, -71.12438203485694999 ) ) ;
#51979 = LINE ( 'NONE', #43899, #52987 ) ;
#51980 = VERTEX_POINT ( 'NONE', #27963 ) ;
#51981 = CARTESIAN_POINT ( 'NONE',  ( -104.3020865355773736, -30.00000000000412825, 196.2433964757412639 ) ) ;
#51982 = ORIENTED_EDGE ( 'NONE', *, *, #91312, .F. ) ;
#51983 = ORIENTED_EDGE ( 'NONE', *, *, #28654, .F. ) ;
#51984 = CARTESIAN_POINT ( 'NONE',  ( 7.619701877737480977, 81.82557840467232779, -2.447562251315978710 ) ) ;
#51985 = CARTESIAN_POINT ( 'NONE',  ( 5.819846122303833802, -6.321060697774956161, -2.051601713727018161 ) ) ;
#51986 = CARTESIAN_POINT ( 'NONE',  ( -15.97423913551834040, 35.08248256844603219, -22.07470797814806929 ) ) ;
#51987 = FACE_BOUND ( 'NONE', #63072, .T. ) ;
#51988 = CARTESIAN_POINT ( 'NONE',  ( 83.33347542712400013, -45.27651489616857106, -13.82556416722983528 ) ) ;
#51990 = AXIS2_PLACEMENT_3D ( 'NONE', #99429, #66018, #74628 ) ;
#51989 = CARTESIAN_POINT ( 'NONE',  ( -41.03101037122678463, 313.1827267563339774, -5.626772567029049377 ) ) ;
#51991 = PLANE ( 'NONE',  #35308 ) ;
#51992 = CARTESIAN_POINT ( 'NONE',  ( -17.95175771543782162, 45.00000000000000711, 62.60109665436401372 ) ) ;
#51993 = CARTESIAN_POINT ( 'NONE',  ( -19.73463816634111012, 304.7971333121958537, 8.925379062039116462 ) ) ;
#51994 = ORIENTED_EDGE ( 'NONE', *, *, #76989, .T. ) ;
#51995 = CARTESIAN_POINT ( 'NONE',  ( 6.500000000000000000, 1.602771114417276932, -0.1495523863686145094 ) ) ;
#51996 = VECTOR ( 'NONE', #35619, 1000.000000000000000 ) ;
#51997 = ORIENTED_EDGE ( 'NONE', *, *, #60913, .F. ) ;
#51998 = FACE_OUTER_BOUND ( 'NONE', #57092, .T. ) ;
#51999 = CARTESIAN_POINT ( 'NONE',  ( 5.700000000000000178, 5.388445916248354013E-16, 4.400000000000000355 ) ) ;
#52001 = ORIENTED_EDGE ( 'NONE', *, *, #38678, .F. ) ;
#52000 = CARTESIAN_POINT ( 'NONE',  ( 6.542048114965975714, 51.42613907887827196, 7.322510233794829126 ) ) ;
#52002 = CARTESIAN_POINT ( 'NONE',  ( 74.53424881736971486, -46.43315849507841619, 123.7959196446912387 ) ) ;
#52003 = ORIENTED_EDGE ( 'NONE', *, *, #26695, .T. ) ;
#52004 = CARTESIAN_POINT ( 'NONE',  ( 5.446579913478287516, -51.29466139981784778, 39.89783452207186087 ) ) ;
#52005 = DIRECTION ( 'NONE',  ( 1.000000000000000000, 0.000000000000000000, 0.000000000000000000 ) ) ;
#52006 = CARTESIAN_POINT ( 'NONE',  ( -2.977408999572654480, -24.12500000204838813, 7.188101187499999156 ) ) ;
#52007 = CARTESIAN_POINT ( 'NONE',  ( -73.23646197434321437, -57.64251361348243563, 182.9240549372742635 ) ) ;
#52008 = ADVANCED_FACE ( 'NONE', ( #3105 ), #84565, .T. ) ;
#52009 = ORIENTED_EDGE ( 'NONE', *, *, #89656, .T. ) ;
#52010 = CIRCLE ( 'NONE', #67507, 3.309500000000001663 ) ;
#52011 = EDGE_CURVE ( 'NONE', #99675, #28267, #40035, .T. ) ;
#52012 = CARTESIAN_POINT ( 'NONE',  ( -25.45921313960911903, 43.62243447522785544, -75.49936859611810291 ) ) ;
#52013 = CIRCLE ( 'NONE', #93380, 5.000000000000010658 ) ;
#52014 = CARTESIAN_POINT ( 'NONE',  ( 105.7766044031187107, -60.15129442481250521, 184.0536137966112733 ) ) ;
#52015 = CARTESIAN_POINT ( 'NONE',  ( 6.392325331821059109, 51.30797053396300100, -7.876575602207272375 ) ) ;
#52016 = ADVANCED_FACE ( 'NONE', ( #78055 ), #50349, .T. ) ;
#52017 = COLOUR_RGB ( '', 0.09019608, 0.27058824, 0.51372549) ;
#52018 = DIRECTION ( 'NONE',  ( 1.000000000000000000, 1.224606353822377258E-16, 0.000000000000000000 ) ) ;
#52019 = CARTESIAN_POINT ( 'NONE',  ( -3.313708498984765161, -19.15625000409676915, 7.999999999999998224 ) ) ;
#52020 = CARTESIAN_POINT ( 'NONE',  ( -51.59293570839133736, -29.92165899869593559, 49.34611889700588705 ) ) ;
#52021 = CARTESIAN_POINT ( 'NONE',  ( 6.249999999999998224, -4.618802153517012954, -8.000000000000001776 ) ) ;
#52022 = EDGE_CURVE ( 'NONE', #38119, #29354, #96875, .T. ) ;
#52023 = CARTESIAN_POINT ( 'NONE',  ( 9.830769230769229594, 1.411358822780289120E-15, 0.000000000000000000 ) ) ;
#52024 = CARTESIAN_POINT ( 'NONE',  ( 66.26095113931063452, 6.856755485862130937E-15, 0.000000000000000000 ) ) ;
#52025 = DIRECTION ( 'NONE',  ( 1.000000000000000000, 0.000000000000000000, 0.000000000000000000 ) ) ;
#52026 = CARTESIAN_POINT ( 'NONE',  ( 33.89250494191496443, 463.6575930728430990, 6.993601543837892898 ) ) ;
#52027 = ORIENTED_EDGE ( 'NONE', *, *, #23962, .T. ) ;
#52028 = CARTESIAN_POINT ( 'NONE',  ( -5.428831668361731033, 41.92214390794531198, -59.12797028773363905 ) ) ;
#52029 = ADVANCED_FACE ( 'NONE', ( #86704 ), #74598, .T. ) ;
#52030 = CARTESIAN_POINT ( 'NONE',  ( 12.34835181856063002, -4.332967528434596538, -12.86601580078908214 ) ) ;
#52031 = LINE ( 'NONE', #26219, #99710 ) ;
#52032 = CARTESIAN_POINT ( 'NONE',  ( -86.40106122215911455, -30.00000000000000355, 180.9903452954047509 ) ) ;
#52033 = B_SPLINE_CURVE_WITH_KNOTS ( 'NONE', 3,
 ( #18241, #84016, #43032, #59756, #75921, #67832, #100722, #18791 ),
 .UNSPECIFIED., .F., .F.,
 ( 4, 2, 2, 4 ),
 ( 0.003797433802554441972, 0.004743183970586237891, 0.005688934138618033376, 0.007580434474681623479 ),
 .UNSPECIFIED. ) ;
#52034 = VERTEX_POINT ( 'NONE', #103913 ) ;
#52035 = CARTESIAN_POINT ( 'NONE',  ( 38.09999999999998721, 0.000000000000000000, 0.000000000000000000 ) ) ;
#52036 = CARTESIAN_POINT ( 'NONE',  ( 77.70728701152813755, -57.51519683822058226, 196.1582150947566845 ) ) ;
#52038 = CARTESIAN_POINT ( 'NONE',  ( 46.00000000000000000, 438.2055348970465616, 15.52909715622263676 ) ) ;
#52037 = FACE_OUTER_BOUND ( 'NONE', #92162, .T. ) ;
#52039 = CARTESIAN_POINT ( 'NONE',  ( 28.37604781422512090, -28.97374409063350598, -38.24945775106650103 ) ) ;
#52040 = DIRECTION ( 'NONE',  ( 0.000000000000000000, 0.9676758637755492609, -0.2521971900443079062 ) ) ;
#52041 = CARTESIAN_POINT ( 'NONE',  ( -43.89370568756214652, 435.4157859805903286, 16.19551141317008813 ) ) ;
#52042 = CARTESIAN_POINT ( 'NONE',  ( -42.28790913546334451, -59.99999999999999289, 55.62912243266985257 ) ) ;
#52043 = CARTESIAN_POINT ( 'NONE',  ( -55.22048556080177661, 48.00000000000000000, 34.80214219306111545 ) ) ;
#52044 = CARTESIAN_POINT ( 'NONE',  ( -86.53326020941184993, -28.12733637824134547, 185.0956260656611505 ) ) ;
#52045 = ORIENTED_EDGE ( 'NONE', *, *, #76810, .F. ) ;
#52046 = CARTESIAN_POINT ( 'NONE',  ( 36.66358481845913531, 432.5585790697741686, 4.915382580107980459 ) ) ;
#52047 = CARTESIAN_POINT ( 'NONE',  ( -0.9943172959230506258, -29.03115895393441193, 28.72817645192477798 ) ) ;
#52048 = DIRECTION ( 'NONE',  ( -0.000000000000000000, -0.000000000000000000, 1.000000000000000000 ) ) ;
#52049 = CIRCLE ( 'NONE', #28012, 8.000000000000014211 ) ;
#52050 = CARTESIAN_POINT ( 'NONE',  ( 86.96164706429843250, -39.85521162617677504, 189.1638891629380623 ) ) ;
#52051 = CARTESIAN_POINT ( 'NONE',  ( -42.41055444770296390, 353.4000580228727131, 15.28812778342764034 ) ) ;
#52052 = ORIENTED_EDGE ( 'NONE', *, *, #53684, .T. ) ;
#52053 = EDGE_CURVE ( 'NONE', #33830, #4002, #78573, .T. ) ;
#52054 = CARTESIAN_POINT ( 'NONE',  ( -36.70797521953156206, 381.7145783656985714, 5.219800535707618039 ) ) ;
#52055 = CARTESIAN_POINT ( 'NONE',  ( 40.22681104634839500, 489.7629721959603444, 10.97561085253236968 ) ) ;
#52056 = CARTESIAN_POINT ( 'NONE',  ( 0.08491295131515702588, 27.29656849860388235, 40.75000000000002132 ) ) ;
#52057 = CARTESIAN_POINT ( 'NONE',  ( -30.90161637171721765, 8.443258198712127793, -41.14563328228313566 ) ) ;
#52058 = CIRCLE ( 'NONE', #28019, 9.500000000000000000 ) ;
#52059 = CARTESIAN_POINT ( 'NONE',  ( 21.29975379448945816, 294.8969325209483827, -1.990407376643369641 ) ) ;
#52060 = CARTESIAN_POINT ( 'NONE',  ( 35.69739812508499455, 430.4862580793411553, 4.964222856391316441 ) ) ;
#52061 = EDGE_CURVE ( 'NONE', #22313, #78629, #55289, .T. ) ;
#52062 = EDGE_CURVE ( 'NONE', #1547, #60518, #24380, .T. ) ;
#52063 = CARTESIAN_POINT ( 'NONE',  ( 8.559508646656350805, 53.96349637827587031, -1.531152949374623651 ) ) ;
#52064 = CARTESIAN_POINT ( 'NONE',  ( 96.14436826854903018, -60.00000000000009237, 39.43554979140174765 ) ) ;
#52065 = CARTESIAN_POINT ( 'NONE',  ( -80.60743116781320339, -39.50081370003077552, 149.7882430904484181 ) ) ;
#52066 = ORIENTED_EDGE ( 'NONE', *, *, #91802, .T. ) ;
#52067 = DIRECTION ( 'NONE',  ( -0.000000000000000000, 1.000000000000000000, -0.000000000000000000 ) ) ;
#52068 = CARTESIAN_POINT ( 'NONE',  ( 0.000000000000000000, -30.00000000000000000, 0.000000000000000000 ) ) ;
#52069 = CARTESIAN_POINT ( 'NONE',  ( 29.76422793413452439, -57.68363811005358599, 45.14079408021506623 ) ) ;
#52070 = CARTESIAN_POINT ( 'NONE',  ( -5.075741750048029743, -4.332638003024074536, -17.09621982684887698 ) ) ;
#52071 = CARTESIAN_POINT ( 'NONE',  ( 36.41659902574616581, 335.0122255936540228, -2.184171530108547810 ) ) ;
#52072 = CARTESIAN_POINT ( 'NONE',  ( 44.29288495124914249, 463.9154455111800530, 8.171315969404531643 ) ) ;
#52073 = ORIENTED_EDGE ( 'NONE', *, *, #97820, .T. ) ;
#52074 = CARTESIAN_POINT ( 'NONE',  ( 5.290067270632161645, 53.47475093287481229, -8.531152949374595451 ) ) ;
#52075 = CARTESIAN_POINT ( 'NONE',  ( 32.09911992168216699, 438.9232547152093957, 23.66653216045977359 ) ) ;
#52076 = EDGE_LOOP ( 'NONE', ( #94196, #60835, #87145, #56976, #89785 ) ) ;
#52077 = DIRECTION ( 'NONE',  ( 0.000000000000000000, 0.000000000000000000, 1.000000000000000000 ) ) ;
#52078 = ADVANCED_FACE ( 'NONE', ( #31650 ), #28159, .T. ) ;
#52079 =( BOUNDED_SURFACE ( )  B_SPLINE_SURFACE ( 2, 3, ( 
 ( #90427, #25187, #49421, #33805, #82324, #74754, #8435, #58598, #99562, #24652, #41335, #17077, #41866, #65620, #64564, #74227, #99024, #304, #98502, #97432, #58045, #90968, #25742, #49953, #97979, #81247, #834, #48355, #23593, #82862, #66682, #89373, #7363, #50476 ),
 ( #89891, #6838, #40275, #15461, #73151, #106053, #65081, #73695, #24132, #56977, #7896, #19779, #67748, #1928, #9485, #92546, #3007, #100635, #51006, #52610, #19254, #61262, #2465, #28388, #44548, #18693, #34879, #27873, #27339, #60217, #77437, #52083, #11080, #93083 ),
 ( #101708, #68830, #1384, #35414, #59665, #85539, #59132, #42396, #84996, #11619, #51552, #60738, #75291, #3551, #44005, #36490, #76892, #35958, #83923, #102237, #34352, #94150, #84465, #67226, #69358, #26795, #10558, #68283, #43475, #76352, #93626, #101179, #20321, #83388 ) ),
 .UNSPECIFIED., .F., .F., .F. ) 
 B_SPLINE_SURFACE_WITH_KNOTS ( ( 3, 3 ),
 ( 4, 2, 2, 2, 2, 2, 2, 2, 2, 2, 2, 2, 2, 2, 2, 2, 4 ),
 ( 0.000000000000000000, 1.000000000000000000 ),
 ( 0.9419214012998449181, 1.216880307836088360, 1.491839214372332023, 1.766798120908575465, 2.041757027444818906, 2.316715933981062570, 2.591674840517305789, 2.866633747053549452, 3.141592653589793116, 3.416551560126036780, 3.691510466662280443, 3.966469373198524107, 4.241428279734767770, 4.516387186271010989, 4.791346092807254209, 5.066304999343497428, 5.341263905879741536 ),
 .UNSPECIFIED. ) 
 GEOMETRIC_REPRESENTATION_ITEM ( )  RATIONAL_B_SPLINE_SURFACE ( (
 ( 1.000000000000000000, 1.000000000000000000, 1.000000000000000000, 1.000000000000000000, 1.000000000000000000, 1.000000000000000000, 1.000000000000000000, 1.000000000000000000, 1.000000000000000000, 1.000000000000000000, 1.000000000000000000, 1.000000000000000000, 1.000000000000000000, 1.000000000000000000, 1.000000000000000000, 1.000000000000000000, 1.000000000000000000, 1.000000000000000000, 1.000000000000000000, 1.000000000000000000, 1.000000000000000000, 1.000000000000000000, 1.000000000000000000, 1.000000000000000000, 1.000000000000000000, 1.000000000000000000, 1.000000000000000000, 1.000000000000000000, 1.000000000000000000, 1.000000000000000000, 1.000000000000000000, 1.000000000000000000, 1.000000000000000000, 1.000000000000000000),
 ( 1.857142857142858317, 1.857142857142858317, 1.857142857142858317, 1.857142857142858317, 1.857142857142858317, 1.857142857142858317, 1.857142857142858317, 1.857142857142858317, 1.857142857142858317, 1.857142857142858317, 1.857142857142858317, 1.857142857142858317, 1.857142857142858317, 1.857142857142858317, 1.857142857142858317, 1.857142857142858317, 1.857142857142858317, 1.857142857142858317, 1.857142857142858317, 1.857142857142858317, 1.857142857142858317, 1.857142857142858317, 1.857142857142858317, 1.857142857142858317, 1.857142857142858317, 1.857142857142858317, 1.857142857142858317, 1.857142857142858317, 1.857142857142858317, 1.857142857142858317, 1.857142857142858317, 1.857142857142858317, 1.857142857142858317, 1.857142857142858317),
 ( 1.000000000000000000, 1.000000000000000000, 1.000000000000000000, 1.000000000000000000, 1.000000000000000000, 1.000000000000000000, 1.000000000000000000, 1.000000000000000000, 1.000000000000000000, 1.000000000000000000, 1.000000000000000000, 1.000000000000000000, 1.000000000000000000, 1.000000000000000000, 1.000000000000000000, 1.000000000000000000, 1.000000000000000000, 1.000000000000000000, 1.000000000000000000, 1.000000000000000000, 1.000000000000000000, 1.000000000000000000, 1.000000000000000000, 1.000000000000000000, 1.000000000000000000, 1.000000000000000000, 1.000000000000000000, 1.000000000000000000, 1.000000000000000000, 1.000000000000000000, 1.000000000000000000, 1.000000000000000000, 1.000000000000000000, 1.000000000000000000) ) ) 
 REPRESENTATION_ITEM ( '' )  SURFACE ( )  );
#52080 = STYLED_ITEM ( 'NONE', ( #71908 ), #95383 ) ;
#52081 = CARTESIAN_POINT ( 'NONE',  ( -12.39578842395469138, 8.431745484731994367, -12.16229915940865070 ) ) ;
#52082 = DIRECTION ( 'NONE',  ( 1.000000000000000000, -0.000000000000000000, -0.000000000000000000 ) ) ;
#52083 = CARTESIAN_POINT ( 'NONE',  ( -58.90678327790940472, 50.00000000004006750, -28.11551192219710771 ) ) ;
#52084 = CARTESIAN_POINT ( 'NONE',  ( 2.680426334985284598, -7.322430019223747699, -13.10127437669147099 ) ) ;
#52085 = EDGE_CURVE ( 'NONE', #25416, #96331, #2567, .T. ) ;
#52086 = DIRECTION ( 'NONE',  ( 0.000000000000000000, 0.000000000000000000, -1.000000000000000000 ) ) ;
#52087 = ORIENTED_EDGE ( 'NONE', *, *, #103113, .T. ) ;
#52088 = CARTESIAN_POINT ( 'NONE',  ( 91.32602593890536014, -59.99999999999998579, -16.10466224646018674 ) ) ;
#52089 = VECTOR ( 'NONE', #62738, 1000.000000000000000 ) ;
#52091 = CARTESIAN_POINT ( 'NONE',  ( 22.50217560053253507, -39.47492995735613164, 31.31568985205594657 ) ) ;
#52090 = CARTESIAN_POINT ( 'NONE',  ( -73.20331151331558317, -59.99999999999998579, 185.6225630369678470 ) ) ;
#52093 = CARTESIAN_POINT ( 'NONE',  ( 121.1901574356003124, 4.501353321498349658, 60.59507871780019883 ) ) ;
#52092 = PRODUCT_DEFINITION_CONTEXT ( 'detailed design', #34237, 'design' ) ;
#52094 = LINE ( 'NONE', #58607, #15540 ) ;
#52095 = CARTESIAN_POINT ( 'NONE',  ( -34.57919986246837141, -60.30355936026654717, 39.05315648927861361 ) ) ;
#52096 = UNCERTAINTY_MEASURE_WITH_UNIT (LENGTH_MEASURE( 1.000000000000000082E-05 ), #79866, 'distance_accuracy_value', 'NONE');
#52097 = ORIENTED_EDGE ( 'NONE', *, *, #94904, .T. ) ;
#52098 = CARTESIAN_POINT ( 'NONE',  ( 0.000000000000000000, 70.00000000000000000, -5.999999999999998224 ) ) ;
#52099 = LINE ( 'NONE', #58059, #104238 ) ;
#52100 = CARTESIAN_POINT ( 'NONE',  ( -13.97203307284001994, -57.87174520061537208, 26.07838388608699631 ) ) ;
#52101 = DIRECTION ( 'NONE',  ( 0.000000000000000000, 1.000000000000000000, 0.000000000000000000 ) ) ;
#52102 = EDGE_CURVE ( 'NONE', #34913, #54018, #65584, .T. ) ;
#52103 = CARTESIAN_POINT ( 'NONE',  ( 8.000086790516061086, -60.99982641893993929, 0.2639471549312821241 ) ) ;
#52104 = ORIENTED_EDGE ( 'NONE', *, *, #51349, .F. ) ;
#52105 =( LENGTH_UNIT ( ) NAMED_UNIT ( * ) SI_UNIT ( .MILLI., .METRE. ) );
#52106 = ORIENTED_EDGE ( 'NONE', *, *, #18042, .T. ) ;
#52107 = CARTESIAN_POINT ( 'NONE',  ( 97.93634479608400056, -29.99999999999999289, 190.5932743339873809 ) ) ;
#52108 = DIRECTION ( 'NONE',  ( 0.000000000000000000, 0.000000000000000000, -1.000000000000000000 ) ) ;
#52109 = CARTESIAN_POINT ( 'NONE',  ( -4.497472161260645862, -84.45777453374053323, -3.972129482042464410 ) ) ;
#52110 = CARTESIAN_POINT ( 'NONE',  ( 80.76301881924163695, -29.99999999999999645, 11.31298429570228059 ) ) ;
#52111 = DIRECTION ( 'NONE',  ( 0.1659550938513567886, -0.9861333108788017388, 8.636585917856486324E-17 ) ) ;
#52112 = ORIENTED_EDGE ( 'NONE', *, *, #35616, .F. ) ;
#52113 = ORIENTED_EDGE ( 'NONE', *, *, #96371, .F. ) ;
#52114 = ORIENTED_EDGE ( 'NONE', *, *, #85377, .F. ) ;
#52115 = CARTESIAN_POINT ( 'NONE',  ( -32.12756478236646984, 464.8250811501316093, 14.60600970021982725 ) ) ;
#52116 = FACE_OUTER_BOUND ( 'NONE', #65350, .T. ) ;
#52117 = CARTESIAN_POINT ( 'NONE',  ( -16.53810334270205828, 303.5675058441541978, 9.876558506355554101 ) ) ;
#52118 = CARTESIAN_POINT ( 'NONE',  ( 5.191472769733073811, -12.64091576718949028, -3.014900733016760537 ) ) ;
#52119 = CARTESIAN_POINT ( 'NONE',  ( -16.64348903516526335, 43.75610143575153899, -4.157797401561264650 ) ) ;
#52120 = CARTESIAN_POINT ( 'NONE',  ( 12.79230769230769305, 1.411358822780289120E-15, 0.000000000000000000 ) ) ;
#52121 = DIRECTION ( 'NONE',  ( 0.000000000000000000, 0.000000000000000000, -1.000000000000000000 ) ) ;
#52122 = ORIENTED_EDGE ( 'NONE', *, *, #84834, .T. ) ;
#52123 = CARTESIAN_POINT ( 'NONE',  ( -9.999999999999989342, 49.99999999999999289, -86.30899693748770574 ) ) ;
#52124 = ORIENTED_EDGE ( 'NONE', *, *, #94914, .T. ) ;
#52125 = PRESENTATION_STYLE_ASSIGNMENT (( #69397 ) ) ;
#52126 = CARTESIAN_POINT ( 'NONE',  ( 71.26571211989046617, -38.32808976662677480, 141.5686193886610624 ) ) ;
#52127 = CARTESIAN_POINT ( 'NONE',  ( 32.04846564072990134, 435.5722017075208896, 16.73368519115310704 ) ) ;
#52128 = CARTESIAN_POINT ( 'NONE',  ( 24.04521816055709138, 295.4566507460422145, 10.06661448227953493 ) ) ;
#52129 = DIRECTION ( 'NONE',  ( 0.000000000000000000, 0.000000000000000000, 1.000000000000000000 ) ) ;
#52130 = CIRCLE ( 'NONE', #62535, 3.309500000000001663 ) ;
#52131 = VERTEX_POINT ( 'NONE', #106022 ) ;
#52132 = CARTESIAN_POINT ( 'NONE',  ( 28.98676785243906906, 9.652684557211529182, -41.90074509620651355 ) ) ;
#52133 = CARTESIAN_POINT ( 'NONE',  ( 13.50000000000000533, -7.794228634059982674, -11.79422863405993382 ) ) ;
#52134 = AXIS2_PLACEMENT_3D ( 'NONE', #13957, #23689, #80821 ) ;
#52135 = CARTESIAN_POINT ( 'NONE',  ( 36.70900294270256126, 306.3085992329407645, 4.617960540507793255 ) ) ;
#52136 = DIRECTION ( 'NONE',  ( 0.9788760387920678596, 0.000000000000000000, -0.2044546421061400610 ) ) ;
#52137 = EDGE_CURVE ( 'NONE', #48559, #81772, #66646, .T. ) ;
#52138 = CARTESIAN_POINT ( 'NONE',  ( -8.000000000000001776, -20.65624999999999289, 3.313708498984759387 ) ) ;
#52139 = ORIENTED_EDGE ( 'NONE', *, *, #16953, .T. ) ;
#52140 = DIRECTION ( 'NONE',  ( 0.9746329792208491272, 0.000000000000000000, 0.2238091951084492937 ) ) ;
#52141 = PRESENTATION_STYLE_ASSIGNMENT (( #3613 ) ) ;
#52142 = FILL_AREA_STYLE_COLOUR ( '', #764 ) ;
#52143 = CARTESIAN_POINT ( 'NONE',  ( 42.77633007798412024, 465.0956601428450767, 12.68100826444438667 ) ) ;
#52144 = CARTESIAN_POINT ( 'NONE',  ( 0.000000000000000000, 0.000000000000000000, 4.000000000000000000 ) ) ;
#52145 = EDGE_CURVE ( 'NONE', #71499, #88866, #19257, .T. ) ;
#52146 = CARTESIAN_POINT ( 'NONE',  ( -7.986711519608431509, 101.0263809637656607, -0.5300249774147618442 ) ) ;
#52147 = EDGE_CURVE ( 'NONE', #53546, #94586, #88933, .T. ) ;
#52148 = CARTESIAN_POINT ( 'NONE',  ( -0.2813450144774459760, 7.667988119308860817, -6.122077150241857169 ) ) ;
#52149 =( REPRESENTATION_RELATIONSHIP ('NONE','NONE', #69581, #22667 ) REPRESENTATION_RELATIONSHIP_WITH_TRANSFORMATION ( #41686 )SHAPE_REPRESENTATION_RELATIONSHIP( ) );
#52150 = CARTESIAN_POINT ( 'NONE',  ( 86.21467851622986700, -50.15124133650150640, 191.0468867715541990 ) ) ;
#52151 = CARTESIAN_POINT ( 'NONE',  ( 17.97174518249911657, 36.40624878439879808, -23.34175835912210317 ) ) ;
#52152 = CARTESIAN_POINT ( 'NONE',  ( -7.939583658491363494, 97.05573068114591706, 0.000000000000000000 ) ) ;
#52153 = ORIENTED_EDGE ( 'NONE', *, *, #60706, .T. ) ;
#52154 = CARTESIAN_POINT ( 'NONE',  ( 63.90509369011976304, -57.67098025992571309, -36.62925744095688430 ) ) ;
#52155 = DIRECTION ( 'NONE',  ( 0.5735764363510462704, 0.8191520442889915765, 0.000000000000000000 ) ) ;
#52156 = CARTESIAN_POINT ( 'NONE',  ( 13.09999999999999787, 1.533819458162526451E-15, 0.000000000000000000 ) ) ;
#52157 = ADVANCED_FACE ( 'NONE', ( #23561 ), #7862, .F. ) ;
#52158 = FACE_OUTER_BOUND ( 'NONE', #26840, .T. ) ;
#52159 = EDGE_CURVE ( 'NONE', #43619, #11977, #17582, .T. ) ;
#52160 =( GEOMETRIC_REPRESENTATION_CONTEXT ( 3 ) GLOBAL_UNCERTAINTY_ASSIGNED_CONTEXT ( ( #76141 ) ) GLOBAL_UNIT_ASSIGNED_CONTEXT ( ( #23130, #78667, #39307 ) ) REPRESENTATION_CONTEXT ( 'NONE', 'WORKASPACE' ) );
#52161 = CARTESIAN_POINT ( 'NONE',  ( -84.31746037670764338, -29.99999999999999645, 52.99187934968279023 ) ) ;
#52162 = STYLED_ITEM ( 'NONE', ( #79323 ), #94732 ) ;
#52163 = FILL_AREA_STYLE ('',( #3089 ) ) ;
#52164 = CARTESIAN_POINT ( 'NONE',  ( 20.89024399768744189, -57.67230926853248718, 42.33697424510430807 ) ) ;
#52166 = FACE_OUTER_BOUND ( 'NONE', #67104, .T. ) ;
#52165 = CARTESIAN_POINT ( 'NONE',  ( -9.165151389911699198, 249.7326484439287810, -4.000000000000002665 ) ) ;
#52167 = CARTESIAN_POINT ( 'NONE',  ( -51.48757442383521976, 38.95383793070303824, -37.45149417477430376 ) ) ;
#52168 = DIRECTION ( 'NONE',  ( -1.000000000000000000, -0.000000000000000000, -0.000000000000000000 ) ) ;
#52169 = CARTESIAN_POINT ( 'NONE',  ( -36.49104508226669452, 491.8392457932882849, 12.58580469730132201 ) ) ;
#52170 = CARTESIAN_POINT ( 'NONE',  ( -10.00000000000000000, 15.00000000000000000, 4.397168787612342200 ) ) ;
#52171 = CARTESIAN_POINT ( 'NONE',  ( 67.48317336153286305, -1.232595164407830946E-29, 4.000000000000007105 ) ) ;
#52172 = CARTESIAN_POINT ( 'NONE',  ( 64.59048453740965101, -29.71741133510901278, -23.23533048826496383 ) ) ;
#52173 = CARTESIAN_POINT ( 'NONE',  ( -25.30535910738106509, -18.61086395607065569, 28.23931188293136785 ) ) ;
#52174 = ORIENTED_EDGE ( 'NONE', *, *, #104594, .T. ) ;
#52175 = CARTESIAN_POINT ( 'NONE',  ( 27.10511071441198894, 36.88665068479745912, 7.556984339683237906 ) ) ;
#52176 = CARTESIAN_POINT ( 'NONE',  ( 48.02835407290504577, -1.200000000000000030E-05, -15.60535821593549954 ) ) ;
#52177 = CARTESIAN_POINT ( 'NONE',  ( -16.50652937410865562, -25.55084766554285736, 28.36507869232989520 ) ) ;
#52179 = CARTESIAN_POINT ( 'NONE',  ( 1.093414209075683985, 36.52532583549212575, -29.11109415026225378 ) ) ;
#52178 = SURFACE_SIDE_STYLE ('',( #77532 ) ) ;
#52180 = ORIENTED_EDGE ( 'NONE', *, *, #59396, .T. ) ;
#52181 = FILL_AREA_STYLE_COLOUR ( '', #59909 ) ;
#52182 = VERTEX_POINT ( 'NONE', #57470 ) ;
#52183 = CARTESIAN_POINT ( 'NONE',  ( 0.000000000000000000, -8.673617379884035472E-16, -17.01589776168603407 ) ) ;
#52184 = ADVANCED_FACE ( 'NONE', ( #50442 ), #43585, .T. ) ;
#52185 = CARTESIAN_POINT ( 'NONE',  ( 38.86638200451619696, 0.000000000000000000, 5.000000000000002665 ) ) ;
#52186 = CARTESIAN_POINT ( 'NONE',  ( 0.4053525175236804556, 3.145852061456246851, 6.499999999999998224 ) ) ;
#52187 = ORIENTED_EDGE ( 'NONE', *, *, #72556, .F. ) ;
#52188 = DIRECTION ( 'NONE',  ( -0.000000000000000000, -1.000000000000000000, -0.000000000000000000 ) ) ;
#52189 = DIRECTION ( 'NONE',  ( 0.5735764363510466035, -0.8191520442889914655, 1.003171929053524500E-16 ) ) ;
#52190 = CARTESIAN_POINT ( 'NONE',  ( 102.0322780741121846, -60.20636929944893012, 194.1630386048543926 ) ) ;
#52191 = AXIS2_PLACEMENT_3D ( 'NONE', #87793, #29587, #86744 ) ;
#52193 = CARTESIAN_POINT ( 'NONE',  ( -3.352941176470600304, -1.200583151104954283, 104.5794940929807524 ) ) ;
#52192 = DIRECTION ( 'NONE',  ( -1.000000000000000000, -1.224606353822377258E-16, -0.000000000000000000 ) ) ;
#52194 = ORIENTED_EDGE ( 'NONE', *, *, #83343, .F. ) ;
#52195 = TOROIDAL_SURFACE ( 'NONE', #57425, 8.500000000000000000, 0.5000000000000000000 ) ;
#52196 = VERTEX_POINT ( 'NONE', #41305 ) ;
#52197 = AXIS2_PLACEMENT_3D ( 'NONE', #27834, #26762, #67716 ) ;
#52198 = ORIENTED_EDGE ( 'NONE', *, *, #49809, .F. ) ;
#52199 = CARTESIAN_POINT ( 'NONE',  ( 23.63920041808693995, 304.8825889122297212, 10.16203760377671017 ) ) ;
#52200 = EDGE_CURVE ( 'NONE', #49037, #46369, #7723, .T. ) ;
#52201 = CARTESIAN_POINT ( 'NONE',  ( -13.50000000000000178, 0.6589394956329809316, -13.00000000000000178 ) ) ;
#52202 = CARTESIAN_POINT ( 'NONE',  ( 37.85084083633367413, 437.2249973798734572, 3.569182825063074382 ) ) ;
#52203 = ORIENTED_EDGE ( 'NONE', *, *, #102203, .T. ) ;
#52204 = CARTESIAN_POINT ( 'NONE',  ( 32.94021323899734455, 485.0599191339525191, 5.361609822540892800 ) ) ;
#52205 = FACE_OUTER_BOUND ( 'NONE', #34659, .T. ) ;
#52206 = CARTESIAN_POINT ( 'NONE',  ( -2.499999999981197707, -21.99834632368703069, -30.53960193249073640 ) ) ;
#52207 = CARTESIAN_POINT ( 'NONE',  ( -94.38618793271719198, -60.00000000000733991, -14.22879310620676740 ) ) ;
#52208 = CARTESIAN_POINT ( 'NONE',  ( 7.896254658894416245, -68.78929182754202998, 1.307282859663299712 ) ) ;
#52209 = CARTESIAN_POINT ( 'NONE',  ( -35.57955382936916067, 363.3973965622570859, 2.919629247011395368 ) ) ;
#52210 = CARTESIAN_POINT ( 'NONE',  ( -6.372519863258895967, 41.41795155077670643, -58.45320710872936587 ) ) ;
#52211 = AXIS2_PLACEMENT_3D ( 'NONE', #3181, #26438, #18874 ) ;
#52212 = CARTESIAN_POINT ( 'NONE',  ( -88.92180072262880230, -30.00000000000001421, -15.18793788064705197 ) ) ;
#52213 = CARTESIAN_POINT ( 'NONE',  ( 66.26095113931063452, 6.856755485862130937E-15, 0.000000000000000000 ) ) ;
#52214 = CARTESIAN_POINT ( 'NONE',  ( -48.50349631401147121, -25.67985106503867598, 44.08718021024470346 ) ) ;
#52215 = ORIENTED_EDGE ( 'NONE', *, *, #52412, .F. ) ;
#52216 = DIRECTION ( 'NONE',  ( 0.000000000000000000, 0.000000000000000000, 1.000000000000000000 ) ) ;
#52217 = ORIENTED_EDGE ( 'NONE', *, *, #97157, .F. ) ;
#52218 = CARTESIAN_POINT ( 'NONE',  ( -95.55881383635450277, -45.25346914612557470, 194.1665852426087326 ) ) ;
#52219 = CARTESIAN_POINT ( 'NONE',  ( 25.11650669486618881, -3.999999999999998224, 0.000000000000000000 ) ) ;
#52220 = EDGE_CURVE ( 'NONE', #43916, #25504, #24681, .T. ) ;
#52221 = CARTESIAN_POINT ( 'NONE',  ( 6.458251213448832573, 3.357560920637069568, 6.499999999999997335 ) ) ;
#52222 = ORIENTED_EDGE ( 'NONE', *, *, #47085, .T. ) ;
#52223 = CARTESIAN_POINT ( 'NONE',  ( 5.649205854336966759, 246.5464546718848169, -2.034449005107570763 ) ) ;
#52224 = CARTESIAN_POINT ( 'NONE',  ( 51.86593418231710473, -38.33572705716591145, 73.09143234397147637 ) ) ;
#52225 = CARTESIAN_POINT ( 'NONE',  ( 8.472476921446266750E-16, 8.716839668575683930, -7.700121441565846325 ) ) ;
#52226 = CARTESIAN_POINT ( 'NONE',  ( 3.564365538398770017, -48.86493411501010087, 104.5953911288812463 ) ) ;
#52227 = VECTOR ( 'NONE', #54246, 1000.000000000000227 ) ;
#52228 = CARTESIAN_POINT ( 'NONE',  ( 7.109733078360420677, 41.69026692163959069, -59.69141567447950081 ) ) ;
#52229 = CARTESIAN_POINT ( 'NONE',  ( 38.36535705883633085, 18.64316884711714550, -5.022013495247578341 ) ) ;
#52230 = CARTESIAN_POINT ( 'NONE',  ( 88.16265431536430697, -29.99999999999999289, 187.1745416955410235 ) ) ;
#52231 = AXIS2_PLACEMENT_3D ( 'NONE', #16617, #10118, #52697 ) ;
#52232 = LINE ( 'NONE', #36107, #45888 ) ;
#52233 = CARTESIAN_POINT ( 'NONE',  ( -0.6447519515824183811, 37.14707136400079435, 27.41619501522666269 ) ) ;
#52234 =( GEOMETRIC_REPRESENTATION_CONTEXT ( 3 ) GLOBAL_UNCERTAINTY_ASSIGNED_CONTEXT ( ( #47001 ) ) GLOBAL_UNIT_ASSIGNED_CONTEXT ( ( #63844, #16332, #23939 ) ) REPRESENTATION_CONTEXT ( 'NONE', 'WORKASPACE' ) );
#52235 = COLOUR_RGB ( '', 0.72549020, 0.75294118, 0.79215686) ;
#52236 = ORIENTED_EDGE ( 'NONE', *, *, #51090, .T. ) ;
#52237 = ORIENTED_EDGE ( 'NONE', *, *, #18279, .F. ) ;
#52238 = CARTESIAN_POINT ( 'NONE',  ( 55.57801962097006765, -32.55754387728045174, 58.72004439221983318 ) ) ;
#52239 = CIRCLE ( 'NONE', #55685, 3.309500000000001663 ) ;
#52240 = CARTESIAN_POINT ( 'NONE',  ( 5.921004257435177998, 41.52415860376049750, -58.52392854124622801 ) ) ;
#52241 = DIRECTION ( 'NONE',  ( 0.000000000000000000, 1.000000000000000000, 0.000000000000000000 ) ) ;
#52242 = ORIENTED_EDGE ( 'NONE', *, *, #76568, .T. ) ;
#52243 = CARTESIAN_POINT ( 'NONE',  ( -85.30392625238515336, -38.35961253370006574, -22.56936445887191311 ) ) ;
#52244 = ORIENTED_EDGE ( 'NONE', *, *, #79892, .T. ) ;
#52245 = DIRECTION ( 'NONE',  ( 0.000000000000000000, 0.000000000000000000, 1.000000000000000000 ) ) ;
#52246 = CARTESIAN_POINT ( 'NONE',  ( 110.3209537404446223, -38.35602685585281080, 183.8300678904132610 ) ) ;
#52247 = CARTESIAN_POINT ( 'NONE',  ( 11.97038518901905668, 19.60005033863593837, 7.528208079863113689 ) ) ;
#52248 = CARTESIAN_POINT ( 'NONE',  ( 84.06531897659476726, -45.28288193063320222, 23.57404419494545067 ) ) ;
#52249 = CARTESIAN_POINT ( 'NONE',  ( -0.7867783998819701807, 45.39444483141824094, -18.48491233039627701 ) ) ;
#52250 = DIRECTION ( 'NONE',  ( 0.000000000000000000, 0.000000000000000000, 1.000000000000000000 ) ) ;
#52251 = CARTESIAN_POINT ( 'NONE',  ( 5.136066607408869444, -12.96798121126263936, -7.569033233149855100 ) ) ;
#52252 = DIRECTION ( 'NONE',  ( 1.000000000000000000, 1.224606353822377258E-16, 0.000000000000000000 ) ) ;
#52253 = CARTESIAN_POINT ( 'NONE',  ( -44.28914958155538528, 435.2230000814720938, 14.00302124382356261 ) ) ;
#52254 = CARTESIAN_POINT ( 'NONE',  ( 8.020865862490420994, 47.74483808550569819, 5.000000000002456702 ) ) ;
#52255 = ORIENTED_EDGE ( 'NONE', *, *, #66503, .F. ) ;
#52256 = DIRECTION ( 'NONE',  ( 0.000000000000000000, -1.000000000000000000, 0.000000000000000000 ) ) ;
#52257 = CARTESIAN_POINT ( 'NONE',  ( 7.036764706176849238, 40.29466777802799271, -71.06385277369803077 ) ) ;
#52258 = DIRECTION ( 'NONE',  ( 0.2282686145788442589, 0.2753452451894767283, 0.9338513990725731961 ) ) ;
#52259 = EDGE_LOOP ( 'NONE', ( #8165, #71817, #37103, #27733, #104591 ) ) ;
#52260 = CARTESIAN_POINT ( 'NONE',  ( 0.3167204509598351980, 5.377136764700157556, 6.686525924292787693 ) ) ;
#52261 = CARTESIAN_POINT ( 'NONE',  ( -35.69538431007205759, 304.3564473186642658, 4.136361301185305095 ) ) ;
#52262 = DIRECTION ( 'NONE',  ( 0.000000000000000000, 1.000000000000000000, 0.000000000000000000 ) ) ;
#52263 = CARTESIAN_POINT ( 'NONE',  ( 0.000000000000000000, 0.000000000000000000, 0.000000000000000000 ) ) ;
#52264 = CARTESIAN_POINT ( 'NONE',  ( -8.000000000000001776, -22.15624999999999289, 3.313708498984758943 ) ) ;
#52265 = CARTESIAN_POINT ( 'NONE',  ( -4.285641891732125508, -12.76267229504570011, 32.13335911023925462 ) ) ;
#52266 = CARTESIAN_POINT ( 'NONE',  ( 52.27951051746358502, 47.99999999999999289, 38.96734372144647551 ) ) ;
#52267 = CIRCLE ( 'NONE', #81502, 5.000000000000011546 ) ;
#52268 = EDGE_LOOP ( 'NONE', ( #52492, #77889, #40522, #88344 ) ) ;
#52269 = CARTESIAN_POINT ( 'NONE',  ( 83.31253321705135306, -53.70450120492168367, 187.1177796283798216 ) ) ;
#52270 = DIRECTION ( 'NONE',  ( -1.000000000000000000, -1.224606353822377258E-16, -0.000000000000000000 ) ) ;
#52271 = DIRECTION ( 'NONE',  ( 0.000000000000000000, 0.000000000000000000, -1.000000000000000000 ) ) ;
#52272 = ORIENTED_EDGE ( 'NONE', *, *, #10240, .T. ) ;
#52273 = CIRCLE ( 'NONE', #95402, 6.999999999999982236 ) ;
#52274 = CARTESIAN_POINT ( 'NONE',  ( -89.89320630590951566, -37.82073183721878706, 78.06522437777182688 ) ) ;
#52275 = DIRECTION ( 'NONE',  ( -3.552713678800500535E-15, 0.000000000000000000, 1.000000000000000000 ) ) ;
#52276 = FACE_OUTER_BOUND ( 'NONE', #16873, .T. ) ;
#52277 = CARTESIAN_POINT ( 'NONE',  ( 32.22120753352783140, 464.6691781026584636, 10.60621122532586291 ) ) ;
#52278 = EDGE_CURVE ( 'NONE', #63779, #101426, #43969, .T. ) ;
#52279 = CARTESIAN_POINT ( 'NONE',  ( -37.04799130315296196, -32.00998463668386051, -37.71207847285617731 ) ) ;
#52280 = AXIS2_PLACEMENT_3D ( 'NONE', #50992, #99008, #90956 ) ;
#52281 = EDGE_CURVE ( 'NONE', #95018, #49969, #2229, .T. ) ;
#52282 = SHAPE_REPRESENTATION_RELATIONSHIP ( 'NONE' , 'NONE' ,  #103287, #1016 ) ;
#52283 = CARTESIAN_POINT ( 'NONE',  ( 39.48197415042214686, -60.00000000000000000, 51.38249238638569238 ) ) ;
#52284 =( GEOMETRIC_REPRESENTATION_CONTEXT ( 3 ) GLOBAL_UNCERTAINTY_ASSIGNED_CONTEXT ( ( #51436 ) ) GLOBAL_UNIT_ASSIGNED_CONTEXT ( ( #19688, #39554, #72430 ) ) REPRESENTATION_CONTEXT ( 'NONE', 'WORKASPACE' ) );
#52285 = CARTESIAN_POINT ( 'NONE',  ( 29.22136840097360633, -31.92850515648737542, 40.14001151005216173 ) ) ;
#52286 = SURFACE_SIDE_STYLE ('',( #4813 ) ) ;
#52287 = CARTESIAN_POINT ( 'NONE',  ( 10.69334538532959122, -13.94028717871298539, 31.85850709728139307 ) ) ;
#52289 = CARTESIAN_POINT ( 'NONE',  ( -12.05941008653503843, 19.79566280298742242, 7.352333506836349564 ) ) ;
#52288 = CARTESIAN_POINT ( 'NONE',  ( 34.47678062874019389, 437.1474145881098821, 5.468662283308706407 ) ) ;
#52290 = CARTESIAN_POINT ( 'NONE',  ( 0.2504595177176738297, 295.3551702420456309, -10.00003484568028611 ) ) ;
#52291 = CARTESIAN_POINT ( 'NONE',  ( 7.188101187500000044, -10.15625000204838457, 0.000000000000000000 ) ) ;
#52292 = CARTESIAN_POINT ( 'NONE',  ( 43.61018511057424973, 374.8234295527117865, 14.44054883524410826 ) ) ;
#52293 = ADVANCED_FACE ( 'NONE', ( #34847 ), #11730, .F. ) ;
#52294 = FACE_OUTER_BOUND ( 'NONE', #85684, .T. ) ;
#52295 = VERTEX_POINT ( 'NONE', #94112 ) ;
#52296 = DIRECTION ( 'NONE',  ( 0.8191520442889884679, 0.000000000000000000, 0.5735764363510509334 ) ) ;
#52297 = CARTESIAN_POINT ( 'NONE',  ( -17.49999999999997513, 51.99999999999955946, 59.64162155654619824 ) ) ;
#52298 = MECHANICAL_DESIGN_GEOMETRIC_PRESENTATION_REPRESENTATION (  '', ( #47140 ), #608 ) ;
#52299 = ORIENTED_EDGE ( 'NONE', *, *, #89325, .F. ) ;
#52300 = SURFACE_SIDE_STYLE ('',( #44227 ) ) ;
#52301 = CARTESIAN_POINT ( 'NONE',  ( 5.980543423763064581, -61.02903592498922336, -0.5500789318242889081 ) ) ;
#52302 = CONICAL_SURFACE ( 'NONE', #2334, 3.309500000000007880, 0.9599310885968770357 ) ;
#52304 = CARTESIAN_POINT ( 'NONE',  ( -16.18453578148346139, -60.22808678499453805, -36.38447698959835463 ) ) ;
#52303 =( LENGTH_UNIT ( ) NAMED_UNIT ( * ) SI_UNIT ( .MILLI., .METRE. ) );
#52305 = COLOUR_RGB ( '', 0.66274510, 0.83137255, 0.94901961) ;
#52306 = ORIENTED_EDGE ( 'NONE', *, *, #52882, .F. ) ;
#52307 = CARTESIAN_POINT ( 'NONE',  ( 10.00232142752224362, 294.6427048180378847, 0.2484324481109706217 ) ) ;
#52308 = LINE ( 'NONE', #85217, #53168 ) ;
#52309 = CIRCLE ( 'NONE', #74705, 15.00000000000000000 ) ;
#52310 = ORIENTED_EDGE ( 'NONE', *, *, #72954, .T. ) ;
#52311 = DIRECTION ( 'NONE',  ( 0.000000000000000000, -1.000000000000000000, 0.000000000000000000 ) ) ;
#52312 = EDGE_CURVE ( 'NONE', #76220, #56216, #81447, .T. ) ;
#52313 = CARTESIAN_POINT ( 'NONE',  ( 30.63612296757489517, 10.92940684821786590, -40.03790167141658429 ) ) ;
#52314 = CARTESIAN_POINT ( 'NONE',  ( -91.86321863162261536, -59.99999999999999289, 13.12527847739685249 ) ) ;
#52315 = SURFACE_SIDE_STYLE ('',( #68526 ) ) ;
#52316 = CARTESIAN_POINT ( 'NONE',  ( 30.00000000000000000, 488.6481008951278113, 3.890293910850189274 ) ) ;
#52317 = FILL_AREA_STYLE ('',( #78194 ) ) ;
#52318 = CARTESIAN_POINT ( 'NONE',  ( -34.62900545891979220, 434.6649403350424450, 8.921687928929188161 ) ) ;
#52319 = CARTESIAN_POINT ( 'NONE',  ( -81.30862360253455279, -49.93417848018496130, 170.6586799718517398 ) ) ;
#52320 = EDGE_LOOP ( 'NONE', ( #96472, #23097, #90782, #75396, #93224 ) ) ;
#52321 = CARTESIAN_POINT ( 'NONE',  ( -44.19062745116208646, 435.2577039776292054, 14.58891375936595836 ) ) ;
#52322 = ORIENTED_EDGE ( 'NONE', *, *, #103994, .F. ) ;
#52323 = ORIENTED_EDGE ( 'NONE', *, *, #49364, .F. ) ;
#52324 = CARTESIAN_POINT ( 'NONE',  ( 10.28624191511809371, -1.200000000000000030E-05, -15.40779740156171762 ) ) ;
#52325 = CARTESIAN_POINT ( 'NONE',  ( -14.99896353599397258, -5.000000000000000888, 9.191463535712019350 ) ) ;
#52326 = EDGE_CURVE ( 'NONE', #78717, #28015, #84941, .T. ) ;
#52327 = SURFACE_SIDE_STYLE ('',( #19490 ) ) ;
#52328 = CARTESIAN_POINT ( 'NONE',  ( 19.00000000000001066, -4.000000000000000000, -1.500000000000001332 ) ) ;
#52329 = ORIENTED_EDGE ( 'NONE', *, *, #89247, .F. ) ;
#52330 = AXIS2_PLACEMENT_3D ( 'NONE', #2329, #67087, #74623 ) ;
#52331 = LINE ( 'NONE', #94950, #99515 ) ;
#52332 = CARTESIAN_POINT ( 'NONE',  ( -94.67953089133513345, -57.66492561105124537, -4.550087184288205577 ) ) ;
#52333 = CARTESIAN_POINT ( 'NONE',  ( 2.500000000000000444, -30.00000000000000000, 28.88619651857252535 ) ) ;
#52334 = CARTESIAN_POINT ( 'NONE',  ( 2.761899744546835519E-15, 36.79151656018385097, -22.55262289886175964 ) ) ;
#52335 = CARTESIAN_POINT ( 'NONE',  ( 91.09088295274877112, -5.000000000000000888, 6.123233995736779101E-16 ) ) ;
#52336 = CARTESIAN_POINT ( 'NONE',  ( -13.64654340589911818, -51.35783868776468353, 30.13167154758286159 ) ) ;
#52337 = CARTESIAN_POINT ( 'NONE',  ( 0.000000000000000000, 0.000000000000000000, -0.4455245229258316120 ) ) ;
#52338 = CARTESIAN_POINT ( 'NONE',  ( 95.99465422657044655, -14.21045842199428222, 88.91344185009528189 ) ) ;
#52339 = CARTESIAN_POINT ( 'NONE',  ( -78.25705875637353870, -14.21045842199447939, 182.3370610225134953 ) ) ;
#52340 = CARTESIAN_POINT ( 'NONE',  ( -59.32705706084635722, -18.65613686416636696, 61.11537755004999894 ) ) ;
#52341 = ORIENTED_EDGE ( 'NONE', *, *, #30862, .F. ) ;
#52342 = CARTESIAN_POINT ( 'NONE',  ( 0.000000000000000000, 23.58303312036771615, -45.10524579772351217 ) ) ;
#52343 = VERTEX_POINT ( 'NONE', #53129 ) ;
#52344 = CARTESIAN_POINT ( 'NONE',  ( -103.4860089683291022, -52.71038146289320991, 188.6634783447426003 ) ) ;
#52345 = FACE_OUTER_BOUND ( 'NONE', #11223, .T. ) ;
#52346 = STYLED_ITEM ( 'NONE', ( #62408 ), #54736 ) ;
#52347 = CARTESIAN_POINT ( 'NONE',  ( 23.73746414932995208, -5.000000000000000888, 6.123233995736769241E-16 ) ) ;
#52348 = EDGE_CURVE ( 'NONE', #36374, #79214, #68247, .T. ) ;
#52349 = ORIENTED_EDGE ( 'NONE', *, *, #94786, .F. ) ;
#52350 = CARTESIAN_POINT ( 'NONE',  ( 19.49911599185411148, 49.99996344174991236, 59.94524073513129991 ) ) ;
#52351 = FILL_AREA_STYLE_COLOUR ( '', #106326 ) ;
#52352 = CARTESIAN_POINT ( 'NONE',  ( -3.355892750373842048, -0.9951980364987413896, 104.3125661743353589 ) ) ;
#52353 = CARTESIAN_POINT ( 'NONE',  ( 7.188101187500001821, -13.43750000204838457, -2.977408999572650483 ) ) ;
#52354 = CARTESIAN_POINT ( 'NONE',  ( 17.33349330513380693, -3.851859888774471706E-31, 4.000000000000001776 ) ) ;
#52355 = DIRECTION ( 'NONE',  ( 0.000000000000000000, -1.000000000000000000, 0.000000000000000000 ) ) ;
#52356 =( LENGTH_UNIT ( ) NAMED_UNIT ( * ) SI_UNIT ( .MILLI., .METRE. ) );
#52357 = CARTESIAN_POINT ( 'NONE',  ( -30.12932728364529922, 334.4140447340107585, 17.11298374841474867 ) ) ;
#52358 = CARTESIAN_POINT ( 'NONE',  ( 23.61963550967466574, 306.0340374937824777, 10.19690224617928287 ) ) ;
#52359 = EDGE_CURVE ( 'NONE', #100497, #24510, #93588, .T. ) ;
#52360 = FACE_OUTER_BOUND ( 'NONE', #82226, .T. ) ;
#52361 = CARTESIAN_POINT ( 'NONE',  ( 73.33904886068935980, -4.000000000000000000, 4.898587196589421703E-16 ) ) ;
#52362 = FILL_AREA_STYLE ('',( #36766 ) ) ;
#52363 = CARTESIAN_POINT ( 'NONE',  ( -31.54433348721467922, -49.90828886377769891, 35.58986079060855445 ) ) ;
#52364 = CARTESIAN_POINT ( 'NONE',  ( 4.000000000000000000, 17.85270131633358304, 5.744562646538042827 ) ) ;
#52365 = UNCERTAINTY_MEASURE_WITH_UNIT (LENGTH_MEASURE( 1.000000000000000082E-05 ), #87594, 'distance_accuracy_value', 'NONE');
#52366 = CARTESIAN_POINT ( 'NONE',  ( 44.62879333611520849, -32.61662185523480417, 41.38689675569595749 ) ) ;
#52367 = CARTESIAN_POINT ( 'NONE',  ( -32.62920465536350889, 486.5749440413351294, 6.880070463950354487 ) ) ;
#52368 = CARTESIAN_POINT ( 'NONE',  ( -7.211357414135268762, 87.01146539934444490, 3.467230644691327690 ) ) ;
#52369 = CARTESIAN_POINT ( 'NONE',  ( -87.30475775079190726, -38.58328791312629846, 199.6746598993676116 ) ) ;
#52370 = ORIENTED_EDGE ( 'NONE', *, *, #88622, .T. ) ;
#52372 = FACE_OUTER_BOUND ( 'NONE', #18734, .T. ) ;
#52371 = DIRECTION ( 'NONE',  ( -0.5735764363510497121, 0.8191520442889892450, 1.003171929053521665E-16 ) ) ;
#52373 = CARTESIAN_POINT ( 'NONE',  ( 12.98019590313349347, 8.542529574688673577, -8.955537626817529073 ) ) ;
#52374 = CARTESIAN_POINT ( 'NONE',  ( -19.20197792873035425, 49.77790350908116324, 61.55673312277118470 ) ) ;
#52375 = CARTESIAN_POINT ( 'NONE',  ( -7.484880931609037447, 40.61737797493887570, -59.44023054564222264 ) ) ;
#52376 = CARTESIAN_POINT ( 'NONE',  ( 6.686881269052097565, 40.00000000387462507, -71.19596970773797295 ) ) ;
#52377 = DIRECTION ( 'NONE',  ( 0.000000000000000000, 0.000000000000000000, 1.000000000000000000 ) ) ;
#52378 = CARTESIAN_POINT ( 'NONE',  ( -24.48540210594370947, 306.7517469399879246, 9.362912201731168338 ) ) ;
#52379 = CARTESIAN_POINT ( 'NONE',  ( 7.500000000000000000, 4.330127018922189208, -7.422398894150033399 ) ) ;
#52380 = CARTESIAN_POINT ( 'NONE',  ( 109.0644082823126695, -60.00000000000001421, 193.5531632337274175 ) ) ;
#52381 = AXIS2_PLACEMENT_3D ( 'NONE', #105610, #89447, #31236 ) ;
#52382 =( BOUNDED_CURVE ( )  B_SPLINE_CURVE ( 2, ( #27439, #100739, #94262, #26901, #11184, #101808, #12262, #67852, #84036 ),
 .UNSPECIFIED., .F., .F. ) 
 B_SPLINE_CURVE_WITH_KNOTS ( ( 3, 2, 2, 2, 3 ),
 ( 0.3676470588235293824, 0.3749999999999999445, 0.3823529411764705621, 0.3897058823529411797, 0.3970588235294117418 ),
 .UNSPECIFIED. ) 
 CURVE ( )  GEOMETRIC_REPRESENTATION_ITEM ( )  RATIONAL_B_SPLINE_CURVE ( ( 1.000000000000000666, 0.9238795325112861834, 1.000000000000000000, 0.9238795325112867385, 1.000000000000000000, 0.9238795325112867385, 1.000000000000000000, 0.9238795325112867385, 1.000000000000000000 ) ) 
 REPRESENTATION_ITEM ( '' )  );
#52383 = AXIS2_PLACEMENT_3D ( 'NONE', #38241, #4252, #94872 ) ;
#52384 = DIRECTION ( 'NONE',  ( -1.000000000000000000, -1.224606353822377258E-16, -0.000000000000000000 ) ) ;
#52385 = ORIENTED_EDGE ( 'NONE', *, *, #21437, .T. ) ;
#52386 = CARTESIAN_POINT ( 'NONE',  ( 9.999999999999996447, 15.00000000000000000, -10.00000000000000000 ) ) ;
#52387 = STYLED_ITEM ( 'NONE', ( #95521 ), #16251 ) ;
#52388 = CARTESIAN_POINT ( 'NONE',  ( -80.72051579742614535, -30.00000000000003197, 13.90560478027946445 ) ) ;
#52389 = VERTEX_POINT ( 'NONE', #1893 ) ;
#52391 = CARTESIAN_POINT ( 'NONE',  ( -9.113097280746998763, -53.73699350858575485, 31.11721482942554928 ) ) ;
#52390 = CARTESIAN_POINT ( 'NONE',  ( -73.58054804561130879, -38.32516351570817648, 156.7495410978815755 ) ) ;
#52392 = CARTESIAN_POINT ( 'NONE',  ( 4.852941176470592310, -3.000000000000002665, -70.80672828634229177 ) ) ;
#52393 = DIRECTION ( 'NONE',  ( 0.000000000000000000, 1.000000000000000000, 0.000000000000000000 ) ) ;
#52394 = CARTESIAN_POINT ( 'NONE',  ( 5.082755093536324154, -13.71875000204838457, 5.082755093536326818 ) ) ;
#52395 = CARTESIAN_POINT ( 'NONE',  ( 11.68767211932355998, -5.000000000000002665, -81.85902538600510070 ) ) ;
#52396 = CARTESIAN_POINT ( 'NONE',  ( 0.000000000000000000, 15.00000000000000000, 0.000000000000000000 ) ) ;
#52397 = EDGE_LOOP ( 'NONE', ( #31052, #32742, #75084, #44434, #26265, #46294 ) ) ;
#52398 = CARTESIAN_POINT ( 'NONE',  ( 84.99175437857353188, -18.63712082014315286, 155.3294098635141438 ) ) ;
#52399 = CARTESIAN_POINT ( 'NONE',  ( -4.334722950434925615, -1.119290245239405790, 104.3859289939576627 ) ) ;
#52400 = CARTESIAN_POINT ( 'NONE',  ( 1.734723475976807094E-15, 8.660254037844390851, 0.000000000000000000 ) ) ;
#52401 = ORIENTED_EDGE ( 'NONE', *, *, #22741, .F. ) ;
#52402 = CARTESIAN_POINT ( 'NONE',  ( 43.03265099500004709, 484.2747968070555089, -0.8099405866658345721 ) ) ;
#52403 = CARTESIAN_POINT ( 'NONE',  ( -47.77442396816168468, 17.34920168383065686, 14.37330342454805177 ) ) ;
#52404 = DIRECTION ( 'NONE',  ( 0.000000000000000000, 0.000000000000000000, 1.000000000000000000 ) ) ;
#52405 = CARTESIAN_POINT ( 'NONE',  ( -5.981118819178464108, 253.9718345618005060, 0.5452870891823475841 ) ) ;
#52406 = CARTESIAN_POINT ( 'NONE',  ( 0.5305815910617995845, 18.60106106186565356, 49.36172356568721398 ) ) ;
#52407 = PRESENTATION_STYLE_ASSIGNMENT (( #36289 ) ) ;
#52408 = ADVANCED_FACE ( 'NONE', ( #101676 ), #92377, .T. ) ;
#52409 = ORIENTED_EDGE ( 'NONE', *, *, #24278, .F. ) ;
#52410 =( NAMED_UNIT ( * ) PLANE_ANGLE_UNIT ( ) SI_UNIT ( $, .RADIAN. ) );
#52411 = CARTESIAN_POINT ( 'NONE',  ( -80.61739365636806554, -30.00000000000000355, -12.80982504787266940 ) ) ;
#52412 = EDGE_CURVE ( 'NONE', #95973, #20227, #84926, .T. ) ;
#52413 = CARTESIAN_POINT ( 'NONE',  ( 38.20903166376764659, 18.64284798592685632, 4.122114450692562215 ) ) ;
#52414 = CARTESIAN_POINT ( 'NONE',  ( 87.42597901065016686, -31.67953177600239201, 188.4201908730174750 ) ) ;
#52416 = CARTESIAN_POINT ( 'NONE',  ( -43.52075891743682234, 484.7805561108189636, 4.063293749114582631 ) ) ;
#52415 = CARTESIAN_POINT ( 'NONE',  ( 19.34999999999999787, 3.309500000000003439, 0.000000000000000000 ) ) ;
#52417 = AXIS2_PLACEMENT_3D ( 'NONE', #67670, #100550, #26713 ) ;
#52418 = CARTESIAN_POINT ( 'NONE',  ( -1.320432766682874540E-15, -28.53125000204838813, 7.188101187500000044 ) ) ;
#52419 = DIRECTION ( 'NONE',  ( -0.000000000000000000, -1.000000000000000000, -0.000000000000000000 ) ) ;
#52420 = CIRCLE ( 'NONE', #5911, 5.000000000000011546 ) ;
#52421 = COLOUR_RGB ( '', 0.40784314, 0.44705882, 0.49803922) ;
#52422 = CARTESIAN_POINT ( 'NONE',  ( 32.15310320217080431, 439.7024266304582056, 23.94087012106557211 ) ) ;
#52423 = STYLED_ITEM ( 'NONE', ( #54597 ), #85465 ) ;
#52424 = ITEM_DEFINED_TRANSFORMATION ( 'NONE', 'NONE', #35246,  #10728 ) ;
#52425 = VERTEX_POINT ( 'NONE', #18523 ) ;
#52426 = CARTESIAN_POINT ( 'NONE',  ( -35.55307928090937963, 490.6489906963894327, 12.31598007740004519 ) ) ;
#52427 = CARTESIAN_POINT ( 'NONE',  ( -5.897136329696558654, 4.642285597044319978, -5.000000000000000000 ) ) ;
#52428 = CARTESIAN_POINT ( 'NONE',  ( 9.184850993605161750E-16, 81.00000000000000000, 7.000000000000006217 ) ) ;
#52429 = ADVANCED_FACE ( 'NONE', ( #99939 ), #12548, .F. ) ;
#52430 = ORIENTED_EDGE ( 'NONE', *, *, #26199, .T. ) ;
#52431 = CARTESIAN_POINT ( 'NONE',  ( -7.312621643696487261, 52.12777849912266248, -2.970404147433324482 ) ) ;
#52432 = CARTESIAN_POINT ( 'NONE',  ( 12.13034742782427955, 48.00000000000000000, -93.82352941176471006 ) ) ;
#52433 = ORIENTED_EDGE ( 'NONE', *, *, #39557, .F. ) ;
#52434 = ADVANCED_FACE ( 'NONE', ( #43309 ), #92375, .F. ) ;
#52435 = CARTESIAN_POINT ( 'NONE',  ( -0.7804241024683111760, 8.373447173740549587, -51.48088908221409099 ) ) ;
#52436 = LINE ( 'NONE', #78312, #94156 ) ;
#52437 = PRESENTATION_STYLE_ASSIGNMENT (( #9315 ) ) ;
#52438 = CARTESIAN_POINT ( 'NONE',  ( -92.96881148959433006, -60.00000000000001421, 202.4687464090484355 ) ) ;
#52439 = CARTESIAN_POINT ( 'NONE',  ( 20.00100000000000477, 12.99999999999999289, 0.000000000000000000 ) ) ;
#52440 = CARTESIAN_POINT ( 'NONE',  ( -45.50145573691759182, 405.2496736015978627, 8.430338687477670234 ) ) ;
#52441 = FILL_AREA_STYLE ('',( #50839 ) ) ;
#52442 =( NAMED_UNIT ( * ) PLANE_ANGLE_UNIT ( ) SI_UNIT ( $, .RADIAN. ) );
#52443 = CARTESIAN_POINT ( 'NONE',  ( -84.92579027340632081, -39.36590996067631920, 183.3526443039159233 ) ) ;
#52444 = AXIS2_PLACEMENT_3D ( 'NONE', #69428, #78558, #4156 ) ;
#52445 = CARTESIAN_POINT ( 'NONE',  ( -4.272532768864641284, 54.28699348431178606, -6.535710695638695888 ) ) ;
#52446 = AXIS2_PLACEMENT_3D ( 'NONE', #61597, #103623, #86411 ) ;
#52447 = EDGE_LOOP ( 'NONE', ( #15177, #71909, #51115, #75058 ) ) ;
#52448 = CARTESIAN_POINT ( 'NONE',  ( -7.409678256911004901, 302.7200037710339871, 9.908966876114519096 ) ) ;
#52449 = EDGE_CURVE ( 'NONE', #39461, #28165, #83230, .T. ) ;
#52450 = EDGE_CURVE ( 'NONE', #15506, #38679, #25744, .T. ) ;
#52451 = CARTESIAN_POINT ( 'NONE',  ( 4.073826509764633563, -1.047876529905043874, 104.5376934966472220 ) ) ;
#52452 =( GEOMETRIC_REPRESENTATION_CONTEXT ( 3 ) GLOBAL_UNCERTAINTY_ASSIGNED_CONTEXT ( ( #49963 ) ) GLOBAL_UNIT_ASSIGNED_CONTEXT ( ( #69815, #61747, #37486 ) ) REPRESENTATION_CONTEXT ( 'NONE', 'WORKASPACE' ) );
#52453 = STYLED_ITEM ( 'NONE', ( #45263 ), #16793 ) ;
#52454 = CARTESIAN_POINT ( 'NONE',  ( -83.97025560380723164, -45.26987198569664628, 3.107597088425433807 ) ) ;
#52455 = LINE ( 'NONE', #27709, #37452 ) ;
#52456 = SURFACE_STYLE_FILL_AREA ( #78329 ) ;
#52457 = CARTESIAN_POINT ( 'NONE',  ( 7.869427812660441113, 87.30462500882723020, -5.000000000000000888 ) ) ;
#52458 = CARTESIAN_POINT ( 'NONE',  ( -6.063014363552454711, -12.44085613821211389, 12.46297707981385727 ) ) ;
#52459 = CARTESIAN_POINT ( 'NONE',  ( -57.69562748392037577, 41.99999999991776178, 15.50526908263360681 ) ) ;
#52460 = CARTESIAN_POINT ( 'NONE',  ( 61.00101809772601769, -14.21045842199439591, 86.19763211990357377 ) ) ;
#52461 = CARTESIAN_POINT ( 'NONE',  ( 0.000000000000000000, 57.18445727710329862, -19.59103268995865221 ) ) ;
#52462 = CARTESIAN_POINT ( 'NONE',  ( -84.89308075164642275, -60.00000000000002842, -27.59301604020478038 ) ) ;
#52463 = CARTESIAN_POINT ( 'NONE',  ( -69.23882386195900551, -29.06181850512027864, 93.49118526020582465 ) ) ;
#52464 = VERTEX_POINT ( 'NONE', #96640 ) ;
#52465 = CARTESIAN_POINT ( 'NONE',  ( 97.13532076618713518, -30.00000000000002842, 199.9107784265496264 ) ) ;
#52466 = CARTESIAN_POINT ( 'NONE',  ( -62.40055500521754794, 40.83861719869454987, 18.44141605947073970 ) ) ;
#52467 = CARTESIAN_POINT ( 'NONE',  ( 19.58684304517602470, -57.67119434593145400, -43.84739835614993808 ) ) ;
#52468 = ORIENTED_EDGE ( 'NONE', *, *, #65619, .F. ) ;
#52469 = CARTESIAN_POINT ( 'NONE',  ( 8.471708131381630480, -12.16652409483400810, 8.774944570614499284 ) ) ;
#52470 = CARTESIAN_POINT ( 'NONE',  ( -5.082755093536325042, -27.96875000204838457, -5.082755093536325930 ) ) ;
#52471 = CARTESIAN_POINT ( 'NONE',  ( -0.1682124922453071825, 27.29656849860387879, -40.75000000000001421 ) ) ;
#52472 = EDGE_LOOP ( 'NONE', ( #12392, #65115 ) ) ;
#52473 = CARTESIAN_POINT ( 'NONE',  ( -16.13647630347073658, 6.334953579828353831, -5.738861489052294651 ) ) ;
#52474 = ORIENTED_EDGE ( 'NONE', *, *, #18357, .T. ) ;
#52475 = FACE_OUTER_BOUND ( 'NONE', #71307, .T. ) ;
#52476 = B_SPLINE_CURVE_WITH_KNOTS ( 'NONE', 3,
 ( #51117, #28488, #68934, #11719 ),
 .UNSPECIFIED., .F., .F.,
 ( 4, 4 ),
 ( 8.673617379884035472E-18, 0.001861443540404362270 ),
 .UNSPECIFIED. ) ;
#52477 = CARTESIAN_POINT ( 'NONE',  ( 46.77788840983939878, 18.69141115048694957, -15.65052543522692652 ) ) ;
#52478 = CARTESIAN_POINT ( 'NONE',  ( -27.14100146121103307, -60.00000000000000711, 44.29861369568705953 ) ) ;
#52479 = CARTESIAN_POINT ( 'NONE',  ( -10.61825212277778796, 43.91732780493584443, 12.90779740156163768 ) ) ;
#52480 = CARTESIAN_POINT ( 'NONE',  ( 7.188101187499999156, -30.12500000204838813, 2.977408999572654924 ) ) ;
#52481 = CARTESIAN_POINT ( 'NONE',  ( -49.13304414347859250, 12.95525746345744622, 16.19504546972465064 ) ) ;
#52482 = CARTESIAN_POINT ( 'NONE',  ( 57.70539558375507738, -4.000000000000000000, 0.000000000000000000 ) ) ;
#52483 = CARTESIAN_POINT ( 'NONE',  ( 6.043427762771891310, 50.00000000000000000, -95.48543666094653304 ) ) ;
#52484 = EDGE_CURVE ( 'NONE', #87039, #95821, #100409, .T. ) ;
#52485 = DIRECTION ( 'NONE',  ( -1.000000000000000000, -0.000000000000000000, -0.000000000000000000 ) ) ;
#52486 = CARTESIAN_POINT ( 'NONE',  ( 41.61741820144892756, 435.6127172585838707, 7.033059668060364089 ) ) ;
#52487 = VECTOR ( 'NONE', #13893, 1000.000000000000000 ) ;
#52488 = ORIENTED_EDGE ( 'NONE', *, *, #18904, .T. ) ;
#52489 = CARTESIAN_POINT ( 'NONE',  ( 4.999999999999993783, -4.000000000000003553, 102.2532056551910387 ) ) ;
#52491 = CARTESIAN_POINT ( 'NONE',  ( 32.55783135264621109, -39.49123201241251024, 34.14412841509428631 ) ) ;
#52490 = CARTESIAN_POINT ( 'NONE',  ( 5.290067270632160756, 52.08006895350504806, -6.031152949374595451 ) ) ;
#52492 = ORIENTED_EDGE ( 'NONE', *, *, #33895, .F. ) ;
#52493 = EDGE_CURVE ( 'NONE', #54493, #54950, #78019, .T. ) ;
#52494 = CARTESIAN_POINT ( 'NONE',  ( -23.05170650452966186, 25.28969635687047202, -33.19779254177406358 ) ) ;
#52495 = AXIS2_PLACEMENT_3D ( 'NONE', #43307, #58969, #68104 ) ;
#52497 = CARTESIAN_POINT ( 'NONE',  ( -35.59667163540026280, 463.9592197885497171, -0.04846191499040426731 ) ) ;
#52496 = CARTESIAN_POINT ( 'NONE',  ( -26.55974056404284767, 34.93710072687599677, -7.679312300194466978 ) ) ;
#52498 = DIRECTION ( 'NONE',  ( -1.000000000000000000, -1.224606353822377258E-16, -0.000000000000000000 ) ) ;
#52499 = CARTESIAN_POINT ( 'NONE',  ( -21.29975379448952211, 294.8969325209483259, -1.990407376643348103 ) ) ;
#52500 = CIRCLE ( 'NONE', #66280, 7.500000000000000000 ) ;
#52501 = AXIS2_PLACEMENT_3D ( 'NONE', #7339, #81221, #50451 ) ;
#52502 = CARTESIAN_POINT ( 'NONE',  ( -7.500000000000007105, -3.000000000000000000, -68.91429205785459544 ) ) ;
#52503 = AXIS2_PLACEMENT_3D ( 'NONE', #5145, #11620, #36491 ) ;
#52504 = CARTESIAN_POINT ( 'NONE',  ( 32.07495350393109135, 464.7631673202251932, 11.47102835346950656 ) ) ;
#52505 = CARTESIAN_POINT ( 'NONE',  ( -35.04496600798486128, 464.5002996787812322, 18.88267410155424031 ) ) ;
#52506 = ORIENTED_EDGE ( 'NONE', *, *, #25561, .T. ) ;
#52507 = CARTESIAN_POINT ( 'NONE',  ( 91.96543020101078980, -60.00000000000000000, 17.51050721529170318 ) ) ;
#52508 = SURFACE_STYLE_USAGE ( .BOTH. , #2361 ) ;
#52510 = ADVANCED_FACE ( 'NONE', ( #4980 ), #72870, .F. ) ;
#52509 = CARTESIAN_POINT ( 'NONE',  ( 33.38752816062147133, 464.7252609254567801, 16.46839106254713414 ) ) ;
#52511 = DIRECTION ( 'NONE',  ( -0.7071067811865530128, 8.659560562354868763E-17, -0.7071067811865421326 ) ) ;
#52512 = VECTOR ( 'NONE', #84377, 1000.000000000000227 ) ;
#52513 = CARTESIAN_POINT ( 'NONE',  ( -5.556063244994718708, 40.28998690596864662, -71.04001413054817249 ) ) ;
#52514 = CARTESIAN_POINT ( 'NONE',  ( -46.77759138928167459, 18.69812886098191385, -15.64253076101933537 ) ) ;
#52515 = ORIENTED_EDGE ( 'NONE', *, *, #74940, .F. ) ;
#52516 = CARTESIAN_POINT ( 'NONE',  ( -108.3254638997414077, -29.99999999997997335, 187.2860949193978684 ) ) ;
#52517 = ORIENTED_EDGE ( 'NONE', *, *, #53627, .T. ) ;
#52518 = CARTESIAN_POINT ( 'NONE',  ( 0.000000000000000000, 0.000000000000000000, 0.000000000000000000 ) ) ;
#52519 = CARTESIAN_POINT ( 'NONE',  ( 7.592810154713590230E-15, 0.000000000000000000, -62.00000000000000000 ) ) ;
#52520 = CARTESIAN_POINT ( 'NONE',  ( 0.000000000000000000, -30.00000000000000000, 0.000000000000000000 ) ) ;
#52521 = CARTESIAN_POINT ( 'NONE',  ( 16.10528882106936521, 21.79591095384835242, 1.082486061783650255 ) ) ;
#52522 = CARTESIAN_POINT ( 'NONE',  ( 85.99566667790004715, -60.22088695362039346, -14.08581190481345402 ) ) ;
#52523 = CARTESIAN_POINT ( 'NONE',  ( -38.37349848668355179, 306.2639072012707402, -7.354698554755767503 ) ) ;
#52524 = DIRECTION ( 'NONE',  ( -0.7142857142857168551, 0.6998542122237625396, 0.000000000000000000 ) ) ;
#52525 = CARTESIAN_POINT ( 'NONE',  ( -17.53184552654991180, 45.00000000000001421, 63.43879945933183961 ) ) ;
#52526 = ORIENTED_EDGE ( 'NONE', *, *, #46194, .F. ) ;
#52527 = EDGE_LOOP ( 'NONE', ( #100240, #99865, #30354, #65247, #17072, #78868 ) ) ;
#52528 = CARTESIAN_POINT ( 'NONE',  ( 17.50000000000004974, 48.00000000000341771, 64.09949417230997426 ) ) ;
#52529 = SURFACE_STYLE_FILL_AREA ( #61179 ) ;
#52531 = VERTEX_POINT ( 'NONE', #88550 ) ;
#52530 = CARTESIAN_POINT ( 'NONE',  ( 6.528903126310523497, 51.53956178974399904, 6.914479967639524993 ) ) ;
#52532 = CARTESIAN_POINT ( 'NONE',  ( 73.98053784616911344, -29.06950772015738238, 109.2017082355514503 ) ) ;
#52533 = EDGE_LOOP ( 'NONE', ( #82004, #102124 ) ) ;
#52534 = CARTESIAN_POINT ( 'NONE',  ( 3.333770628267000546, -49.25119931019934683, 44.08595898032793059 ) ) ;
#52535 = CARTESIAN_POINT ( 'NONE',  ( -5.082755093536325042, -18.59375000204838457, -5.082755093536325930 ) ) ;
#52536 = AXIS2_PLACEMENT_3D ( 'NONE', #29645, #85743, #29134 ) ;
#52537 = CARTESIAN_POINT ( 'NONE',  ( -112.2456557016906942, -57.67113047748567567, 190.5314477545807392 ) ) ;
#52538 = ADVANCED_FACE ( 'NONE', ( #89612 ), #4194, .T. ) ;
#52539 = VERTEX_POINT ( 'NONE', #24372 ) ;
#52540 = FILL_AREA_STYLE ('',( #13134 ) ) ;
#52541 = CARTESIAN_POINT ( 'NONE',  ( -16.52732684424165654, 43.98685724163156863, -87.77868211029610279 ) ) ;
#52542 = CARTESIAN_POINT ( 'NONE',  ( 102.7781224394537816, -37.84834821706366625, 170.2548301641596140 ) ) ;
#52543 = EDGE_CURVE ( 'NONE', #89905, #93842, #10207, .T. ) ;
#52544 = CARTESIAN_POINT ( 'NONE',  ( -37.40764580657506855, 27.65900449730653321, -13.45617127781033595 ) ) ;
#52545 = CARTESIAN_POINT ( 'NONE',  ( 32.61650669486618881, 1.474610560812782335E-15, 0.000000000000000000 ) ) ;
#52546 = CARTESIAN_POINT ( 'NONE',  ( -5.656854249492381470, -20.75000000409676915, 5.656854249492379694 ) ) ;
#52547 = CARTESIAN_POINT ( 'NONE',  ( -45.23652315699401072, -28.37715625667643948, 40.32569774422481856 ) ) ;
#52548 = CARTESIAN_POINT ( 'NONE',  ( -37.40563201180869868, 25.53133898278100133, 13.45617127781066102 ) ) ;
#52549 = ADVANCED_FACE ( 'NONE', ( #51790 ), #59381, .F. ) ;
#52550 = FACE_OUTER_BOUND ( 'NONE', #4484, .T. ) ;
#52551 = CARTESIAN_POINT ( 'NONE',  ( 0.000000000000000000, 0.000000000000000000, -8.028130060628445364 ) ) ;
#52552 = CONICAL_SURFACE ( 'NONE', #54460, 3.309499999999999886, 0.7853981633974407295 ) ;
#52553 = CARTESIAN_POINT ( 'NONE',  ( 104.7329176528308210, 546.5234784715348724, 200.1325441657752151 ) ) ;
#52554 = CARTESIAN_POINT ( 'NONE',  ( 4.000000000000000000, 4.898587196589412829E-16, -2.296599999999999753 ) ) ;
#52555 = ORIENTED_EDGE ( 'NONE', *, *, #74999, .F. ) ;
#52556 = CARTESIAN_POINT ( 'NONE',  ( -2.049017173238487644, -49.86226168011652504, 44.73325810198269181 ) ) ;
#52557 = CARTESIAN_POINT ( 'NONE',  ( -1.469576158976823947E-15, -27.87499999999999645, 8.000000000000000000 ) ) ;
#52558 = DIRECTION ( 'NONE',  ( 0.000000000000000000, -1.000000000000000000, 0.000000000000000000 ) ) ;
#52559 = CARTESIAN_POINT ( 'NONE',  ( -36.06522973182497793, -23.67578041333969452, -31.09724018593250960 ) ) ;
#52560 = CARTESIAN_POINT ( 'NONE',  ( -89.55025994633662378, -30.00000000000000355, 189.4425988133392025 ) ) ;
#52561 = ADVANCED_FACE ( 'NONE', ( #83623 ), #4109, .F. ) ;
#52562 = VECTOR ( 'NONE', #12451, 1000.000000000000000 ) ;
#52563 = ORIENTED_EDGE ( 'NONE', *, *, #106328, .F. ) ;
#52564 = CARTESIAN_POINT ( 'NONE',  ( -26.94608050197553695, 36.94240651728468805, -7.556984339685585361 ) ) ;
#52565 = CARTESIAN_POINT ( 'NONE',  ( 76.55898268265609374, -57.53316911256309396, 194.3133562938762680 ) ) ;
#52566 = AXIS2_PLACEMENT_3D ( 'NONE', #85283, #6875, #65655 ) ;
#52567 = CARTESIAN_POINT ( 'NONE',  ( 46.00000000000000711, 436.0044609852890289, 15.17967024743226645 ) ) ;
#52568 = CARTESIAN_POINT ( 'NONE',  ( 37.71804776410431259, -32.22589162183228240, -37.65546176092030350 ) ) ;
#52569 = FACE_OUTER_BOUND ( 'NONE', #84088, .T. ) ;
#52570 = CIRCLE ( 'NONE', #62917, 4.000000000000003553 ) ;
#52571 = CARTESIAN_POINT ( 'NONE',  ( 1.308996938995747872, -3.000000000000001776, -95.00000000000001421 ) ) ;
#52572 = CARTESIAN_POINT ( 'NONE',  ( -71.88192843937767407, -59.99999999999999289, 153.4067312503538005 ) ) ;
#52573 =( GEOMETRIC_REPRESENTATION_CONTEXT ( 3 ) GLOBAL_UNCERTAINTY_ASSIGNED_CONTEXT ( ( #85006 ) ) GLOBAL_UNIT_ASSIGNED_CONTEXT ( ( #82207, #55790, #40165 ) ) REPRESENTATION_CONTEXT ( 'NONE', 'WORKASPACE' ) );
#52574 = PRESENTATION_LAYER_ASSIGNMENT (  '', '', ( #85313 ) ) ;
#52575 = CARTESIAN_POINT ( 'NONE',  ( -86.80266053460367459, -28.05398439696902457, 186.1832171119652628 ) ) ;
#52576 = ORIENTED_EDGE ( 'NONE', *, *, #102166, .F. ) ;
#52577 = CARTESIAN_POINT ( 'NONE',  ( 30.82851008854570196, 15.24887380073564280, 40.33969805263195241 ) ) ;
#52578 = CARTESIAN_POINT ( 'NONE',  ( -5.068928611176632515, -39.47589145737825334, 30.45902526352114847 ) ) ;
#52579 = STYLED_ITEM ( 'NONE', ( #79868 ), #13656 ) ;
#52580 = CARTESIAN_POINT ( 'NONE',  ( -6.031326303077676698, 41.99459390127218938, -59.73016711425880487 ) ) ;
#52581 = CYLINDRICAL_SURFACE ( 'NONE', #90775, 8.000000000000000000 ) ;
#52583 = FACE_OUTER_BOUND ( 'NONE', #875, .T. ) ;
#52582 = CARTESIAN_POINT ( 'NONE',  ( -22.75399275862038095, 295.1281901880543046, 1.996464526093286507 ) ) ;
#52584 = ORIENTED_EDGE ( 'NONE', *, *, #11537, .T. ) ;
#52585 = CARTESIAN_POINT ( 'NONE',  ( 3.444109705163657007E-15, 24.73290587908618932, 14.06164498842270483 ) ) ;
#52586 = FACE_OUTER_BOUND ( 'NONE', #43182, .T. ) ;
#52587 = DIRECTION ( 'NONE',  ( -1.000000000000000000, -0.000000000000000000, -0.000000000000000000 ) ) ;
#52588 = DIRECTION ( 'NONE',  ( -0.000000000000000000, -1.000000000000000000, -0.000000000000000000 ) ) ;
#52589 = CARTESIAN_POINT ( 'NONE',  ( 21.51569398614867623, 294.9107018935608266, -9.987480606144547579 ) ) ;
#52590 = CARTESIAN_POINT ( 'NONE',  ( 26.97491686565329161, 307.4599153070161606, -9.420584459367200125 ) ) ;
#52591 = DIRECTION ( 'NONE',  ( 0.000000000000000000, -1.000000000000000000, 0.000000000000000000 ) ) ;
#52592 = FILL_AREA_STYLE ('',( #19758 ) ) ;
#52593 = CARTESIAN_POINT ( 'NONE',  ( 87.68135845022958108, -14.21045842199445275, 32.26523303912966156 ) ) ;
#52594 = CARTESIAN_POINT ( 'NONE',  ( -79.80561878445170976, -53.38318872916766367, 161.8232012627484551 ) ) ;
#52595 = ORIENTED_EDGE ( 'NONE', *, *, #50456, .T. ) ;
#52596 = DIRECTION ( 'NONE',  ( 0.000000000000000000, -1.000000000000000000, 0.000000000000000000 ) ) ;
#52597 = DIRECTION ( 'NONE',  ( 0.000000000000000000, -1.000000000000000000, 0.000000000000000000 ) ) ;
#52598 = DIRECTION ( 'NONE',  ( 0.000000000000000000, 0.000000000000000000, 1.000000000000000000 ) ) ;
#52599 = CARTESIAN_POINT ( 'NONE',  ( 39.30001941745848626, 312.0126453433533698, 2.100405576424947629 ) ) ;
#52600 = DIRECTION ( 'NONE',  ( 1.000000000000000000, 1.224606353822377258E-16, 0.000000000000000000 ) ) ;
#52601 = VERTEX_POINT ( 'NONE', #25440 ) ;
#52602 = CARTESIAN_POINT ( 'NONE',  ( -16.96954359408614366, 304.5683848806726814, 9.876757081930351845 ) ) ;
#52603 = CARTESIAN_POINT ( 'NONE',  ( 31.03517274901688694, 439.3343806745134543, 22.67962720703587820 ) ) ;
#52604 = CARTESIAN_POINT ( 'NONE',  ( -5.082755093536325042, -33.59375000204838813, -5.082755093536325930 ) ) ;
#52605 = ORIENTED_EDGE ( 'NONE', *, *, #79709, .F. ) ;
#52606 = AXIS2_PLACEMENT_3D ( 'NONE', #43280, #52419, #41683 ) ;
#52607 = DIRECTION ( 'NONE',  ( 0.000000000000000000, -1.000000000000000000, 0.000000000000000000 ) ) ;
#52608 = CARTESIAN_POINT ( 'NONE',  ( 6.159998411599313606, 41.93068706783093091, -70.02314924739579283 ) ) ;
#52609 = EDGE_CURVE ( 'NONE', #90391, #32226, #71223, .T. ) ;
#52610 = CARTESIAN_POINT ( 'NONE',  ( -23.38163988261890225, 49.99999999999999289, 60.94087333798560735 ) ) ;
#52611 = CARTESIAN_POINT ( 'NONE',  ( -43.00000000000000000, 500.0000000000002274, 15.00000000000000711 ) ) ;
#52612 = B_SPLINE_CURVE_WITH_KNOTS ( 'NONE', 3,
 ( #60477, #50730, #83640, #9745 ),
 .UNSPECIFIED., .F., .F.,
 ( 4, 4 ),
 ( 0.000000000000000000, 0.001128230833659103153 ),
 .UNSPECIFIED. ) ;
#52613 = EDGE_CURVE ( 'NONE', #53891, #74726, #66933, .T. ) ;
#52614 = CARTESIAN_POINT ( 'NONE',  ( -23.21751746555280249, 27.38103382803677022, -33.20617127781034839 ) ) ;
#52615 = VERTEX_POINT ( 'NONE', #91738 ) ;
#52616 = CARTESIAN_POINT ( 'NONE',  ( 92.17363683422854592, -59.99999999999997868, -13.42148695742234921 ) ) ;
#52618 = CARTESIAN_POINT ( 'NONE',  ( 20.07868812831179284, -35.99339030059921640, 30.40546157090997070 ) ) ;
#52617 = CARTESIAN_POINT ( 'NONE',  ( -62.54317499552948334, -60.00000000000000711, 118.0918133646953976 ) ) ;
#52619 = CARTESIAN_POINT ( 'NONE',  ( 33.83237027343564307, 58.72416816948007323, 16.91618513671782509 ) ) ;
#52620 = ADVANCED_FACE ( 'NONE', ( #35658 ), #84702, .F. ) ;
#52621 = CARTESIAN_POINT ( 'NONE',  ( -38.62665293114096698, -49.89296806199684653, 39.81745112272700737 ) ) ;
#52622 = ORIENTED_EDGE ( 'NONE', *, *, #42330, .F. ) ;
#52623 = CARTESIAN_POINT ( 'NONE',  ( 88.48689482502902592, 1.016364837396684119E-14, 0.000000000000000000 ) ) ;
#52624 = SURFACE_STYLE_FILL_AREA ( #102250 ) ;
#52625 = CARTESIAN_POINT ( 'NONE',  ( -43.10371592039292921, 462.6168321841616375, 4.970041475408518927 ) ) ;
#52626 = FACE_OUTER_BOUND ( 'NONE', #13663, .T. ) ;
#52627 = CARTESIAN_POINT ( 'NONE',  ( 7.986539162393901492, -61.02672828942549899, -0.5321833565149892697 ) ) ;
#52628 = LINE ( 'NONE', #11636, #31475 ) ;
#52629 = ORIENTED_EDGE ( 'NONE', *, *, #21622, .T. ) ;
#52630 = CARTESIAN_POINT ( 'NONE',  ( 0.000000000000000000, 0.000000000000000000, -0.02540000000000007530 ) ) ;
#52631 = DIRECTION ( 'NONE',  ( 0.000000000000000000, 0.000000000000000000, -1.000000000000000000 ) ) ;
#52632 = ORIENTED_EDGE ( 'NONE', *, *, #4582, .T. ) ;
#52633 = VECTOR ( 'NONE', #61622, 1000.000000000000000 ) ;
#52634 = CARTESIAN_POINT ( 'NONE',  ( 91.96900705543794174, -29.99999999999987921, 190.8564251733103276 ) ) ;
#52635 = CARTESIAN_POINT ( 'NONE',  ( 41.70086632176889196, 39.59106985249150057, -50.69632281737485613 ) ) ;
#52636 = UNCERTAINTY_MEASURE_WITH_UNIT (LENGTH_MEASURE( 1.000000000000000082E-05 ), #6914, 'distance_accuracy_value', 'NONE');
#52638 = ADVANCED_FACE ( 'NONE', ( #10787 ), #48908, .F. ) ;
#52637 = CARTESIAN_POINT ( 'NONE',  ( 34.42407431220851066, -4.999999999999990230, 0.000000000000000000 ) ) ;
#52639 = CARTESIAN_POINT ( 'NONE',  ( 81.33900641567250034, -30.00000000000000355, -1.065096365412631529 ) ) ;
#52640 = VERTEX_POINT ( 'NONE', #17326 ) ;
#52641 = VECTOR ( 'NONE', #85166, 999.9999999999998863 ) ;
#52642 = ORIENTED_EDGE ( 'NONE', *, *, #10190, .F. ) ;
#52643 = VERTEX_POINT ( 'NONE', #42108 ) ;
#52644 = CARTESIAN_POINT ( 'NONE',  ( 22.33349330513380337, -4.000000000000000888, 4.898587196589416773E-16 ) ) ;
#52645 = DIRECTION ( 'NONE',  ( 0.000000000000000000, 0.000000000000000000, -1.000000000000000000 ) ) ;
#52646 = CARTESIAN_POINT ( 'NONE',  ( -15.71086122448608613, 303.5558210301048803, 9.874087016084169832 ) ) ;
#52647 = VECTOR ( 'NONE', #100122, 1000.000000000000000 ) ;
#52648 = AXIS2_PLACEMENT_3D ( 'NONE', #73576, #81143, #89787 ) ;
#52649 = CARTESIAN_POINT ( 'NONE',  ( 4.660674839411965920, -11.31782485304406904, -3.778981567323763890 ) ) ;
#52650 = CARTESIAN_POINT ( 'NONE',  ( -31.39343312534550989, 438.8553142255844364, 23.06001087143945227 ) ) ;
#52651 = DIRECTION ( 'NONE',  ( 0.000000000000000000, 0.000000000000000000, 1.000000000000000000 ) ) ;
#52652 = CARTESIAN_POINT ( 'NONE',  ( 25.60851123679735863, 50.00000000031798919, -75.29411764726214074 ) ) ;
#52653 = ORIENTED_EDGE ( 'NONE', *, *, #6332, .T. ) ;
#52654 = CARTESIAN_POINT ( 'NONE',  ( -11.68767211932491179, 50.00000000000000000, -81.85902538600507228 ) ) ;
#52655 = ORIENTED_EDGE ( 'NONE', *, *, #71304, .T. ) ;
#52656 = CARTESIAN_POINT ( 'NONE',  ( 74.38267031189917589, -38.32888619803856756, 163.7218043044017293 ) ) ;
#52657 = DIRECTION ( 'NONE',  ( 0.000000000000000000, -1.000000000000000000, 0.000000000000000000 ) ) ;
#52658 = CIRCLE ( 'NONE', #42332, 1.000000000000000222 ) ;
#52659 = CARTESIAN_POINT ( 'NONE',  ( 24.90251836858309886, 295.6281153014862753, 2.103653583787406856 ) ) ;
#52660 = AXIS2_PLACEMENT_3D ( 'NONE', #44131, #50077, #101303 ) ;
#52661 = VECTOR ( 'NONE', #40523, 1000.000000000000000 ) ;
#52662 = FACE_OUTER_BOUND ( 'NONE', #94093, .T. ) ;
#52663 = PRODUCT_DEFINITION_SHAPE ( 'NONE', 'NONE',  #106787 ) ;
#52664 = ORIENTED_EDGE ( 'NONE', *, *, #56058, .T. ) ;
#52665 = DIRECTION ( 'NONE',  ( -1.000000000000000000, -0.000000000000000000, -0.000000000000000000 ) ) ;
#52666 = VECTOR ( 'NONE', #72449, 1000.000000000000000 ) ;
#52667 = CARTESIAN_POINT ( 'NONE',  ( 100.6222222222222200, 1.023464760207051730E-14, 0.000000000000000000 ) ) ;
#52668 = DIRECTION ( 'NONE',  ( -1.000000000000000000, 0.000000000000000000, 0.000000000000000000 ) ) ;
#52669 = CARTESIAN_POINT ( 'NONE',  ( 22.61650669486618526, 4.898587196589413815E-16, -4.000000000000000888 ) ) ;
#52670 = ADVANCED_FACE ( 'NONE', ( #54424 ), #45378, .T. ) ;
#52671 = ORIENTED_EDGE ( 'NONE', *, *, #48638, .T. ) ;
#52672 = DIRECTION ( 'NONE',  ( 0.000000000000000000, -1.000000000000000000, 0.000000000000000000 ) ) ;
#52673 = SURFACE_SIDE_STYLE ('',( #29515 ) ) ;
#52674 = CARTESIAN_POINT ( 'NONE',  ( 89.99999999999997158, -52.00000000000000000, 196.0238439516549818 ) ) ;
#52675 = EDGE_CURVE ( 'NONE', #38791, #63501, #29553, .T. ) ;
#52676 = ADVANCED_FACE ( 'NONE', ( #13450 ), #24747, .T. ) ;
#52677 = DIRECTION ( 'NONE',  ( 0.000000000000000000, 0.000000000000000000, -1.000000000000000000 ) ) ;
#52678 = CARTESIAN_POINT ( 'NONE',  ( 29.08076923076923137, 1.411358822780289120E-15, 0.000000000000000000 ) ) ;
#52679 = CARTESIAN_POINT ( 'NONE',  ( 86.30431136706036455, -24.61821740116755208, 182.2296409677384759 ) ) ;
#52680 = CARTESIAN_POINT ( 'NONE',  ( 17.99637020931140441, 36.53998198029805877, -22.85704674614672172 ) ) ;
#52681 = CARTESIAN_POINT ( 'NONE',  ( -8.971954110182338127, 136.3305255230980606, 4.999999999999998224 ) ) ;
#52682 = EDGE_LOOP ( 'NONE', ( #46225, #22457, #49732, #2972 ) ) ;
#52683 = LINE ( 'NONE', #34949, #106695 ) ;
#52684 = CARTESIAN_POINT ( 'NONE',  ( -3.462711550064783150, -15.46674754799754226, -35.18986906109944357 ) ) ;
#52685 = CARTESIAN_POINT ( 'NONE',  ( 0.000000000000000000, 0.000000000000000000, 0.000000000000000000 ) ) ;
#52686 = CARTESIAN_POINT ( 'NONE',  ( 13.42019126081076941, -52.95647893691098318, 30.98765330636284077 ) ) ;
#52687 = DIRECTION ( 'NONE',  ( 0.000000000000000000, 0.000000000000000000, 1.000000000000000000 ) ) ;
#52688 = AXIS2_PLACEMENT_3D ( 'NONE', #50042, #16620, #9575 ) ;
#52689 = CARTESIAN_POINT ( 'NONE',  ( -94.06284170466219052, -29.99999999999999289, 112.3432347928509074 ) ) ;
#52690 = ADVANCED_FACE ( 'NONE', ( #94405 ), #59162, .F. ) ;
#52691 = CARTESIAN_POINT ( 'NONE',  ( 0.000000000000000000, 34.19642918197134662, -12.16579798332631945 ) ) ;
#52692 = CARTESIAN_POINT ( 'NONE',  ( 35.03266159394272705, -57.69518171884941893, 49.17802768995313301 ) ) ;
#52694 = DIRECTION ( 'NONE',  ( -1.000000000000000000, -1.224606353822377258E-16, -0.000000000000000000 ) ) ;
#52693 = CARTESIAN_POINT ( 'NONE',  ( 37.38584400634713489, 490.8443720919671023, 12.40597885709908077 ) ) ;
#52695 = EDGE_CURVE ( 'NONE', #70272, #105135, #92548, .T. ) ;
#52696 = CARTESIAN_POINT ( 'NONE',  ( -30.04543272336563575, 41.08154905281699598, -66.19662526517841172 ) ) ;
#52697 = DIRECTION ( 'NONE',  ( 1.000000000000000000, 0.000000000000000000, 0.000000000000000000 ) ) ;
#52698 = DIRECTION ( 'NONE',  ( 1.000000000000000000, 0.000000000000000000, 0.000000000000000000 ) ) ;
#52699 = CARTESIAN_POINT ( 'NONE',  ( 7.022229286271646664, -4.221542269094484823, -17.11103215588186544 ) ) ;
#52700 = SURFACE_STYLE_USAGE ( .BOTH. , #93711 ) ;
#52701 = EDGE_CURVE ( 'NONE', #15859, #38000, #1200, .T. ) ;
#52702 = CARTESIAN_POINT ( 'NONE',  ( 23.19675064131305930, -19.50463141275981016, -33.27316171080115481 ) ) ;
#52703 = AXIS2_PLACEMENT_3D ( 'NONE', #96088, #22754, #55071 ) ;
#52704 = CARTESIAN_POINT ( 'NONE',  ( -22.09705705695840550, -25.55721621211691286, 28.90405252608048414 ) ) ;
#52705 = ORIENTED_EDGE ( 'NONE', *, *, #1475, .T. ) ;
#52706 = CARTESIAN_POINT ( 'NONE',  ( 5.817469134863316960, 12.07282864079881790, 3.893337541178056416 ) ) ;
#52707 =( LENGTH_UNIT ( ) NAMED_UNIT ( * ) SI_UNIT ( .MILLI., .METRE. ) );
#52708 = CARTESIAN_POINT ( 'NONE',  ( -16.57135497164903981, -29.03224908037524798, 28.95071076732330795 ) ) ;
#52709 =( BOUNDED_SURFACE ( )  B_SPLINE_SURFACE ( 3, 2, ( 
 ( #53925, #78213, #29702 ),
 ( #4327, #86856, #12932 ),
 ( #37262, #60468, #45852 ),
 ( #61524, #93873, #44262 ) ),
 .UNSPECIFIED., .F., .F., .F. ) 
 B_SPLINE_SURFACE_WITH_KNOTS ( ( 4, 4 ),
 ( 3, 3 ),
 ( 4.163336342344337027E-17, 0.0002182426145221272784 ),
 ( 0.000000000000000000, 1.000000000000000000 ),
 .UNSPECIFIED. ) 
 GEOMETRIC_REPRESENTATION_ITEM ( )  RATIONAL_B_SPLINE_SURFACE ( (
 ( 1.000000000000000000, 0.8308329163121006555, 1.000000000000000000),
 ( 1.000000000000000000, 0.8297634434905108991, 1.000000000000000000),
 ( 1.000000000000000000, 0.8286461416559528503, 1.000000000000000000),
 ( 1.000000000000000000, 0.8274831119537282564, 1.000000000000000000) ) ) 
 REPRESENTATION_ITEM ( '' )  SURFACE ( )  );
#52711 = CARTESIAN_POINT ( 'NONE',  ( -39.33352494920633546, 438.9614613858099119, 23.36191803517838395 ) ) ;
#52710 = CARTESIAN_POINT ( 'NONE',  ( -0.6415267897369668626, 27.35808064800162853, 40.57598378311829634 ) ) ;
#52712 = MECHANICAL_DESIGN_GEOMETRIC_PRESENTATION_REPRESENTATION (  '', ( #69971 ), #81958 ) ;
#52713 = EDGE_LOOP ( 'NONE', ( #27066, #78260, #61847, #87138, #105391, #75776 ) ) ;
#52714 = DIRECTION ( 'NONE',  ( 0.5735764363510440500, 0.8191520442889932418, 0.000000000000000000 ) ) ;
#52715 = ORIENTED_EDGE ( 'NONE', *, *, #31090, .T. ) ;
#52716 = DIRECTION ( 'NONE',  ( 1.000000000000000000, -0.000000000000000000, -0.000000000000000000 ) ) ;
#52717 = VECTOR ( 'NONE', #35073, 1000.000000000000000 ) ;
#52718 = CARTESIAN_POINT ( 'NONE',  ( 72.85555555555556850, 6.915964383211875250E-15, 0.000000000000000000 ) ) ;
#52719 = CIRCLE ( 'NONE', #61369, 7.500000000000000888 ) ;
#52720 = CARTESIAN_POINT ( 'NONE',  ( 74.07777777777778283, 6.915964383211875250E-15, 0.000000000000000000 ) ) ;
#52721 = ORIENTED_EDGE ( 'NONE', *, *, #67922, .F. ) ;
#52722 = CARTESIAN_POINT ( 'NONE',  ( 33.07276483573660641, 438.9325140356084489, 23.89537236861389502 ) ) ;
#52723 = CIRCLE ( 'NONE', #104393, 4.000000000000000888 ) ;
#52724 = CARTESIAN_POINT ( 'NONE',  ( 10.47772246152095477, 50.00000000000000711, -91.06170733474699830 ) ) ;
#52725 = AXIS2_PLACEMENT_3D ( 'NONE', #16809, #34089, #66961 ) ;
#52726 = CARTESIAN_POINT ( 'NONE',  ( 103.7490062218180356, -60.15690558421150058, 191.4294801856832180 ) ) ;
#52727 = MECHANICAL_DESIGN_GEOMETRIC_PRESENTATION_REPRESENTATION (  '', ( #50945 ), #102708 ) ;
#52729 = DIRECTION ( 'NONE',  ( 0.000000000000000000, 1.000000000000000000, 1.224646799147353207E-16 ) ) ;
#52728 = CARTESIAN_POINT ( 'NONE',  ( 35.17791155467128306, -33.08171577008500464, 34.16701531372348200 ) ) ;
#52730 = ORIENTED_EDGE ( 'NONE', *, *, #41088, .T. ) ;
#52731 = AXIS2_PLACEMENT_3D ( 'NONE', #103111, #29262, #29782 ) ;
#52732 = ORIENTED_EDGE ( 'NONE', *, *, #101530, .T. ) ;
#52733 = STYLED_ITEM ( 'NONE', ( #50177 ), #14716 ) ;
#52734 = ORIENTED_EDGE ( 'NONE', *, *, #22258, .T. ) ;
#52735 = CARTESIAN_POINT ( 'NONE',  ( 23.77937657248197922, 306.1093036377834551, 9.213915351946365462 ) ) ;
#52736 = CARTESIAN_POINT ( 'NONE',  ( -40.45545246860710620, 460.8457769820571457, 2.191470225627486723 ) ) ;
#52737 = PLANE ( 'NONE',  #93274 ) ;
#52738 = ORIENTED_EDGE ( 'NONE', *, *, #49904, .F. ) ;
#52739 = EDGE_CURVE ( 'NONE', #4006, #66536, #55724, .T. ) ;
#52740 = DIRECTION ( 'NONE',  ( 0.000000000000000000, 1.000000000000000000, 0.000000000000000000 ) ) ;
#52741 = CARTESIAN_POINT ( 'NONE',  ( -5.175364584845236315, 41.93912275385426369, -69.86374487332780348 ) ) ;
#52742 = CARTESIAN_POINT ( 'NONE',  ( -88.66004994158249986, -60.00000000000486011, -24.41333391927541641 ) ) ;
#52743 = DIRECTION ( 'NONE',  ( 0.000000000000000000, 1.000000000000000000, 0.000000000000000000 ) ) ;
#52744 = CARTESIAN_POINT ( 'NONE',  ( 2.816747937689971781, -59.99999999995171862, -45.00000176639943561 ) ) ;
#52745 = CARTESIAN_POINT ( 'NONE',  ( -16.39454849390063629, -4.999999999999998224, -0.9786395306135168282 ) ) ;
#52746 = CARTESIAN_POINT ( 'NONE',  ( -5.659803839289578420, 41.67004224697031844, -58.69865676442391589 ) ) ;
#52748 = CARTESIAN_POINT ( 'NONE',  ( 6.981006337927150973, -18.58620748038632442, 26.97765893144556770 ) ) ;
#52747 = CARTESIAN_POINT ( 'NONE',  ( -112.0516705497441876, -59.99999999999997868, 140.8505598867089645 ) ) ;
#52749 = EDGE_CURVE ( 'NONE', #73667, #25325, #45014, .T. ) ;
#52750 = CARTESIAN_POINT ( 'NONE',  ( 18.86650669486618881, -3.851859888774471706E-31, 4.000000000000000888 ) ) ;
#52751 = EDGE_CURVE ( 'NONE', #103692, #57232, #8910, .T. ) ;
#52752 = CARTESIAN_POINT ( 'NONE',  ( -48.01388463784094540, -42.98496168698468267, 48.71257218748448281 ) ) ;
#52753 = ORIENTED_EDGE ( 'NONE', *, *, #43936, .T. ) ;
#52754 = CARTESIAN_POINT ( 'NONE',  ( -4.000000000000000000, 17.85270131633358304, 5.744562646538042827 ) ) ;
#52755 = PRODUCT_DEFINITION_SHAPE ( 'NONE', 'NONE',  #39722 ) ;
#52756 = VERTEX_POINT ( 'NONE', #8949 ) ;
#52757 = CARTESIAN_POINT ( 'NONE',  ( 35.45036406932566564, 436.3203772529585649, 5.179456583034234285 ) ) ;
#52758 = CARTESIAN_POINT ( 'NONE',  ( 0.000000000000000000, 36.79151656018385097, 0.000000000000000000 ) ) ;
#52759 = EDGE_CURVE ( 'NONE', #10334, #46987, #100388, .T. ) ;
#52760 = CARTESIAN_POINT ( 'NONE',  ( 6.352644769543418946, 2.685840869108941931, 6.500000000000298428 ) ) ;
#52762 = ORIENTED_EDGE ( 'NONE', *, *, #64402, .T. ) ;
#52761 = COLOUR_RGB ( '', 0.31764706, 0.68627451, 0.89019608) ;
#52763 = CARTESIAN_POINT ( 'NONE',  ( 9.797174393178825657E-16, 0.000000000000000000, 8.000000000000000000 ) ) ;
#52764 = ORIENTED_EDGE ( 'NONE', *, *, #8547, .F. ) ;
#52765 = CARTESIAN_POINT ( 'NONE',  ( 90.72652982786716791, -30.00000000012070345, 36.53626809240827811 ) ) ;
#52766 = FACE_OUTER_BOUND ( 'NONE', #81212, .T. ) ;
#52767 =( NAMED_UNIT ( * ) SI_UNIT ( $, .STERADIAN. ) SOLID_ANGLE_UNIT ( ) );
#52769 = EDGE_CURVE ( 'NONE', #13768, #56970, #86723, .T. ) ;
#52768 = FACE_OUTER_BOUND ( 'NONE', #32374, .T. ) ;
#52770 = AXIS2_PLACEMENT_3D ( 'NONE', #9890, #42801, #7766 ) ;
#52771 = CARTESIAN_POINT ( 'NONE',  ( -38.36535705883633085, 18.64316884711714195, 5.022013495247505510 ) ) ;
#52772 = CARTESIAN_POINT ( 'NONE',  ( 91.30097760447456778, -30.00000000000000000, 190.6181298806798736 ) ) ;
#52773 = DIRECTION ( 'NONE',  ( 0.000000000000000000, -0.4999999999999996114, 0.8660254037844388186 ) ) ;
#52774 = ORIENTED_EDGE ( 'NONE', *, *, #43711, .T. ) ;
#52775 = ORIENTED_EDGE ( 'NONE', *, *, #38834, .F. ) ;
#52776 = VERTEX_POINT ( 'NONE', #100087 ) ;
#52777 = CARTESIAN_POINT ( 'NONE',  ( 53.77059603358078022, -53.37413041404379754, 63.18823621241026700 ) ) ;
#52778 = CARTESIAN_POINT ( 'NONE',  ( 7.090506028190234566, 41.24768140130692728, -58.61601156502441512 ) ) ;
#52779 = DIRECTION ( 'NONE',  ( 0.000000000000000000, -1.000000000000000000, 0.000000000000000000 ) ) ;
#52780 = ORIENTED_EDGE ( 'NONE', *, *, #102752, .F. ) ;
#52781 = CARTESIAN_POINT ( 'NONE',  ( -88.12222426954021159, -38.37225613763864374, -19.40653620767198007 ) ) ;
#52782 = ORIENTED_EDGE ( 'NONE', *, *, #27418, .F. ) ;
#52783 = SURFACE_SIDE_STYLE ('',( #53327 ) ) ;
#52784 = CARTESIAN_POINT ( 'NONE',  ( 108.2513347943879722, -38.35773709419970601, 192.2701858252870295 ) ) ;
#52785 = CARTESIAN_POINT ( 'NONE',  ( 13.10236887572196274, 21.82069291473259298, 4.738654922942245662 ) ) ;
#52786 = CARTESIAN_POINT ( 'NONE',  ( 86.12903045990179862, -60.13851843310877854, 12.57144976733284025 ) ) ;
#52787 = CARTESIAN_POINT ( 'NONE',  ( 40.91702039389569023, 378.5672949884566378, 26.48911381135054555 ) ) ;
#52788 = CARTESIAN_POINT ( 'NONE',  ( 5.446322446741273637, -11.07408952718074602, -10.13262891269592458 ) ) ;
#52789 = APPLICATION_CONTEXT ( 'automotive_design' ) ;
#52790 = CARTESIAN_POINT ( 'NONE',  ( 86.17777777777776294, -4.171999999999998820, 5.616230220889773285E-16 ) ) ;
#52791 = AXIS2_PLACEMENT_3D ( 'NONE', #40853, #33321, #58095 ) ;
#52792 = CARTESIAN_POINT ( 'NONE',  ( -16.64348903516526335, 43.75610143575153899, -4.157797401561264650 ) ) ;
#52793 = CARTESIAN_POINT ( 'NONE',  ( 8.986804597297368247, 136.5680015418640778, 4.999999999999385381 ) ) ;
#52794 = ORIENTED_EDGE ( 'NONE', *, *, #50695, .F. ) ;
#52795 = CARTESIAN_POINT ( 'NONE',  ( 63.56127108291158123, 6.975173280561618775E-15, 0.000000000000000000 ) ) ;
#52796 = VECTOR ( 'NONE', #67699, 1000.000000000000000 ) ;
#52797 = DIRECTION ( 'NONE',  ( 0.000000000000000000, 1.000000000000000000, -1.224646799147353207E-16 ) ) ;
#52798 = DIRECTION ( 'NONE',  ( -1.000000000000000000, -1.224606353822377258E-16, -0.000000000000000000 ) ) ;
#52799 = ORIENTED_EDGE ( 'NONE', *, *, #18306, .F. ) ;
#52800 = CARTESIAN_POINT ( 'NONE',  ( -33.57932678495680534, 327.5754790332646280, -3.422513633634138408 ) ) ;
#52801 = CARTESIAN_POINT ( 'NONE',  ( -37.52685452098302932, 308.4526037119397870, 5.153401396366573906 ) ) ;
#52802 = DIRECTION ( 'NONE',  ( -1.000000000000000000, -0.000000000000000000, -0.000000000000000000 ) ) ;
#52803 = CARTESIAN_POINT ( 'NONE',  ( -13.00569629258622939, 42.57699573218433642, -92.62012368208512214 ) ) ;
#52804 = CARTESIAN_POINT ( 'NONE',  ( -5.656854249492379694, -23.93749999999999289, -5.656854249492380582 ) ) ;
#52805 = CARTESIAN_POINT ( 'NONE',  ( 2.957810341175842961, -12.64483219941317138, 32.16612171018341826 ) ) ;
#52806 = EDGE_CURVE ( 'NONE', #49640, #77164, #78077, .T. ) ;
#52807 = MECHANICAL_DESIGN_GEOMETRIC_PRESENTATION_REPRESENTATION (  '', ( #95854 ), #97519 ) ;
#52808 = AXIS2_PLACEMENT_3D ( 'NONE', #24739, #16621, #106142 ) ;
#52809 = DIRECTION ( 'NONE',  ( -1.000000000000000000, -0.000000000000000000, -0.000000000000000000 ) ) ;
#52810 = VECTOR ( 'NONE', #78860, 1000.000000000000000 ) ;
#52811 = ORIENTED_EDGE ( 'NONE', *, *, #85297, .T. ) ;
#52812 = CARTESIAN_POINT ( 'NONE',  ( 86.11061767232767750, -21.49857324288878502, 175.3763454229637659 ) ) ;
#52813 = CARTESIAN_POINT ( 'NONE',  ( 88.48689482502902592, -2.002967142162725287E-29, 5.000000000000011546 ) ) ;
#52814 = CARTESIAN_POINT ( 'NONE',  ( -16.32302039041868724, 45.99487210642904955, 4.188696036803978728 ) ) ;
#52815 = ORIENTED_EDGE ( 'NONE', *, *, #33202, .F. ) ;
#52816 = CARTESIAN_POINT ( 'NONE',  ( -87.71484843151664279, -60.15235330828886617, 36.79746090376434609 ) ) ;
#52817 = DIRECTION ( 'NONE',  ( 0.000000000000000000, 0.000000000000000000, -1.000000000000000000 ) ) ;
#52818 = CARTESIAN_POINT ( 'NONE',  ( -10.71924530988990476, -5.000000000000002665, -74.44967652504222144 ) ) ;
#52819 = CARTESIAN_POINT ( 'NONE',  ( 0.000000000000000000, 304.8518027762758038, 8.936999415352287812 ) ) ;
#52820 = STYLED_ITEM ( 'NONE', ( #72479 ), #15259 ) ;
#52821 = CARTESIAN_POINT ( 'NONE',  ( -4.823443502104696634, -21.62908485124496138, -38.54787723814094846 ) ) ;
#52822 = CARTESIAN_POINT ( 'NONE',  ( 29.71588918770380161, -60.00000000000002132, 42.89755770512662991 ) ) ;
#52823 = CARTESIAN_POINT ( 'NONE',  ( 14.84465811918519584, -22.60273344730966727, 35.91147243655147037 ) ) ;
#52824 = CARTESIAN_POINT ( 'NONE',  ( 3.471301144393694749, -0.8437115307660071339, 103.7432070447316050 ) ) ;
#52825 = CARTESIAN_POINT ( 'NONE',  ( 39.86870225387427524, -26.26949144110688650, 35.87748434985530821 ) ) ;
#52827 = CARTESIAN_POINT ( 'NONE',  ( -12.41697196639879586, 22.56423331549411415, 6.101092351693879756 ) ) ;
#52826 = CARTESIAN_POINT ( 'NONE',  ( -33.24326047732412093, -34.51171323919459155, 42.75321002329071973 ) ) ;
#52828 = ADVANCED_FACE ( 'NONE', ( #18136 ), #31612, .T. ) ;
#52829 = CARTESIAN_POINT ( 'NONE',  ( 5.833922283576983503, 294.7609306416175059, -8.134666899186667521 ) ) ;
#52830 = CARTESIAN_POINT ( 'NONE',  ( 45.48003679188781234, 379.8448106960472614, 7.220331889307936457 ) ) ;
#52831 =( NAMED_UNIT ( * ) SI_UNIT ( $, .STERADIAN. ) SOLID_ANGLE_UNIT ( ) );
#52832 = CARTESIAN_POINT ( 'NONE',  ( 6.222742520105473574, 7.673830019007162662, 0.2914634815676395707 ) ) ;
#52833 = ORIENTED_EDGE ( 'NONE', *, *, #52062, .T. ) ;
#52834 = ADVANCED_FACE ( 'NONE', ( #17063 ), #82846, .F. ) ;
#52835 = FACE_OUTER_BOUND ( 'NONE', #11588, .T. ) ;
#52836 = CONICAL_SURFACE ( 'NONE', #87344, 3.309500000000001663, 0.9599310885968770357 ) ;
#52837 = CARTESIAN_POINT ( 'NONE',  ( -2.064928172609607149, -60.00000000000000711, 39.63619459862159289 ) ) ;
#52838 = ORIENTED_EDGE ( 'NONE', *, *, #32136, .T. ) ;
#52839 = CARTESIAN_POINT ( 'NONE',  ( -12.32676478774256523, -2.923359614653776362, 20.67314872818923988 ) ) ;
#52840 = FACE_OUTER_BOUND ( 'NONE', #31712, .T. ) ;
#52841 = CONICAL_SURFACE ( 'NONE', #66625, 4.000000000000001776, 0.9599310885968774798 ) ;
#52842 = DIRECTION ( 'NONE',  ( -1.000000000000000000, -1.224606353822377258E-16, -0.000000000000000000 ) ) ;
#52844 = CARTESIAN_POINT ( 'NONE',  ( -19.42937613716337353, -60.22819676930696886, -36.14109189875915717 ) ) ;
#52843 = CARTESIAN_POINT ( 'NONE',  ( 19.50000000000000000, 12.99999999999999289, 0.000000000000000000 ) ) ;
#52845 = B_SPLINE_CURVE_WITH_KNOTS ( 'NONE', 3,
 ( #94746, #20895, #45650, #78526, #37592, #95265, #2510, #35455, #68329, #101225 ),
 .UNSPECIFIED., .F., .F.,
 ( 4, 2, 2, 2, 4 ),
 ( -2.000195913693545311E-05, 0.001085800244612924147, 0.002191602448362783492, 0.003297404652112643272, 0.004403206855862503051 ),
 .UNSPECIFIED. ) ;
#52846 = ORIENTED_EDGE ( 'NONE', *, *, #97623, .T. ) ;
#52847 = DIRECTION ( 'NONE',  ( 1.000000000000000000, 0.000000000000000000, 0.000000000000000000 ) ) ;
#52848 = CARTESIAN_POINT ( 'NONE',  ( -3.999986872311680042, -9.563226186441980303, 6.928210809543925208 ) ) ;
#52849 = ORIENTED_EDGE ( 'NONE', *, *, #55747, .T. ) ;
#52850 = DIRECTION ( 'NONE',  ( -1.000000000000000000, -0.000000000000000000, -0.000000000000000000 ) ) ;
#52851 = DIRECTION ( 'NONE',  ( -1.000000000000000000, -1.224606353822377258E-16, -0.000000000000000000 ) ) ;
#52852 = PRODUCT_DEFINITION ( 'UNKNOWN', '', #66325, #1392 ) ;
#52853 = CARTESIAN_POINT ( 'NONE',  ( -92.22380160643884039, -59.99999999999999289, 2.566636606020737954 ) ) ;
#52854 = EDGE_LOOP ( 'NONE', ( #92891, #40375, #67760, #47181, #93222, #104250 ) ) ;
#52855 = CARTESIAN_POINT ( 'NONE',  ( -27.10511071441183262, -1.200000000000000030E-05, 10.05698433968616001 ) ) ;
#52856 = CARTESIAN_POINT ( 'NONE',  ( 11.36650669486618881, 1.474610560812782335E-15, 0.000000000000000000 ) ) ;
#52857 = DIRECTION ( 'NONE',  ( -0.000000000000000000, -1.000000000000000000, -0.000000000000000000 ) ) ;
#52858 = CARTESIAN_POINT ( 'NONE',  ( 0.000000000000000000, 0.000000000000000000, 4.000000000000000888 ) ) ;
#52859 = VECTOR ( 'NONE', #31505, 1000.000000000000114 ) ;
#52860 = CARTESIAN_POINT ( 'NONE',  ( 37.83989825151499531, 491.0717236019729057, 13.27726931866749460 ) ) ;
#52861 = CARTESIAN_POINT ( 'NONE',  ( -82.18019381229618148, -42.97457168899456548, 167.7073896577822154 ) ) ;
#52862 = ORIENTED_EDGE ( 'NONE', *, *, #52359, .F. ) ;
#52863 = CARTESIAN_POINT ( 'NONE',  ( -11.24487389204439580, 0.000000000000000000, -12.81917055449304854 ) ) ;
#52864 = EDGE_LOOP ( 'NONE', ( #78022, #78073, #3405, #22438, #34040, #56189 ) ) ;
#52865 = ORIENTED_EDGE ( 'NONE', *, *, #48450, .T. ) ;
#52866 = CARTESIAN_POINT ( 'NONE',  ( -17.55833715088017044, -4.999999999999999112, -1.075502477179389960 ) ) ;
#52867 = CARTESIAN_POINT ( 'NONE',  ( -1.139671569113011707, -70.62079937436291743, 13.04394488173644540 ) ) ;
#52868 =( NAMED_UNIT ( * ) PLANE_ANGLE_UNIT ( ) SI_UNIT ( $, .RADIAN. ) );
#52869 = ORIENTED_EDGE ( 'NONE', *, *, #34582, .F. ) ;
#52870 = DIRECTION ( 'NONE',  ( -0.000000000000000000, 1.000000000000000000, -0.000000000000000000 ) ) ;
#52871 = CARTESIAN_POINT ( 'NONE',  ( -94.30414684669057124, -57.67279326051714605, 1.132156541063573441 ) ) ;
#52872 = CARTESIAN_POINT ( 'NONE',  ( 6.928203230275508773, -10.26479267253572480, 3.999999999999999112 ) ) ;
#52873 = ADVANCED_FACE ( 'NONE', ( #28920 ), #91859, .F. ) ;
#52874 = CARTESIAN_POINT ( 'NONE',  ( 33.58349330513379982, 1.593028355512270567E-15, 0.000000000000000000 ) ) ;
#52875 = CIRCLE ( 'NONE', #40867, 3.309500000000001663 ) ;
#52876 = CARTESIAN_POINT ( 'NONE',  ( 24.47192364801414755, 27.44308780173428985, 32.07880713850987320 ) ) ;
#52877 = CARTESIAN_POINT ( 'NONE',  ( -13.98725534264629466, -50.02704942377346953, 27.65002740835610240 ) ) ;
#52878 = STYLED_ITEM ( 'NONE', ( #47273 ), #59337 ) ;
#52879 = CARTESIAN_POINT ( 'NONE',  ( -17.53793833829797322, 36.29671191971048927, -24.04345926538308831 ) ) ;
#52880 = CARTESIAN_POINT ( 'NONE',  ( 93.27827242126578255, -14.21045842199433729, 72.77868743038563082 ) ) ;
#52881 = SHAPE_REPRESENTATION ( '2. Holder', ( #10728 ), #93449 ) ;
#52882 = EDGE_CURVE ( 'NONE', #32906, #70854, #580, .T. ) ;
#52883 = CARTESIAN_POINT ( 'NONE',  ( -104.4188068117427264, -29.99999999999997868, 196.2181340123987923 ) ) ;
#52884 = CARTESIAN_POINT ( 'NONE',  ( -55.55496807634862932, -60.32879899568890636, 70.31421429908731113 ) ) ;
#52885 = ORIENTED_EDGE ( 'NONE', *, *, #7981, .T. ) ;
#52886 = FACE_OUTER_BOUND ( 'NONE', #25222, .T. ) ;
#52888 = ORIENTED_EDGE ( 'NONE', *, *, #68759, .T. ) ;
#52887 = VECTOR ( 'NONE', #91064, 1000.000000000000000 ) ;
#52889 = PRESENTATION_LAYER_ASSIGNMENT (  '', '', ( #32274 ) ) ;
#52890 = CARTESIAN_POINT ( 'NONE',  ( -102.5962067017768220, -37.82042529878841464, 179.2107196536337597 ) ) ;
#52891 = DIRECTION ( 'NONE',  ( 0.000000000000000000, 1.000000000000000000, 0.000000000000000000 ) ) ;
#52892 = CARTESIAN_POINT ( 'NONE',  ( -5.855392133367304908, 51.27352836932585944, 8.399161085123857617 ) ) ;
#52893 = VERTEX_POINT ( 'NONE', #102223 ) ;
#52894 = CARTESIAN_POINT ( 'NONE',  ( 19.49590807900633038, 49.99971735798833095, 59.99840023191819682 ) ) ;
#52895 = CARTESIAN_POINT ( 'NONE',  ( -9.878668896128520061, -59.99999999999998579, 39.64507338328628094 ) ) ;
#52896 = CARTESIAN_POINT ( 'NONE',  ( -2.100699074824130985, -0.1482055178558705777, 102.1543794502939022 ) ) ;
#52897 = CARTESIAN_POINT ( 'NONE',  ( -2.977408999572650039, -16.06250000204838457, -7.188101187500001821 ) ) ;
#52898 = CARTESIAN_POINT ( 'NONE',  ( 0.5805565836007654523, 7.505553499465140277, 2.211437577243512467E-16 ) ) ;
#52899 = CIRCLE ( 'NONE', #32285, 4.000000000000001776 ) ;
#52901 = ADVANCED_FACE ( 'NONE', ( #101161 ), #19764, .T. ) ;
#52900 = CARTESIAN_POINT ( 'NONE',  ( 14.85284876471456350, 5.000000000000003553, 0.000000000000000000 ) ) ;
#52902 = CARTESIAN_POINT ( 'NONE',  ( 7.801339272325196639, -81.41268528040301078, -1.788609912539668612 ) ) ;
#52903 = CARTESIAN_POINT ( 'NONE',  ( -11.55835547680480069, -4.925501566984745061, -12.56497939361423200 ) ) ;
#52904 = CARTESIAN_POINT ( 'NONE',  ( 43.00000000000000000, 485.2629658518202405, -2.796394914059364911 ) ) ;
#52905 = ADVANCED_FACE ( 'NONE', ( #60724 ), #21301, .T. ) ;
#52906 = CARTESIAN_POINT ( 'NONE',  ( -8.613443109969679767, 128.9903607843504005, -5.777789833161706683E-31 ) ) ;
#52907 = CARTESIAN_POINT ( 'NONE',  ( -7.500000000000001776, 13.44157116919690331, -32.95552552993890316 ) ) ;
#52908 = CARTESIAN_POINT ( 'NONE',  ( -28.08878474957800719, -29.05689031911417430, 30.69116238151102749 ) ) ;
#52909 = CARTESIAN_POINT ( 'NONE',  ( -18.00000000000000355, 12.99999999999999289, 0.000000000000000000 ) ) ;
#52910 = EDGE_CURVE ( 'NONE', #6036, #70572, #38514, .T. ) ;
#52911 = CARTESIAN_POINT ( 'NONE',  ( 46.97773782595957925, -60.26704657434898138, 52.32291326186037850 ) ) ;
#52912 = CARTESIAN_POINT ( 'NONE',  ( 6.162888688655347558, 7.505553499465140277, 0.000000000000000000 ) ) ;
#52913 = CARTESIAN_POINT ( 'NONE',  ( 0.000000000000000000, 0.000000000000000000, 0.000000000000000000 ) ) ;
#52914 = CARTESIAN_POINT ( 'NONE',  ( -89.72076565952676219, -38.51974297931068492, 200.4973812629772851 ) ) ;
#52915 = VERTEX_POINT ( 'NONE', #1914 ) ;
#52916 = CARTESIAN_POINT ( 'NONE',  ( -16.11737681246611942, 21.56249621366126945, -2.179529459285463933 ) ) ;
#52917 = CARTESIAN_POINT ( 'NONE',  ( 16.00000000000008882, 4.197692598229698646, -4.745459346021210223 ) ) ;
#52918 = CARTESIAN_POINT ( 'NONE',  ( -19.34201468796980095, 49.89488280191405778, 61.20624413881779446 ) ) ;
#52919 = CARTESIAN_POINT ( 'NONE',  ( 5.548194972809757708, 40.55407393629103296, -71.04437963701762726 ) ) ;
#52920 = CARTESIAN_POINT ( 'NONE',  ( -32.04928241692800839, 435.9036815552922803, 19.85315484758348248 ) ) ;
#52921 = CARTESIAN_POINT ( 'NONE',  ( -53.08935917470201815, -30.00000000000000000, 52.21147893555080799 ) ) ;
#52922 = CARTESIAN_POINT ( 'NONE',  ( 32.70838245875363270, 434.6727645417001327, 17.17179653056833644 ) ) ;
#52923 = CIRCLE ( 'NONE', #6393, 22.55262289886175964 ) ;
#52924 = CARTESIAN_POINT ( 'NONE',  ( 112.1626836976212189, -59.99999999999999289, 168.5469237518007901 ) ) ;
#52925 = CIRCLE ( 'NONE', #89113, 5.000000000000004441 ) ;
#52926 = CARTESIAN_POINT ( 'NONE',  ( -7.801339272325197527, -68.58731471959700343, -1.788609912539672164 ) ) ;
#52927 = EDGE_LOOP ( 'NONE', ( #43273, #88087, #53349, #51840, #102029 ) ) ;
#52928 = CARTESIAN_POINT ( 'NONE',  ( 35.49824309011672341, 438.0806692989502835, 4.093885194487875800 ) ) ;
#52929 = CARTESIAN_POINT ( 'NONE',  ( -81.07966025770872420, -30.00000000000007816, -11.61909237075606782 ) ) ;
#52930 = VERTEX_POINT ( 'NONE', #36475 ) ;
#52932 = CARTESIAN_POINT ( 'NONE',  ( 5.294781512610923002, 18.76028034990808635, -38.10389976851315907 ) ) ;
#52931 = CARTESIAN_POINT ( 'NONE',  ( -78.99534078293335426, -38.69139673457585360, 190.9623183980413046 ) ) ;
#52933 = CARTESIAN_POINT ( 'NONE',  ( 7.999999999999998224, -21.59374999999999645, 3.313708498984766049 ) ) ;
#52934 = CARTESIAN_POINT ( 'NONE',  ( 5.040301471719072168, 5.750234626350511746, -0.09933465333850823031 ) ) ;
#52935 = DIRECTION ( 'NONE',  ( -0.5735764363510497121, 0.8191520442889892450, 1.003171929053521665E-16 ) ) ;
#52936 = CARTESIAN_POINT ( 'NONE',  ( -5.082755093536325042, -12.96875000204838280, -5.082755093536325930 ) ) ;
#52937 = COLOUR_RGB ( '', 0.40784314, 0.44705882, 0.49803922) ;
#52938 = EDGE_CURVE ( 'NONE', #33104, #7789, #7453, .T. ) ;
#52939 = SURFACE_SIDE_STYLE ('',( #87447 ) ) ;
#52940 = AXIS2_PLACEMENT_3D ( 'NONE', #53502, #12490, #45424 ) ;
#52941 = VERTEX_POINT ( 'NONE', #60203 ) ;
#52942 = CARTESIAN_POINT ( 'NONE',  ( 81.10180942102270762, -56.95487215000356684, 179.5490733622490325 ) ) ;
#52943 = DIRECTION ( 'NONE',  ( 0.000000000000000000, 0.000000000000000000, -1.000000000000000000 ) ) ;
#52944 = PRESENTATION_LAYER_ASSIGNMENT (  '', '', ( #95986 ) ) ;
#52945 = DIRECTION ( 'NONE',  ( 0.000000000000000000, -1.000000000000000000, 0.000000000000000000 ) ) ;
#52946 = VERTEX_POINT ( 'NONE', #94133 ) ;
#52947 = DIRECTION ( 'NONE',  ( 0.000000000000000000, 1.000000000000000000, 0.000000000000000000 ) ) ;
#52948 = FILL_AREA_STYLE_COLOUR ( '', #78584 ) ;
#52949 = PRESENTATION_STYLE_ASSIGNMENT (( #11948 ) ) ;
#52950 = CARTESIAN_POINT ( 'NONE',  ( -29.27049653814488295, 13.57913911089069003, -39.67351191892544193 ) ) ;
#52951 = CARTESIAN_POINT ( 'NONE',  ( 33.00540147335379260, 487.4196752801331627, 9.523982417622169905 ) ) ;
#52952 = CARTESIAN_POINT ( 'NONE',  ( 37.96538461538461462, 1.411358822780289120E-15, 0.000000000000000000 ) ) ;
#52953 = ADVANCED_FACE ( 'NONE', ( #4067 ), #2294, .T. ) ;
#52954 = ORIENTED_EDGE ( 'NONE', *, *, #95578, .F. ) ;
#52955 = PRESENTATION_LAYER_ASSIGNMENT (  '', '', ( #102928 ) ) ;
#52956 = MECHANICAL_DESIGN_GEOMETRIC_PRESENTATION_REPRESENTATION (  '', ( #46042 ), #58108 ) ;
#52957 = CARTESIAN_POINT ( 'NONE',  ( -75.46669749351579526, -30.00000000000000355, -17.70126405444623430 ) ) ;
#52958 = CARTESIAN_POINT ( 'NONE',  ( -1.000000000000000000, -4.607398061199006634, -14.28094137034753608 ) ) ;
#52959 = CARTESIAN_POINT ( 'NONE',  ( 0.000000000000000000, -80.00000000000000000, 39.00000000000000000 ) ) ;
#52961 = LINE ( 'NONE', #13012, #84313 ) ;
#52960 = CARTESIAN_POINT ( 'NONE',  ( 0.000000000000000000, 0.000000000000000000, 0.000000000000000000 ) ) ;
#52962 = CARTESIAN_POINT ( 'NONE',  ( -1.320432766682874540E-15, -25.53125000204838813, 7.188101187500000044 ) ) ;
#52963 = CIRCLE ( 'NONE', #6436, 1.000000000000013989 ) ;
#52964 = AXIS2_PLACEMENT_3D ( 'NONE', #98855, #9851, #83220 ) ;
#52965 = CARTESIAN_POINT ( 'NONE',  ( 1.224646799147353256E-15, 115.0000000000000000, 10.00000000000000000 ) ) ;
#52966 = AXIS2_PLACEMENT_3D ( 'NONE', #85104, #60845, #77007 ) ;
#52967 = CIRCLE ( 'NONE', #56399, 10.00000000000003730 ) ;
#52968 = CARTESIAN_POINT ( 'NONE',  ( 6.145819459792239314, -5.000000000000000000, 7.996135855217247013 ) ) ;
#52969 = EDGE_CURVE ( 'NONE', #92577, #73080, #102874, .T. ) ;
#52970 = CARTESIAN_POINT ( 'NONE',  ( 0.000000000000000000, 67.05096163904791240, -10.02537308446410691 ) ) ;
#52971 = ITEM_DEFINED_TRANSFORMATION ( 'NONE', 'NONE', #28415,  #10728 ) ;
#52972 = EDGE_LOOP ( 'NONE', ( #21463, #33623, #72358, #78436, #49990, #86068 ) ) ;
#52973 = CARTESIAN_POINT ( 'NONE',  ( 1.405425595346621037E-06, -60.00000000000000000, -42.63907915653317104 ) ) ;
#52974 = DIRECTION ( 'NONE',  ( 1.000000000000000000, -0.000000000000000000, -0.000000000000000000 ) ) ;
#52975 = CARTESIAN_POINT ( 'NONE',  ( -9.421434414708310001, 10.25265380211026667, -5.000000000000000000 ) ) ;
#52976 = VECTOR ( 'NONE', #34494, 1000.000000000000000 ) ;
#52977 = EDGE_CURVE ( 'NONE', #94655, #59491, #48807, .T. ) ;
#52978 = B_SPLINE_CURVE_WITH_KNOTS ( 'NONE', 3,
 ( #63640, #26396, #66810, #49005, #41461, #106720 ),
 .UNSPECIFIED., .F., .F.,
 ( 4, 2, 4 ),
 ( 2.380731631042988191E-07, 0.002336973833157630128, 0.004673709593152156581 ),
 .UNSPECIFIED. ) ;
#52979 = VERTEX_POINT ( 'NONE', #12667 ) ;
#52980 = AXIS2_PLACEMENT_3D ( 'NONE', #45427, #29273, #54532 ) ;
#52981 = CARTESIAN_POINT ( 'NONE',  ( 5.656854249492380582, -16.81249999999999289, -5.656854249492379694 ) ) ;
#52982 = CARTESIAN_POINT ( 'NONE',  ( 8.000000000000000000, -21.68750000409676915, 0.000000000000000000 ) ) ;
#52983 = ORIENTED_EDGE ( 'NONE', *, *, #15113, .T. ) ;
#52984 = MANIFOLD_SOLID_BREP ( 'ThdSchPat', #104913 ) ;
#52985 = CARTESIAN_POINT ( 'NONE',  ( -27.10511071441183617, 34.75829513984614039, 7.556984339678626483 ) ) ;
#52986 = CARTESIAN_POINT ( 'NONE',  ( -3.313708498984779371, -22.71875000409676915, -7.999999999999981348 ) ) ;
#52987 = VECTOR ( 'NONE', #59569, 1000.000000000000000 ) ;
#52988 = DIRECTION ( 'NONE',  ( 0.5735764363510466035, -0.8191520442889914655, 1.003171929053524500E-16 ) ) ;
#52989 = SURFACE_SIDE_STYLE ('',( #69188 ) ) ;
#52990 = CARTESIAN_POINT ( 'NONE',  ( -95.46090277292731230, -60.00000000000000711, 202.5799021258702055 ) ) ;
#52991 =( NAMED_UNIT ( * ) PLANE_ANGLE_UNIT ( ) SI_UNIT ( $, .RADIAN. ) );
#52992 = DIRECTION ( 'NONE',  ( 0.000000000000000000, 0.000000000000000000, 1.000000000000000000 ) ) ;
#52993 = CARTESIAN_POINT ( 'NONE',  ( 22.33349330513380337, 1.593028355512270567E-15, 0.000000000000000000 ) ) ;
#52994 =( LENGTH_UNIT ( ) NAMED_UNIT ( * ) SI_UNIT ( .MILLI., .METRE. ) );
#52995 =( GEOMETRIC_REPRESENTATION_CONTEXT ( 3 ) GLOBAL_UNCERTAINTY_ASSIGNED_CONTEXT ( ( #45097 ) ) GLOBAL_UNIT_ASSIGNED_CONTEXT ( ( #23073, #51434, #49295 ) ) REPRESENTATION_CONTEXT ( 'NONE', 'WORKASPACE' ) );
#52996 = CARTESIAN_POINT ( 'NONE',  ( -85.41187482593770142, -28.71929674247896358, 176.9217622319580130 ) ) ;
#52997 = EDGE_CURVE ( 'NONE', #72225, #5970, #95251, .T. ) ;
#52998 = CARTESIAN_POINT ( 'NONE',  ( 39.84006773347349650, 41.92684729384938436, -55.72896217575698330 ) ) ;
#52999 = ORIENTED_EDGE ( 'NONE', *, *, #30573, .T. ) ;
#53000 = CARTESIAN_POINT ( 'NONE',  ( -9.960122430517547087, 45.46309208840077076, -15.36726729605914166 ) ) ;
#53001 = CARTESIAN_POINT ( 'NONE',  ( 0.000000000000000000, 0.000000000000000000, -7.657127082228716297 ) ) ;
#53002 = CARTESIAN_POINT ( 'NONE',  ( -85.09040274407558968, -52.70139051021373433, 5.151369049883602891 ) ) ;
#53003 = CARTESIAN_POINT ( 'NONE',  ( -1.688865360058640741, -5.975540627551688466, -13.79722992719856123 ) ) ;
#53004 = CARTESIAN_POINT ( 'NONE',  ( 8.763392006746210328, 132.4000990056190403, 0.000000000000000000 ) ) ;
#53005 = CYLINDRICAL_SURFACE ( 'NONE', #44199, 4.000000000000000888 ) ;
#53006 = CARTESIAN_POINT ( 'NONE',  ( 37.36680950587120975, 18.64316884708630084, 10.04205104290988437 ) ) ;
#53007 = AXIS2_PLACEMENT_3D ( 'NONE', #9513, #42425, #75318 ) ;
#53008 = CARTESIAN_POINT ( 'NONE',  ( 73.77841798646971938, -29.99999999999998934, 147.9493570314868123 ) ) ;
#53009 = CARTESIAN_POINT ( 'NONE',  ( -89.21407719722087393, -30.00000000000005684, 9.591031914958218607 ) ) ;
#53010 = CARTESIAN_POINT ( 'NONE',  ( -65.24994020922159166, -25.57926860193576601, 79.70707070267074812 ) ) ;
#53011 = EDGE_LOOP ( 'NONE', ( #37709, #49387, #32204, #18642, #13789, #52653, #18669 ) ) ;
#53012 = CARTESIAN_POINT ( 'NONE',  ( 105.6362521817138713, -29.99999999999994671, 194.5266552104434368 ) ) ;
#53013 = CARTESIAN_POINT ( 'NONE',  ( 14.81491239056285991, 40.83920115135541096, 63.35878236462720281 ) ) ;
#53014 = CARTESIAN_POINT ( 'NONE',  ( 63.81996746097805584, -57.67113359436530118, -36.65424566499065406 ) ) ;
#53015 = ORIENTED_EDGE ( 'NONE', *, *, #73268, .T. ) ;
#53016 = CARTESIAN_POINT ( 'NONE',  ( -33.88461414431147745, 464.6055380068506224, 6.798187872896692241 ) ) ;
#53017 = CARTESIAN_POINT ( 'NONE',  ( 5.082755093536325930, -26.84375000204838813, -5.082755093536325042 ) ) ;
#53018 = AXIS2_PLACEMENT_3D ( 'NONE', #14350, #39721, #72073 ) ;
#53019 = CARTESIAN_POINT ( 'NONE',  ( -5.856955515201466511, -6.217109411191364288, 1.326217528971455950 ) ) ;
#53020 = ORIENTED_EDGE ( 'NONE', *, *, #46527, .T. ) ;
#53022 = FACE_OUTER_BOUND ( 'NONE', #4461, .T. ) ;
#53021 = PRESENTATION_LAYER_ASSIGNMENT (  '', '', ( #11666 ) ) ;
#53023 = VERTEX_POINT ( 'NONE', #105408 ) ;
#53024 = CARTESIAN_POINT ( 'NONE',  ( 46.02200000000003399, 0.000000000000000000, 0.000000000000000000 ) ) ;
#53025 = CYLINDRICAL_SURFACE ( 'NONE', #81571, 10.00000000000000178 ) ;
#53026 = CARTESIAN_POINT ( 'NONE',  ( -9.852487725491519299, -60.00000000001466560, 42.00587080741184565 ) ) ;
#53027 = FACE_BOUND ( 'NONE', #75591, .T. ) ;
#53028 = CARTESIAN_POINT ( 'NONE',  ( -2.977408999572650039, -32.56250000204838813, -7.188101187500001821 ) ) ;
#53029 = CARTESIAN_POINT ( 'NONE',  ( -48.15153125426052583, 16.50033784694647920, 14.35535821593516204 ) ) ;
#53030 = EDGE_CURVE ( 'NONE', #45061, #876, #17894, .T. ) ;
#53031 =( BOUNDED_CURVE ( )  B_SPLINE_CURVE ( 2, ( #15413, #24075, #5731 ),
 .UNSPECIFIED., .F., .F. ) 
 B_SPLINE_CURVE_WITH_KNOTS ( ( 3, 3 ),
 ( 0.000000000000000000, 1.000000000000000000 ),
 .UNSPECIFIED. ) 
 CURVE ( )  GEOMETRIC_REPRESENTATION_ITEM ( )  RATIONAL_B_SPLINE_CURVE ( ( 1.000000000000000000, 1.857142857142858317, 1.000000000000000000 ) ) 
 REPRESENTATION_ITEM ( '' )  );
#53032 = CARTESIAN_POINT ( 'NONE',  ( 37.56673239365870387, -1.200000000000000030E-05, 12.20617127780998956 ) ) ;
#53033 = CARTESIAN_POINT ( 'NONE',  ( -1.570796324976843295, 50.00000000000000000, -73.00000000000001421 ) ) ;
#53034 = EDGE_CURVE ( 'NONE', #59650, #34382, #79686, .T. ) ;
#53035 = CARTESIAN_POINT ( 'NONE',  ( -7.934914944860276265, 108.8684564720010997, -1.051261972695692659 ) ) ;
#53036 = CARTESIAN_POINT ( 'NONE',  ( 37.71459991402554124, 437.7716825518408541, 4.505118785440091145 ) ) ;
#53037 = B_SPLINE_CURVE_WITH_KNOTS ( 'NONE', 3,
 ( #44303, #77198, #3310, #77739, #3849, #66993, #83681, #26046, #9787, #12446, #22171, #45374 ),
 .UNSPECIFIED., .F., .F.,
 ( 4, 2, 2, 2, 2, 4 ),
 ( 0.008226835460202822081, 0.01428459443934570333, 0.02034235341848858458, 0.03245787137677434708, 0.04457338933506011652, 0.05668890729334587902 ),
 .UNSPECIFIED. ) ;
#53038 = VERTEX_POINT ( 'NONE', #63908 ) ;
#53039 = CARTESIAN_POINT ( 'NONE',  ( 5.238409285680427629, -1.996984918271484277, 104.1169421774613681 ) ) ;
#53040 = MECHANICAL_DESIGN_GEOMETRIC_PRESENTATION_REPRESENTATION (  '', ( #82362 ), #42717 ) ;
#53041 = CIRCLE ( 'NONE', #23723, 3.309500000000007880 ) ;
#53043 = CARTESIAN_POINT ( 'NONE',  ( 35.24668317487790148, -49.89395819369836715, 37.46068582077064235 ) ) ;
#53042 = CARTESIAN_POINT ( 'NONE',  ( 5.290067270632158980, 51.34639538792298197, -8.531152949374604333 ) ) ;
#53044 = CARTESIAN_POINT ( 'NONE',  ( -24.56594385547200687, -4.285714285715344296, -6.601913983219908744 ) ) ;
#53045 = EDGE_CURVE ( 'NONE', #58831, #70947, #43524, .T. ) ;
#53046 = EDGE_LOOP ( 'NONE', ( #5692, #44422, #93329, #72022 ) ) ;
#53047 = CARTESIAN_POINT ( 'NONE',  ( -21.96336593612924659, 25.92439649894939890, -31.83037853264628225 ) ) ;
#53049 = CARTESIAN_POINT ( 'NONE',  ( -30.95643954367146833, 313.8918926584737505, -7.857037206977866006 ) ) ;
#53048 = CARTESIAN_POINT ( 'NONE',  ( -27.10511071441193565, 34.75829513984539432, -7.556984339685824281 ) ) ;
#53050 = COLOUR_RGB ( '', 0.72549020, 0.75294118, 0.79215686) ;
#53051 = DIRECTION ( 'NONE',  ( 0.000000000000000000, 0.000000000000000000, 1.000000000000000000 ) ) ;
#53052 = CARTESIAN_POINT ( 'NONE',  ( -43.66784424860031066, 484.4037905981319909, 1.818048676808925013 ) ) ;
#53053 = COLOUR_RGB ( '', 0.66274510, 0.83137255, 0.94901961) ;
#53054 = CARTESIAN_POINT ( 'NONE',  ( 6.573529411764729602, 40.00000000373363918, -71.39502911389392636 ) ) ;
#53055 = DIRECTION ( 'NONE',  ( 0.000000000000000000, -1.000000000000000000, 0.000000000000000000 ) ) ;
#53056 = SURFACE_SIDE_STYLE ('',( #45509 ) ) ;
#53057 = VERTEX_POINT ( 'NONE', #96794 ) ;
#53058 = CARTESIAN_POINT ( 'NONE',  ( 92.68096304076409808, -60.00000000000000711, -4.348986201877333535 ) ) ;
#53059 = CARTESIAN_POINT ( 'NONE',  ( 31.08349330513380337, 1.593028355512270567E-15, 0.000000000000000000 ) ) ;
#53060 = CARTESIAN_POINT ( 'NONE',  ( 32.45893998680863746, 464.7013998967805719, 16.05169235330116706 ) ) ;
#53061 = CARTESIAN_POINT ( 'NONE',  ( -36.55581286090212956, 364.8155619110331713, 3.255690858065809934 ) ) ;
#53062 = CARTESIAN_POINT ( 'NONE',  ( -5.207235045403211693, 40.28819020782994187, -70.92786788965571532 ) ) ;
#53063 = LINE ( 'NONE', #29351, #1298 ) ;
#53064 = ORIENTED_EDGE ( 'NONE', *, *, #92084, .F. ) ;
#53065 =( GEOMETRIC_REPRESENTATION_CONTEXT ( 3 ) GLOBAL_UNCERTAINTY_ASSIGNED_CONTEXT ( ( #55962 ) ) GLOBAL_UNIT_ASSIGNED_CONTEXT ( ( #19870, #64020, #88802 ) ) REPRESENTATION_CONTEXT ( 'NONE', 'WORKASPACE' ) );
#53066 = CARTESIAN_POINT ( 'NONE',  ( -94.81618536359641780, -30.00000000002265210, 199.9516214458937782 ) ) ;
#53067 = ORIENTED_EDGE ( 'NONE', *, *, #19213, .F. ) ;
#53068 = FACE_OUTER_BOUND ( 'NONE', #84709, .T. ) ;
#53069 = CARTESIAN_POINT ( 'NONE',  ( 33.07276483573664905, 438.9325140356084489, 23.89537236861388081 ) ) ;
#53070 = CARTESIAN_POINT ( 'NONE',  ( 82.64754189831576525, -37.80179898866133215, -12.22144125512486390 ) ) ;
#53071 = CARTESIAN_POINT ( 'NONE',  ( 2.977408999572651815, -31.81250000204839168, 7.188101187500000933 ) ) ;
#53072 = CARTESIAN_POINT ( 'NONE',  ( -17.39904316874586598, 34.80796549191882150, 21.94102072422699123 ) ) ;
#53073 = CARTESIAN_POINT ( 'NONE',  ( 0.000000000000000000, 1.000000000000000888, 0.000000000000000000 ) ) ;
#53074 = ORIENTED_EDGE ( 'NONE', *, *, #98376, .F. ) ;
#53075 = CARTESIAN_POINT ( 'NONE',  ( 89.93133926947346879, 6.123233995736582872E-16, -5.000000000000011546 ) ) ;
#53076 = ORIENTED_EDGE ( 'NONE', *, *, #71202, .F. ) ;
#53077 = EDGE_CURVE ( 'NONE', #34913, #100497, #7532, .T. ) ;
#53078 = CARTESIAN_POINT ( 'NONE',  ( 48.55208739724518807, 8.680497950467705337, -16.74317141725391878 ) ) ;
#53079 = AXIS2_PLACEMENT_3D ( 'NONE', #21507, #72150, #79177 ) ;
#53081 = EDGE_LOOP ( 'NONE', ( #9603, #41973 ) ) ;
#53080 = DIRECTION ( 'NONE',  ( -0.5735764363510494901, -0.8191520442889894671, 0.000000000000000000 ) ) ;
#53082 = CARTESIAN_POINT ( 'NONE',  ( 81.81383369307825149, -25.62393137265173237, 141.9806983117227048 ) ) ;
#53083 = ADVANCED_FACE ( 'NONE', ( #5647 ), #76216, .T. ) ;
#53084 = ORIENTED_EDGE ( 'NONE', *, *, #70607, .F. ) ;
#53085 = CARTESIAN_POINT ( 'NONE',  ( 2.992324825358647189, -53.48068721642265899, 40.67781845958850084 ) ) ;
#53086 = CARTESIAN_POINT ( 'NONE',  ( -2.977408999572650039, -17.18750000204838813, -7.188101187500000933 ) ) ;
#53087 = CARTESIAN_POINT ( 'NONE',  ( -89.37884834614470719, -57.60609784898206698, 203.8391154356046115 ) ) ;
#53088 = EDGE_CURVE ( 'NONE', #15159, #10424, #34927, .T. ) ;
#53089 = ORIENTED_EDGE ( 'NONE', *, *, #53175, .F. ) ;
#53090 =( LENGTH_UNIT ( ) NAMED_UNIT ( * ) SI_UNIT ( .MILLI., .METRE. ) );
#53091 = FACE_OUTER_BOUND ( 'NONE', #64718, .T. ) ;
#53092 = MECHANICAL_DESIGN_GEOMETRIC_PRESENTATION_REPRESENTATION (  '', ( #42759 ), #44558 ) ;
#53093 = CARTESIAN_POINT ( 'NONE',  ( -10.00004721872059577, 80.99988195318846351, -0.2617599822266473142 ) ) ;
#53094 = CARTESIAN_POINT ( 'NONE',  ( 49.27914886956165930, 13.08292563505449024, -15.56788460764872717 ) ) ;
#53095 = CARTESIAN_POINT ( 'NONE',  ( -8.000000000000000000, -19.53125000409677980, -3.313708498984762496 ) ) ;
#53096 = CARTESIAN_POINT ( 'NONE',  ( -46.94109106579729485, -28.93092366380357205, 42.27278928388007984 ) ) ;
#53097 = DIRECTION ( 'NONE',  ( 0.000000000000000000, -1.000000000000000000, 0.000000000000000000 ) ) ;
#53098 = COLOUR_RGB ( '', 0.66274510, 0.83137255, 0.94901961) ;
#53099 = CARTESIAN_POINT ( 'NONE',  ( -9.333892298909264085, 86.78275731625036826, -3.590295303293451923 ) ) ;
#53100 = FACE_OUTER_BOUND ( 'NONE', #47540, .T. ) ;
#53101 = APPLICATION_PROTOCOL_DEFINITION ( 'draft international standard', 'automotive_design', 1998, #100339 ) ;
#53102 = DIRECTION ( 'NONE',  ( -1.000000000000000000, -0.000000000000000000, -0.000000000000000000 ) ) ;
#53103 = ORIENTED_EDGE ( 'NONE', *, *, #35845, .F. ) ;
#53104 = CARTESIAN_POINT ( 'NONE',  ( -5.459621313820996136, -51.29419033140447226, 39.89514185836628712 ) ) ;
#53105 = FACE_OUTER_BOUND ( 'NONE', #43247, .T. ) ;
#53106 = DIRECTION ( 'NONE',  ( -0.8191520442889884679, 1.003171929053520679E-16, 0.5735764363510509334 ) ) ;
#53107 = CARTESIAN_POINT ( 'NONE',  ( -52.88890906521714186, -28.13393072479325951, -27.22359359308505589 ) ) ;
#53108 = CARTESIAN_POINT ( 'NONE',  ( -62.53308941777711993, -30.00000000000000000, 73.43786462750344413 ) ) ;
#53109 = EDGE_CURVE ( 'NONE', #102808, #29354, #21340, .T. ) ;
#53110 = B_SPLINE_CURVE_WITH_KNOTS ( 'NONE', 3,
 ( #61703, #68722, #27760, #102664, #69772, #2358, #36384, #93521, #86512 ),
 .UNSPECIFIED., .F., .F.,
 ( 4, 2, 1, 2, 4 ),
 ( 0.000000000000000000, 0.002165063509461097498, 0.004330127018922194995, 0.006495190528383292493, 0.008660254037844389990 ),
 .UNSPECIFIED. ) ;
#53111 = EDGE_LOOP ( 'NONE', ( #5419, #56354, #32313, #63005 ) ) ;
#53112 = AXIS2_PLACEMENT_3D ( 'NONE', #71992, #104904, #96810 ) ;
#53113 = DIRECTION ( 'NONE',  ( 0.000000000000000000, 0.000000000000000000, 1.000000000000000000 ) ) ;
#53114 = AXIS2_PLACEMENT_3D ( 'NONE', #57907, #56848, #22933 ) ;
#53115 = CARTESIAN_POINT ( 'NONE',  ( 74.64417150186339711, -57.58847707714879505, 189.5392262892293616 ) ) ;
#53116 = CIRCLE ( 'NONE', #51327, 5.000000000000001776 ) ;
#53117 = CARTESIAN_POINT ( 'NONE',  ( 46.00000000000000000, 438.0646818832677809, 14.80758164884668560 ) ) ;
#53118 = EDGE_CURVE ( 'NONE', #23867, #1766, #15370, .T. ) ;
#53119 = CIRCLE ( 'NONE', #48168, 3.000000000000000000 ) ;
#53120 = CARTESIAN_POINT ( 'NONE',  ( 28.87846294582190509, -29.15946654300748975, -38.22760178079393967 ) ) ;
#53121 = FILL_AREA_STYLE_COLOUR ( '', #5341 ) ;
#53122 = CARTESIAN_POINT ( 'NONE',  ( 10.59999999999999609, -3.309499999999999886, 0.000000000000000000 ) ) ;
#53123 = CARTESIAN_POINT ( 'NONE',  ( -57.21714066519500363, -60.00000000000000711, 91.78310137730963447 ) ) ;
#53124 = CONICAL_SURFACE ( 'NONE', #73743, 4.000000000000007105, 0.9599310885968835860 ) ;
#53125 = CARTESIAN_POINT ( 'NONE',  ( -6.878751942472531411, 3.924677726130911815, -6.573129608219088205 ) ) ;
#53126 = CARTESIAN_POINT ( 'NONE',  ( 63.03617022296134564, 48.00000000000000000, -16.93907820452146851 ) ) ;
#53127 = CARTESIAN_POINT ( 'NONE',  ( -86.23427538531471725, -28.26129243476134079, 183.4415589754995892 ) ) ;
#53128 = ORIENTED_EDGE ( 'NONE', *, *, #35573, .T. ) ;
#53129 = CARTESIAN_POINT ( 'NONE',  ( 10.59999999999999609, -3.309499999999999886, 4.475777889183790779E-16 ) ) ;
#53130 = CARTESIAN_POINT ( 'NONE',  ( -2.989696676026662558, -25.54936876401580292, 28.14337665864941229 ) ) ;
#53131 = CARTESIAN_POINT ( 'NONE',  ( -6.913779242700421435, 41.73441082398074542, -59.30275289623196500 ) ) ;
#53132 = LINE ( 'NONE', #86049, #28851 ) ;
#53133 = CARTESIAN_POINT ( 'NONE',  ( -8.239589396826303869, 54.07616056299237073, 1.561881609672474136 ) ) ;
#53134 = VERTEX_POINT ( 'NONE', #74086 ) ;
#53135 = CARTESIAN_POINT ( 'NONE',  ( 7.500000000000007105, -3.000000000000000000, -68.91429205785459544 ) ) ;
#53136 = CARTESIAN_POINT ( 'NONE',  ( 10.59999999999999609, 3.309500000000003439, 4.052968581778167743E-16 ) ) ;
#53137 = MECHANICAL_DESIGN_GEOMETRIC_PRESENTATION_REPRESENTATION (  '', ( #1447 ), #11844 ) ;
#53138 = CARTESIAN_POINT ( 'NONE',  ( 6.162888688655350222, -7.505553499465148271, 0.000000000000000000 ) ) ;
#53139 = PLANE ( 'NONE',  #84360 ) ;
#53140 = ORIENTED_EDGE ( 'NONE', *, *, #97311, .T. ) ;
#53141 = CARTESIAN_POINT ( 'NONE',  ( 17.66271159654818845, 50.00000000000000711, 62.46904644769021075 ) ) ;
#53142 = CARTESIAN_POINT ( 'NONE',  ( 36.91281931599076671, 303.7809130842520631, -7.959270006439831846 ) ) ;
#53144 = CARTESIAN_POINT ( 'NONE',  ( -5.820808985953483727, -9.668376379147026354E-13, -21.65942590380073085 ) ) ;
#53143 = B_SPLINE_CURVE_WITH_KNOTS ( 'NONE', 3,
 ( #79814, #72257, #8041, #72771, #25330, #976, #105677, #48494, #83006, #58746, #42009, #49024, #64700, #74366, #99720, #49568, #32357, #91641, #98121, #17229, #89511, #31815 ),
 .UNSPECIFIED., .F., .F.,
 ( 4, 2, 2, 2, 2, 2, 2, 2, 2, 2, 4 ),
 ( 0.007084402336705432693, 0.007336525902261045382, 0.007588649467816658070, 0.008092896598927895591, 0.008345020164483511749, 0.008597143730039126172, 0.009101390861150355019, 0.009605637992261582131, 0.01010988512337281098, 0.01061413225448403982, 0.01111837938559526694 ),
 .UNSPECIFIED. ) ;
#53145 = AXIS2_PLACEMENT_3D ( 'NONE', #38214, #106083, #47323 ) ;
#53146 = CARTESIAN_POINT ( 'NONE',  ( -34.84618260875176787, 489.9833681528637044, 11.97975507378787619 ) ) ;
#53147 =( GEOMETRIC_REPRESENTATION_CONTEXT ( 3 ) GLOBAL_UNCERTAINTY_ASSIGNED_CONTEXT ( ( #99086 ) ) GLOBAL_UNIT_ASSIGNED_CONTEXT ( ( #9638, #46158, #13762 ) ) REPRESENTATION_CONTEXT ( 'NONE', 'WORKASPACE' ) );
#53148 = CARTESIAN_POINT ( 'NONE',  ( 94.62301060094824834, -14.21045842199438525, 80.84833697736402769 ) ) ;
#53149 = CARTESIAN_POINT ( 'NONE',  ( -80.10456516755152734, -46.43972398824795533, 154.7502001011243351 ) ) ;
#53150 = ORIENTED_EDGE ( 'NONE', *, *, #8152, .F. ) ;
#53151 = FACE_OUTER_BOUND ( 'NONE', #41567, .T. ) ;
#53152 = CARTESIAN_POINT ( 'NONE',  ( 0.000000000000000000, 0.000000000000000000, -60.00000000000000000 ) ) ;
#53153 = CARTESIAN_POINT ( 'NONE',  ( 36.72327209579803764, -57.69637131458309653, 51.04913384944509147 ) ) ;
#53154 = CARTESIAN_POINT ( 'NONE',  ( -3.601054696133250315E-15, 5.788408252967898626, 2.974182810908597929 ) ) ;
#53156 = CIRCLE ( 'NONE', #3183, 13.50000000000000000 ) ;
#53155 = CARTESIAN_POINT ( 'NONE',  ( 45.29236137015085006, 362.1850291255836396, 4.988315089120307633 ) ) ;
#53157 = CARTESIAN_POINT ( 'NONE',  ( 43.71999369284589676, 463.9422086738373991, 7.488562083390279511 ) ) ;
#53158 = ORIENTED_EDGE ( 'NONE', *, *, #86406, .T. ) ;
#53159 = CARTESIAN_POINT ( 'NONE',  ( 4.063874237994596683, 54.18639730106497865, -6.988267930799597849 ) ) ;
#53160 = CARTESIAN_POINT ( 'NONE',  ( 31.35397047751884614, 438.7442028766091653, 22.94603175516938265 ) ) ;
#53161 = CARTESIAN_POINT ( 'NONE',  ( -2.977408999572654480, -27.12500000204838457, 7.188101187499999156 ) ) ;
#53162 = ORIENTED_EDGE ( 'NONE', *, *, #93261, .T. ) ;
#53163 = CARTESIAN_POINT ( 'NONE',  ( -7.500000000000000888, 0.000000000000000000, 1.734723475976807094E-15 ) ) ;
#53164 = CARTESIAN_POINT ( 'NONE',  ( 5.465597732043399049, 41.93635053422439540, -70.00903522191315176 ) ) ;
#53165 = EDGE_CURVE ( 'NONE', #12223, #43916, #26542, .T. ) ;
#53166 = CARTESIAN_POINT ( 'NONE',  ( 26.78649824955473235, 36.71831459666817210, 10.02601051567788204 ) ) ;
#53167 = CARTESIAN_POINT ( 'NONE',  ( 2.349637580323456376, -6.873737774778126308, -13.34209367997882900 ) ) ;
#53169 = CARTESIAN_POINT ( 'NONE',  ( 0.000000000000000000, 0.000000000000000000, -2.296599999999999753 ) ) ;
#53168 = VECTOR ( 'NONE', #77125, 999.9999999999998863 ) ;
#53170 = VERTEX_POINT ( 'NONE', #172 ) ;
#53171 = CARTESIAN_POINT ( 'NONE',  ( 80.53725183873906701, -60.00000000000002132, -27.62580428353563633 ) ) ;
#53173 = CARTESIAN_POINT ( 'NONE',  ( 23.01660328067156769, -18.59970856359895564, 27.84350729933087365 ) ) ;
#53172 = CARTESIAN_POINT ( 'NONE',  ( -35.98784834194372451, -29.99999999999998934, 43.73664282352994803 ) ) ;
#53174 = FACE_OUTER_BOUND ( 'NONE', #76791, .T. ) ;
#53175 = EDGE_CURVE ( 'NONE', #76534, #77405, #40138, .T. ) ;
#53176 = CLOSED_SHELL ( 'NONE', ( #55887, #61803, #20554, #99188, #21598, #19597, #41411, #73760, #22353, #28353 ) ) ;
#53177 = CARTESIAN_POINT ( 'NONE',  ( -38.28055269113645664, -42.97469174897878474, 38.10477465472399672 ) ) ;
#53178 = EDGE_LOOP ( 'NONE', ( #75746, #92270, #43976, #79590, #101053 ) ) ;
#53179 = CARTESIAN_POINT ( 'NONE',  ( 34.40200853651277413, 463.9211969149139918, 5.556884403146712614 ) ) ;
#53180 = DIRECTION ( 'NONE',  ( 0.000000000000000000, 1.000000000000000000, 0.000000000000000000 ) ) ;
#53181 = CARTESIAN_POINT ( 'NONE',  ( -13.60715398569422874, -56.44111117512002096, 30.29660545413128503 ) ) ;
#53182 = VECTOR ( 'NONE', #40805, 1000.000000000000000 ) ;
#53183 = CARTESIAN_POINT ( 'NONE',  ( -33.49615637169856086, 465.2403011571850584, 8.307633084691179448 ) ) ;
#53184 = CARTESIAN_POINT ( 'NONE',  ( 29.68315524077033629, 13.47185074185905584, 42.10535821593451544 ) ) ;
#53185 = CARTESIAN_POINT ( 'NONE',  ( 12.15800707188965113, -2.467988851150757057, 20.68556527105151943 ) ) ;
#53186 = ORIENTED_EDGE ( 'NONE', *, *, #100644, .T. ) ;
#53187 = CARTESIAN_POINT ( 'NONE',  ( -75.99682948615210876, -38.37765750765254325, 178.3306665773977500 ) ) ;
#53188 = AXIS2_PLACEMENT_3D ( 'NONE', #5090, #12627, #78432 ) ;
#53189 = CARTESIAN_POINT ( 'NONE',  ( 97.53565773566364783, -30.00000000000016698, 190.8694968829258301 ) ) ;
#53190 = CARTESIAN_POINT ( 'NONE',  ( -11.53828704146876660, 7.329576385473249189, -9.371820186362002758 ) ) ;
#53191 = CARTESIAN_POINT ( 'NONE',  ( 2.797224791467302740, 15.83450757143047305, 9.607634652978001455 ) ) ;
#53192 = CARTESIAN_POINT ( 'NONE',  ( 80.74124341164603891, -30.00000000000000355, -12.54865364685866247 ) ) ;
#53193 = LINE ( 'NONE', #71477, #88088 ) ;
#53194 = ORIENTED_EDGE ( 'NONE', *, *, #20351, .T. ) ;
#53195 = B_SPLINE_CURVE_WITH_KNOTS ( 'NONE', 3,
 ( #60194, #52056, #34856, #68805, #34326, #100078, #11056, #10535, #18126, #84442, #35390, #67724, #60714, #93600, #100610, #50982, #83895, #19752, #42916, #75807, #26771, #1903 ),
 .UNSPECIFIED., .F., .F.,
 ( 4, 2, 2, 2, 2, 2, 2, 2, 2, 2, 4 ),
 ( 0.003192110316504342005, 0.003444089597595979216, 0.003696068878687615994, 0.004200027440870891283, 0.004703986003054166573, 0.005207944565237442730, 0.006215861689604012391, 0.006467840970695656541, 0.006719820251787300691, 0.006971799532878944841, 0.007223778813970588991 ),
 .UNSPECIFIED. ) ;
#53196 = ORIENTED_EDGE ( 'NONE', *, *, #13466, .T. ) ;
#53197 = ORIENTED_EDGE ( 'NONE', *, *, #29125, .T. ) ;
#53198 = CARTESIAN_POINT ( 'NONE',  ( 5.299999999999999822, 7.505553499465139389, -6.505213034913023646E-16 ) ) ;
#53199 = CARTESIAN_POINT ( 'NONE',  ( 8.377077475354079672E-17, 56.87938524157181774, 0.6840402866513453084 ) ) ;
#53200 = CIRCLE ( 'NONE', #85927, 7.500000000000006217 ) ;
#53201 = DIRECTION ( 'NONE',  ( -0.000000000000000000, 1.000000000000000000, -0.000000000000000000 ) ) ;
#53202 = CARTESIAN_POINT ( 'NONE',  ( 6.045898094491907848, 53.95739701478677119, 6.272836224203895306 ) ) ;
#53203 = CARTESIAN_POINT ( 'NONE',  ( 0.000000000000000000, -5.629165124598843661, 3.250000000000011990 ) ) ;
#53204 = ORIENTED_EDGE ( 'NONE', *, *, #35567, .T. ) ;
#53205 = CARTESIAN_POINT ( 'NONE',  ( -6.145467200818548470, 49.99999999999999289, -77.00333157709850695 ) ) ;
#53206 = VERTEX_POINT ( 'NONE', #33135 ) ;
#53207 = CARTESIAN_POINT ( 'NONE',  ( -5.383284837158154090, -61.99950656484222122, 2.657356347551696807 ) ) ;
#53208 = CARTESIAN_POINT ( 'NONE',  ( 37.88504238421471371, 464.3115779013475048, 20.35635421821805480 ) ) ;
#53209 = CARTESIAN_POINT ( 'NONE',  ( 31.84999999999999787, 1.533819458162526451E-15, 0.000000000000000000 ) ) ;
#53210 = CARTESIAN_POINT ( 'NONE',  ( 29.45187729973999069, 297.5878244927288279, 2.537403480031316771 ) ) ;
#53211 = AXIS2_PLACEMENT_3D ( 'NONE', #91176, #7557, #90626 ) ;
#53212 = CARTESIAN_POINT ( 'NONE',  ( 7.188569307834695721, 302.2771564544925695, -10.02656284648950624 ) ) ;
#53213 = CARTESIAN_POINT ( 'NONE',  ( 64.03239688625770043, -39.48186605976993491, 83.36271444441133838 ) ) ;
#53214 = ORIENTED_EDGE ( 'NONE', *, *, #86807, .T. ) ;
#53215 = LINE ( 'NONE', #27923, #82284 ) ;
#53216 = DIRECTION ( 'NONE',  ( 0.000000000000000000, -1.000000000000000000, 0.000000000000000000 ) ) ;
#53217 = DIRECTION ( 'NONE',  ( -0.9861333108787085910, 0.1659550938519105401, 0.000000000000000000 ) ) ;
#53218 = CARTESIAN_POINT ( 'NONE',  ( 43.00000000000000000, 435.7055874969797742, 20.39059140826877226 ) ) ;
#53219 = EDGE_CURVE ( 'NONE', #24036, #6482, #95183, .T. ) ;
#53220 = ORIENTED_EDGE ( 'NONE', *, *, #97880, .T. ) ;
#53221 = COLOUR_RGB ( '', 0.66274510, 0.83137255, 0.94901961) ;
#53222 = CARTESIAN_POINT ( 'NONE',  ( 0.000000000000000000, 0.000000000000000000, 0.000000000000000000 ) ) ;
#53223 = PRESENTATION_STYLE_ASSIGNMENT (( #3068 ) ) ;
#53224 = FILL_AREA_STYLE ('',( #61329 ) ) ;
#53225 = AXIS2_PLACEMENT_3D ( 'NONE', #91056, #43022, #17164 ) ;
#53226 = AXIS2_PLACEMENT_3D ( 'NONE', #40833, #18175, #66168 ) ;
#53227 = AXIS2_PLACEMENT_3D ( 'NONE', #51499, #50955, #52558 ) ;
#53228 = CARTESIAN_POINT ( 'NONE',  ( 8.000000000000000000, -33.59375000409677625, -3.313708498984761608 ) ) ;
#53229 = FACE_OUTER_BOUND ( 'NONE', #38060, .T. ) ;
#53230 = CARTESIAN_POINT ( 'NONE',  ( 86.09253067001675674, -31.93605399604700068, 184.2217672492984377 ) ) ;
#53231 = AXIS2_PLACEMENT_3D ( 'NONE', #67747, #44003, #76888 ) ;
#53232 = CARTESIAN_POINT ( 'NONE',  ( 32.81992448453895150, 465.7192846569213316, 11.17271167765130890 ) ) ;
#53233 = CARTESIAN_POINT ( 'NONE',  ( -8.623093486246707684, 129.1228760232886259, 6.361996342910116291E-13 ) ) ;
#53234 = ORIENTED_EDGE ( 'NONE', *, *, #73121, .F. ) ;
#53235 = FACE_OUTER_BOUND ( 'NONE', #69613, .T. ) ;
#53236 = CARTESIAN_POINT ( 'NONE',  ( 5.296018678377662603, -15.62506502678866127, -35.11036406914151797 ) ) ;
#53237 = CARTESIAN_POINT ( 'NONE',  ( 13.45079846400083312, -54.00000000000000711, 23.11721482942554928 ) ) ;
#53238 = CARTESIAN_POINT ( 'NONE',  ( 34.42490260133396873, 435.3680287947617558, 9.712724143469429805 ) ) ;
#53239 = CARTESIAN_POINT ( 'NONE',  ( -83.59878907863057407, -30.00000000000000355, 47.68203053101536426 ) ) ;
#53240 = EDGE_CURVE ( 'NONE', #42388, #10713, #10762, .T. ) ;
#53241 = AXIS2_PLACEMENT_3D ( 'NONE', #60186, #25709, #100071 ) ;
#53242 = FACE_OUTER_BOUND ( 'NONE', #103351, .T. ) ;
#53243 = CARTESIAN_POINT ( 'NONE',  ( 29.78108665591588888, -57.68312184062244086, 45.10668838524471624 ) ) ;
#53244 = STYLED_ITEM ( 'NONE', ( #70779 ), #185 ) ;
#53246 = CARTESIAN_POINT ( 'NONE',  ( 9.797174393178825657E-16, -30.00000000000000000, -8.000000000000000000 ) ) ;
#53245 = CARTESIAN_POINT ( 'NONE',  ( 9.295649250257604024, 43.59667780448855723, 14.93671105746132710 ) ) ;
#53247 = EDGE_CURVE ( 'NONE', #28968, #101925, #71917, .T. ) ;
#53248 = SURFACE_SIDE_STYLE ('',( #75916 ) ) ;
#53249 = CARTESIAN_POINT ( 'NONE',  ( -48.49798649753537916, -37.71222160853894678, 47.78134261254622572 ) ) ;
#53250 = CARTESIAN_POINT ( 'NONE',  ( -18.83156529568702808, 50.00000000000000000, 60.81392993381482626 ) ) ;
#53251 = CARTESIAN_POINT ( 'NONE',  ( 18.91791044776121211, 45.00000000000000711, 62.18611311450882795 ) ) ;
#53252 = CARTESIAN_POINT ( 'NONE',  ( 45.99999999999999289, 486.8231468695055923, 5.689692765235318639 ) ) ;
#53253 = CARTESIAN_POINT ( 'NONE',  ( 49.23114114914121586, -27.31787067993425211, -28.17124660505862010 ) ) ;
#53254 = CONICAL_SURFACE ( 'NONE', #75640, 3.309500000000001663, 0.9599310885968770357 ) ;
#53255 = CARTESIAN_POINT ( 'NONE',  ( -23.01798323853113004, -18.59969654692860530, 27.84368168669262644 ) ) ;
#53256 = EDGE_CURVE ( 'NONE', #37041, #38119, #57270, .T. ) ;
#53257 = ORIENTED_EDGE ( 'NONE', *, *, #8993, .F. ) ;
#53258 = DIRECTION ( 'NONE',  ( 0.000000000000000000, 0.000000000000000000, 1.000000000000000000 ) ) ;
#53259 = CARTESIAN_POINT ( 'NONE',  ( -19.25491102509279528, -49.92033008237394398, 32.66346180105560393 ) ) ;
#53261 = DIRECTION ( 'NONE',  ( -0.8191520442889974607, 0.000000000000000000, -0.5735764363510379438 ) ) ;
#53260 = CARTESIAN_POINT ( 'NONE',  ( -1.011534475481120854, 28.02053069269880226, 38.74788564449888639 ) ) ;
#53262 = ORIENTED_EDGE ( 'NONE', *, *, #100548, .F. ) ;
#53263 = CARTESIAN_POINT ( 'NONE',  ( 14.44581512914855459, 5.963299184997036484, -7.135127315211338583 ) ) ;
#53264 = ORIENTED_EDGE ( 'NONE', *, *, #87288, .T. ) ;
#53265 = SURFACE_SIDE_STYLE ('',( #10136 ) ) ;
#53266 = AXIS2_PLACEMENT_3D ( 'NONE', #78542, #70986, #53740 ) ;
#53267 = CARTESIAN_POINT ( 'NONE',  ( 15.20015366321729466, 3.406002745425039890, -3.875710626021652949 ) ) ;
#53268 = CARTESIAN_POINT ( 'NONE',  ( 0.000000000000000000, 0.000000000000000000, 5.000000000000002665 ) ) ;
#53269 = ORIENTED_EDGE ( 'NONE', *, *, #44034, .F. ) ;
#53270 = SURFACE_STYLE_FILL_AREA ( #4720 ) ;
#53271 = AXIS2_PLACEMENT_3D ( 'NONE', #6258, #14883, #47776 ) ;
#53272 = CARTESIAN_POINT ( 'NONE',  ( 101.9973258343542426, -45.28264241616768970, 189.2080144842875598 ) ) ;
#53273 = PRESENTATION_LAYER_ASSIGNMENT (  '', '', ( #72207 ) ) ;
#53275 = DIRECTION ( 'NONE',  ( -1.000000000000000000, 0.000000000000000000, 0.000000000000000000 ) ) ;
#53274 = DIRECTION ( 'NONE',  ( -1.000000000000000000, -0.000000000000000000, -0.000000000000000000 ) ) ;
#53276 = ORIENTED_EDGE ( 'NONE', *, *, #70438, .T. ) ;
#53277 = ORIENTED_EDGE ( 'NONE', *, *, #51918, .F. ) ;
#53278 = VERTEX_POINT ( 'NONE', #49274 ) ;
#53279 = CARTESIAN_POINT ( 'NONE',  ( 26.01244650717567453, 309.4037012981271459, 11.00800451746652975 ) ) ;
#53280 = CARTESIAN_POINT ( 'NONE',  ( 4.898587196589412829E-16, -19.62499999999999289, -8.000000000000000000 ) ) ;
#53281 = FILL_AREA_STYLE_COLOUR ( '', #5423 ) ;
#53282 = ORIENTED_EDGE ( 'NONE', *, *, #90654, .T. ) ;
#53283 = ADVANCED_FACE ( 'NONE', ( #91361 ), #12372, .T. ) ;
#53284 = CARTESIAN_POINT ( 'NONE',  ( 22.61650669486618526, 1.474610560812782335E-15, 0.000000000000000000 ) ) ;
#53285 = CARTESIAN_POINT ( 'NONE',  ( -7.748892321275496542, 5.864906519858121392, -4.492850722662553586 ) ) ;
#53286 = CONICAL_SURFACE ( 'NONE', #80908, 4.000000000000001776, 0.9599310885968774798 ) ;
#53287 = CARTESIAN_POINT ( 'NONE',  ( -94.27213507841179307, -59.99999999999998579, 8.085468415347424553 ) ) ;
#53288 = DIRECTION ( 'NONE',  ( 0.000000000000000000, 1.000000000000000000, 0.000000000000000000 ) ) ;
#53289 = CARTESIAN_POINT ( 'NONE',  ( 28.14493782455200943, -59.99999999999997868, 42.15984703162648373 ) ) ;
#53290 = CARTESIAN_POINT ( 'NONE',  ( 14.68325236364846198, -5.000000000000000000, -7.358060591975124076 ) ) ;
#53291 = CARTESIAN_POINT ( 'NONE',  ( -6.453255531754163776, 41.48539074419475980, -58.52372506869146918 ) ) ;
#53293 = CARTESIAN_POINT ( 'NONE',  ( 5.086408192983678411, -42.95350893056307484, 31.03852461352498793 ) ) ;
#53292 = CARTESIAN_POINT ( 'NONE',  ( -95.99503958615204624, -14.21045842199434794, 88.91558689677049188 ) ) ;
#53294 = EDGE_CURVE ( 'NONE', #90391, #30344, #86085, .T. ) ;
#53296 = EDGE_CURVE ( 'NONE', #29639, #45973, #23036, .T. ) ;
#53295 = DIRECTION ( 'NONE',  ( 0.5735764363510491570, -0.8191520442889895781, 1.003171929053522035E-16 ) ) ;
#53297 = CARTESIAN_POINT ( 'NONE',  ( -48.89129092203405946, -22.21415037853287089, 43.54257904152331804 ) ) ;
#53298 = EDGE_LOOP ( 'NONE', ( #12329, #40246, #72977, #60482, #33386 ) ) ;
#53299 = CARTESIAN_POINT ( 'NONE',  ( 4.424150818701950705, -68.80753671330023735, 13.71457674299446694 ) ) ;
#53300 = ORIENTED_EDGE ( 'NONE', *, *, #5283, .T. ) ;
#53301 = DIRECTION ( 'NONE',  ( 0.000000000000000000, -1.000000000000000000, 0.000000000000000000 ) ) ;
#53302 = CARTESIAN_POINT ( 'NONE',  ( 17.53793833829814375, 36.29671191971048927, 24.04345926538296396 ) ) ;
#53303 = ADVANCED_FACE ( 'NONE', ( #8166 ), #53815, .T. ) ;
#53304 = CARTESIAN_POINT ( 'NONE',  ( 5.999511540169428336, -6.000732691145679532, -0.2833228702578348135 ) ) ;
#53305 = VERTEX_POINT ( 'NONE', #36219 ) ;
#53306 = CARTESIAN_POINT ( 'NONE',  ( -8.237488943525885787, -5.130131229380902269, 14.25442149443525786 ) ) ;
#53307 = ORIENTED_EDGE ( 'NONE', *, *, #48632, .F. ) ;
#53308 = CARTESIAN_POINT ( 'NONE',  ( 107.3415078906099041, -30.00000000001339728, 143.3259930713776384 ) ) ;
#53309 = FILL_AREA_STYLE_COLOUR ( '', #35377 ) ;
#53310 = CARTESIAN_POINT ( 'NONE',  ( -2.103213117735936333, -7.611216007246521364, -13.05636887007053026 ) ) ;
#53311 = CARTESIAN_POINT ( 'NONE',  ( -7.754160006593189713, 42.00000000000000711, 59.23741894013591036 ) ) ;
#53312 = CARTESIAN_POINT ( 'NONE',  ( 98.44576339691531075, -30.00000000000000000, 189.9304428966003684 ) ) ;
#53313 = CARTESIAN_POINT ( 'NONE',  ( -0.7774258472507343809, 36.39397619591250788, 29.48229727820018553 ) ) ;
#53314 = VERTEX_POINT ( 'NONE', #2729 ) ;
#53315 = EDGE_CURVE ( 'NONE', #6418, #653, #92808, .T. ) ;
#53316 = CIRCLE ( 'NONE', #87738, 5.000000000000011546 ) ;
#53317 = ORIENTED_EDGE ( 'NONE', *, *, #82466, .T. ) ;
#53318 = ORIENTED_EDGE ( 'NONE', *, *, #57290, .F. ) ;
#53319 = CARTESIAN_POINT ( 'NONE',  ( 55.06520104054218478, -22.15438351385262550, 53.58026775065899727 ) ) ;
#53320 = CARTESIAN_POINT ( 'NONE',  ( 43.74985542820358830, 435.5770091380369990, 16.96136490515564077 ) ) ;
#53321 = CARTESIAN_POINT ( 'NONE',  ( -7.500000000000007105, 42.00000000000000711, -62.89165061483231511 ) ) ;
#53322 = EDGE_CURVE ( 'NONE', #37979, #47288, #5623, .T. ) ;
#53323 = ORIENTED_EDGE ( 'NONE', *, *, #6584, .T. ) ;
#53324 = CARTESIAN_POINT ( 'NONE',  ( -88.05788157026037766, -38.37130978355936151, -19.49573130021213174 ) ) ;
#53325 = AXIS2_PLACEMENT_3D ( 'NONE', #37414, #6049, #54060 ) ;
#53326 = ORIENTED_EDGE ( 'NONE', *, *, #98199, .T. ) ;
#53327 = SURFACE_STYLE_FILL_AREA ( #68990 ) ;
#53328 = CARTESIAN_POINT ( 'NONE',  ( 105.4234212887860593, -38.38633086054609578, 197.0379193257338386 ) ) ;
#53329 = CARTESIAN_POINT ( 'NONE',  ( 11.52612706373040119, 20.62001236652582747, 7.987291842674246745 ) ) ;
#53330 = CARTESIAN_POINT ( 'NONE',  ( 82.43424158715217231, -37.85663943339775273, 13.21557699368458749 ) ) ;
#53331 = CARTESIAN_POINT ( 'NONE',  ( 42.76923532591476373, 409.3122222668040990, 19.95929303662902754 ) ) ;
#53332 = CARTESIAN_POINT ( 'NONE',  ( 0.000000000000000000, 44.84115912518001323, 56.85174851683467523 ) ) ;
#53333 = AXIS2_PLACEMENT_3D ( 'NONE', #87297, #54902, #13379 ) ;
#53334 = CARTESIAN_POINT ( 'NONE',  ( -43.72886361455299919, 434.3043191535924734, 13.94145212282985469 ) ) ;
#53335 = CARTESIAN_POINT ( 'NONE',  ( 106.4000000000000057, 0.000000000000000000, 0.000000000000000000 ) ) ;
#53336 = EDGE_LOOP ( 'NONE', ( #50337, #29084, #98046, #19300 ) ) ;
#53337 = CARTESIAN_POINT ( 'NONE',  ( -9.607612890400021755, 15.83452282593334992, -2.797297131808753168 ) ) ;
#53338 = CARTESIAN_POINT ( 'NONE',  ( 0.9999999999999956701, 0.000000000000000000, 42.58845726811989607 ) ) ;
#53339 = CARTESIAN_POINT ( 'NONE',  ( 51.01037695545453232, 500.0000000000002274, -5.000000000000001776 ) ) ;
#53340 = ORIENTED_EDGE ( 'NONE', *, *, #82481, .F. ) ;
#53341 = CARTESIAN_POINT ( 'NONE',  ( -29.89885390591881276, 311.8322808163144373, -7.366452359367730018 ) ) ;
#53342 = CARTESIAN_POINT ( 'NONE',  ( -38.65178583513453248, 312.1935651169637822, 6.094317023448435400 ) ) ;
#53343 = CARTESIAN_POINT ( 'NONE',  ( 34.83349330513379982, -7.703719777548943412E-31, 4.000000000000001776 ) ) ;
#53344 = CARTESIAN_POINT ( 'NONE',  ( 4.898587196589412829E-16, -22.62499999999999289, -8.000000000000000000 ) ) ;
#53345 = CARTESIAN_POINT ( 'NONE',  ( -31.57410453687917240, -24.95193506975139996, 39.69783569089302944 ) ) ;
#53346 = AXIS2_PLACEMENT_3D ( 'NONE', #52023, #18085, #100572 ) ;
#53347 = B_SPLINE_CURVE_WITH_KNOTS ( 'NONE', 3,
 ( #95404, #86277, #68487, #19971, #43661, #102970 ),
 .UNSPECIFIED., .F., .F.,
 ( 4, 2, 4 ),
 ( 2.380731629569644788E-07, 0.002336973833157563341, 0.004673709593152168724 ),
 .UNSPECIFIED. ) ;
#53348 = DIRECTION ( 'NONE',  ( -1.000000000000000000, -1.224606353822377258E-16, -0.000000000000000000 ) ) ;
#53349 = ORIENTED_EDGE ( 'NONE', *, *, #45847, .T. ) ;
#53350 = CARTESIAN_POINT ( 'NONE',  ( 83.54813190880366847, -50.11917785585441010, 185.4780095451953628 ) ) ;
#53351 = CARTESIAN_POINT ( 'NONE',  ( -48.15129163819138824, 9.495040186444070329, 16.85535821593516559 ) ) ;
#53352 = CARTESIAN_POINT ( 'NONE',  ( -85.95674408092972385, -47.25038601905195179, 189.6969179814721542 ) ) ;
#53353 = ORIENTED_EDGE ( 'NONE', *, *, #86606, .F. ) ;
#53354 = CARTESIAN_POINT ( 'NONE',  ( -84.25945711018864870, -37.82198024268028291, 39.37117510918165664 ) ) ;
#53355 = CARTESIAN_POINT ( 'NONE',  ( 44.78945892759311675, -5.000000000000009770, 0.000000000000000000 ) ) ;
#53356 = CARTESIAN_POINT ( 'NONE',  ( 10.71924530989560154, -5.000000000000002665, -74.44967652503841293 ) ) ;
#53357 = CARTESIAN_POINT ( 'NONE',  ( -30.90717084365936529, 9.524046525575998956, 40.57283699552785095 ) ) ;
#53358 =( BOUNDED_SURFACE ( )  B_SPLINE_SURFACE ( 3, 2, ( 
 ( #104579, #87357, #30735 ),
 ( #71672, #102471, #4302 ),
 ( #37239, #5372, #54414 ),
 ( #63621, #70099, #62037 ),
 ( #96509, #38292, #55478 ),
 ( #104048, #95975, #88415 ) ),
 .UNSPECIFIED., .F., .F., .F. ) 
 B_SPLINE_SURFACE_WITH_KNOTS ( ( 4, 2, 4 ),
 ( 3, 3 ),
 ( 0.003199762745115999809, 0.007302762474435751071, 0.01140576220375550190 ),
 ( 0.000000000000000000, 1.000000000000000000 ),
 .UNSPECIFIED. ) 
 GEOMETRIC_REPRESENTATION_ITEM ( )  RATIONAL_B_SPLINE_SURFACE ( (
 ( 1.000000000000000000, 0.8047731410850422762, 1.000000000000000000),
 ( 1.000000000000000000, 0.8125552299159720659, 1.000000000000000000),
 ( 1.000000000000000000, 0.8191520442885290576, 1.000000000000000000),
 ( 1.000000000000000000, 0.8191520442894507648, 1.000000000000000000),
 ( 1.000000000000000000, 0.8125552299152799529, 1.000000000000000000),
 ( 1.000000000000000000, 0.8047731410850428313, 1.000000000000000000) ) ) 
 REPRESENTATION_ITEM ( '' )  SURFACE ( )  );
#53359 = EDGE_CURVE ( 'NONE', #30449, #26965, #7301, .T. ) ;
#53360 =( LENGTH_UNIT ( ) NAMED_UNIT ( * ) SI_UNIT ( .MILLI., .METRE. ) );
#53361 = CARTESIAN_POINT ( 'NONE',  ( 17.70487366776518456, -59.99999999999999289, 39.97903104620380788 ) ) ;
#53362 = AXIS2_PLACEMENT_3D ( 'NONE', #6788, #30566, #47763 ) ;
#53363 = CARTESIAN_POINT ( 'NONE',  ( 10.34872164634795944, -20.36626283564415374, 35.40946532406196923 ) ) ;
#53364 =( NAMED_UNIT ( * ) SI_UNIT ( $, .STERADIAN. ) SOLID_ANGLE_UNIT ( ) );
#53365 = CARTESIAN_POINT ( 'NONE',  ( 33.70824286937537551, -23.45512021558194959, 33.05602448900377510 ) ) ;
#53366 = EDGE_CURVE ( 'NONE', #44884, #90212, #90003, .T. ) ;
#53369 = CARTESIAN_POINT ( 'NONE',  ( -11.82426874482432133, 21.31901130677117351, 7.426196524752196382 ) ) ;
#53368 = AXIS2_PLACEMENT_3D ( 'NONE', #67308, #16615, #10116 ) ;
#53367 = CARTESIAN_POINT ( 'NONE',  ( -30.90129479073731034, -33.04371094065780312, 41.11476907690651217 ) ) ;
#53370 = ADVANCED_FACE ( 'NONE', ( #52886 ), #18967, .F. ) ;
#53371 = CARTESIAN_POINT ( 'NONE',  ( 4.055648887448357165, 294.8040761930213307, -9.158006418842486340 ) ) ;
#53372 = PRESENTATION_STYLE_ASSIGNMENT (( #12363 ) ) ;
#53373 = CARTESIAN_POINT ( 'NONE',  ( 31.76566490452815117, 299.0319430614179055, -1.071778121186186317 ) ) ;
#53374 = CARTESIAN_POINT ( 'NONE',  ( 3.454253436624921569, -49.15858197120396511, 103.7259032015043090 ) ) ;
#53375 = DIRECTION ( 'NONE',  ( -0.000000000000000000, 1.000000000000000000, -0.000000000000000000 ) ) ;
#53376 = CONICAL_SURFACE ( 'NONE', #70390, 8.000000000000000000, 0.9599310885968911355 ) ;
#53377 = CARTESIAN_POINT ( 'NONE',  ( 0.000000000000000000, 70.00000000000000000, -7.025805963803935406 ) ) ;
#53378 = EDGE_CURVE ( 'NONE', #59016, #103960, #48875, .T. ) ;
#53379 = VERTEX_POINT ( 'NONE', #66953 ) ;
#53380 = CARTESIAN_POINT ( 'NONE',  ( -14.45621599724610462, 0.5024826578611153449, 14.99287714740787081 ) ) ;
#53381 = LINE ( 'NONE', #86300, #568 ) ;
#53382 = CARTESIAN_POINT ( 'NONE',  ( 4.656749229489883568, -63.68239591873568628, -3.785628640239150133 ) ) ;
#53383 = CONICAL_SURFACE ( 'NONE', #94756, 4.172000000000009479, 0.9599310885968813656 ) ;
#53385 = CARTESIAN_POINT ( 'NONE',  ( 7.860286775113991098, -34.58965292698938754, -32.51041876009787757 ) ) ;
#53384 = CARTESIAN_POINT ( 'NONE',  ( 26.08349330513380337, 1.593028355512270567E-15, 0.000000000000000000 ) ) ;
#53386 = ORIENTED_EDGE ( 'NONE', *, *, #105099, .F. ) ;
#53387 = B_SPLINE_CURVE_WITH_KNOTS ( 'NONE', 3,
 ( #21745, #29314, #95089, #37935, #80459, #6041, #22801, #62714 ),
 .UNSPECIFIED., .F., .F.,
 ( 4, 2, 2, 4 ),
 ( 0.000000000000000000, 0.0002399497798984991234, 0.0004798995597969982468, 0.0009597991195940054924 ),
 .UNSPECIFIED. ) ;
#53388 = COLOUR_RGB ( '', 0.08235294, 0.09019608, 0.10196078) ;
#53389 = CARTESIAN_POINT ( 'NONE',  ( 27.26394779839380433, 36.55151123035060579, 10.05698433968587580 ) ) ;
#53390 = DIRECTION ( 'NONE',  ( 0.000000000000000000, -1.000000000000000000, 0.000000000000000000 ) ) ;
#53391 = VERTEX_POINT ( 'NONE', #58867 ) ;
#53392 = CARTESIAN_POINT ( 'NONE',  ( 29.68315524076926337, 8.302504244945327017, -42.10535821593530414 ) ) ;
#53393 = CIRCLE ( 'NONE', #56835, 65.00000000000000000 ) ;
#53394 = LINE ( 'NONE', #77130, #21891 ) ;
#53395 = CARTESIAN_POINT ( 'NONE',  ( -93.39800921275812584, -60.00000000000001421, 36.10795237943069225 ) ) ;
#53396 = ORIENTED_EDGE ( 'NONE', *, *, #34685, .F. ) ;
#53397 = DIRECTION ( 'NONE',  ( 0.8191520442889974607, 1.003171929053531649E-16, -0.5735764363510380548 ) ) ;
#53398 = CARTESIAN_POINT ( 'NONE',  ( 25.59999999999999787, 1.533819458162526451E-15, 0.000000000000000000 ) ) ;
#53399 = FACE_OUTER_BOUND ( 'NONE', #84342, .T. ) ;
#53400 = CARTESIAN_POINT ( 'NONE',  ( -9.253500431420430772, 28.70228450082293037, 3.792688295761953210 ) ) ;
#53402 = FILL_AREA_STYLE_COLOUR ( '', #70215 ) ;
#53401 =( NAMED_UNIT ( * ) PLANE_ANGLE_UNIT ( ) SI_UNIT ( $, .RADIAN. ) );
#53403 = AXIS2_PLACEMENT_3D ( 'NONE', #87632, #103282, #70909 ) ;
#53404 = CARTESIAN_POINT ( 'NONE',  ( -80.75355258942967396, -56.92082733154106933, 176.6204916418753328 ) ) ;
#53405 = EDGE_LOOP ( 'NONE', ( #15179, #98926, #69580, #50627 ) ) ;
#53406 = DIRECTION ( 'NONE',  ( -1.000000000000000000, 0.000000000000000000, 0.000000000000000000 ) ) ;
#53407 = ORIENTED_EDGE ( 'NONE', *, *, #59961, .F. ) ;
#53408 = EDGE_LOOP ( 'NONE', ( #54871, #4981, #66795, #38185 ) ) ;
#53409 = CARTESIAN_POINT ( 'NONE',  ( -3.510455435514055811, -4.999999999999999112, 17.23741894013592102 ) ) ;
#53410 = CARTESIAN_POINT ( 'NONE',  ( -6.691148393532302840, -12.00380193953480124, 9.409600457876113211 ) ) ;
#53411 = SURFACE_SIDE_STYLE ('',( #60980 ) ) ;
#53412 = ORIENTED_EDGE ( 'NONE', *, *, #89996, .F. ) ;
#53413 = EDGE_CURVE ( 'NONE', #38472, #23399, #52612, .T. ) ;
#53414 = CARTESIAN_POINT ( 'NONE',  ( 3.433099864421321978, -0.8249814671519515308, 103.8029710478607939 ) ) ;
#53415 = CARTESIAN_POINT ( 'NONE',  ( -76.10153353667877241, -57.67120126903460431, -32.17100317442078961 ) ) ;
#53416 = CARTESIAN_POINT ( 'NONE',  ( 7.897196874019790869, -13.79127204167806831, -1.302055520192090254 ) ) ;
#53417 = FACE_OUTER_BOUND ( 'NONE', #79524, .T. ) ;
#53418 = CARTESIAN_POINT ( 'NONE',  ( 24.29659155877487464, 27.70505434333144379, 31.30545107321081133 ) ) ;
#53419 = CARTESIAN_POINT ( 'NONE',  ( -13.45079846400083490, -53.73428511282628506, 23.11721482942555284 ) ) ;
#53420 = CARTESIAN_POINT ( 'NONE',  ( -17.73901163440277884, 36.76451030150755628, -22.27377543627849121 ) ) ;
#53421 = AXIS2_PLACEMENT_3D ( 'NONE', #32561, #98328, #71930 ) ;
#53422 = CARTESIAN_POINT ( 'NONE',  ( 89.36652584573501201, -30.00000000000001421, 5.436425775551051665 ) ) ;
#53423 = EDGE_CURVE ( 'NONE', #1532, #93240, #51256, .T. ) ;
#53424 = CARTESIAN_POINT ( 'NONE',  ( -71.37516729659446924, -14.21045842199439946, 121.5232625957608974 ) ) ;
#53425 = CARTESIAN_POINT ( 'NONE',  ( -56.02824104333507904, -32.55801343818508542, 59.69165126840069036 ) ) ;
#53426 = ORIENTED_EDGE ( 'NONE', *, *, #36078, .F. ) ;
#53427 = CARTESIAN_POINT ( 'NONE',  ( 6.880652008360423899, 16.78823603829223643, -1.310808761845548620 ) ) ;
#53428 = VERTEX_POINT ( 'NONE', #38324 ) ;
#53429 = CARTESIAN_POINT ( 'NONE',  ( -101.9318200314704654, -60.21492788965887399, 194.2758051580982510 ) ) ;
#53430 = CARTESIAN_POINT ( 'NONE',  ( 101.3518415701702509, -38.00000000000003553, 187.1895103287365600 ) ) ;
#53431 = CARTESIAN_POINT ( 'NONE',  ( -30.90725857724320846, 14.69157187025842859, -40.57373053090537240 ) ) ;
#53432 = ORIENTED_EDGE ( 'NONE', *, *, #7720, .T. ) ;
#53433 = CARTESIAN_POINT ( 'NONE',  ( 6.256238905641753334, -4.999999999999998224, -71.20382033076053574 ) ) ;
#53434 = DIRECTION ( 'NONE',  ( 0.000000000000000000, 0.000000000000000000, 1.000000000000000000 ) ) ;
#53435 = CARTESIAN_POINT ( 'NONE',  ( -7.188101187500002709, -14.18750000204838280, 2.977408999572648707 ) ) ;
#53436 = FACE_OUTER_BOUND ( 'NONE', #103233, .T. ) ;
#53437 = SURFACE_SIDE_STYLE ('',( #103571 ) ) ;
#53438 = CARTESIAN_POINT ( 'NONE',  ( 69.28798965557233203, -30.00000000000000000, 93.06143263165685653 ) ) ;
#53439 = CARTESIAN_POINT ( 'NONE',  ( 31.21759734847655210, 387.2566916973277671, 24.99345285570965913 ) ) ;
#53440 = CARTESIAN_POINT ( 'NONE',  ( -9.176942142885224030, 44.04119814292888435, -13.55851898737775052 ) ) ;
#53441 = DIRECTION ( 'NONE',  ( -1.000000000000000000, -1.224606353822377258E-16, -0.000000000000000000 ) ) ;
#53442 = CARTESIAN_POINT ( 'NONE',  ( -7.500000000018718360, -2.376982511157173406, -18.31627213068317062 ) ) ;
#53443 = UNCERTAINTY_MEASURE_WITH_UNIT (LENGTH_MEASURE( 1.000000000000000082E-05 ), #89906, 'distance_accuracy_value', 'NONE');
#53444 = CARTESIAN_POINT ( 'NONE',  ( -27.03878911781851713, -32.52845681216340523, 31.02526571752343543 ) ) ;
#53445 = CIRCLE ( 'NONE', #98156, 14.78272384904389192 ) ;
#53446 = CARTESIAN_POINT ( 'NONE',  ( 48.21714293254901662, -53.35939452937847705, 52.27498384522137798 ) ) ;
#53447 = EDGE_LOOP ( 'NONE', ( #63615, #80398, #48581, #10808, #87688, #50220 ) ) ;
#53448 = FACE_OUTER_BOUND ( 'NONE', #48354, .T. ) ;
#53449 = CARTESIAN_POINT ( 'NONE',  ( -1.250293961483907923, 45.68606392481615330, 17.65583989057408587 ) ) ;
#53450 = AXIS2_PLACEMENT_3D ( 'NONE', #84422, #10516, #93040 ) ;
#53451 = B_SPLINE_CURVE_WITH_KNOTS ( 'NONE', 3,
 ( #83891, #93593, #91984, #100606 ),
 .UNSPECIFIED., .F., .F.,
 ( 4, 4 ),
 ( 0.0009672625908194888017, 0.02103544345022531625 ),
 .UNSPECIFIED. ) ;
#53452 = CARTESIAN_POINT ( 'NONE',  ( -93.96311375434591184, -38.49251773605704585, 201.1897569393096603 ) ) ;
#53453 = ORIENTED_EDGE ( 'NONE', *, *, #10689, .T. ) ;
#53454 = CARTESIAN_POINT ( 'NONE',  ( 90.72286138954092394, -38.34264739770473085, 7.039974769606621940 ) ) ;
#53455 = CARTESIAN_POINT ( 'NONE',  ( 13.94390863237126155, 6.957792695931584781, -7.985806807401195861 ) ) ;
#53456 = CARTESIAN_POINT ( 'NONE',  ( 0.000000000000000000, 4.898587196589412829E-16, -4.000000000000000000 ) ) ;
#53457 = CARTESIAN_POINT ( 'NONE',  ( 5.625019092414619948, 41.66287055497627989, -70.61600277306789053 ) ) ;
#53458 = CARTESIAN_POINT ( 'NONE',  ( 7.999999999999998224, -26.28125000409676915, 3.313708498984766049 ) ) ;
#53459 = CARTESIAN_POINT ( 'NONE',  ( -33.13096700376747350, 488.4252353400770517, 9.689492806026361649 ) ) ;
#53460 = FACE_OUTER_BOUND ( 'NONE', #93622, .T. ) ;
#53461 = EDGE_CURVE ( 'NONE', #54111, #3901, #16170, .T. ) ;
#53462 = CARTESIAN_POINT ( 'NONE',  ( 108.8942926950823562, -60.00000000000000000, 193.9232647688770896 ) ) ;
#53463 = VECTOR ( 'NONE', #34917, 1000.000000000000000 ) ;
#53464 = CARTESIAN_POINT ( 'NONE',  ( -7.151217271224853178, -66.78749400445718720, -3.587901469523285591 ) ) ;
#53465 = ORIENTED_EDGE ( 'NONE', *, *, #39569, .T. ) ;
#53466 = CARTESIAN_POINT ( 'NONE',  ( 7.212994264445061532, 32.01711344340037613, 3.463766307298584479 ) ) ;
#53467 = LINE ( 'NONE', #86387, #22946 ) ;
#53468 = ORIENTED_EDGE ( 'NONE', *, *, #34273, .F. ) ;
#53469 = AXIS2_PLACEMENT_3D ( 'NONE', #55460, #47381, #54390 ) ;
#53470 = DIRECTION ( 'NONE',  ( -0.000000000000000000, 1.000000000000000000, -0.000000000000000000 ) ) ;
#53471 = CARTESIAN_POINT ( 'NONE',  ( 3.313708498984722972, -21.21874999999998934, -8.000000000000040856 ) ) ;
#53472 = CARTESIAN_POINT ( 'NONE',  ( -6.397334739185441599, -3.000000000000000444, -4.916373759799320453 ) ) ;
#53473 = CARTESIAN_POINT ( 'NONE',  ( 40.96169049688617037, 435.9986040634733513, 6.367590718067603461 ) ) ;
#53474 = CARTESIAN_POINT ( 'NONE',  ( -7.188101187500001821, -11.37500000204838813, -2.977408999572651371 ) ) ;
#53475 = SURFACE_STYLE_FILL_AREA ( #69141 ) ;
#53476 = CIRCLE ( 'NONE', #98188, 4.000000000000007105 ) ;
#53477 = CARTESIAN_POINT ( 'NONE',  ( 30.90153257058524972, 13.61190038887009024, -41.14606609713278118 ) ) ;
#53479 = VERTEX_POINT ( 'NONE', #79809 ) ;
#53478 = CARTESIAN_POINT ( 'NONE',  ( 6.162888688655344893, -3.752776749732565253, 6.499999999999999112 ) ) ;
#53480 = CARTESIAN_POINT ( 'NONE',  ( 85.83717647578178855, -18.50068724157089761, 163.5510133277480520 ) ) ;
#53481 = VECTOR ( 'NONE', #64163, 1000.000000000000227 ) ;
#53482 = CARTESIAN_POINT ( 'NONE',  ( -41.72774289522170221, 484.6318496107492138, -3.104024719548849731 ) ) ;
#53483 = PLANE ( 'NONE',  #66097 ) ;
#53484 = EDGE_LOOP ( 'NONE', ( #68237, #48672, #26947, #23253 ) ) ;
#53485 = DIRECTION ( 'NONE',  ( 0.000000000000000000, 0.000000000000000000, -1.000000000000000000 ) ) ;
#53486 = LINE ( 'NONE', #36285, #40369 ) ;
#53487 = FACE_OUTER_BOUND ( 'NONE', #15193, .T. ) ;
#53488 = CARTESIAN_POINT ( 'NONE',  ( 24.05868969682389036, 1.340359594676612611E-15, 0.000000000000000000 ) ) ;
#53489 = CARTESIAN_POINT ( 'NONE',  ( 0.9986426376963660756, 14.07186834901433770, 51.25504895071563283 ) ) ;
#53490 = ORIENTED_EDGE ( 'NONE', *, *, #43555, .F. ) ;
#53491 = EDGE_CURVE ( 'NONE', #29335, #25223, #71701, .T. ) ;
#53492 = CARTESIAN_POINT ( 'NONE',  ( -71.80342408229677176, -30.00000000000000000, -19.71767938363507966 ) ) ;
#53493 = CARTESIAN_POINT ( 'NONE',  ( -5.000000000000000888, -32.16754151681192297, -4.059900122541123757 ) ) ;
#53494 = CARTESIAN_POINT ( 'NONE',  ( 14.78113245926357777, 22.77943572013436579, -2.487919536197025216 ) ) ;
#53495 = EDGE_CURVE ( 'NONE', #15460, #81556, #29996, .T. ) ;
#53497 = FILL_AREA_STYLE ('',( #69167 ) ) ;
#53496 = CARTESIAN_POINT ( 'NONE',  ( 60.63333333333333286, -3.309500000000000774, 0.000000000000000000 ) ) ;
#53498 = EDGE_CURVE ( 'NONE', #73607, #20227, #36750, .T. ) ;
#53499 = CARTESIAN_POINT ( 'NONE',  ( -2.977408999572650039, -24.68750000204838457, -7.188101187500001821 ) ) ;
#53500 = CARTESIAN_POINT ( 'NONE',  ( 15.67124661040751299, 294.5587369836088101, -10.06229308860519467 ) ) ;
#53501 = DIRECTION ( 'NONE',  ( -1.000000000000000000, 0.000000000000000000, 0.000000000000000000 ) ) ;
#53502 = CARTESIAN_POINT ( 'NONE',  ( 0.000000000000000000, 0.000000000000000000, -8.125150395352576993 ) ) ;
#53503 = CONTEXT_DEPENDENT_SHAPE_REPRESENTATION ( #35652, #3744 ) ;
#53504 = ORIENTED_EDGE ( 'NONE', *, *, #58597, .T. ) ;
#53505 = CARTESIAN_POINT ( 'NONE',  ( -36.89244916174478561, 490.9813517997146164, 12.46623585235509601 ) ) ;
#53506 = EDGE_CURVE ( 'NONE', #20836, #68326, #66763, .T. ) ;
#53507 = DIRECTION ( 'NONE',  ( -0.000000000000000000, -1.000000000000000000, -0.000000000000000000 ) ) ;
#53508 = CARTESIAN_POINT ( 'NONE',  ( -9.875464621210269911, 7.754124811870932277, 0.000000000000000000 ) ) ;
#53509 = FILL_AREA_STYLE_COLOUR ( '', #60207 ) ;
#53510 = CIRCLE ( 'NONE', #93085, 5.000000000000011546 ) ;
#53511 = ORIENTED_EDGE ( 'NONE', *, *, #93262, .F. ) ;
#53512 = CARTESIAN_POINT ( 'NONE',  ( 4.898587196589412829E-16, -16.62499999999999289, -8.000000000000000000 ) ) ;
#53513 = ORIENTED_EDGE ( 'NONE', *, *, #22767, .T. ) ;
#53514 =( BOUNDED_SURFACE ( )  B_SPLINE_SURFACE ( 3, 2, ( 
 ( #99226, #18900, #91178 ),
 ( #82532, #91697, #90629 ),
 ( #8635, #42595, #500 ),
 ( #92744, #8100, #41011 ) ),
 .UNSPECIFIED., .F., .F., .F. ) 
 B_SPLINE_SURFACE_WITH_KNOTS ( ( 4, 4 ),
 ( 3, 3 ),
 ( -1.569924745759010420E-16, 0.0002622513198881918023 ),
 ( 0.000000000000000000, 1.000000000000000000 ),
 .UNSPECIFIED. ) 
 GEOMETRIC_REPRESENTATION_ITEM ( )  RATIONAL_B_SPLINE_SURFACE ( (
 ( 1.000000000000000000, 0.7874655377939425716, 1.000000000000000000),
 ( 1.000000000000000000, 0.7887353030063650738, 1.000000000000000000),
 ( 1.000000000000000000, 0.7900011776560427190, 1.000000000000000000),
 ( 1.000000000000000000, 0.7912633096139881639, 1.000000000000000000) ) ) 
 REPRESENTATION_ITEM ( '' )  SURFACE ( )  );
#53515 = CARTESIAN_POINT ( 'NONE',  ( -28.08610930860416843, 34.36935600744033792, 8.015707762699872063 ) ) ;
#53516 = CARTESIAN_POINT ( 'NONE',  ( -1.992238869817333669, -0.1163433470869644354, 102.1880563748278519 ) ) ;
#53517 = CARTESIAN_POINT ( 'NONE',  ( 9.644834624769973885, 101.9910949979422412, 2.648308524638421702 ) ) ;
#53518 = UNCERTAINTY_MEASURE_WITH_UNIT (LENGTH_MEASURE( 1.000000000000000082E-05 ), #26770, 'distance_accuracy_value', 'NONE');
#53519 = CARTESIAN_POINT ( 'NONE',  ( -111.1270554948388138, -59.99999999999997868, 186.6394392527870423 ) ) ;
#53520 = DIRECTION ( 'NONE',  ( 0.000000000000000000, 0.000000000000000000, 1.000000000000000000 ) ) ;
#53521 = SURFACE_STYLE_USAGE ( .BOTH. , #104180 ) ;
#53522 = CARTESIAN_POINT ( 'NONE',  ( 26.08349330513380693, 1.593028355512270962E-15, 0.000000000000000000 ) ) ;
#53523 = CARTESIAN_POINT ( 'NONE',  ( 17.71323538867952152, 34.18408009164598127, -23.86039338639478302 ) ) ;
#53524 = CARTESIAN_POINT ( 'NONE',  ( -84.85100970293773059, -32.35236433163615288, 176.2939257893381182 ) ) ;
#53525 = CARTESIAN_POINT ( 'NONE',  ( 0.000000000000000000, 16.00000000000000000, 0.000000000000000000 ) ) ;
#53526 = CONICAL_SURFACE ( 'NONE', #75860, 4.250000000000000000, 0.9599310885968754814 ) ;
#53527 =( GEOMETRIC_REPRESENTATION_CONTEXT ( 3 ) GLOBAL_UNCERTAINTY_ASSIGNED_CONTEXT ( ( #18215 ) ) GLOBAL_UNIT_ASSIGNED_CONTEXT ( ( #20619, #26312, #25783 ) ) REPRESENTATION_CONTEXT ( 'NONE', 'WORKASPACE' ) );
#53528 = EDGE_LOOP ( 'NONE', ( #84809, #31678, #56525, #30263 ) ) ;
#53529 = CARTESIAN_POINT ( 'NONE',  ( -12.12010901803227192, 302.5867799420356619, 9.880676471810863504 ) ) ;
#53530 = CARTESIAN_POINT ( 'NONE',  ( 7.500000000000001776, 0.000000000000000000, 8.400000000000000355 ) ) ;
#53531 = CARTESIAN_POINT ( 'NONE',  ( -85.67862191555909135, -52.72633685597455155, -3.980294966729134742 ) ) ;
#53532 = CARTESIAN_POINT ( 'NONE',  ( -1.574031687317222650, -6.039084736198661041, -13.77476369210226537 ) ) ;
#53533 = CARTESIAN_POINT ( 'NONE',  ( -4.250302202869334245, 140.3077797975455212, -4.999999999999999112 ) ) ;
#53534 = CARTESIAN_POINT ( 'NONE',  ( 3.168323364912392748, 112.8168162893846329, -5.000000000000000000 ) ) ;
#53535 = DIRECTION ( 'NONE',  ( -0.9488877907218322694, 0.1950364375161481589, -0.2481385674578820699 ) ) ;
#53536 = CARTESIAN_POINT ( 'NONE',  ( -33.52312678242540755, 18.64316884714407152, -19.32152200344674498 ) ) ;
#53537 = AXIS2_PLACEMENT_3D ( 'NONE', #12926, #29180, #20573 ) ;
#53538 = CARTESIAN_POINT ( 'NONE',  ( 92.04793376076307254, -60.00000000000014211, 204.8851669578057795 ) ) ;
#53539 = EDGE_CURVE ( 'NONE', #100925, #45269, #17864, .T. ) ;
#53540 = CARTESIAN_POINT ( 'NONE',  ( -89.36642547188127139, -29.99999999999995381, 5.438168021589780743 ) ) ;
#53541 = CARTESIAN_POINT ( 'NONE',  ( -65.34887224726313093, -18.62568967254298258, 76.43621171049910856 ) ) ;
#53542 = ORIENTED_EDGE ( 'NONE', *, *, #67974, .F. ) ;
#53543 = CARTESIAN_POINT ( 'NONE',  ( 88.91505260351625850, -29.99999999999995381, 199.0551756924508879 ) ) ;
#53544 = CARTESIAN_POINT ( 'NONE',  ( -65.03121167221090104, 39.42464376491766842, -2.179090956683532809 ) ) ;
#53545 = CARTESIAN_POINT ( 'NONE',  ( 24.18667721825848105, -60.00000000000492406, 43.38656107002559281 ) ) ;
#53546 = VERTEX_POINT ( 'NONE', #63651 ) ;
#53547 = CARTESIAN_POINT ( 'NONE',  ( 104.9555555555555486, -4.171999999999998820, 0.000000000000000000 ) ) ;
#53548 = CARTESIAN_POINT ( 'NONE',  ( 7.188101187500000933, -26.93750000204838457, -2.977408999572650483 ) ) ;
#53549 = CARTESIAN_POINT ( 'NONE',  ( -0.08440048694455513922, 28.20649408426940496, -38.25000000000000000 ) ) ;
#53550 = ORIENTED_EDGE ( 'NONE', *, *, #50569, .F. ) ;
#53551 = DIRECTION ( 'NONE',  ( -1.000000000000000000, -1.224606353822377258E-16, -0.000000000000000000 ) ) ;
#53552 = ORIENTED_EDGE ( 'NONE', *, *, #2710, .F. ) ;
#53553 = DIRECTION ( 'NONE',  ( 0.000000000000000000, -1.000000000000000000, 0.000000000000000000 ) ) ;
#53554 = CARTESIAN_POINT ( 'NONE',  ( -41.71039089156239044, 485.6269440496943730, -4.295528331867323857 ) ) ;
#53555 = CARTESIAN_POINT ( 'NONE',  ( -91.70308476423518584, -60.00000000000001421, -15.04706914105544335 ) ) ;
#53556 = CARTESIAN_POINT ( 'NONE',  ( 36.61859841430800344, 369.8167902991359028, 3.938666744591956981 ) ) ;
#53557 = CARTESIAN_POINT ( 'NONE',  ( -4.413588872740236368, -9.188952367645423891, 5.751921314332417268 ) ) ;
#53558 = CARTESIAN_POINT ( 'NONE',  ( 32.84237740334679501, 485.2251842821274295, 5.746442123022993620 ) ) ;
#53559 = FACE_OUTER_BOUND ( 'NONE', #32108, .T. ) ;
#53560 = CARTESIAN_POINT ( 'NONE',  ( 5.000000000003806733, -51.23885339962929208, 3.814018968197090853 ) ) ;
#53561 = CARTESIAN_POINT ( 'NONE',  ( 7.374560640984048732, 50.00000000000000000, -94.59600210749853488 ) ) ;
#53562 = EDGE_CURVE ( 'NONE', #19817, #41440, #71293, .T. ) ;
#53563 = CARTESIAN_POINT ( 'NONE',  ( -7.344505440741524005, 107.4461892729869987, -3.175463080953003114 ) ) ;
#53564 = CARTESIAN_POINT ( 'NONE',  ( 6.936184427528457874, 0.000000000000000000, 0.000000000000000000 ) ) ;
#53565 = AXIS2_PLACEMENT_3D ( 'NONE', #74985, #1076, #77677 ) ;
#53566 = ORIENTED_EDGE ( 'NONE', *, *, #77098, .F. ) ;
#53567 = CARTESIAN_POINT ( 'NONE',  ( -38.34155876363399074, 18.64284798593178394, -2.616639027941926710 ) ) ;
#53569 = CARTESIAN_POINT ( 'NONE',  ( 36.78006001946765480, -56.81696112801252951, 39.80776084952203320 ) ) ;
#53568 = CARTESIAN_POINT ( 'NONE',  ( 4.959933632926892599, 51.41894395452099786, -8.497788349702878108 ) ) ;
#53570 = SURFACE_STYLE_FILL_AREA ( #3429 ) ;
#53571 = VERTEX_POINT ( 'NONE', #4336 ) ;
#53572 = CARTESIAN_POINT ( 'NONE',  ( -9.739726766683149961, 48.00000000000000000, -82.38252115640720774 ) ) ;
#53573 = CIRCLE ( 'NONE', #86314, 3.400000000000000355 ) ;
#53575 = CARTESIAN_POINT ( 'NONE',  ( -26.97491686565329161, 307.4599153070161606, -9.420584459367196573 ) ) ;
#53574 = DIRECTION ( 'NONE',  ( -1.000000000000000000, -1.224606353822377258E-16, -0.000000000000000000 ) ) ;
#53576 = DIRECTION ( 'NONE',  ( -0.000000000000000000, -1.000000000000000000, -0.000000000000000000 ) ) ;
#53577 = CARTESIAN_POINT ( 'NONE',  ( -43.75010090113831751, 464.8337800386757408, 11.75004750935459263 ) ) ;
#53578 = CARTESIAN_POINT ( 'NONE',  ( -41.15811204217362018, 436.5847606186492840, 6.466625614335570482 ) ) ;
#53580 = EDGE_CURVE ( 'NONE', #85025, #83274, #44814, .T. ) ;
#53579 = CARTESIAN_POINT ( 'NONE',  ( -48.90276556242077532, 14.54846953981632396, -14.70164374843202992 ) ) ;
#53581 = CARTESIAN_POINT ( 'NONE',  ( -34.88900972249390975, 464.6206820655984302, 18.69027339340992455 ) ) ;
#53582 = ORIENTED_EDGE ( 'NONE', *, *, #22604, .F. ) ;
#53583 = ADVANCED_FACE ( 'NONE', ( #45861 ), #86661, .F. ) ;
#53584 = CARTESIAN_POINT ( 'NONE',  ( 91.99065738214881094, -59.99999999999998579, 18.16284596454354272 ) ) ;
#53585 = CARTESIAN_POINT ( 'NONE',  ( 9.797174393178823685E-16, 0.000000000000000000, 7.999999999999994671 ) ) ;
#53586 = CYLINDRICAL_SURFACE ( 'NONE', #104823, 5.000000000000000888 ) ;
#53587 = CARTESIAN_POINT ( 'NONE',  ( -5.569577480994083452, 40.00000000004619949, -71.04463856145632406 ) ) ;
#53588 = CARTESIAN_POINT ( 'NONE',  ( 0.000000000000000000, 0.000000000000000000, 0.000000000000000000 ) ) ;
#53589 = ORIENTED_EDGE ( 'NONE', *, *, #76103, .T. ) ;
#53590 = AXIS2_PLACEMENT_3D ( 'NONE', #99729, #41487, #66299 ) ;
#53591 = CARTESIAN_POINT ( 'NONE',  ( -99.52556328755157722, -30.00000000001300293, 199.2777381299856359 ) ) ;
#53592 = EDGE_LOOP ( 'NONE', ( #60162, #103992, #63872, #63851, #73717 ) ) ;
#53593 = DIRECTION ( 'NONE',  ( -1.000000000000000000, -0.000000000000000000, -0.000000000000000000 ) ) ;
#53594 = CARTESIAN_POINT ( 'NONE',  ( 15.68546860017339384, 21.68927415056955965, -4.769872285904347642 ) ) ;
#53595 = CARTESIAN_POINT ( 'NONE',  ( -2.977408999572650039, -34.06250000204839523, -7.188101187500001821 ) ) ;
#53596 = CARTESIAN_POINT ( 'NONE',  ( -17.96996975600059088, 45.00000000000001421, 62.58803962699757761 ) ) ;
#53597 = LINE ( 'NONE', #11525, #71235 ) ;
#53598 = CARTESIAN_POINT ( 'NONE',  ( 32.84724555423649406, 479.6954591023948637, 7.498461155472820217 ) ) ;
#53599 = ORIENTED_EDGE ( 'NONE', *, *, #103844, .T. ) ;
#53600 = CARTESIAN_POINT ( 'NONE',  ( 17.50000000000002842, 47.00000000000000000, 64.09953197959339377 ) ) ;
#53602 = ORIENTED_EDGE ( 'NONE', *, *, #64247, .F. ) ;
#53601 = CARTESIAN_POINT ( 'NONE',  ( -44.21332904831282917, 435.2494715644501184, 14.45449769377396976 ) ) ;
#53603 = CARTESIAN_POINT ( 'NONE',  ( 78.93084866786456644, -36.02569822567065216, 136.0482817868801533 ) ) ;
#53604 = AXIS2_PLACEMENT_3D ( 'NONE', #50314, #15831, #1206 ) ;
#53605 = VERTEX_POINT ( 'NONE', #22134 ) ;
#53606 = CARTESIAN_POINT ( 'NONE',  ( 1.266928293263013039, -50.00000000000000000, 44.94249618006135449 ) ) ;
#53607 = CARTESIAN_POINT ( 'NONE',  ( -1.320432766682874540E-15, -16.53125000204838813, 7.188101187500000044 ) ) ;
#53608 = VECTOR ( 'NONE', #48140, 1000.000000000000000 ) ;
#53609 = CARTESIAN_POINT ( 'NONE',  ( -73.03813016181682372, -57.65004463643786892, 181.4998991682408302 ) ) ;
#53610 = VERTEX_POINT ( 'NONE', #64181 ) ;
#53611 = CONICAL_SURFACE ( 'NONE', #101880, 4.000000000000001776, 0.9599310885968774798 ) ;
#53613 = CARTESIAN_POINT ( 'NONE',  ( 0.000000000000000000, 274.9999999999999432, -7.999999999999986677 ) ) ;
#53612 = CIRCLE ( 'NONE', #60563, 5.000000000000011546 ) ;
#53614 = CARTESIAN_POINT ( 'NONE',  ( 7.133125581337410814, 41.57693000336763589, -59.23559349472980529 ) ) ;
#53615 = AXIS2_PLACEMENT_3D ( 'NONE', #5332, #38255, #54919 ) ;
#53616 = DIRECTION ( 'NONE',  ( 0.000000000000000000, 0.000000000000000000, -1.000000000000000000 ) ) ;
#53617 = CARTESIAN_POINT ( 'NONE',  ( 5.656854249492380582, -15.50000000409677092, -5.656854249492379694 ) ) ;
#53618 = CARTESIAN_POINT ( 'NONE',  ( -38.83689927739595049, -25.82488296874500477, 35.22879776301019206 ) ) ;
#53619 = CARTESIAN_POINT ( 'NONE',  ( 9.090909090909084611, 16.00000000000000000, 4.165977904505317575 ) ) ;
#53620 = CARTESIAN_POINT ( 'NONE',  ( -43.97892253343325564, 485.8746234537493365, 4.637105959633198715 ) ) ;
#53621 = CYLINDRICAL_SURFACE ( 'NONE', #55594, 4.000000000000000000 ) ;
#53622 = CARTESIAN_POINT ( 'NONE',  ( 4.297616547240164842, 51.67621034708934502, 8.057714428547381402 ) ) ;
#53623 = CARTESIAN_POINT ( 'NONE',  ( 131.8829176528314235, 104.1183258647170362, 161.0998715582510670 ) ) ;
#53624 = CARTESIAN_POINT ( 'NONE',  ( 33.74362713068861552, 463.9326864247046274, 7.533159870298661076 ) ) ;
#53625 = ORIENTED_EDGE ( 'NONE', *, *, #40202, .F. ) ;
#53626 = CARTESIAN_POINT ( 'NONE',  ( 41.50820411079202898, 461.5963371455317770, 2.703439750996501800 ) ) ;
#53627 = EDGE_CURVE ( 'NONE', #48268, #7084, #8570, .T. ) ;
#53628 = FACE_OUTER_BOUND ( 'NONE', #98414, .T. ) ;
#53629 = CARTESIAN_POINT ( 'NONE',  ( 1.328130235833654194, -17.76412090456761206, -37.95834240885186972 ) ) ;
#53630 = CARTESIAN_POINT ( 'NONE',  ( -65.73160349868967955, -30.00000000000001066, 82.32586786504053578 ) ) ;
#53631 = ADVANCED_FACE ( 'NONE', ( #49559 ), #81436, .T. ) ;
#53632 = CARTESIAN_POINT ( 'NONE',  ( 0.000000000000000000, 0.000000000000000000, 0.000000000000000000 ) ) ;
#53633 = CONICAL_SURFACE ( 'NONE', #39860, 5.000000000000001776, 0.9599310885968803664 ) ;
#53634 = EDGE_LOOP ( 'NONE', ( #96726, #21448 ) ) ;
#53635 = CARTESIAN_POINT ( 'NONE',  ( -14.82275922467060347, -4.333298119783967728, -10.06958627510921467 ) ) ;
#53636 = CARTESIAN_POINT ( 'NONE',  ( 77.67582994109527306, -57.51557269059810551, 196.1127657593792435 ) ) ;
#53637 = CIRCLE ( 'NONE', #39945, 4.000000000000000888 ) ;
#53638 = CARTESIAN_POINT ( 'NONE',  ( 0.000000000000000000, -46.00000000000000000, 119.0000000000000142 ) ) ;
#53639 = CARTESIAN_POINT ( 'NONE',  ( 76.12557658274099026, -38.35599704320051018, -28.58424740099938077 ) ) ;
#53640 = AXIS2_PLACEMENT_3D ( 'NONE', #91067, #65175, #41956 ) ;
#53641 = CARTESIAN_POINT ( 'NONE',  ( 37.33349330513379982, 1.593028355512270962E-15, 0.000000000000000000 ) ) ;
#53642 = PRODUCT ( '6. Link', '6. Link', '', ( #97788 ) ) ;
#53643 = CARTESIAN_POINT ( 'NONE',  ( -61.37266631565433528, -59.99999999999999289, 105.1188813016446488 ) ) ;
#53644 = CARTESIAN_POINT ( 'NONE',  ( 1.592040838891563829E-15, 1.000000000000000888, 13.00000000000003730 ) ) ;
#53645 = DIRECTION ( 'NONE',  ( 0.000000000000000000, -1.000000000000000000, 0.000000000000000000 ) ) ;
#53646 = B_SPLINE_CURVE_WITH_KNOTS ( 'NONE', 3,
 ( #35175, #59441, #4776, #21007, #5313, #70037 ),
 .UNSPECIFIED., .F., .F.,
 ( 4, 2, 4 ),
 ( 2.380729204593255505E-07, 0.003943479449179646337, 0.007886720825438833446 ),
 .UNSPECIFIED. ) ;
#53647 = CARTESIAN_POINT ( 'NONE',  ( 62.34828826643940403, 50.00000000000000000, -10.72527895994504199 ) ) ;
#53648 = CARTESIAN_POINT ( 'NONE',  ( -85.23892774877984380, -46.56544201171040953, 188.0817372555855229 ) ) ;
#53649 = ORIENTED_EDGE ( 'NONE', *, *, #42711, .F. ) ;
#53650 = CARTESIAN_POINT ( 'NONE',  ( 35.42407507202594275, 370.4409409265608133, 4.769248333007578999 ) ) ;
#53651 = CARTESIAN_POINT ( 'NONE',  ( -15.01526311245582335, 41.97362032292153344, -85.67311622495091683 ) ) ;
#53652 = CARTESIAN_POINT ( 'NONE',  ( -5.682852537008046490, 41.94661668455005810, -59.19459683319861654 ) ) ;
#53653 = DIRECTION ( 'NONE',  ( -1.000000000000000000, -1.224606353822377258E-16, -0.000000000000000000 ) ) ;
#53654 =( BOUNDED_SURFACE ( )  B_SPLINE_SURFACE ( 3, 3, ( 
 ( #61660, #20701, #101020, #36339 ),
 ( #85932, #18537, #44390, #77819 ),
 ( #43324, #51930, #76737, #86468 ),
 ( #69209, #102077, #68679, #101560 ),
 ( #3929, #60590, #93479, #12526 ),
 ( #11463, #78334, #19628, #59517 ),
 ( #52461, #4451, #37394, #105659 ),
 ( #6962, #4992, #80850, #56568 ),
 ( #78864, #45985, #70784, #54039 ),
 ( #48479, #89493, #82454, #8021 ),
 ( #40931, #65745, #41460, #37923 ),
 ( #15588, #81371, #73824, #62191 ),
 ( #95076, #97556, #21209, #106719 ),
 ( #81905, #47942, #65207, #103679 ),
 ( #7481, #39880, #98102, #31796 ),
 ( #72753, #86984, #32868, #64684 ),
 ( #13053, #24253, #97039, #29824 ),
 ( #88959, #23716, #49004, #73280 ) ),
 .UNSPECIFIED., .F., .F., .F. ) 
 B_SPLINE_SURFACE_WITH_KNOTS ( ( 4, 2, 2, 2, 2, 2, 2, 2, 4 ),
 ( 4, 4 ),
 ( 0.000000000000000000, 0.06249999999999997224, 0.1249999999999999445, 0.2500000000000000000, 0.3750000000000000555, 0.5000000000000000000, 0.7500000000000000000, 0.8750000000000000000, 1.000000000000000000 ),
 ( 0.000000000000000000, 1.000000000000000000 ),
 .UNSPECIFIED. ) 
 GEOMETRIC_REPRESENTATION_ITEM ( )  RATIONAL_B_SPLINE_SURFACE ( (
 ( 1.000000000000000000, 0.3333333333333334259, 0.3333333333333334259, 1.000000000000000000),
 ( 1.000000000000000000, 0.3333333333333334259, 0.3333333333333334259, 1.000000000000000000),
 ( 1.000000000000000000, 0.3333333333333334259, 0.3333333333333334259, 1.000000000000000000),
 ( 1.000000000000000000, 0.3333333333333334259, 0.3333333333333334259, 1.000000000000000000),
 ( 1.000000000000000000, 0.3333333333333334259, 0.3333333333333334259, 1.000000000000000000),
 ( 1.000000000000000000, 0.3333333333333334259, 0.3333333333333334259, 1.000000000000000000),
 ( 1.000000000000000000, 0.3333333333333334259, 0.3333333333333334259, 1.000000000000000000),
 ( 1.000000000000000000, 0.3333333333333334259, 0.3333333333333334259, 1.000000000000000000),
 ( 1.000000000000000000, 0.3333333333333334259, 0.3333333333333334259, 1.000000000000000000),
 ( 1.000000000000000000, 0.3333333333333334259, 0.3333333333333334259, 1.000000000000000000),
 ( 1.000000000000000000, 0.3333333333333334259, 0.3333333333333334259, 1.000000000000000000),
 ( 1.000000000000000000, 0.3333333333333334259, 0.3333333333333334259, 1.000000000000000000),
 ( 1.000000000000000000, 0.3333333333333334259, 0.3333333333333334259, 1.000000000000000000),
 ( 1.000000000000000000, 0.3333333333333334259, 0.3333333333333334259, 1.000000000000000000),
 ( 1.000000000000000000, 0.3333333333333334259, 0.3333333333333334259, 1.000000000000000000),
 ( 1.000000000000000000, 0.3333333333333334259, 0.3333333333333334259, 1.000000000000000000),
 ( 1.000000000000000000, 0.3333333333333334259, 0.3333333333333334259, 1.000000000000000000),
 ( 1.000000000000000000, 0.3333333333333334259, 0.3333333333333334259, 1.000000000000000000) ) ) 
 REPRESENTATION_ITEM ( '' )  SURFACE ( )  );
#53655 = DIRECTION ( 'NONE',  ( -0.000000000000000000, -0.000000000000000000, -1.000000000000000000 ) ) ;
#53656 = FACE_OUTER_BOUND ( 'NONE', #92567, .T. ) ;
#53657 = DIRECTION ( 'NONE',  ( -1.000000000000000000, 0.000000000000000000, 0.000000000000000000 ) ) ;
#53658 = DIRECTION ( 'NONE',  ( -0.5735764363510510444, -0.8191520442889883569, 0.000000000000000000 ) ) ;
#53659 = FACE_OUTER_BOUND ( 'NONE', #5045, .T. ) ;
#53660 = ORIENTED_EDGE ( 'NONE', *, *, #75133, .T. ) ;
#53661 = CARTESIAN_POINT ( 'NONE',  ( 18.71624549538633531, 50.00000000000000711, 60.97025553402504272 ) ) ;
#53662 = DIRECTION ( 'NONE',  ( 0.5735764363510466035, -0.8191520442889914655, 1.003171929053524500E-16 ) ) ;
#53663 = EDGE_CURVE ( 'NONE', #50732, #14213, #56413, .T. ) ;
#53664 = CARTESIAN_POINT ( 'NONE',  ( 107.3070812967312833, -60.00000000000004263, 109.8435067956896063 ) ) ;
#53665 = CARTESIAN_POINT ( 'NONE',  ( -80.68031237769524466, -36.03175770690578616, 146.2908660090107560 ) ) ;
#53666 = ORIENTED_EDGE ( 'NONE', *, *, #89658, .F. ) ;
#53667 = LINE ( 'NONE', #46636, #98078 ) ;
#53668 = DIRECTION ( 'NONE',  ( -0.000000000000000000, -0.000000000000000000, -1.000000000000000000 ) ) ;
#53669 = CARTESIAN_POINT ( 'NONE',  ( 45.02094980754542775, -57.68314110126151206, 65.19008676313157480 ) ) ;
#53670 = CARTESIAN_POINT ( 'NONE',  ( 63.05051047626579219, 50.00000000000000000, -0.01845826744785798376 ) ) ;
#53671 = CARTESIAN_POINT ( 'NONE',  ( 37.40222091011669647, 356.7670940962378836, 2.253866884981312602 ) ) ;
#53672 = CARTESIAN_POINT ( 'NONE',  ( 38.85838656119408085, 485.2519550107940063, -4.251882965831066841 ) ) ;
#53673 = VERTEX_POINT ( 'NONE', #7494 ) ;
#53674 = LINE ( 'NONE', #54187, #77096 ) ;
#53675 = AXIS2_PLACEMENT_3D ( 'NONE', #5327, #14985, #104000 ) ;
#53676 = CARTESIAN_POINT ( 'NONE',  ( 32.17889379758944557, 439.3695696554026995, 23.63219374846804044 ) ) ;
#53677 = CARTESIAN_POINT ( 'NONE',  ( -7.188101187500001821, -23.00000000204839523, -2.977408999572651371 ) ) ;
#53678 = VERTEX_POINT ( 'NONE', #99166 ) ;
#53679 = CARTESIAN_POINT ( 'NONE',  ( 43.68138489372805822, 484.4283016034004277, 2.027755642628115140 ) ) ;
#53680 = CIRCLE ( 'NONE', #22686, 15.00000000000000000 ) ;
#53681 = PLANE ( 'NONE',  #60179 ) ;
#53682 = CARTESIAN_POINT ( 'NONE',  ( 10.28624191511840458, 45.38549880562042205, 15.40779740156149202 ) ) ;
#53683 = ADVANCED_FACE ( 'NONE', ( #90560 ), #53887, .F. ) ;
#53684 = EDGE_CURVE ( 'NONE', #92773, #90141, #36699, .T. ) ;
#53685 = CARTESIAN_POINT ( 'NONE',  ( 72.37206225042174879, 6.856755485862130937E-15, 0.000000000000000000 ) ) ;
#53686 = CARTESIAN_POINT ( 'NONE',  ( -1.469576158976823947E-15, -17.37499999999999289, 8.000000000000000000 ) ) ;
#53687 = CARTESIAN_POINT ( 'NONE',  ( 4.898587196589412829E-16, -22.81250000409677270, -8.000000000000000000 ) ) ;
#53688 = ORIENTED_EDGE ( 'NONE', *, *, #46273, .F. ) ;
#53689 = CARTESIAN_POINT ( 'NONE',  ( 1.104211576045296406, 14.95094041744785329, -12.16229915940863293 ) ) ;
#53690 = AXIS2_PLACEMENT_3D ( 'NONE', #15212, #48099, #70281 ) ;
#53692 = CARTESIAN_POINT ( 'NONE',  ( 27.46944893902966811, -42.95628726384470042, 32.94719848304510634 ) ) ;
#53691 = CARTESIAN_POINT ( 'NONE',  ( -65.47633411339396048, -60.00000000000000000, 130.5853305762684329 ) ) ;
#53693 = CARTESIAN_POINT ( 'NONE',  ( -2.071635198146551927E-15, 58.72416816948006613, 16.91618513671782509 ) ) ;
#53694 = ORIENTED_EDGE ( 'NONE', *, *, #105400, .F. ) ;
#53695 = AXIS2_PLACEMENT_3D ( 'NONE', #52678, #93692, #103373 ) ;
#53696 = UNCERTAINTY_MEASURE_WITH_UNIT (LENGTH_MEASURE( 1.000000000000000082E-05 ), #57945, 'distance_accuracy_value', 'NONE');
#53697 = ORIENTED_EDGE ( 'NONE', *, *, #32270, .F. ) ;
#53698 = PRODUCT_DEFINITION_SHAPE ( 'NONE', 'NONE',  #106806 ) ;
#53699 = CARTESIAN_POINT ( 'NONE',  ( 72.50181414422412729, -37.99999999999997868, -21.26202816386757277 ) ) ;
#53700 = CARTESIAN_POINT ( 'NONE',  ( -13.99726531479253566, -57.99988801012565887, 27.38140257663831889 ) ) ;
#53701 = CARTESIAN_POINT ( 'NONE',  ( 27.10511071441176867, 34.75829513984540142, -7.556984339686343866 ) ) ;
#53702 = CARTESIAN_POINT ( 'NONE',  ( 6.169949891409287623, 4.949864754176874548, 4.426582755168845473 ) ) ;
#53703 = VERTEX_POINT ( 'NONE', #80323 ) ;
#53704 = EDGE_CURVE ( 'NONE', #96955, #80696, #98636, .T. ) ;
#53705 = SURFACE_STYLE_USAGE ( .BOTH. , #95766 ) ;
#53706 = CARTESIAN_POINT ( 'NONE',  ( 84.25466803195676846, -30.00000000000000711, 52.81349775392430956 ) ) ;
#53707 = CARTESIAN_POINT ( 'NONE',  ( 31.59761973271792002, 40.88238628480267067, -64.13876536422311858 ) ) ;
#53708 = LINE ( 'NONE', #37572, #78949 ) ;
#53709 = CARTESIAN_POINT ( 'NONE',  ( 81.45592718107263863, -29.99999999999999289, -9.616827637468841061 ) ) ;
#53710 = EDGE_CURVE ( 'NONE', #82451, #57189, #7541, .T. ) ;
#53711 = DIRECTION ( 'NONE',  ( -0.8257009859295904031, 0.000000000000000000, 0.5641080409238132809 ) ) ;
#53712 = ORIENTED_EDGE ( 'NONE', *, *, #38903, .F. ) ;
#53713 = AXIS2_PLACEMENT_3D ( 'NONE', #80856, #63644, #73286 ) ;
#53714 = ORIENTED_EDGE ( 'NONE', *, *, #54688, .F. ) ;
#53715 = ORIENTED_EDGE ( 'NONE', *, *, #7810, .T. ) ;
#53716 = DIRECTION ( 'NONE',  ( -0.5735764363510459374, -0.8191520442889919096, 0.000000000000000000 ) ) ;
#53717 = DIRECTION ( 'NONE',  ( -1.000000000000000000, -1.224606353822377258E-16, -0.000000000000000000 ) ) ;
#53718 = CARTESIAN_POINT ( 'NONE',  ( 100.6222222222222200, -4.171999999999998820, 0.000000000000000000 ) ) ;
#53719 = COLOUR_RGB ( '', 0.66274510, 0.83137255, 0.94901961) ;
#53720 = CARTESIAN_POINT ( 'NONE',  ( -5.656854249492381470, -16.25000000409677270, 5.656854249492379694 ) ) ;
#53721 = CARTESIAN_POINT ( 'NONE',  ( -1.729270706310499062, -69.60346723319459272, 12.84471657573915593 ) ) ;
#53722 = EDGE_CURVE ( 'NONE', #39800, #48174, #28072, .T. ) ;
#53723 = FACE_OUTER_BOUND ( 'NONE', #72155, .T. ) ;
#53724 = CARTESIAN_POINT ( 'NONE',  ( -6.499999999999999112, 3.752776749732556816, -8.000000000000000000 ) ) ;
#53725 = VERTEX_POINT ( 'NONE', #73290 ) ;
#53726 = CARTESIAN_POINT ( 'NONE',  ( 9.739726766100236688, 48.00000000000000000, -87.61747884500007899 ) ) ;
#53727 = VECTOR ( 'NONE', #73111, 1000.000000000000000 ) ;
#53728 = ORIENTED_EDGE ( 'NONE', *, *, #15652, .F. ) ;
#53729 = CARTESIAN_POINT ( 'NONE',  ( -4.595881407952570719, -63.93374566798679126, -3.857520671226067233 ) ) ;
#53730 = CARTESIAN_POINT ( 'NONE',  ( 47.25211357378231014, -38.32332363358291616, 62.33327775702132811 ) ) ;
#53731 = CARTESIAN_POINT ( 'NONE',  ( 31.79718767439307925, 436.0559061093508149, 18.03304884062774249 ) ) ;
#53732 = CARTESIAN_POINT ( 'NONE',  ( 28.10695518871528265, 297.0756177938578730, 10.42354765638709502 ) ) ;
#53733 = CARTESIAN_POINT ( 'NONE',  ( 9.970195021754669540, 302.6460196488382053, -10.04373974541433689 ) ) ;
#53734 = CARTESIAN_POINT ( 'NONE',  ( 64.25190437804278076, -36.00576792741288301, 82.20812981856342105 ) ) ;
#53735 = ADVANCED_FACE ( 'NONE', ( #105671 ), #21220, .T. ) ;
#53736 = VERTEX_POINT ( 'NONE', #57112 ) ;
#53737 = DIRECTION ( 'NONE',  ( -0.000000000000000000, -1.000000000000000000, -0.000000000000000000 ) ) ;
#53738 = CARTESIAN_POINT ( 'NONE',  ( -48.09573466820452836, -35.14038410512238642, -36.46244952396737915 ) ) ;
#53739 = CARTESIAN_POINT ( 'NONE',  ( -6.086031112480590366, 10.98017962735528386, -3.462237351910362193 ) ) ;
#53740 = DIRECTION ( 'NONE',  ( 1.000000000000000000, 0.000000000000000000, 0.000000000000000000 ) ) ;
#53741 = ORIENTED_EDGE ( 'NONE', *, *, #102806, .T. ) ;
#53742 = SHAPE_REPRESENTATION_RELATIONSHIP ( 'NONE' , 'NONE' ,  #59830, #19059 ) ;
#53743 = CARTESIAN_POINT ( 'NONE',  ( 58.92761780597729881, 6.856755485862130937E-15, 0.000000000000000000 ) ) ;
#53744 = LINE ( 'NONE', #95281, #52227 ) ;
#53745 = DIRECTION ( 'NONE',  ( -1.000000000000000000, 0.000000000000000000, -0.000000000000000000 ) ) ;
#53746 = CYLINDRICAL_SURFACE ( 'NONE', #84043, 1.999999999999998224 ) ;
#53747 = B_SPLINE_CURVE_WITH_KNOTS ( 'NONE', 3,
 ( #97918, #98963, #66618, #57985, #49895, #8904, #81193, #82803, #74693, #775, #25677, #48295, #39706, #91443, #72581, #47762, #80666, #64510, #97378, #89312, #7302, #40214, #73087, #32146, #26736, #43417, #69299, #18086, #77373, #35353, #75226, #59071, #68221, #19713 ),
 .UNSPECIFIED., .F., .F.,
 ( 4, 2, 2, 2, 2, 2, 2, 2, 2, 2, 2, 2, 2, 2, 2, 2, 4 ),
 ( 0.01263889472610567159, 0.01342810546992894739, 0.01421731621375222493, 0.01500652695757550073, 0.01579573770139877653, 0.01658494844522205580, 0.01737415918904533160, 0.01816336993286860740, 0.01895258067669188320, 0.01974179142051515901, 0.02053100216433843828, 0.02132021290816171408, 0.02210942365198498988, 0.02289863439580826915, 0.02368784513963154148, 0.02447705588345482075, 0.02526626662727809655 ),
 .UNSPECIFIED. ) ;
#53748 = CARTESIAN_POINT ( 'NONE',  ( -5.580966921651770022E-13, 25.16821295365027211, 40.75000000000505906 ) ) ;
#53749 = CARTESIAN_POINT ( 'NONE',  ( 9.999999999999998224, 15.11738935797198913, 0.3539438260532097869 ) ) ;
#53750 = CARTESIAN_POINT ( 'NONE',  ( 86.18704556189692312, -42.85049290463535243, 188.6112712611597999 ) ) ;
#53751 = CARTESIAN_POINT ( 'NONE',  ( 44.14911905790283697, 464.3766534542007207, 9.623404994951284763 ) ) ;
#53752 = B_SPLINE_CURVE_WITH_KNOTS ( 'NONE', 3,
 ( #12681, #30496, #54196, #63922, #54727, #13743, #63399, #78486, #104350, #71451, #21887, #62860, #87662, #46651, #79551, #5144, #6182, #53166, #87135, #4614 ),
 .UNSPECIFIED., .F., .F.,
 ( 4, 2, 2, 2, 2, 2, 2, 2, 2, 4 ),
 ( 0.007145084556283989689, 0.007649977546646419616, 0.008154870537008848674, 0.008659763527371279468, 0.009164656517733708527, 0.009417103012914925658, 0.009669549508096141055, 0.01017444249845856838, 0.01067933548882099570, 0.01118422847918342303 ),
 .UNSPECIFIED. ) ;
#53753 = CARTESIAN_POINT ( 'NONE',  ( -5.891808878741445099, 4.649940788608668107, 4.999999999999999112 ) ) ;
#53754 = CYLINDRICAL_SURFACE ( 'NONE', #32682, 1.250000000000000222 ) ;
#53755 = VECTOR ( 'NONE', #66473, 1000.000000000000000 ) ;
#53756 = CARTESIAN_POINT ( 'NONE',  ( 40.11650669486618881, 1.474610560812782335E-15, 0.000000000000000000 ) ) ;
#53757 = SURFACE_STYLE_FILL_AREA ( #78036 ) ;
#53758 = CARTESIAN_POINT ( 'NONE',  ( 5.000000000000000000, -13.79684580664352112, 10.70524563074489954 ) ) ;
#53759 = CARTESIAN_POINT ( 'NONE',  ( -97.61462959795420602, -29.99999999999999289, 134.8380256732861824 ) ) ;
#53760 = EDGE_CURVE ( 'NONE', #64846, #3711, #78541, .T. ) ;
#53761 = FACE_OUTER_BOUND ( 'NONE', #58432, .T. ) ;
#53762 = AXIS2_PLACEMENT_3D ( 'NONE', #14943, #47837, #6859 ) ;
#53763 = CARTESIAN_POINT ( 'NONE',  ( 0.5184698344275693316, -57.67120215776962056, 41.61168020182621063 ) ) ;
#53764 = EDGE_CURVE ( 'NONE', #9002, #72021, #2398, .T. ) ;
#53765 = CARTESIAN_POINT ( 'NONE',  ( 20.59999999999999787, 1.533819458162526451E-15, 0.000000000000000000 ) ) ;
#53766 = AXIS2_PLACEMENT_3D ( 'NONE', #22496, #73096, #30575 ) ;
#53767 = CARTESIAN_POINT ( 'NONE',  ( -32.19136361712720884, 464.6890450778107038, 10.76797718186653974 ) ) ;
#53768 = CARTESIAN_POINT ( 'NONE',  ( 7.270302578000960914, -3.659675574284857458, -18.03744543698567782 ) ) ;
#53769 =( LENGTH_UNIT ( ) NAMED_UNIT ( * ) SI_UNIT ( .MILLI., .METRE. ) );
#53770 = FACE_OUTER_BOUND ( 'NONE', #51455, .T. ) ;
#53771 = DIRECTION ( 'NONE',  ( -1.000000000000000000, -0.000000000000000000, -0.000000000000000000 ) ) ;
#53772 = ORIENTED_EDGE ( 'NONE', *, *, #65638, .T. ) ;
#53773 = CARTESIAN_POINT ( 'NONE',  ( 5.763702088647362665, 12.46422006045349917, 3.972887565972252233 ) ) ;
#53774 = DIRECTION ( 'NONE',  ( 1.000000000000000000, 1.224606353822377258E-16, 0.000000000000000000 ) ) ;
#53775 = CARTESIAN_POINT ( 'NONE',  ( -20.95351130271008699, -25.55484898855512910, 28.74739769140940382 ) ) ;
#53777 = CARTESIAN_POINT ( 'NONE',  ( 0.9545024399685089200, 36.45430134163607505, -29.31124438187364234 ) ) ;
#53776 = CARTESIAN_POINT ( 'NONE',  ( -85.33010815977807795, -59.99999999999997868, -15.43476000316156060 ) ) ;
#53778 = ORIENTED_EDGE ( 'NONE', *, *, #29706, .T. ) ;
#53779 = AXIS2_PLACEMENT_3D ( 'NONE', #60341, #43074, #16664 ) ;
#53780 = ORIENTED_EDGE ( 'NONE', *, *, #100437, .F. ) ;
#53781 = CARTESIAN_POINT ( 'NONE',  ( 42.72730916065222573, 485.8496625309479668, 7.279181987626980543 ) ) ;
#53782 = CIRCLE ( 'NONE', #46927, 5.000000000000011546 ) ;
#53783 = AXIS2_PLACEMENT_3D ( 'NONE', #15699, #80431, #64278 ) ;
#53784 = CARTESIAN_POINT ( 'NONE',  ( 15.38120149535017234, 2.925591750578491634, -2.537117285856969939 ) ) ;
#53785 = EDGE_CURVE ( 'NONE', #75857, #38628, #102088, .T. ) ;
#53786 = CARTESIAN_POINT ( 'NONE',  ( 0.000000000000000000, -1.023477375540016387, 0.000000000000000000 ) ) ;
#53787 = ORIENTED_EDGE ( 'NONE', *, *, #55995, .T. ) ;
#53788 = CARTESIAN_POINT ( 'NONE',  ( 32.74748809522914428, 438.8765027064216042, 23.82522251964440585 ) ) ;
#53789 = CARTESIAN_POINT ( 'NONE',  ( 0.000000000000000000, -46.00000000000000000, 112.0000000000000000 ) ) ;
#53790 = CARTESIAN_POINT ( 'NONE',  ( 103.1999130473613917, -52.71749418885885774, 189.5266586246194720 ) ) ;
#53791 = AXIS2_PLACEMENT_3D ( 'NONE', #46168, #21913, #5177 ) ;
#53793 = CARTESIAN_POINT ( 'NONE',  ( -13.00000000000003730, -65.00000000000000000, 0.000000000000000000 ) ) ;
#53792 = CARTESIAN_POINT ( 'NONE',  ( 33.59409845015440510, -32.33189051068966791, 33.26142729798142739 ) ) ;
#53794 = VERTEX_POINT ( 'NONE', #17748 ) ;
#53795 = ORIENTED_EDGE ( 'NONE', *, *, #79589, .F. ) ;
#53796 = ORIENTED_EDGE ( 'NONE', *, *, #16300, .T. ) ;
#53797 = CARTESIAN_POINT ( 'NONE',  ( 26.97263248440125238, 311.5055359114008979, 10.53075476637147823 ) ) ;
#53798 = CARTESIAN_POINT ( 'NONE',  ( -40.09057539293822714, 460.7411201710883688, 2.126307971704060495 ) ) ;
#53800 = EDGE_CURVE ( 'NONE', #14939, #84383, #29834, .T. ) ;
#53799 = ORIENTED_EDGE ( 'NONE', *, *, #80679, .T. ) ;
#53801 = CARTESIAN_POINT ( 'NONE',  ( 1.494796585009793288, -5.000000000000002665, -71.77219432632382734 ) ) ;
#53802 = CARTESIAN_POINT ( 'NONE',  ( -5.892293466952475356, 42.00785640414562039, -69.46301900959564080 ) ) ;
#53803 = CARTESIAN_POINT ( 'NONE',  ( -94.26650740058524036, -60.00000000002918199, 16.35100827053066652 ) ) ;
#53804 = DIRECTION ( 'NONE',  ( 0.000000000000000000, 0.000000000000000000, -1.000000000000000000 ) ) ;
#53805 = CARTESIAN_POINT ( 'NONE',  ( 9.945383863341344721, -59.99999999999997868, 39.64580126611800637 ) ) ;
#53806 = CARTESIAN_POINT ( 'NONE',  ( 12.86717642718393151, -5.000000000000000000, -10.20629072649130009 ) ) ;
#53807 = CARTESIAN_POINT ( 'NONE',  ( -5.398219627755024952, 41.68867587866067481, -58.74408776841643487 ) ) ;
#53809 = CARTESIAN_POINT ( 'NONE',  ( 12.17534591919128673, -22.06765856734515197, 27.61564892469329990 ) ) ;
#53808 = CARTESIAN_POINT ( 'NONE',  ( -104.6757555735165113, -59.99999999999997158, 94.38003174760403624 ) ) ;
#53810 = CARTESIAN_POINT ( 'NONE',  ( -8.239512452575834089, 51.94782406950919551, 1.561983666614737309 ) ) ;
#53811 = CARTESIAN_POINT ( 'NONE',  ( -48.85398691093387669, -25.67600413001694548, 44.56680585668343753 ) ) ;
#53812 = CARTESIAN_POINT ( 'NONE',  ( -3.737430656567119147, 19.28391223636466734, 5.919045189202371660 ) ) ;
#53813 = ORIENTED_EDGE ( 'NONE', *, *, #93690, .T. ) ;
#53814 = FACE_OUTER_BOUND ( 'NONE', #13422, .T. ) ;
#53815 = CONICAL_SURFACE ( 'NONE', #67839, 3.309500000000001663, 0.9599310885968770357 ) ;
#53816 = DIRECTION ( 'NONE',  ( -0.000000000000000000, 1.000000000000000000, -0.000000000000000000 ) ) ;
#53817 = DIRECTION ( 'NONE',  ( 0.000000000000000000, 1.000000000000000000, 0.000000000000000000 ) ) ;
#53818 = ORIENTED_EDGE ( 'NONE', *, *, #56578, .T. ) ;
#53819 = CARTESIAN_POINT ( 'NONE',  ( -8.643860566174014437, -4.452774918521638980, 14.41948991096433907 ) ) ;
#53820 = ORIENTED_EDGE ( 'NONE', *, *, #82191, .T. ) ;
#53821 = CARTESIAN_POINT ( 'NONE',  ( 105.1748584867626448, -29.99999999979880272, 127.7968817635670149 ) ) ;
#53822 = CARTESIAN_POINT ( 'NONE',  ( 4.245164436741635683, -48.92819220080328080, 104.4592797835102687 ) ) ;
#53823 = AXIS2_PLACEMENT_3D ( 'NONE', #70729, #3344, #93951 ) ;
#53824 = CARTESIAN_POINT ( 'NONE',  ( 6.913779129928546929, 41.73441125232163529, -59.30275354417915423 ) ) ;
#53825 = CARTESIAN_POINT ( 'NONE',  ( -36.40416150961017649, 41.99999999999999289, 47.37019975558912677 ) ) ;
#53826 = CARTESIAN_POINT ( 'NONE',  ( 98.00383005827913507, -30.00000000000000711, 190.5271024077575248 ) ) ;
#53827 = AXIS2_PLACEMENT_3D ( 'NONE', #18247, #90515, #32305 ) ;
#53828 = EDGE_CURVE ( 'NONE', #52643, #32906, #85128, .T. ) ;
#53829 = CARTESIAN_POINT ( 'NONE',  ( -1.130607513584494406, 36.55099619479304351, 29.03907309283103544 ) ) ;
#53830 = VERTEX_POINT ( 'NONE', #25881 ) ;
#53831 = COLOUR_RGB ( '', 0.66274510, 0.83137255, 0.94901961) ;
#53832 = VERTEX_POINT ( 'NONE', #101319 ) ;
#53833 = EDGE_LOOP ( 'NONE', ( #12375, #100619, #103437, #28676 ) ) ;
#53834 = CARTESIAN_POINT ( 'NONE',  ( 55.26720936171336973, -39.49716498785167573, 60.87020311775951598 ) ) ;
#53835 = CARTESIAN_POINT ( 'NONE',  ( 43.71037717921923615, 462.3391554988761527, 4.824299547763561513 ) ) ;
#53836 = COLOUR_RGB ( '', 0.08235294, 0.09019608, 0.10196078) ;
#53837 = ADVANCED_FACE ( 'NONE', ( #60347 ), #22900, .T. ) ;
#53838 = DIRECTION ( 'NONE',  ( -1.000000000000000000, -1.224606353822377258E-16, -0.000000000000000000 ) ) ;
#53839 = EDGE_CURVE ( 'NONE', #61668, #1636, #71139, .T. ) ;
#53840 = ORIENTED_EDGE ( 'NONE', *, *, #11140, .T. ) ;
#53841 = CARTESIAN_POINT ( 'NONE',  ( -84.13976397268963581, -38.35808942511454234, -23.59170179902847053 ) ) ;
#53842 = ORIENTED_EDGE ( 'NONE', *, *, #97176, .T. ) ;
#53843 = CARTESIAN_POINT ( 'NONE',  ( 3.750000000000007105, 6.495190528383288253, 1.734723475976807094E-15 ) ) ;
#53844 = CARTESIAN_POINT ( 'NONE',  ( 91.09535448090358045, -38.50834339303245457, 200.8244615020851711 ) ) ;
#53845 = CARTESIAN_POINT ( 'NONE',  ( 10.83667890787061516, 18.77600344465571780, 9.158742226827682131 ) ) ;
#53846 = CARTESIAN_POINT ( 'NONE',  ( 86.21060625849945325, -60.13110528944792321, 7.291613586972188088 ) ) ;
#53847 = CARTESIAN_POINT ( 'NONE',  ( 0.05533025579362222529, 4.993776679985858280, 4.350525068611868384 ) ) ;
#53848 = CARTESIAN_POINT ( 'NONE',  ( 40.95803508205418808, 397.0725699660951591, 27.65389706927792446 ) ) ;
#53849 = CARTESIAN_POINT ( 'NONE',  ( 21.08349330513380337, 1.593028355512270567E-15, 0.000000000000000000 ) ) ;
#53850 = ADVANCED_FACE ( 'NONE', ( #3149 ), #64234, .T. ) ;
#53851 = CARTESIAN_POINT ( 'NONE',  ( -40.06570913992068483, 460.7366702961384703, 2.123561850759500214 ) ) ;
#53852 = FACE_OUTER_BOUND ( 'NONE', #85347, .T. ) ;
#53853 = EDGE_LOOP ( 'NONE', ( #90868, #11194, #15228, #82251, #49416, #38246 ) ) ;
#53854 = CIRCLE ( 'NONE', #93446, 4.000000000000001776 ) ;
#53855 = CARTESIAN_POINT ( 'NONE',  ( 6.162888688655347558, 7.505553499465140277, 0.000000000000000000 ) ) ;
#53856 = CARTESIAN_POINT ( 'NONE',  ( 16.41900535493345359, 37.18348077072297997, -21.84048156163012067 ) ) ;
#53857 = STYLED_ITEM ( 'NONE', ( #33869 ), #89702 ) ;
#53858 = CARTESIAN_POINT ( 'NONE',  ( -3.983822489248328047, 136.6779593738534118, 4.999999999999998224 ) ) ;
#53859 = EDGE_LOOP ( 'NONE', ( #195, #105964, #13854, #65137 ) ) ;
#53860 = CARTESIAN_POINT ( 'NONE',  ( 99.75754961941544252, 1.030564683017419500E-14, 0.000000000000000000 ) ) ;
#53861 = CARTESIAN_POINT ( 'NONE',  ( -29.99619012559378461, 316.1192097185598300, 13.18038979099694252 ) ) ;
#53862 = LINE ( 'NONE', #28044, #48498 ) ;
#53863 = CARTESIAN_POINT ( 'NONE',  ( -8.000000000000000000, -23.84374999999999645, -3.313708498984762496 ) ) ;
#53864 = AXIS2_PLACEMENT_3D ( 'NONE', #21140, #64225, #63157 ) ;
#53865 = CARTESIAN_POINT ( 'NONE',  ( 40.21925173228400752, -28.65855273295322903, 47.52501080937051370 ) ) ;
#53866 = CARTESIAN_POINT ( 'NONE',  ( 39.84523985364286602, 437.5033382181499064, 4.901783744328642278 ) ) ;
#53867 = EDGE_LOOP ( 'NONE', ( #101370, #75062, #30530, #71275 ) ) ;
#53868 = CARTESIAN_POINT ( 'NONE',  ( 82.95844489808305866, -57.27508763463553976, 188.3864809084460603 ) ) ;
#53869 = CARTESIAN_POINT ( 'NONE',  ( 15.59999999999999787, 3.309500000000003439, 0.000000000000000000 ) ) ;
#53870 = EDGE_LOOP ( 'NONE', ( #73183, #86273, #10626, #26589, #32086, #55050 ) ) ;
#53871 = CARTESIAN_POINT ( 'NONE',  ( -85.96746068820245057, -45.26520172839578748, 43.44881241068694067 ) ) ;
#53872 = FILL_AREA_STYLE_COLOUR ( '', #95582 ) ;
#53873 = CARTESIAN_POINT ( 'NONE',  ( 13.14930780082191752, -5.000000000000002665, -86.33530272369397096 ) ) ;
#53874 = CARTESIAN_POINT ( 'NONE',  ( -30.90131729786687842, 8.441056540751493031, 41.14701368050880603 ) ) ;
#53875 = EDGE_CURVE ( 'NONE', #43496, #67063, #69401, .T. ) ;
#53876 = CARTESIAN_POINT ( 'NONE',  ( 11.54496644200874833, -20.90541225272014714, 35.52027033150145741 ) ) ;
#53877 = FACE_OUTER_BOUND ( 'NONE', #50729, .T. ) ;
#53878 = CARTESIAN_POINT ( 'NONE',  ( 51.38629157293619443, -29.89924560112501695, 48.97383748303278139 ) ) ;
#53879 = ADVANCED_FACE ( 'NONE', ( #75967, #11213 ), #2064, .T. ) ;
#53881 = CARTESIAN_POINT ( 'NONE',  ( -10.18285864187934209, 15.98045425121740237, 10.18118249357682359 ) ) ;
#53880 = DIRECTION ( 'NONE',  ( -1.000000000000000000, -0.000000000000000000, -0.000000000000000000 ) ) ;
#53882 = CARTESIAN_POINT ( 'NONE',  ( 8.823089264674861099, 295.7038567688685475, -10.03557449693187564 ) ) ;
#53883 = CARTESIAN_POINT ( 'NONE',  ( 40.95595929481465447, 405.2208686710653183, 27.85131585683114963 ) ) ;
#53884 = ORIENTED_EDGE ( 'NONE', *, *, #22361, .T. ) ;
#53885 = CARTESIAN_POINT ( 'NONE',  ( 41.71937287857456056, 325.3183896825876786, 5.429541239482419179 ) ) ;
#53886 = CARTESIAN_POINT ( 'NONE',  ( -2.212097561415797387, 14.31130214556278268, -12.46447053051441678 ) ) ;
#53887 = CONICAL_SURFACE ( 'NONE', #14229, 6.900000000000000355, 0.9599310885968801443 ) ;
#53888 = EDGE_CURVE ( 'NONE', #87052, #40910, #35015, .T. ) ;
#53889 = CARTESIAN_POINT ( 'NONE',  ( -82.65439507748990877, -38.00000000000004263, 4.655876099402581403 ) ) ;
#53890 = AXIS2_PLACEMENT_3D ( 'NONE', #93160, #68362, #4155 ) ;
#53891 = VERTEX_POINT ( 'NONE', #2600 ) ;
#53892 = CARTESIAN_POINT ( 'NONE',  ( -9.397382606151760243, -3.219694582843974473, 14.78427261612472599 ) ) ;
#53893 = CARTESIAN_POINT ( 'NONE',  ( 46.00000000000000711, 488.0062820891759543, 1.479102482845579658 ) ) ;
#53894 = COLOUR_RGB ( '', 0.09019608, 0.27058824, 0.51372549) ;
#53895 = DIRECTION ( 'NONE',  ( 0.000000000000000000, -0.8267102254944250772, -0.5626279437274306350 ) ) ;
#53897 = CARTESIAN_POINT ( 'NONE',  ( -4.645929030050260700, -21.77035645984657108, -30.46299186750976062 ) ) ;
#53896 = CARTESIAN_POINT ( 'NONE',  ( 0.000000000000000000, 37.86482112153537116, -10.52123582012687919 ) ) ;
#53898 = EDGE_CURVE ( 'NONE', #53023, #72526, #36093, .T. ) ;
#53899 = ORIENTED_EDGE ( 'NONE', *, *, #101734, .F. ) ;
#53900 = DIRECTION ( 'NONE',  ( 0.000000000000000000, 0.000000000000000000, 1.000000000000000000 ) ) ;
#53901 = CARTESIAN_POINT ( 'NONE',  ( -44.49616267108482504, 470.0857873864311500, 4.037868210216608134 ) ) ;
#53902 = ORIENTED_EDGE ( 'NONE', *, *, #79990, .F. ) ;
#53903 = FACE_BOUND ( 'NONE', #88741, .T. ) ;
#53904 = CARTESIAN_POINT ( 'NONE',  ( -30.00000000000000000, 461.8163627757383551, 11.11111419091028729 ) ) ;
#53905 = CARTESIAN_POINT ( 'NONE',  ( -93.45431775348167491, -59.99999999999999289, 36.62235110546294692 ) ) ;
#53906 = ORIENTED_EDGE ( 'NONE', *, *, #19572, .T. ) ;
#53907 = DIRECTION ( 'NONE',  ( 0.000000000000000000, -1.000000000000000000, 0.000000000000000000 ) ) ;
#53908 = CARTESIAN_POINT ( 'NONE',  ( 20.11650669486618881, 1.474610560812782335E-15, 0.000000000000000000 ) ) ;
#53909 = CARTESIAN_POINT ( 'NONE',  ( -4.335182740494876619, -48.88046597750100375, 104.3855524028883792 ) ) ;
#53910 = DIRECTION ( 'NONE',  ( -0.7071067811865456854, 8.659560562354957510E-17, -0.7071067811865493491 ) ) ;
#53911 = CARTESIAN_POINT ( 'NONE',  ( -83.59546275602320975, -32.52938965378904612, 164.2985913065920727 ) ) ;
#53912 = EDGE_LOOP ( 'NONE', ( #66059, #47354, #103564, #73067 ) ) ;
#53913 = CARTESIAN_POINT ( 'NONE',  ( -1.113195845631288261, 0.000000000000000000, -17.01594651244888468 ) ) ;
#53914 = ORIENTED_EDGE ( 'NONE', *, *, #56125, .F. ) ;
#53915 = ORIENTED_EDGE ( 'NONE', *, *, #90343, .F. ) ;
#53916 = CARTESIAN_POINT ( 'NONE',  ( -10.34493385746986505, -4.332661967061189223, -14.59917742215393588 ) ) ;
#53917 = AXIS2_PLACEMENT_3D ( 'NONE', #34249, #74129, #67121 ) ;
#53918 = CARTESIAN_POINT ( 'NONE',  ( -5.000000000000000000, -12.42851940633630825, 8.537252933895542739 ) ) ;
#53919 = CARTESIAN_POINT ( 'NONE',  ( -18.99999999999999289, -5.000000000000000000, 25.00000000000000000 ) ) ;
#53920 = ORIENTED_EDGE ( 'NONE', *, *, #57357, .T. ) ;
#53921 = CARTESIAN_POINT ( 'NONE',  ( -4.250000000000000000, 5.204748896376250699E-16, -6.606815774914157835 ) ) ;
#53922 = CARTESIAN_POINT ( 'NONE',  ( 15.11650669486618881, 1.474610560812782335E-15, 0.000000000000000000 ) ) ;
#53923 = CARTESIAN_POINT ( 'NONE',  ( -93.89173215636174064, -57.65323629495627245, -14.51111636511549996 ) ) ;
#53924 = CARTESIAN_POINT ( 'NONE',  ( 6.928203230275508773, -10.00000000000001066, -4.000000000000000000 ) ) ;
#53925 = CARTESIAN_POINT ( 'NONE',  ( 44.14911905790289381, 464.3766534542008344, 9.623404994951240354 ) ) ;
#53926 = CARTESIAN_POINT ( 'NONE',  ( -9.482945380845299255, 102.5566694122106810, 3.177595346755238914 ) ) ;
#53927 = CARTESIAN_POINT ( 'NONE',  ( -13.77155591953703961, -50.98632431394131714, 24.47427385584959225 ) ) ;
#53928 = CARTESIAN_POINT ( 'NONE',  ( 2.918503601030701056, 15.30040232763830765, -9.571198553003721798 ) ) ;
#53929 = CARTESIAN_POINT ( 'NONE',  ( 85.55833380596646975, -30.00000000000001776, -20.40969086358413520 ) ) ;
#53930 = CARTESIAN_POINT ( 'NONE',  ( -41.69391581180516937, -30.00000000000004974, 49.76410629065788527 ) ) ;
#53931 = CARTESIAN_POINT ( 'NONE',  ( -56.75726646438702261, -36.02614299241896845, 62.71715199122408535 ) ) ;
#53932 = VERTEX_POINT ( 'NONE', #26932 ) ;
#53933 = CARTESIAN_POINT ( 'NONE',  ( 5.763828452502797184, 13.53687047224920192, -3.972702736835264314 ) ) ;
#53934 = ORIENTED_EDGE ( 'NONE', *, *, #30725, .T. ) ;
#53935 = CARTESIAN_POINT ( 'NONE',  ( -100.7672544247349720, -52.74092989697082601, 193.5979465487865241 ) ) ;
#53936 = CARTESIAN_POINT ( 'NONE',  ( -30.77392345931232143, 15.52887250063908731, -40.23353194602704264 ) ) ;
#53937 = ORIENTED_EDGE ( 'NONE', *, *, #92660, .T. ) ;
#53938 = CARTESIAN_POINT ( 'NONE',  ( 19.47291202602108484, 49.99135632267985585, 60.38177670907871430 ) ) ;
#53939 = CARTESIAN_POINT ( 'NONE',  ( 5.082755093536324154, -13.71875000204838457, 5.082755093536326818 ) ) ;
#53940 = CARTESIAN_POINT ( 'NONE',  ( -1.901054659336256725, -69.56322987786279555, 12.86594763132180397 ) ) ;
#53941 = CARTESIAN_POINT ( 'NONE',  ( -1.469576158976823947E-15, -20.37499999999999289, 8.000000000000000000 ) ) ;
#53942 =( BOUNDED_CURVE ( )  B_SPLINE_CURVE ( 2, ( #598, #33563, #27089 ),
 .UNSPECIFIED., .F., .F. ) 
 B_SPLINE_CURVE_WITH_KNOTS ( ( 3, 3 ),
 ( 0.4303818025102752465, 1.000000000000000000 ),
 .UNSPECIFIED. ) 
 CURVE ( )  GEOMETRIC_REPRESENTATION_ITEM ( )  RATIONAL_B_SPLINE_CURVE ( ( 1.420262811277054782, 1.488244169276907503, 1.000000000000000000 ) ) 
 REPRESENTATION_ITEM ( '' )  );
#53943 = CARTESIAN_POINT ( 'NONE',  ( 6.026974479199131350E-05, -59.99999999999998579, 33.88964995960238014 ) ) ;
#53944 = CARTESIAN_POINT ( 'NONE',  ( -40.07586470527510158, 337.7832441655235129, 20.21182470898328631 ) ) ;
#53945 = CARTESIAN_POINT ( 'NONE',  ( -8.011504011031322037, 103.5457333638258604, 1.027162637006525905E-30 ) ) ;
#53946 = CARTESIAN_POINT ( 'NONE',  ( -0.7775020681061201033, 34.26564639408222490, 29.48222419693123797 ) ) ;
#53947 = EDGE_CURVE ( 'NONE', #62139, #97780, #96938, .T. ) ;
#53948 = DIRECTION ( 'NONE',  ( 0.000000000000000000, -1.000000000000000000, 0.000000000000000000 ) ) ;
#53949 = CARTESIAN_POINT ( 'NONE',  ( -27.34044518871554175, -25.57706821543484565, 29.89117138373360660 ) ) ;
#53950 = ORIENTED_EDGE ( 'NONE', *, *, #783, .T. ) ;
#53951 = ORIENTED_EDGE ( 'NONE', *, *, #22910, .F. ) ;
#53952 = CARTESIAN_POINT ( 'NONE',  ( 48.55886448841192049, -18.75703111879850127, 42.04255479722105804 ) ) ;
#53953 = CARTESIAN_POINT ( 'NONE',  ( -1.248974075102163850, 10.99431765185030052, 50.37162249473301756 ) ) ;
#53954 = DIRECTION ( 'NONE',  ( 0.000000000000000000, 0.000000000000000000, -1.000000000000000000 ) ) ;
#53955 = CARTESIAN_POINT ( 'NONE',  ( -110.5591912841294686, -38.35612243691561218, 181.8259589841011632 ) ) ;
#53956 = VERTEX_POINT ( 'NONE', #101836 ) ;
#53957 = CARTESIAN_POINT ( 'NONE',  ( 91.08098746901168852, -38.40443225276378314, -12.15589167778872692 ) ) ;
#53958 = CARTESIAN_POINT ( 'NONE',  ( -18.96508653188647031, 49.38837234725952641, 61.98939791137838995 ) ) ;
#53959 = CARTESIAN_POINT ( 'NONE',  ( 6.392921707093107919, 41.54610357469336179, -70.64273453041053585 ) ) ;
#53961 = CARTESIAN_POINT ( 'NONE',  ( 7.999999999999998224, -17.28125000409677625, 3.313708498984766049 ) ) ;
#53960 = AXIS2_PLACEMENT_3D ( 'NONE', #70287, #71333, #104225 ) ;
#53962 = FACE_OUTER_BOUND ( 'NONE', #105127, .T. ) ;
#53963 = CARTESIAN_POINT ( 'NONE',  ( 110.4675968189470012, -59.99999999999997868, 189.7332865883540478 ) ) ;
#53964 = AXIS2_PLACEMENT_3D ( 'NONE', #53398, #77676, #86319 ) ;
#53965 = EDGE_CURVE ( 'NONE', #25469, #8540, #43578, .T. ) ;
#53966 = AXIS2_PLACEMENT_3D ( 'NONE', #52068, #35943, #77421 ) ;
#53967 = CARTESIAN_POINT ( 'NONE',  ( -15.65011139837766230, 35.03623782845583889, 22.46068017020301255 ) ) ;
#53968 = EDGE_LOOP ( 'NONE', ( #74361, #86134, #97301, #52180 ) ) ;
#53969 = DIRECTION ( 'NONE',  ( 0.000000000000000000, -1.000000000000000000, 0.000000000000000000 ) ) ;
#53970 = B_SPLINE_CURVE_WITH_KNOTS ( 'NONE', 3,
 ( #2960, #19736, #85497, #84956 ),
 .UNSPECIFIED., .F., .F.,
 ( 4, 4 ),
 ( 0.000000000000000000, 1.000000000000000000 ),
 .UNSPECIFIED. ) ;
#53971 = CARTESIAN_POINT ( 'NONE',  ( -13.50000000000000178, -1.317096457811610888, -13.00000000000000178 ) ) ;
#53972 = ORIENTED_EDGE ( 'NONE', *, *, #35771, .T. ) ;
#53974 = DIRECTION ( 'NONE',  ( -1.000000000000000000, -0.000000000000000000, -0.000000000000000000 ) ) ;
#53973 = CARTESIAN_POINT ( 'NONE',  ( -110.8177222418062655, -38.35606902373660887, 164.8957494206476611 ) ) ;
#53975 = CARTESIAN_POINT ( 'NONE',  ( 8.000000000000000000, -21.49999999999999645, 0.000000000000000000 ) ) ;
#53976 = CARTESIAN_POINT ( 'NONE',  ( 29.83349330513380693, 1.593028355512270962E-15, 0.000000000000000000 ) ) ;
#53977 = FACE_OUTER_BOUND ( 'NONE', #5489, .T. ) ;
#53978 = CIRCLE ( 'NONE', #29920, 13.00000000000003730 ) ;
#53979 = CARTESIAN_POINT ( 'NONE',  ( -5.082755093536325042, -14.46875000204838457, -5.082755093536325930 ) ) ;
#53980 = CARTESIAN_POINT ( 'NONE',  ( 2.617478844991767861, -5.000000000000002665, -75.26027323389092771 ) ) ;
#53981 = CARTESIAN_POINT ( 'NONE',  ( 30.22873954704373745, 12.95661247755295875, -41.98212759391220317 ) ) ;
#53982 = ORIENTED_EDGE ( 'NONE', *, *, #33997, .T. ) ;
#53983 = CARTESIAN_POINT ( 'NONE',  ( 84.64420705326479322, -28.97169219033941445, 168.9226975528648040 ) ) ;
#53984 = CARTESIAN_POINT ( 'NONE',  ( 7.347880794884120722E-16, -99.99999999999997158, -6.000000000000000888 ) ) ;
#53985 = CARTESIAN_POINT ( 'NONE',  ( 9.989690267985803729, 88.97444416594913719, -0.5238310916885796642 ) ) ;
#53986 = EDGE_LOOP ( 'NONE', ( #90653, #52097, #65305, #18549 ) ) ;
#53987 = CARTESIAN_POINT ( 'NONE',  ( -36.34301548518092062, 333.8034728139880372, -2.455839358024256569 ) ) ;
#53988 = VECTOR ( 'NONE', #61328, 1000.000000000000000 ) ;
#53989 = CARTESIAN_POINT ( 'NONE',  ( -46.86052085224959995, 18.87480283624657673, 15.15319613412692590 ) ) ;
#53990 =( LENGTH_UNIT ( ) NAMED_UNIT ( * ) SI_UNIT ( .MILLI., .METRE. ) );
#53991 =( NAMED_UNIT ( * ) SI_UNIT ( $, .STERADIAN. ) SOLID_ANGLE_UNIT ( ) );
#53992 = CARTESIAN_POINT ( 'NONE',  ( 0.000000000000000000, 273.9999999999999432, 0.000000000000000000 ) ) ;
#53994 = CARTESIAN_POINT ( 'NONE',  ( 17.27446834819473054, 43.52264201582065084, 4.281299067926229718 ) ) ;
#53993 = COLOUR_RGB ( '', 0.31764706, 0.68627451, 0.89019608) ;
#53995 = ORIENTED_EDGE ( 'NONE', *, *, #58689, .F. ) ;
#53996 = EDGE_CURVE ( 'NONE', #88846, #97550, #67690, .T. ) ;
#53997 = CIRCLE ( 'NONE', #67811, 4.172000000000001485 ) ;
#53998 = DIRECTION ( 'NONE',  ( 0.000000000000000000, -1.000000000000000000, 0.000000000000000000 ) ) ;
#53999 = CARTESIAN_POINT ( 'NONE',  ( 37.56673239365870387, 25.47613764497372557, 13.45617127780999134 ) ) ;
#54000 = CARTESIAN_POINT ( 'NONE',  ( 32.04230769230768772, 1.411358822780289120E-15, 0.000000000000000000 ) ) ;
#54001 = EDGE_CURVE ( 'NONE', #11941, #9727, #57788, .T. ) ;
#54002 = EDGE_CURVE ( 'NONE', #85904, #92815, #60868, .T. ) ;
#54004 = DIRECTION ( 'NONE',  ( -1.000000000000000000, -0.000000000000000000, -0.000000000000000000 ) ) ;
#54003 = FACE_BOUND ( 'NONE', #30472, .T. ) ;
#54005 = CARTESIAN_POINT ( 'NONE',  ( 7.188101187499999156, -19.25000000204838813, 2.977408999572654924 ) ) ;
#54006 = CARTESIAN_POINT ( 'NONE',  ( 46.00000000000000000, 437.9690125970931831, 14.09127711025711349 ) ) ;
#54007 = FACE_BOUND ( 'NONE', #79988, .T. ) ;
#54008 = EDGE_LOOP ( 'NONE', ( #45739, #92959, #105305, #49276 ) ) ;
#54009 = DIRECTION ( 'NONE',  ( -0.000000000000000000, 1.000000000000000000, 0.000000000000000000 ) ) ;
#54010 = DIRECTION ( 'NONE',  ( -1.000000000000000000, 0.000000000000000000, 0.000000000000000000 ) ) ;
#54011 = CARTESIAN_POINT ( 'NONE',  ( -9.460558175875586784, 9.928212646478041137, 0.000000000000000000 ) ) ;
#54012 = DIRECTION ( 'NONE',  ( 0.000000000000000000, 0.000000000000000000, 1.000000000000000000 ) ) ;
#54013 = CARTESIAN_POINT ( 'NONE',  ( -14.97192734824248461, 2.056257465145892027, -0.8331214207561096208 ) ) ;
#54014 = EDGE_CURVE ( 'NONE', #89753, #24036, #12816, .T. ) ;
#54015 = VERTEX_POINT ( 'NONE', #12291 ) ;
#54016 = DIRECTION ( 'NONE',  ( -1.000000000000000000, -1.224606353822377258E-16, -0.000000000000000000 ) ) ;
#54017 = CARTESIAN_POINT ( 'NONE',  ( 2.354803500934600891, 50.00000000000001421, -100.0000000000000000 ) ) ;
#54018 = VERTEX_POINT ( 'NONE', #78612 ) ;
#54019 = ADVANCED_FACE ( 'NONE', ( #13875 ), #21484, .F. ) ;
#54020 = CARTESIAN_POINT ( 'NONE',  ( -28.10445496912546659, 34.19346676493858439, 9.576006629673763371 ) ) ;
#54021 = CARTESIAN_POINT ( 'NONE',  ( 7.347880794884118356E-15, 45.50000000000000711, -60.00000000000000000 ) ) ;
#54022 = CARTESIAN_POINT ( 'NONE',  ( 0.000000000000000000, 43.00000000000000000, 0.000000000000000000 ) ) ;
#54023 = CARTESIAN_POINT ( 'NONE',  ( -111.6689541673699750, -60.00000000000000000, 183.3448424905921286 ) ) ;
#54024 = CARTESIAN_POINT ( 'NONE',  ( 6.499999999999999112, 3.752776749732595452, -0.7999999999999977129 ) ) ;
#54025 = CARTESIAN_POINT ( 'NONE',  ( -7.681258945454893382E-14, -1.200000000000000030E-05, -39.50000000000000000 ) ) ;
#54026 = EDGE_CURVE ( 'NONE', #31057, #86235, #34728, .T. ) ;
#54027 = CARTESIAN_POINT ( 'NONE',  ( 43.43869229197127169, 464.9661605157749591, 13.42065392471465834 ) ) ;
#54028 = CARTESIAN_POINT ( 'NONE',  ( -85.31393835196715258, -28.76575568053742415, 175.9393138315395504 ) ) ;
#54029 = CONICAL_SURFACE ( 'NONE', #33364, 3.309500000000001663, 0.9599310885968770357 ) ;
#54030 = CARTESIAN_POINT ( 'NONE',  ( 43.64059727138994305, 41.42723139259643972, -50.50409788923168009 ) ) ;
#54031 = EDGE_LOOP ( 'NONE', ( #13017, #65589, #6191, #43922, #88258, #68246 ) ) ;
#54032 = CARTESIAN_POINT ( 'NONE',  ( 4.656390720430120922, -66.31646185960548223, 3.786082374785837867 ) ) ;
#54033 = CARTESIAN_POINT ( 'NONE',  ( -86.12938452815190260, -60.14213912132001383, 12.56794793439099500 ) ) ;
#54034 = CARTESIAN_POINT ( 'NONE',  ( -1.000000000000000000, -5.000000000000015099, -14.14213562373094923 ) ) ;
#54035 = CARTESIAN_POINT ( 'NONE',  ( -2.845103660799776613, 79.93183047064682967, -4.999999999999998224 ) ) ;
#54036 = LINE ( 'NONE', #30338, #25279 ) ;
#54037 = CARTESIAN_POINT ( 'NONE',  ( 59.23741894013591036, 42.00000000000000711, -7.754160006507188285 ) ) ;
#54038 = CARTESIAN_POINT ( 'NONE',  ( 103.1541778469752160, -29.99999999999992184, 197.4146557462016176 ) ) ;
#54039 = CARTESIAN_POINT ( 'NONE',  ( -3.409519076813957649E-15, 51.11204936430951307, 27.84083606136722366 ) ) ;
#54040 = CARTESIAN_POINT ( 'NONE',  ( -106.1205840060921730, -60.00000000000004263, 102.8126256328862667 ) ) ;
#54041 = CARTESIAN_POINT ( 'NONE',  ( -64.56638066497201578, -25.57904519531993870, 77.78355544515780196 ) ) ;
#54042 = B_SPLINE_CURVE_WITH_KNOTS ( 'NONE', 3,
 ( #77922, #77387, #53635, #78970, #84946, #94656, #3501, #46088, #36442, #94100, #70362, #12108, #11036, #76845, #86568, #5095, #2950, #20802 ),
 .UNSPECIFIED., .F., .F.,
 ( 4, 2, 2, 2, 2, 2, 2, 2, 4 ),
 ( 0.000000000000000000, 0.06249999999964576253, 0.1249999999992915251, 0.1874999999989372945, 0.2499999999985830501, 0.3124999999982288057, 0.3749999999978745890, 0.4374999999975203169, 0.4999999999971661002 ),
 .UNSPECIFIED. ) ;
#54043 = VERTEX_POINT ( 'NONE', #13342 ) ;
#54044 = CARTESIAN_POINT ( 'NONE',  ( 93.93534938131868728, -14.21045842199442433, 198.1410878059230072 ) ) ;
#54045 = CARTESIAN_POINT ( 'NONE',  ( -62.40064228140166591, 39.42532419955585254, 18.44113199567702921 ) ) ;
#54046 = CARTESIAN_POINT ( 'NONE',  ( 77.77493926578759442, -60.00000000000120792, 197.3217668548883239 ) ) ;
#54047 = ORIENTED_EDGE ( 'NONE', *, *, #57983, .F. ) ;
#54048 = CARTESIAN_POINT ( 'NONE',  ( -32.94352307842197547, 463.6326549538489985, 6.941370215387414611 ) ) ;
#54049 = CARTESIAN_POINT ( 'NONE',  ( -2.977408999572650039, -17.56250000204838813, -7.188101187500000933 ) ) ;
#54050 =( LENGTH_UNIT ( ) NAMED_UNIT ( * ) SI_UNIT ( .MILLI., .METRE. ) );
#54051 = ORIENTED_EDGE ( 'NONE', *, *, #18641, .T. ) ;
#54052 = DIRECTION ( 'NONE',  ( -1.000000000000000000, -0.000000000000000000, -0.000000000000000000 ) ) ;
#54053 = ORIENTED_EDGE ( 'NONE', *, *, #77588, .T. ) ;
#54054 = DIRECTION ( 'NONE',  ( 0.000000000000000000, 1.000000000000000000, 0.000000000000000000 ) ) ;
#54055 = AXIS2_PLACEMENT_3D ( 'NONE', #19705, #14065, #95535 ) ;
#54056 = LINE ( 'NONE', #28795, #95388 ) ;
#54057 = CARTESIAN_POINT ( 'NONE',  ( -92.45990064392792362, -60.00000000000002842, -11.61392837640961595 ) ) ;
#54058 = CARTESIAN_POINT ( 'NONE',  ( 6.177150199754223969, -12.02207793746708830, -1.226588410918951848E-14 ) ) ;
#54059 = CARTESIAN_POINT ( 'NONE',  ( 7.188101187499999156, -31.62500000204838813, 2.977408999572654924 ) ) ;
#54060 = DIRECTION ( 'NONE',  ( 0.000000000000000000, 0.000000000000000000, 1.000000000000000000 ) ) ;
#54061 = CARTESIAN_POINT ( 'NONE',  ( 21.88880945939638067, -4.285714285714295357, 12.64023069600375493 ) ) ;
#54062 = CARTESIAN_POINT ( 'NONE',  ( 1.000000000000000000, -56.64186896442130603, 6.232146447172338455 ) ) ;
#54063 = DIRECTION ( 'NONE',  ( 0.000000000000000000, -1.000000000000000000, 0.000000000000000000 ) ) ;
#54064 = CARTESIAN_POINT ( 'NONE',  ( -6.928203230275509661, 105.2693092969554129, -4.000000000000002665 ) ) ;
#54065 = CARTESIAN_POINT ( 'NONE',  ( 39.57869015843260740, 437.2512761492686195, 5.285341955750249454 ) ) ;
#54066 = EDGE_CURVE ( 'NONE', #73855, #33037, #12536, .T. ) ;
#54067 = CARTESIAN_POINT ( 'NONE',  ( 33.81356276710358344, 316.6001882432930188, -6.691973795892937282 ) ) ;
#54068 =( GEOMETRIC_REPRESENTATION_CONTEXT ( 3 ) GLOBAL_UNCERTAINTY_ASSIGNED_CONTEXT ( ( #16539 ) ) GLOBAL_UNIT_ASSIGNED_CONTEXT ( ( #17816, #58807, #50163 ) ) REPRESENTATION_CONTEXT ( 'NONE', 'WORKASPACE' ) );
#54069 = B_SPLINE_CURVE_WITH_KNOTS ( 'NONE', 3,
 ( #2028, #65179, #98072, #89986, #16093, #48972 ),
 .UNSPECIFIED., .F., .F.,
 ( 4, 2, 4 ),
 ( 0.000000000000000000, 0.0004189869898914155171, 0.0008379739797828289743 ),
 .UNSPECIFIED. ) ;
#54070 = VECTOR ( 'NONE', #46954, 1000.000000000000000 ) ;
#54071 = ORIENTED_EDGE ( 'NONE', *, *, #58333, .F. ) ;
#54072 = CARTESIAN_POINT ( 'NONE',  ( -9.781128050978084687, 53.39489088403298211, -3.094517574441575380 ) ) ;
#54073 = CARTESIAN_POINT ( 'NONE',  ( 22.33349330513380693, 1.593028355512270962E-15, 0.000000000000000000 ) ) ;
#54074 = CARTESIAN_POINT ( 'NONE',  ( 34.85686279961707612, -22.18117105793543331, 31.83958341934053848 ) ) ;
#54075 = CARTESIAN_POINT ( 'NONE',  ( -19.43146043915540488, 9.659702761776270386E-13, -11.19959342721046980 ) ) ;
#54076 = ORIENTED_EDGE ( 'NONE', *, *, #57683, .T. ) ;
#54077 = EDGE_CURVE ( 'NONE', #104064, #104530, #84934, .T. ) ;
#54078 = FACE_OUTER_BOUND ( 'NONE', #24768, .T. ) ;
#54079 = ADVANCED_FACE ( 'NONE', ( #46791 ), #102371, .T. ) ;
#54081 = CARTESIAN_POINT ( 'NONE',  ( 42.33349330513380693, 4.000000000000003553, 0.000000000000000000 ) ) ;
#54080 = CARTESIAN_POINT ( 'NONE',  ( 9.361783665678713007, -4.999999999999999112, -18.66271547844284484 ) ) ;
#54082 = DIRECTION ( 'NONE',  ( 0.000000000000000000, -1.000000000000000000, 0.000000000000000000 ) ) ;
#54083 = CARTESIAN_POINT ( 'NONE',  ( -33.00000000000000000, 463.5362553048592531, 6.739467187734380360 ) ) ;
#54084 =( NAMED_UNIT ( * ) PLANE_ANGLE_UNIT ( ) SI_UNIT ( $, .RADIAN. ) );
#54085 = SURFACE_STYLE_FILL_AREA ( #77856 ) ;
#54086 = CARTESIAN_POINT ( 'NONE',  ( -49.15106604892663711, 13.74065395669281919, -15.05054071407247740 ) ) ;
#54087 = CARTESIAN_POINT ( 'NONE',  ( -4.562211633346542783, -47.83778420154242639, 43.06387934016247243 ) ) ;
#54088 = VERTEX_POINT ( 'NONE', #45220 ) ;
#54089 = EDGE_CURVE ( 'NONE', #2153, #19188, #59165, .T. ) ;
#54090 = CARTESIAN_POINT ( 'NONE',  ( 92.27083909279834018, -59.99999999999999289, 1.911750569454251814 ) ) ;
#54091 = CARTESIAN_POINT ( 'NONE',  ( 27.86890485335036871, 34.24656432884084722, -9.810347930556213569 ) ) ;
#54092 = CARTESIAN_POINT ( 'NONE',  ( -43.50718830201091691, 484.7945958152782282, 4.126963862728817212 ) ) ;
#54093 = EDGE_CURVE ( 'NONE', #81027, #9677, #65978, .T. ) ;
#54094 = CARTESIAN_POINT ( 'NONE',  ( -5.558537907172038217, 40.95020998767025588, -70.99752123435956719 ) ) ;
#54095 = CARTESIAN_POINT ( 'NONE',  ( -13.27104247666666126, 19.68897887149177350, -7.441391031246531007 ) ) ;
#54096 = VERTEX_POINT ( 'NONE', #81263 ) ;
#54097 = STYLED_ITEM ( 'NONE', ( #35832 ), #61965 ) ;
#54098 = CARTESIAN_POINT ( 'NONE',  ( -106.3631125035437464, -30.00000000000582290, 193.1115520981887812 ) ) ;
#54099 = VERTEX_POINT ( 'NONE', #32760 ) ;
#54100 = CARTESIAN_POINT ( 'NONE',  ( 33.33990657616778464, 464.2315420232596921, 17.97851960990114151 ) ) ;
#54101 = SURFACE_STYLE_FILL_AREA ( #46560 ) ;
#54102 = CARTESIAN_POINT ( 'NONE',  ( 0.000000000000000000, 0.000000000000000000, 4.000000000000000000 ) ) ;
#54103 = CARTESIAN_POINT ( 'NONE',  ( 84.09852957777411575, -60.17183186639107362, -17.33093850757677146 ) ) ;
#54104 = CARTESIAN_POINT ( 'NONE',  ( 7.188101187500000044, -30.03125000204838813, 0.000000000000000000 ) ) ;
#54105 = CARTESIAN_POINT ( 'NONE',  ( -7.000000000000000000, 8.572527594031471218E-16, -13.00000000000000000 ) ) ;
#54106 = CARTESIAN_POINT ( 'NONE',  ( 73.50474219086036953, -59.99999999999997158, -24.84696050693406022 ) ) ;
#54107 = DIRECTION ( 'NONE',  ( 0.000000000000000000, 0.000000000000000000, 1.000000000000000000 ) ) ;
#54108 = ORIENTED_EDGE ( 'NONE', *, *, #74995, .F. ) ;
#54109 = AXIS2_PLACEMENT_3D ( 'NONE', #46279, #74778, #42423 ) ;
#54110 = AXIS2_PLACEMENT_3D ( 'NONE', #25972, #84161, #85219 ) ;
#54111 = VERTEX_POINT ( 'NONE', #41349 ) ;
#54112 = CARTESIAN_POINT ( 'NONE',  ( 77.90476537984217487, -53.37054513156353863, 147.1940195355752792 ) ) ;
#54113 = AXIS2_PLACEMENT_3D ( 'NONE', #6728, #88191, #14809 ) ;
#54114 = FACE_OUTER_BOUND ( 'NONE', #30507, .T. ) ;
#54115 = ORIENTED_EDGE ( 'NONE', *, *, #57720, .T. ) ;
#54116 = CARTESIAN_POINT ( 'NONE',  ( -12.50000000000000178, 28.79325661138934223, -46.42958547950013326 ) ) ;
#54117 = CARTESIAN_POINT ( 'NONE',  ( -5.082755093536325042, -17.09375000204838813, -5.082755093536325930 ) ) ;
#54118 = CARTESIAN_POINT ( 'NONE',  ( -93.14832842661381562, -57.61817439972283239, 204.4570750068989469 ) ) ;
#54119 = EDGE_LOOP ( 'NONE', ( #93729, #96956 ) ) ;
#54120 = CARTESIAN_POINT ( 'NONE',  ( -6.000469943554648466, -14.00070491670499884, 0.2622423038614475899 ) ) ;
#54121 = CARTESIAN_POINT ( 'NONE',  ( -9.537291425704609082, 82.35595622667227644, 3.012810007365997134 ) ) ;
#54122 = EDGE_CURVE ( 'NONE', #47288, #80922, #33286, .T. ) ;
#54123 = DIRECTION ( 'NONE',  ( 0.000000000000000000, -1.000000000000000000, 0.000000000000000000 ) ) ;
#54124 = CARTESIAN_POINT ( 'NONE',  ( -8.000000000000000000, -13.43750000409676915, -9.797174393178825657E-16 ) ) ;
#54125 = DIRECTION ( 'NONE',  ( 0.000000000000000000, -1.000000000000000000, 0.000000000000000000 ) ) ;
#54126 =( BOUNDED_SURFACE ( )  B_SPLINE_SURFACE ( 3, 2, ( 
 ( #37620, #3625, #70483 ),
 ( #29525, #30567, #79092 ),
 ( #22489, #106001, #105488 ),
 ( #14872, #96873, #87203 ) ),
 .UNSPECIFIED., .F., .F., .T. ) 
 B_SPLINE_SURFACE_WITH_KNOTS ( ( 4, 4 ),
 ( 3, 3 ),
 ( -3.035766082959412415E-18, 0.002033478645168744405 ),
 ( 0.000000000000000000, 1.000000000000000000 ),
 .UNSPECIFIED. ) 
 GEOMETRIC_REPRESENTATION_ITEM ( )  RATIONAL_B_SPLINE_SURFACE ( (
 ( 1.000000000000000000, 0.8239349643288668146, 1.000000000000000000),
 ( 1.000000000000000000, 0.8158483196103311075, 1.000000000000000000),
 ( 1.000000000000000000, 0.8066624588212628622, 1.000000000000000000),
 ( 1.000000000000000000, 0.7976994903569351036, 1.000000000000000000) ) ) 
 REPRESENTATION_ITEM ( '' )  SURFACE ( )  );
#54127 = CARTESIAN_POINT ( 'NONE',  ( -1.000000000000000000, -64.45248229066025658, 10.00070197187164389 ) ) ;
#54128 = ADVANCED_FACE ( 'NONE', ( #96933 ), #47310, .T. ) ;
#54129 = B_SPLINE_CURVE_WITH_KNOTS ( 'NONE', 3,
 ( #24755, #49525, #17187, #65724, #89474, #25294, #100210, #8002 ),
 .UNSPECIFIED., .F., .F.,
 ( 4, 2, 2, 4 ),
 ( 0.003797433802554453248, 0.004743183970586247432, 0.005688934138618042050, 0.007580434474681629550 ),
 .UNSPECIFIED. ) ;
#54130 = CARTESIAN_POINT ( 'NONE',  ( 6.827804075408431927, -2.999999999999529265, -71.19745151638494463 ) ) ;
#54131 = CARTESIAN_POINT ( 'NONE',  ( 5.290067270632455632, 51.34639538792298197, 8.531152949374481764 ) ) ;
#54133 = CIRCLE ( 'NONE', #100659, 12.00000000000001066 ) ;
#54132 = DIRECTION ( 'NONE',  ( -1.000000000000000000, 7.216449660063517513E-16, -4.520949615337404585E-17 ) ) ;
#54134 = CARTESIAN_POINT ( 'NONE',  ( 37.72563823326647992, 27.83002455384509233, 10.95617127780987410 ) ) ;
#54135 = VERTEX_POINT ( 'NONE', #39777 ) ;
#54136 = CARTESIAN_POINT ( 'NONE',  ( -4.415716460554405032, -52.49535300446108721, 40.28654576308774438 ) ) ;
#54137 = DIRECTION ( 'NONE',  ( 0.000000000000000000, 1.000000000000000000, 0.000000000000000000 ) ) ;
#54138 = CARTESIAN_POINT ( 'NONE',  ( 72.11682663846713126, 6.975173280561618775E-15, 0.000000000000000000 ) ) ;
#54139 = PRESENTATION_LAYER_ASSIGNMENT (  '', '', ( #55826 ) ) ;
#54140 = CARTESIAN_POINT ( 'NONE',  ( -60.05068428883747345, -29.84980960968719188, -32.87300430704357268 ) ) ;
#54141 = CARTESIAN_POINT ( 'NONE',  ( -82.83898444641884851, -29.99999999999999645, 151.7304382314388249 ) ) ;
#54142 = CARTESIAN_POINT ( 'NONE',  ( 0.000000000000000000, 115.0000000000000000, 0.000000000000000000 ) ) ;
#54143 = AXIS2_PLACEMENT_3D ( 'NONE', #92484, #777, #99505 ) ;
#54144 = ORIENTED_EDGE ( 'NONE', *, *, #33390, .T. ) ;
#54145 = CARTESIAN_POINT ( 'NONE',  ( 104.9555555555555486, 4.172000000000019249, 5.109226446042768454E-16 ) ) ;
#54146 = CARTESIAN_POINT ( 'NONE',  ( 74.24793750212994325, -57.60337406675898819, 188.0840138985208512 ) ) ;
#54147 = CARTESIAN_POINT ( 'NONE',  ( 32.99999999999997868, 439.0771093100264011, 24.89389206971034341 ) ) ;
#54148 = CARTESIAN_POINT ( 'NONE',  ( 0.2259792476677682238, -7.636022678937430364, -6.470294263593375561 ) ) ;
#54149 = CARTESIAN_POINT ( 'NONE',  ( -14.81542429970186348, 22.88666905516585004, 2.089502384907108379 ) ) ;
#54150 = CARTESIAN_POINT ( 'NONE',  ( -5.290067270632282437, 54.20842449845790867, 6.031152949371105798 ) ) ;
#54151 = CARTESIAN_POINT ( 'NONE',  ( -68.42323370297573604, -60.00000000000000711, 133.1930357778236385 ) ) ;
#54152 = DIRECTION ( 'NONE',  ( -0.5735764363510512664, 0.8191520442889881348, 1.003171929053520309E-16 ) ) ;
#54153 = EDGE_CURVE ( 'NONE', #83606, #80083, #93642, .T. ) ;
#54154 = CARTESIAN_POINT ( 'NONE',  ( -22.66220480930539338, 50.00000000000000000, 59.06576954297837290 ) ) ;
#54155 = CARTESIAN_POINT ( 'NONE',  ( -84.77375970704859753, -53.83494961134933021, 190.3341756863800356 ) ) ;
#54156 = EDGE_LOOP ( 'NONE', ( #12165, #30763, #62380, #41329, #47390 ) ) ;
#54157 = CARTESIAN_POINT ( 'NONE',  ( 33.35361065611909481, 318.9767138392345487, -6.332425068735285656 ) ) ;
#54158 = CARTESIAN_POINT ( 'NONE',  ( -3.493042281569127550, 304.8518027749427119, -10.00000000028269298 ) ) ;
#54159 = CARTESIAN_POINT ( 'NONE',  ( -6.982952086341226661, 41.78396327145789257, -59.69785475644857797 ) ) ;
#54160 = DIRECTION ( 'NONE',  ( 0.000000000000000000, 0.6543614439339219269, -0.7561819230137102332 ) ) ;
#54161 = CARTESIAN_POINT ( 'NONE',  ( 32.99999999999962341, 465.3568906370355762, 17.69306951624823654 ) ) ;
#54162 = VECTOR ( 'NONE', #2391, 1000.000000000000000 ) ;
#54164 = CARTESIAN_POINT ( 'NONE',  ( 0.000000000000000000, 7.505553499465139389, -6.505213034913023646E-16 ) ) ;
#54163 = AXIS2_PLACEMENT_3D ( 'NONE', #74381, #17244, #24286 ) ;
#54165 = CARTESIAN_POINT ( 'NONE',  ( -85.28245759913484392, -60.20252963265404844, -15.59029267851214584 ) ) ;
#54166 = DIRECTION ( 'NONE',  ( -1.000000000000000000, -1.224606353822377258E-16, -0.000000000000000000 ) ) ;
#54167 = DIRECTION ( 'NONE',  ( 0.000000000000000000, -0.9405207353770788092, 0.3397362893859868782 ) ) ;
#54168 = ORIENTED_EDGE ( 'NONE', *, *, #94440, .F. ) ;
#54169 = PRESENTATION_STYLE_ASSIGNMENT (( #104876 ) ) ;
#54170 = CARTESIAN_POINT ( 'NONE',  ( -1.206569728928480911, -7.963640680051490506, -0.4524126574264524248 ) ) ;
#54171 = SURFACE_STYLE_USAGE ( .BOTH. , #26777 ) ;
#54172 = CARTESIAN_POINT ( 'NONE',  ( -6.928203230275508773, 105.0000000000000000, 4.000000000000001776 ) ) ;
#54173 = CARTESIAN_POINT ( 'NONE',  ( 89.21217950020245269, -30.00000000000004974, 13.74488734703711934 ) ) ;
#54174 = CARTESIAN_POINT ( 'NONE',  ( -78.19826841161986408, -53.37652838430405922, 149.2861074551972536 ) ) ;
#54175 = PRODUCT_DEFINITION ( 'UNKNOWN', '', #2496, #31687 ) ;
#54176 = VERTEX_POINT ( 'NONE', #88325 ) ;
#54177 = LINE ( 'NONE', #3536, #61932 ) ;
#54178 = DIRECTION ( 'NONE',  ( 0.000000000000000000, -1.000000000000000000, 0.000000000000000000 ) ) ;
#54179 = CARTESIAN_POINT ( 'NONE',  ( 82.65254975104842572, -57.52971634350765839, 200.9502613691210229 ) ) ;
#54180 = CIRCLE ( 'NONE', #31809, 0.4999999999999987232 ) ;
#54181 = FILL_AREA_STYLE_COLOUR ( '', #78671 ) ;
#54182 = UNCERTAINTY_MEASURE_WITH_UNIT (LENGTH_MEASURE( 1.000000000000000082E-05 ), #85424, 'distance_accuracy_value', 'NONE');
#54183 = CONICAL_SURFACE ( 'NONE', #16315, 4.000000000000001776, 0.9599310885968808105 ) ;
#54184 = CARTESIAN_POINT ( 'NONE',  ( 42.85049267684065910, 321.7985655941586174, -3.456638000609795647 ) ) ;
#54185 = DIRECTION ( 'NONE',  ( 0.000000000000000000, 0.000000000000000000, 1.000000000000000000 ) ) ;
#54186 = ORIENTED_EDGE ( 'NONE', *, *, #9734, .T. ) ;
#54187 = CARTESIAN_POINT ( 'NONE',  ( 28.58349330513380337, -4.000000000000000000, 4.898587196589415787E-16 ) ) ;
#54188 = FILL_AREA_STYLE_COLOUR ( '', #73731 ) ;
#54189 = DIRECTION ( 'NONE',  ( -1.000000000000000000, -1.224606353822377258E-16, -0.000000000000000000 ) ) ;
#54190 = CARTESIAN_POINT ( 'NONE',  ( 7.188101187499999156, -22.25000000204839168, 2.977408999572654924 ) ) ;
#54191 = VERTEX_POINT ( 'NONE', #23605 ) ;
#54192 = DIRECTION ( 'NONE',  ( -1.000000000000000000, -1.224606353822377258E-16, -0.000000000000000000 ) ) ;
#54193 = AXIS2_PLACEMENT_3D ( 'NONE', #33082, #98826, #38644 ) ;
#54194 = CARTESIAN_POINT ( 'NONE',  ( 72.11682663846713126, 6.975173280561618775E-15, 0.000000000000000000 ) ) ;
#54195 = CARTESIAN_POINT ( 'NONE',  ( -44.00767003729956883, 435.4943399909807340, 9.943675474308832918 ) ) ;
#54196 = CARTESIAN_POINT ( 'NONE',  ( 26.78538857523856720, 36.99571777491210867, 7.587731473697932216 ) ) ;
#54197 = DIRECTION ( 'NONE',  ( -0.5735764363510494901, -0.8191520442889894671, 0.000000000000000000 ) ) ;
#54198 = CARTESIAN_POINT ( 'NONE',  ( 17.62275466961044401, 43.36964291604525812, -4.614633819576646978 ) ) ;
#54199 = ORIENTED_EDGE ( 'NONE', *, *, #86921, .F. ) ;
#54200 = CARTESIAN_POINT ( 'NONE',  ( 91.56522374861557978, -59.99999999999998579, -15.43920004744107644 ) ) ;
#54202 = CARTESIAN_POINT ( 'NONE',  ( 26.89278686401765484, -29.04926881985026554, 30.38490685316056883 ) ) ;
#54201 = CARTESIAN_POINT ( 'NONE',  ( -76.24265395543058332, -14.21045842199434794, 145.5858823757693301 ) ) ;
#54203 = CARTESIAN_POINT ( 'NONE',  ( -5.404594501095027787E-15, 34.25047185182970111, 44.13186320217320713 ) ) ;
#54204 = ORIENTED_EDGE ( 'NONE', *, *, #101977, .F. ) ;
#54205 = EDGE_CURVE ( 'NONE', #15279, #49001, #68115, .T. ) ;
#54206 = ORIENTED_EDGE ( 'NONE', *, *, #37517, .T. ) ;
#54207 = CARTESIAN_POINT ( 'NONE',  ( 33.95156263172585653, 464.5083255208626838, 6.608064661821390295 ) ) ;
#54208 = CARTESIAN_POINT ( 'NONE',  ( -5.683639242321874008, -47.06573826195067056, 103.9372442403038121 ) ) ;
#54209 = DIRECTION ( 'NONE',  ( 0.000000000000000000, 0.000000000000000000, 1.000000000000000000 ) ) ;
#54210 = CARTESIAN_POINT ( 'NONE',  ( -15.79261075262893677, 4.810720122707396129, 5.431533035186010494 ) ) ;
#54211 = EDGE_LOOP ( 'NONE', ( #81406, #55287 ) ) ;
#54212 = FACE_OUTER_BOUND ( 'NONE', #37111, .T. ) ;
#54213 = CARTESIAN_POINT ( 'NONE',  ( 85.68806591786149340, -29.99999999999991473, 176.4821778899267599 ) ) ;
#54214 = CARTESIAN_POINT ( 'NONE',  ( -13.59282890840906610, 24.77131182429118184, 0.3401920232233912045 ) ) ;
#54215 = CARTESIAN_POINT ( 'NONE',  ( -0.000000000000000000, 17.51648154115788714, -55.02144460582525909 ) ) ;
#54216 = EDGE_CURVE ( 'NONE', #22959, #9861, #24740, .T. ) ;
#54217 = CARTESIAN_POINT ( 'NONE',  ( 81.43563566675868515, -30.00000000000000711, -9.788353114720324655 ) ) ;
#54218 = CIRCLE ( 'NONE', #71475, 4.000000000000000888 ) ;
#54219 = EDGE_CURVE ( 'NONE', #79952, #43184, #24663, .T. ) ;
#54220 = DIRECTION ( 'NONE',  ( -1.000000000000000000, -1.224606353822377258E-16, -0.000000000000000000 ) ) ;
#54221 = ORIENTED_EDGE ( 'NONE', *, *, #3504, .F. ) ;
#54222 = PRODUCT_DEFINITION_FORMATION_WITH_SPECIFIED_SOURCE ( 'ANY', '', #19103, .NOT_KNOWN. ) ;
#54223 = VERTEX_POINT ( 'NONE', #47831 ) ;
#54224 = ORIENTED_EDGE ( 'NONE', *, *, #17507, .T. ) ;
#54225 = DIRECTION ( 'NONE',  ( 1.000000000000000000, 0.000000000000000000, -0.000000000000000000 ) ) ;
#54226 = DIRECTION ( 'NONE',  ( 0.000000000000000000, -0.8660254037844382635, -0.5000000000000008882 ) ) ;
#54227 = CARTESIAN_POINT ( 'NONE',  ( 5.700000000000000178, 0.000000000000000000, 0.000000000000000000 ) ) ;
#54228 = CARTESIAN_POINT ( 'NONE',  ( -6.943482370013978944, -85.52848370260724664, 3.973876482044368164 ) ) ;
#54229 = CYLINDRICAL_SURFACE ( 'NONE', #41512, 5.000000000000002665 ) ;
#54230 = ORIENTED_EDGE ( 'NONE', *, *, #94181, .F. ) ;
#54231 = CARTESIAN_POINT ( 'NONE',  ( 9.999999999999994671, 48.00000000000000000, -86.30899693747679180 ) ) ;
#54232 = ORIENTED_EDGE ( 'NONE', *, *, #70142, .T. ) ;
